#53009 = DIRECTION ( 'NONE',  ( 0.000000000000000000, 0.000000000000000000, 1.000000000000000000 ) ) ;
#53010 = CARTESIAN_POINT ( 'NONE',  ( 5.897433631820129918, 8.863794422890064695, -1.082531754730537976 ) ) ;
#53012 =( BOUNDED_CURVE ( )  B_SPLINE_CURVE ( 2, ( #167144, #51256, #100002, #38205, #68539, #166069, #168202, #153020, #202808, #121675, #134667, #34984, #154092, #69606, #4595, #120600, #200670, #17656, #84813, #102133, #186577, #71740, #187640, #55519, #83739, #18729, #5660, #104279, #19801, #170323, #184436, #137854, #21911, #149831, #1401, #101055, #88020, #169267, #203875, #67462, #133608, #199613, #183378, #150902, #37126, #20853, #2463, #185501, #103205, #52320, #118449, #36053, #85885, #135713, #151961, #3531, #201739, #53380, #119515, #194245, #108802, #160686, #75171, #144480, #211547, #93573, #95713, #92516, #78359, #29628, #61049, #63182, #127209, #126132, #109872, #13358, #193177, #12281, #142337, #141281, #143408, #207289, #175885 ),
 .UNSPECIFIED., .F., .T. ) 
 B_SPLINE_CURVE_WITH_KNOTS ( ( 3, 2, 2, 2, 2, 2, 2, 2, 2, 2, 2, 2, 2, 2, 2, 2, 2, 2, 2, 2, 2, 2, 2, 2, 2, 2, 2, 2, 2, 2, 2, 2, 2, 2, 2, 2, 2, 2, 2, 2, 2, 3 ),
 ( 0.1856859352924667417, 0.1944444444444444475, 0.2083333333333333426, 0.2222222222222222099, 0.2361111111111111049, 0.2500000000000000000, 0.2638888888888888951, 0.2777777777777777901, 0.2916666666666666852, 0.3055555555555555802, 0.3194444444444444198, 0.3333333333333333148, 0.3472222222222222099, 0.3611111111111111049, 0.3750000000000000000, 0.3888888888888888951, 0.4027777777777777901, 0.4166666666666666852, 0.4305555555555555802, 0.4444444444444444198, 0.4583333333333333148, 0.4722222222222222099, 0.4861111111111111049, 0.5000000000000000000, 0.5138888888888888395, 0.5277777777777777901, 0.5416666666666666297, 0.5555555555555555802, 0.5694444444444444198, 0.5833333333333333703, 0.5972222222222222099, 0.6111111111111111605, 0.6250000000000000000, 0.6388888888888888395, 0.6527777777777777901, 0.6666666666666667407, 0.6805555555555555802, 0.6944444444444444198, 0.7083333333333332593, 0.7222222222222220989, 0.7361111111111111605, 0.7435077961461751261 ),
 .UNSPECIFIED. ) 
 CURVE ( )  GEOMETRIC_REPRESENTATION_ITEM ( )  RATIONAL_B_SPLINE_CURVE ( ( 0.9375838258011983672, 0.9155139236497713551, 1.000000000000000000, 0.8660254037844387076, 1.000000000000000000, 0.8660254037844387076, 1.000000000000000000, 0.8660254037844387076, 1.000000000000000000, 0.8660254037844387076, 1.000000000000000000, 0.8660254037844387076, 1.000000000000000000, 0.8660254037844387076, 1.000000000000000000, 0.8660254037844387076, 1.000000000000000000, 0.8660254037844387076, 1.000000000000000000, 0.8660254037844387076, 1.000000000000000000, 0.8660254037844387076, 1.000000000000000000, 0.8660254037844387076, 1.000000000000000000, 0.8660254037844387076, 1.000000000000000000, 0.8660254037844387076, 1.000000000000000000, 0.8660254037844387076, 1.000000000000000000, 0.8660254037844387076, 1.000000000000000000, 0.8660254037844387076, 1.000000000000000000, 0.8660254037844387076, 1.000000000000000000, 0.8660254037844387076, 1.000000000000000000, 0.8660254037844387076, 1.000000000000000000, 0.8660254037844387076, 1.000000000000000000, 0.8660254037844387076, 1.000000000000000000, 0.8660254037844387076, 1.000000000000000000, 0.8660254037844387076, 1.000000000000000000, 0.8660254037844387076, 1.000000000000000000, 0.8660254037844387076, 1.000000000000000000, 0.8660254037844387076, 1.000000000000000000, 0.8660254037844387076, 1.000000000000000000, 0.8660254037844387076, 1.000000000000000000, 0.8660254037844387076, 1.000000000000000000, 0.8660254037844387076, 1.000000000000000000, 0.8660254037844387076, 1.000000000000000000, 0.8660254037844387076, 1.000000000000000000, 0.8660254037844387076, 1.000000000000000000, 0.8660254037844387076, 1.000000000000000000, 0.8660254037844387076, 1.000000000000000000, 0.8660254037844387076, 1.000000000000000000, 0.8660254037844387076, 1.000000000000000000, 0.8660254037844387076, 1.000000000000000000, 0.8660254037844387076, 1.000000000000000000, 0.9286503118547393409, 0.9332967922701964625 ) ) 
 REPRESENTATION_ITEM ( '' )  );
#53011 = CARTESIAN_POINT ( 'NONE',  ( 1.364683531249996529, 13.27604166700806765, 0.7879004041258403923 ) ) ;
#53014 = CARTESIAN_POINT ( 'NONE',  ( 1.101899038012419174, -0.8149344392366760781, 1.617857622727811862 ) ) ;
#53013 = CARTESIAN_POINT ( 'NONE',  ( 6.343235766347262938, 8.493804042195527870, -1.599625672291281386 ) ) ;
#53015 = CARTESIAN_POINT ( 'NONE',  ( -8.128276786592724790, 9.441743324901704426, -1.199719254218446718 ) ) ;
#53016 = CARTESIAN_POINT ( 'NONE',  ( 4.656335691289526402, 7.519809842224722374, -1.199719254218452047 ) ) ;
#53017 = DIRECTION ( 'NONE',  ( -1.000000000000000000, 5.578564026256490882E-16, -1.264049978315544409E-61 ) ) ;
#53018 = CARTESIAN_POINT ( 'NONE',  ( -11.49978884755372732, 11.24270821162817668, 3.429452816445257124 ) ) ;
#53019 = CARTESIAN_POINT ( 'NONE',  ( 3.928111819657337911, 5.605883094398769195, 1.599625672291267398 ) ) ;
#53020 = ORIENTED_EDGE ( 'NONE', *, *, #129464, .T. ) ;
#53021 = CARTESIAN_POINT ( 'NONE',  ( 5.923453886551514280, -1.462456689723025782, -1.388475849216065372 ) ) ;
#53022 = CARTESIAN_POINT ( 'NONE',  ( -0.1104750535120025967, -0.004616138082884357029, -2.103378236956429337 ) ) ;
#53023 = CARTESIAN_POINT ( 'NONE',  ( -2.995508107964761191, 6.411541510041463887, -0.7147908198718248007 ) ) ;
#53024 = CARTESIAN_POINT ( 'NONE',  ( 0.1405533004714800693, 1.287645162063441928, -2.525240623925705474 ) ) ;
#53025 = DIRECTION ( 'NONE',  ( 6.314299915563594049E-62, 8.546850786086437571E-32, 1.000000000000000000 ) ) ;
#53026 = CARTESIAN_POINT ( 'NONE',  ( -4.067082894419624672, 6.728385229256075739, 1.082531754730560403 ) ) ;
#53027 = CARTESIAN_POINT ( 'NONE',  ( 8.595506201384004896, 12.01154575404795466, 1.082531754730546636 ) ) ;
#53028 = CARTESIAN_POINT ( 'NONE',  ( 3.731269929808676000, 0.05278475387572807015, -1.968924232409387409 ) ) ;
#53029 = CARTESIAN_POINT ( 'NONE',  ( 4.288685525864014636, 1.556897452430844320, -1.281376678550147474 ) ) ;
#53030 = CARTESIAN_POINT ( 'NONE',  ( -5.910464900553636269, 8.982960586366182554, -1.199719254218440723 ) ) ;
#53031 = CARTESIAN_POINT ( 'NONE',  ( 6.727182134110196721, 6.033756510516266935, 2.783943001041962795 ) ) ;
#53032 = CARTESIAN_POINT ( 'NONE',  ( 4.752002516643937469, 0.8370584164609263800, 2.025481692006773748 ) ) ;
#53033 = CARTESIAN_POINT ( 'NONE',  ( -10.18461545817740088, 3.956598013261175772, 5.433575010662861082 ) ) ;
#53034 = CARTESIAN_POINT ( 'NONE',  ( 2.625899107431714175, -1.107553820047700199, -1.575994028688005644 ) ) ;
#53035 = CARTESIAN_POINT ( 'NONE',  ( -8.694856585065634746, 9.038420858865048757, 0.7998128361456462443 ) ) ;
#53036 = CARTESIAN_POINT ( 'NONE',  ( -0.1294898018152226826, 6.948707995275583471, -2.521562306467279857 ) ) ;
#53037 = CARTESIAN_POINT ( 'NONE',  ( 0.1533209562146371774, -1.769702838771534559, 1.318327933512997152 ) ) ;
#53038 = DIRECTION ( 'NONE',  ( 1.214306433183764966E-17, 1.000000000000000000, 5.200010849845536803E-32 ) ) ;
#53039 = EDGE_CURVE ( 'NONE', #145305, #160077, #106576, .T. ) ;
#53040 = VERTEX_POINT ( 'NONE', #155279 ) ;
#53041 = CARTESIAN_POINT ( 'NONE',  ( 5.085717018901939390, 5.105960408239938353, 0.000000000000000000 ) ) ;
#53042 = ORIENTED_EDGE ( 'NONE', *, *, #207178, .T. ) ;
#53043 = CARTESIAN_POINT ( 'NONE',  ( 5.102387438446081447, 1.963913563476852309, 0.1487572088093111478 ) ) ;
#53045 = CARTESIAN_POINT ( 'NONE',  ( 4.248693477488805215, 1.974695210492120045, 0.3904942472512766827 ) ) ;
#53044 = CARTESIAN_POINT ( 'NONE',  ( 0.6791179963998601465, 1.305170301278056444, 1.438240348306470739 ) ) ;
#53046 = CARTESIAN_POINT ( 'NONE',  ( 5.782642724008081103, -2.244312133422786015, 0.4951331349164668216 ) ) ;
#53048 = CARTESIAN_POINT ( 'NONE',  ( 3.994834637159989654, 0.2691826048217076384, 1.841218289905453664 ) ) ;
#53047 = CARTESIAN_POINT ( 'NONE',  ( 10.59763834280244232, 9.799999999999998934, -3.303285708550596222 ) ) ;
#53049 = CARTESIAN_POINT ( 'NONE',  ( 6.688968683495743583, 8.897159112202094988, -1.599625672291283607 ) ) ;
#53050 = CARTESIAN_POINT ( 'NONE',  ( -7.777967379493323286, -6.134628647623485698, -7.664830294503433450 ) ) ;
#53051 = CARTESIAN_POINT ( 'NONE',  ( 4.207966135563078858, 7.175396087857926375, 7.500000000000000000 ) ) ;
#53052 = CARTESIAN_POINT ( 'NONE',  ( -5.194745412330402878, 9.212286747694129474, 0.000000000000000000 ) ) ;
#53053 = CARTESIAN_POINT ( 'NONE',  ( -3.375444385298249195, -0.9484041558699626284, 0.1508549929727657779 ) ) ;
#53054 = CARTESIAN_POINT ( 'NONE',  ( 0.4334776158547505864, -1.553986563932317377, -1.545601477622601472 ) ) ;
#53055 = CARTESIAN_POINT ( 'NONE',  ( 6.371969008742804697, 7.496680600697164465, -1.082531754730543083 ) ) ;
#53056 = VERTEX_POINT ( 'NONE', #74028 ) ;
#53057 = LINE ( 'NONE', #88779, #150419 ) ;
#53058 = CARTESIAN_POINT ( 'NONE',  ( 0.4162703231485806454, 1.261427835099769634, -1.320066674804179385 ) ) ;
#53059 = CARTESIAN_POINT ( 'NONE',  ( -5.284980951228653190, 5.060232619388524533, 0.000000000000000000 ) ) ;
#53060 = AXIS2_PLACEMENT_3D ( 'NONE', #127579, #211912, #195687 ) ;
#53061 = CARTESIAN_POINT ( 'NONE',  ( 2.478840559695635548, -1.729657056378102853, -0.1252908626025364403 ) ) ;
#53062 = CARTESIAN_POINT ( 'NONE',  ( 1.499999999999959588, 8.500000000000000000, -10.89724735885168805 ) ) ;
#53063 = CARTESIAN_POINT ( 'NONE',  ( -11.04536101718726293, 10.09409062111168964, -1.100000000000000311 ) ) ;
#53064 = CARTESIAN_POINT ( 'NONE',  ( 0.4288785890452541105, 3.049942316455306113, 0.4196807566830256797 ) ) ;
#53065 = TOROIDAL_SURFACE ( 'NONE', #70209, 10.89999999999920632, 0.2000000000000000111 ) ;
#53066 = CARTESIAN_POINT ( 'NONE',  ( 5.022008369909983116, -0.9795521577263366364, -1.540466923627185292 ) ) ;
#53067 = CARTESIAN_POINT ( 'NONE',  ( 2.957805016080543137, -0.6199431972748243869, 1.861265166911832081 ) ) ;
#53068 = CARTESIAN_POINT ( 'NONE',  ( 0.6124999999999534150, -1.104166665983841167, 1.060881119635882497 ) ) ;
#53069 = CARTESIAN_POINT ( 'NONE',  ( -8.422639742587602285, 10.84949900448412841, -1.599625672291263179 ) ) ;
#53070 = CARTESIAN_POINT ( 'NONE',  ( 7.558834334818744338, 8.777393797832065303, 1.199719254218462483 ) ) ;
#53071 = CARTESIAN_POINT ( 'NONE',  ( 4.600305182625006317, -0.9987976242244798186, 1.870504488178956759 ) ) ;
#53072 = CARTESIAN_POINT ( 'NONE',  ( 7.856023664475727308, 8.130058794835305136, -0.7998128361456341429 ) ) ;
#53073 = CARTESIAN_POINT ( 'NONE',  ( -10.48453286206953727, 11.12637651536962125, 0.7998128361456462443 ) ) ;
#53074 = CIRCLE ( 'NONE', #87714, 0.07999999999999993228 ) ;
#53075 = CARTESIAN_POINT ( 'NONE',  ( 2.711853232431875593, 0.5564382603544039130, -1.993978196652478996 ) ) ;
#53077 = B_SPLINE_CURVE_WITH_KNOTS ( 'NONE', 3,
 ( #73815, #173478, #140995, #157212, #207003, #9872, #124787, #13061, #29336, #159329 ),
 .UNSPECIFIED., .F., .F.,
 ( 4, 3, 3, 4 ),
 ( 3.907308343762969252E-16, 8.899070015639609047E-05, 0.0001343825223669382267, 0.0001804666533476734377 ),
 .UNSPECIFIED. ) ;
#53076 = CARTESIAN_POINT ( 'NONE',  ( 1.364683531249986537, 0.4260416670080872659, 0.7879004041258500513 ) ) ;
#53079 = ORIENTED_EDGE ( 'NONE', *, *, #18341, .F. ) ;
#53078 = CARTESIAN_POINT ( 'NONE',  ( 4.336746411289113645, 1.366526421497065824, -1.751164563135388041 ) ) ;
#53080 = CARTESIAN_POINT ( 'NONE',  ( 3.323114718373169740, 1.032193166631629078, -2.053959190227053533 ) ) ;
#53081 = CARTESIAN_POINT ( 'NONE',  ( 7.619319141200051604, 11.83303006480134911, 0.7216878364870438212 ) ) ;
#53083 = CARTESIAN_POINT ( 'NONE',  ( 3.285556943749998737, -3.055208332855376518, -1.896917185911906500 ) ) ;
#53082 = CARTESIAN_POINT ( 'NONE',  ( 6.373741612200160667, 9.489763409991955001, 1.082531754730549078 ) ) ;
#53084 = ADVANCED_FACE ( 'NONE', ( #53501 ), #195363, .F. ) ;
#53085 = CARTESIAN_POINT ( 'NONE',  ( 0.000000000000000000, 2.499999999999998668, -4.500000000000000000 ) ) ;
#53086 =( NAMED_UNIT ( * ) PLANE_ANGLE_UNIT ( ) SI_UNIT ( $, .RADIAN. ) );
#53087 = ORIENTED_EDGE ( 'NONE', *, *, #118912, .F. ) ;
#53088 = CARTESIAN_POINT ( 'NONE',  ( -5.520955638564554846, 6.243838396700211568, -0.9653654033580265637 ) ) ;
#53089 = CARTESIAN_POINT ( 'NONE',  ( 2.918110517850933672, -1.910018876965378309, 0.09814724848770939314 ) ) ;
#53090 = CARTESIAN_POINT ( 'NONE',  ( 3.475000000000000533, -1.254166666666665098, 2.006292185433948827 ) ) ;
#53091 = CARTESIAN_POINT ( 'NONE',  ( 4.295721138614797319, -0.6590762262537721572, 1.594082981517078945 ) ) ;
#53092 = CARTESIAN_POINT ( 'NONE',  ( 2.887907956677421062, -2.014008092954455265, 0.1037802451031161616 ) ) ;
#53093 = CARTESIAN_POINT ( 'NONE',  ( 4.500793239850611194, -2.254531372669385636, 0.4477389049844481272 ) ) ;
#53094 = CARTESIAN_POINT ( 'NONE',  ( 0.000000000000000000, 13.49999999999999822, -1.500000000000000222 ) ) ;
#53095 = CARTESIAN_POINT ( 'NONE',  ( 6.076811011874215573, -1.999271364452784638, -0.6623750905550094270 ) ) ;
#53096 = CARTESIAN_POINT ( 'NONE',  ( -5.858531774880906262, 6.967946837850073294, 1.082531754730549078 ) ) ;
#53097 = ORIENTED_EDGE ( 'NONE', *, *, #209714, .F. ) ;
#53098 = CARTESIAN_POINT ( 'NONE',  ( 4.885902211565920972, -0.8344178305333300738, 1.560695085661115922 ) ) ;
#53099 = EDGE_CURVE ( 'NONE', #75305, #186393, #36441, .T. ) ;
#53101 = CARTESIAN_POINT ( 'NONE',  ( 0.7621917111494004304, 1.134545731666029011, 1.991736209811171054 ) ) ;
#53100 = CARTESIAN_POINT ( 'NONE',  ( 6.230854113932139171, 9.427024345299638952, 1.199719254218452047 ) ) ;
#53102 = CARTESIAN_POINT ( 'NONE',  ( 0.05802509242504564485, -1.552030147408272054, -0.7874549631982865616 ) ) ;
#53103 = CARTESIAN_POINT ( 'NONE',  ( -1.843739406749240750, 8.499999999999996447, -0.7749999999999996891 ) ) ;
#53104 = CARTESIAN_POINT ( 'NONE',  ( 6.386699327874667098, 1.908680410311427433, -1.076638258889956345 ) ) ;
#53105 = CARTESIAN_POINT ( 'NONE',  ( -5.004894982100124068, 5.868074229652107121, 1.199719254218452935 ) ) ;
#53106 = DIRECTION ( 'NONE',  ( -0.000000000000000000, 1.000000000000000000, -0.000000000000000000 ) ) ;
#53107 = CARTESIAN_POINT ( 'NONE',  ( 3.953965674029162436, 7.318484642604417445, -0.9046105126420730391 ) ) ;
#53108 = CARTESIAN_POINT ( 'NONE',  ( 6.777786256569462431, -2.009253640576996514, 0.4989836931604470505 ) ) ;
#53109 = CARTESIAN_POINT ( 'NONE',  ( 1.639861632979456418, 2.010800986640928656, -0.1531718788195315928 ) ) ;
#53110 = CARTESIAN_POINT ( 'NONE',  ( 1.364683531249990311, 5.613541667008087543, 0.7879004041258500513 ) ) ;
#53111 = CARTESIAN_POINT ( 'NONE',  ( 4.951747152513418904, 0.6024649636334912239, -1.829943702413504791 ) ) ;
#53112 = CARTESIAN_POINT ( 'NONE',  ( -1.364683531250010295, 11.38020833367473728, 0.7879004041258445001 ) ) ;
#53113 = CARTESIAN_POINT ( 'NONE',  ( 1.354101172232239580, -1.613524214714330940, -1.527088627841047375 ) ) ;
#53115 = VERTEX_POINT ( 'NONE', #75094 ) ;
#53114 = CARTESIAN_POINT ( 'NONE',  ( 8.380911511541880188, 12.92948053010758258, 0.7998128361456462443 ) ) ;
#53117 = DIRECTION ( 'NONE',  ( 0.000000000000000000, 1.000000000000000000, 6.661338147750951075E-16 ) ) ;
#53116 = CARTESIAN_POINT ( 'NONE',  ( 1.217358635584784965, 3.014784080462326266, -0.7749999999999840350 ) ) ;
#53118 = CYLINDRICAL_SURFACE ( 'NONE', #102730, 1.250000000000000000 ) ;
#53119 = CARTESIAN_POINT ( 'NONE',  ( 9.134442807305049428, 11.67993591332117376, 1.599625672291281386 ) ) ;
#53120 = CARTESIAN_POINT ( 'NONE',  ( -5.395781948114519722, 5.397426482329451325, 0.000000000000000000 ) ) ;
#53121 = LINE ( 'NONE', #3278, #177088 ) ;
#53122 = CARTESIAN_POINT ( 'NONE',  ( 4.616618505336416156, -0.07905358554981949115, 1.738770568734932853 ) ) ;
#53123 = CARTESIAN_POINT ( 'NONE',  ( 1.996468121258226924, 1.940055844723225009, 0.2909814450420752929 ) ) ;
#53125 = CARTESIAN_POINT ( 'NONE',  ( -0.6823417656250003738, 3.030208333674754062, -1.181850606188749264 ) ) ;
#53124 = CARTESIAN_POINT ( 'NONE',  ( 3.388648328411762556, 6.040841252200647382, 1.199719254218462483 ) ) ;
#53126 = CARTESIAN_POINT ( 'NONE',  ( -5.852179643265606579, 6.035944939585320412, -0.4116468081218557784 ) ) ;
#53127 = CARTESIAN_POINT ( 'NONE',  ( 8.530051201292206287, 13.10347683481629488, 0.000000000000000000 ) ) ;
#53128 = CIRCLE ( 'NONE', #136171, 0.07999999999999940492 ) ;
#53129 = VECTOR ( 'NONE', #203836, 1000.000000000000000 ) ;
#53130 = CARTESIAN_POINT ( 'NONE',  ( 6.197705743426439540, -1.420020466879829302, -1.353909852041992767 ) ) ;
#53131 = CARTESIAN_POINT ( 'NONE',  ( -7.588813295347149435, 9.876701482703580837, -1.599625672291263179 ) ) ;
#53132 = EDGE_CURVE ( 'NONE', #21505, #62722, #147729, .T. ) ;
#53133 = CARTESIAN_POINT ( 'NONE',  ( -3.253593677155282471, 6.739683690082376444, 1.040834085586084257E-14 ) ) ;
#53134 = CARTESIAN_POINT ( 'NONE',  ( 1.499281897245376527, 1.848817473390499844, -1.303928773892924609 ) ) ;
#53136 = VERTEX_POINT ( 'NONE', #131367 ) ;
#53135 = CARTESIAN_POINT ( 'NONE',  ( -5.904739593951539689, 6.847616600153594746, 1.199719254218450271 ) ) ;
#53137 = CARTESIAN_POINT ( 'NONE',  ( -0.7500000000000006661, 0.3895833340161539149, -1.299038105676652011 ) ) ;
#53138 = CARTESIAN_POINT ( 'NONE',  ( 1.809613641711980359, -1.857008771552502768, 0.2239427725650791623 ) ) ;
#53139 = CARTESIAN_POINT ( 'NONE',  ( 0.2989044949552251418, 1.198067244415670141, -1.254020425504979164 ) ) ;
#53140 = VECTOR ( 'NONE', #42323, 1000.000000000000114 ) ;
#53141 = CARTESIAN_POINT ( 'NONE',  ( 4.704715985517350596, 1.906866092115505840, 1.080010033982371498 ) ) ;
#53142 = CARTESIAN_POINT ( 'NONE',  ( 5.034332918631054810, 1.191367258472323831, -1.976142064534849307 ) ) ;
#53143 = CARTESIAN_POINT ( 'NONE',  ( 1.463821189631772990, 2.030551501382936497, -0.3513165408277911794 ) ) ;
#53144 = CARTESIAN_POINT ( 'NONE',  ( 3.152217820003437421, -1.470166820979129207, 1.268861441860974049 ) ) ;
#53145 = CARTESIAN_POINT ( 'NONE',  ( -4.406036734316900905, 5.203092947200234519, -1.082531754730543971 ) ) ;
#53146 = CARTESIAN_POINT ( 'NONE',  ( 5.395714598229544023, -0.6742385858747660388, 1.744967798948720228 ) ) ;
#53147 = CARTESIAN_POINT ( 'NONE',  ( 4.001984418394623155, 7.593073144423666321, -0.1798963839820325039 ) ) ;
#53148 = CARTESIAN_POINT ( 'NONE',  ( 6.556017512941495262, 1.755498886817616677, -0.9912500394320120645 ) ) ;
#53149 = CARTESIAN_POINT ( 'NONE',  ( 4.041739190649647817, 6.769093918182960579, -1.082531754730548412 ) ) ;
#53150 = CARTESIAN_POINT ( 'NONE',  ( -1.360316468750013108, 1.140625000341413564, -2.081668171172168513E-14 ) ) ;
#53152 = CARTESIAN_POINT ( 'NONE',  ( 4.430314669760617718, -1.560499787156752971, -1.277043788614096176 ) ) ;
#53151 = AXIS2_PLACEMENT_3D ( 'NONE', #35961, #18637, #134574 ) ;
#53153 = CARTESIAN_POINT ( 'NONE',  ( -4.758548728272219641, 4.653987725846768342, 0.7216878364870317197 ) ) ;
#53154 = CARTESIAN_POINT ( 'NONE',  ( -6.642568916052639771, 6.714361588341672515, 0.000000000000000000 ) ) ;
#53155 = CARTESIAN_POINT ( 'NONE',  ( 8.259941899223605333, 10.65968485389279508, -1.599625672291268286 ) ) ;
#53157 = CARTESIAN_POINT ( 'NONE',  ( -1.230761180058579152, 3.146116465842661025, 0.7750000000000100142 ) ) ;
#53156 = CARTESIAN_POINT ( 'NONE',  ( 1.646812808029130215, -1.543121136568927243, 0.9753659028155501343 ) ) ;
#53158 = CARTESIAN_POINT ( 'NONE',  ( -4.797606254389363833, 6.690569611577942943, 1.599625672291263179 ) ) ;
#53159 = CARTESIAN_POINT ( 'NONE',  ( -5.438755897737433287, 6.374245297895642537, -1.199719254218453823 ) ) ;
#53160 = CARTESIAN_POINT ( 'NONE',  ( -10.12531724201500616, 3.239403609407997653, 5.873437370650227862 ) ) ;
#53161 = VERTEX_POINT ( 'NONE', #98819 ) ;
#53162 = CARTESIAN_POINT ( 'NONE',  ( -6.007671464186866928, 8.102312356341712984, 1.443375672974058777 ) ) ;
#53163 = UNCERTAINTY_MEASURE_WITH_UNIT (LENGTH_MEASURE( 1.000000000000000082E-05 ), #207917, 'distance_accuracy_value', 'NONE');
#53164 = CARTESIAN_POINT ( 'NONE',  ( -3.898132859128961236, 4.506575409527250997, -1.199719254218452047 ) ) ;
#53165 = CARTESIAN_POINT ( 'NONE',  ( -10.63367255181986160, 11.30037282007833532, 1.040834085586084257E-14 ) ) ;
#53166 = CARTESIAN_POINT ( 'NONE',  ( 5.795571226005820087, 1.865288689459403848, -0.7749498061812712946 ) ) ;
#53168 = ORIENTED_EDGE ( 'NONE', *, *, #106621, .T. ) ;
#53167 = CARTESIAN_POINT ( 'NONE',  ( 0.5398874254142792539, -2.012210497580559476, 0.6691108114003360141 ) ) ;
#53169 = CARTESIAN_POINT ( 'NONE',  ( -6.180537922983287302, 8.303989891604203422, -1.599625672291271394 ) ) ;
#53170 = CARTESIAN_POINT ( 'NONE',  ( 6.166260936116925606, 6.088392601758203071, 0.7998128361456341429 ) ) ;
#53171 = CARTESIAN_POINT ( 'NONE',  ( 5.084866380259029484, -0.2499542577577648639, -2.045595823183245621 ) ) ;
#53172 = CARTESIAN_POINT ( 'NONE',  ( 4.606092368833686557, -0.09613688574180989654, 2.014232646917232916 ) ) ;
#53173 = VERTEX_POINT ( 'NONE', #197362 ) ;
#53174 = ORIENTED_EDGE ( 'NONE', *, *, #185954, .T. ) ;
#53175 = CARTESIAN_POINT ( 'NONE',  ( 10.04733898909039702, 1.529612873802630224, 6.247711339170956890 ) ) ;
#53176 = CARTESIAN_POINT ( 'NONE',  ( -1.861683537984881509, 2.483860266822599083, 2.478752606221127142 ) ) ;
#53178 = ORIENTED_EDGE ( 'NONE', *, *, #151345, .F. ) ;
#53177 = CARTESIAN_POINT ( 'NONE',  ( -5.468734858265826837, 7.473552982767158070, 1.599625672291263179 ) ) ;
#53179 = CARTESIAN_POINT ( 'NONE',  ( 5.184698244283005408, 7.856242361780820360, 1.254847465626233616 ) ) ;
#53180 = CARTESIAN_POINT ( 'NONE',  ( 5.518907608433407219, 2.013924273726455549, -0.09612181791086168992 ) ) ;
#53181 = CARTESIAN_POINT ( 'NONE',  ( 3.960763856159645879, 0.2235175650571289141, -1.827449369368571386 ) ) ;
#53182 = CARTESIAN_POINT ( 'NONE',  ( -0.02319159430947542386, 0.2540490248266329965, -1.846305437520213477 ) ) ;
#53183 = CARTESIAN_POINT ( 'NONE',  ( 1.647554839532150872, -1.947651944554330772, 1.237524531948221096 ) ) ;
#53184 = CARTESIAN_POINT ( 'NONE',  ( 7.679767667498067496, 7.924426798361372093, 0.000000000000000000 ) ) ;
#53185 = CARTESIAN_POINT ( 'NONE',  ( 4.376362478467909156, -1.248523626585487989, 1.764366501186130698 ) ) ;
#53186 = CARTESIAN_POINT ( 'NONE',  ( 7.086107841436786181, 11.41887624831828418, 1.040834085586084257E-14 ) ) ;
#53188 = CARTESIAN_POINT ( 'NONE',  ( 2.676970549635893537, 1.727063564601112100, -1.040793759654296213 ) ) ;
#53187 = CARTESIAN_POINT ( 'NONE',  ( -0.05917297228825654093, -1.501800262597710267, -1.231000148999121357 ) ) ;
#53189 = CARTESIAN_POINT ( 'NONE',  ( -6.084912014434944894, 5.993485526462540847, -0.7998128361456291469 ) ) ;
#53190 = DIRECTION ( 'NONE',  ( -0.6743504407188151140, 0.000000000000000000, -0.7384114592165670343 ) ) ;
#53191 = CARTESIAN_POINT ( 'NONE',  ( -3.578989363883261277, 7.119311991265024453, 1.040834085586084257E-14 ) ) ;
#53192 = CARTESIAN_POINT ( 'NONE',  ( 3.819104250046548632, -0.1383300533824398659, 1.865606469731183825 ) ) ;
#53193 = CARTESIAN_POINT ( 'NONE',  ( 6.631714602856194851, -1.287423518921044341, -1.493153376739835947 ) ) ;
#53195 = CARTESIAN_POINT ( 'NONE',  ( -7.425025402139490360, 8.691559719698066289, 1.199719254218452047 ) ) ;
#53194 = CARTESIAN_POINT ( 'NONE',  ( -0.7500000000000249800, -1.277083332650516656, 1.299038105676659116 ) ) ;
#53196 = CARTESIAN_POINT ( 'NONE',  ( 1.541937560865791479, -1.600244427420342896, -1.519961040588948986 ) ) ;
#53197 = ORIENTED_EDGE ( 'NONE', *, *, #212020, .T. ) ;
#53198 = CARTESIAN_POINT ( 'NONE',  ( 11.78331023100045627, 13.79999999999998295, 1.799999999999999600 ) ) ;
#53199 = CARTESIAN_POINT ( 'NONE',  ( 3.181359600701000989, 6.863336634126477875, 0.000000000000000000 ) ) ;
#53200 = CARTESIAN_POINT ( 'NONE',  ( -3.411848212133334446, 7.132240014130862171, 0.7998128361456341429 ) ) ;
#53201 = CARTESIAN_POINT ( 'NONE',  ( -7.784592198500340565, -5.601927612791713251, 7.772296586883744141 ) ) ;
#53202 = CARTESIAN_POINT ( 'NONE',  ( 6.789933821422706295, -0.8420773930338676383, 1.780570074765168043 ) ) ;
#53203 = CARTESIAN_POINT ( 'NONE',  ( 0.3765545373161778286, 1.332373789618445770, 1.883912488508274752 ) ) ;
#53204 = CARTESIAN_POINT ( 'NONE',  ( 0.4671467121175364445, 1.705069321186868159, 0.9702857188121425391 ) ) ;
#53205 = CARTESIAN_POINT ( 'NONE',  ( 4.522371018022923295, 0.9678747400500853360, 1.821345444039919270 ) ) ;
#53206 = CARTESIAN_POINT ( 'NONE',  ( 5.666945020832177882, 6.674152614801420746, 1.082531754730558626 ) ) ;
#53207 = CARTESIAN_POINT ( 'NONE',  ( 5.397027666691686321, 8.454226823519094935, 1.199719254218451159 ) ) ;
#53208 = ORIENTED_EDGE ( 'NONE', *, *, #198981, .F. ) ;
#53209 =( BOUNDED_CURVE ( )  B_SPLINE_CURVE ( 2, ( #172382, #156136, #7718, #139896, #27176, #62876, #79129, #177716, #109582 ),
 .UNSPECIFIED., .F., .T. ) 
 B_SPLINE_CURVE_WITH_KNOTS ( ( 3, 2, 2, 2, 3 ),
 ( 0.8660714285714286031, 0.8690476190476190688, 0.8750000000000000000, 0.8809523809523809312, 0.8839285714285713969 ),
 .UNSPECIFIED. ) 
 CURVE ( )  GEOMETRIC_REPRESENTATION_ITEM ( )  RATIONAL_B_SPLINE_CURVE ( ( 0.9330127018922194093, 0.9330127018922194093, 1.000000000000000000, 0.8660254037844387076, 1.000000000000000000, 0.8660254037844387076, 1.000000000000000000, 0.9330127018922194093, 0.9330127018922194093 ) ) 
 REPRESENTATION_ITEM ( '' )  );
#53210 = CARTESIAN_POINT ( 'NONE',  ( 7.795575137733369075, 9.157554417852841411, -1.082531754730537976 ) ) ;
#53211 = CARTESIAN_POINT ( 'NONE',  ( 1.364683531249990311, 5.196875000341417916, 1.214306433183764966E-14 ) ) ;
#53212 = CARTESIAN_POINT ( 'NONE',  ( -10.30773516381138855, 3.837475087047823141, -6.058016394929252257 ) ) ;
#53213 = CARTESIAN_POINT ( 'NONE',  ( 4.731432421044862835, 6.543090462684225450, -1.443375672974051449 ) ) ;
#53214 = CARTESIAN_POINT ( 'NONE',  ( 6.602019255160630706, 0.8372048429528687885, -2.003470777635954381 ) ) ;
#53216 = CARTESIAN_POINT ( 'NONE',  ( 5.618664544990171095, -0.03892770779775727580, 1.841008343696965310 ) ) ;
#53215 = CARTESIAN_POINT ( 'NONE',  ( 9.498884310698278099, -9.746166700192997467, -0.1658036423878402332 ) ) ;
#53217 = CARTESIAN_POINT ( 'NONE',  ( -2.483409115735836892, 3.555461883994699868, 11.68352130004407030 ) ) ;
#53218 = CARTESIAN_POINT ( 'NONE',  ( 1.947569660854353790, 3.752493983412333645, 0.4616071351972801939 ) ) ;
#53219 = DIRECTION ( 'NONE',  ( 0.000000000000000000, 0.000000000000000000, -1.000000000000000000 ) ) ;
#53220 = CARTESIAN_POINT ( 'NONE',  ( -4.357679483485834560, 7.387146062586773532, 1.181458644690215998 ) ) ;
#53221 = CARTESIAN_POINT ( 'NONE',  ( -0.4000000000000114575, 2.902482508373164904, 2.023857702507793288 ) ) ;
#53222 = CARTESIAN_POINT ( 'NONE',  ( 5.364607279338250656, 7.693244595681929532, -1.319704323257679057 ) ) ;
#53223 = CARTESIAN_POINT ( 'NONE',  ( -0.6823417656249969321, 5.280208333674756283, -1.181850606188749264 ) ) ;
#53224 = CARTESIAN_POINT ( 'NONE',  ( 1.629408300089077111, -0.2329066467734331181, 1.897959532673603844 ) ) ;
#53225 = CARTESIAN_POINT ( 'NONE',  ( 1.709447022217532641, -1.756973726300320449, 0.2123998563456699906 ) ) ;
#53226 = CARTESIAN_POINT ( 'NONE',  ( 5.883453010584854148, 0.1459518013421389204, -2.007843741401983184 ) ) ;
#53228 = CARTESIAN_POINT ( 'NONE',  ( 4.306187113567048641, 1.175507255964372222, -1.512451795395561405 ) ) ;
#53227 = CARTESIAN_POINT ( 'NONE',  ( -8.292783513053063160, 12.82666453187061073, 0.7998128361456481317 ) ) ;
#53229 = DIRECTION ( 'NONE',  ( -7.387867266669436732E-31, -1.000000000000000000, 8.546850786086437571E-32 ) ) ;
#53230 = B_SPLINE_CURVE_WITH_KNOTS ( 'NONE', 3,
 ( #167611, #84221, #129865, #115714 ),
 .UNSPECIFIED., .F., .F.,
 ( 4, 4 ),
 ( -1.944647862007489213E-06, 0.0001035599091551129175 ),
 .UNSPECIFIED. ) ;
#53231 = CARTESIAN_POINT ( 'NONE',  ( 5.125436402459787821, 0.1948648891074710732, -1.959901157258244098 ) ) ;
#53232 = CARTESIAN_POINT ( 'NONE',  ( 0.3871773095200456982, -1.998849835692744659, -0.7086421328065874992 ) ) ;
#53233 = CARTESIAN_POINT ( 'NONE',  ( 0.000000000000000000, -6.893137084989842123, 0.000000000000000000 ) ) ;
#53234 = CARTESIAN_POINT ( 'NONE',  ( 4.240975883383619305, -1.627667033997456381, 0.9218181776217827528 ) ) ;
#53236 = ORIENTED_EDGE ( 'NONE', *, *, #58935, .F. ) ;
#53235 = CARTESIAN_POINT ( 'NONE',  ( 6.340463942928090901, 1.707257656261139234, 0.2451334271395839426 ) ) ;
#53238 = DIRECTION ( 'NONE',  ( -0.05727394217551268901, 3.884134901109067902E-16, -0.9983585005135560131 ) ) ;
#53237 = CARTESIAN_POINT ( 'NONE',  ( 3.651171877326536030, -1.804458330144659950, 1.270265763067345066 ) ) ;
#53239 = EDGE_CURVE ( 'NONE', #146583, #64997, #10735, .T. ) ;
#53240 = CARTESIAN_POINT ( 'NONE',  ( -0.6823417656250212460, 4.113541667008085767, 1.181850606188767472 ) ) ;
#53241 = CARTESIAN_POINT ( 'NONE',  ( 0.8188879582939897483, -1.495318261269963589, 1.421039783695568604 ) ) ;
#53242 = CARTESIAN_POINT ( 'NONE',  ( 8.288111976655649471, 8.563885482386732306, -0.7998128361456291469 ) ) ;
#53243 = CARTESIAN_POINT ( 'NONE',  ( -7.492852449846775897, 11.89341162479659531, 0.000000000000000000 ) ) ;
#53244 = CARTESIAN_POINT ( 'NONE',  ( -9.333041836226904309, 15.44694763438996077, -7.472413793095822321 ) ) ;
#53245 = CARTESIAN_POINT ( 'NONE',  ( -4.416205349749324327, 6.175325546172741653, 1.599625672291267175 ) ) ;
#53246 = CARTESIAN_POINT ( 'NONE',  ( -5.277545713794630444, 7.647399700472480077, -1.235574677996098325 ) ) ;
#53247 = ORIENTED_EDGE ( 'NONE', *, *, #910, .F. ) ;
#53248 = CARTESIAN_POINT ( 'NONE',  ( 2.945825538390862697, 1.462269270728074222, 1.465923284304726737 ) ) ;
#53249 = CARTESIAN_POINT ( 'NONE',  ( 1.499999999999990896, 4.275000000000021672, 1.214306433183764966E-14 ) ) ;
#53250 = CARTESIAN_POINT ( 'NONE',  ( 5.335297142177534369, 6.183267073083954735, -1.199719254218452047 ) ) ;
#53251 = CARTESIAN_POINT ( 'NONE',  ( -6.592485395868785680, 6.772832640907240354, 0.2792626473412176957 ) ) ;
#53252 = CARTESIAN_POINT ( 'NONE',  ( 0.9088601047923352549, -0.4930153254206064428, -1.958433058913966018 ) ) ;
#53253 = SURFACE_STYLE_FILL_AREA ( #186437 ) ;
#53254 = EDGE_LOOP ( 'NONE', ( #74761, #81117, #9415, #66185, #149490 ) ) ;
#53256 = CARTESIAN_POINT ( 'NONE',  ( 7.890482213473377193, 11.18901776815221716, -1.082531754730543083 ) ) ;
#53255 = CARTESIAN_POINT ( 'NONE',  ( 0.07499057489264349119, 0.2503043380940940810, -1.990932473338621778 ) ) ;
#53257 = CARTESIAN_POINT ( 'NONE',  ( 6.626327358740755180, 0.3474107405085808953, -1.985797104380654376 ) ) ;
#53258 = CARTESIAN_POINT ( 'NONE',  ( 5.577321932364699641, 1.455147452656019524, 1.246156846922679584 ) ) ;
#53259 = CARTESIAN_POINT ( 'NONE',  ( 6.539320575229251808, 6.034535422585679321, 2.798157489527762554 ) ) ;
#53260 = CARTESIAN_POINT ( 'NONE',  ( 4.212563348414651188, 2.004022095860341413, 0.8874167208733558798 ) ) ;
#53261 = CARTESIAN_POINT ( 'NONE',  ( -1.499999999999997780, 3.931250000682819046, 1.214306433183764966E-14 ) ) ;
#53262 = CARTESIAN_POINT ( 'NONE',  ( 3.129067941553372645, 1.730785544086024696, 0.8136490247460312908 ) ) ;
#53263 = CARTESIAN_POINT ( 'NONE',  ( -4.055860508782465068, 7.883587693554856557, 1.040834085586084257E-14 ) ) ;
#53264 = CARTESIAN_POINT ( 'NONE',  ( 3.755245360860917536, 5.404205559136275205, -1.443375672974051449 ) ) ;
#53266 = CARTESIAN_POINT ( 'NONE',  ( 0.6851730022342136239, 1.650096953764205399, 1.158669022729153175 ) ) ;
#53265 = LINE ( 'NONE', #205903, #73478 ) ;
#53267 = CARTESIAN_POINT ( 'NONE',  ( -1.364683531250010295, 11.44270833367472662, 0.7879004041258445001 ) ) ;
#53269 = CARTESIAN_POINT ( 'NONE',  ( -4.817943484809863008, 6.714296380401858499, 1.599625672291263179 ) ) ;
#53268 = CARTESIAN_POINT ( 'NONE',  ( 5.776942576169182608, 2.025397260235710206, -0.8375503648087383457 ) ) ;
#53271 = EDGE_LOOP ( 'NONE', ( #103103, #212461, #64697, #109125 ) ) ;
#53270 = CARTESIAN_POINT ( 'NONE',  ( 3.311258828109595154, -0.3375135790737812114, 1.691226829923969666 ) ) ;
#53272 = CARTESIAN_POINT ( 'NONE',  ( -0.1405533004718313439, 1.431097497908106808, -1.984188993888830632 ) ) ;
#53273 = CARTESIAN_POINT ( 'NONE',  ( 6.771407655021410399, 9.987393799911945536, -1.199719254218441611 ) ) ;
#53274 = CARTESIAN_POINT ( 'NONE',  ( 5.660692828905515839, 6.562895374266609849, -1.199719254218445830 ) ) ;
#53275 = DIRECTION ( 'NONE',  ( 0.000000000000000000, 1.000000000000000000, 0.000000000000000000 ) ) ;
#53276 = CARTESIAN_POINT ( 'NONE',  ( 1.381223342121252085, -0.05156877537583307025, 1.961363007973878858 ) ) ;
#53277 = CARTESIAN_POINT ( 'NONE',  ( 3.734381245560244089, 6.444196322207211836, 1.199719254218462483 ) ) ;
#53278 = CARTESIAN_POINT ( 'NONE',  ( 0.1755611466353291517, 1.991966693188641280, -2.657903234774192658 ) ) ;
#53279 = ORIENTED_EDGE ( 'NONE', *, *, #174533, .T. ) ;
#53280 = CARTESIAN_POINT ( 'NONE',  ( 0.000000000000000000, 2.000000000000001776, -10.25000000000000000 ) ) ;
#53281 = ORIENTED_EDGE ( 'NONE', *, *, #78072, .T. ) ;
#53282 = CARTESIAN_POINT ( 'NONE',  ( 4.336430608486574911, 1.111010274217393956, -1.430681851146862416 ) ) ;
#53283 = EDGE_LOOP ( 'NONE', ( #167868, #163308, #30424, #119957 ) ) ;
#53284 = CARTESIAN_POINT ( 'NONE',  ( 9.348510611822643313, 10.86534945433664134, 1.199719254218453823 ) ) ;
#53285 = DIRECTION ( 'NONE',  ( -0.6483454320283799088, 0.000000000000000000, 0.7613463080411786432 ) ) ;
#53286 = CARTESIAN_POINT ( 'NONE',  ( 5.197853184559683370, 1.220981990389960581, 1.338314830865680261 ) ) ;
#53287 = CARTESIAN_POINT ( 'NONE',  ( 6.441532379824158383, 9.568852638886589546, -1.082531754730548412 ) ) ;
#53288 = CARTESIAN_POINT ( 'NONE',  ( -6.500815859342971237, -6.554751161430533379, -6.901817408925770891 ) ) ;
#53289 = CARTESIAN_POINT ( 'NONE',  ( 5.387724311900628393, 6.300193624175450147, -1.063853923354351361 ) ) ;
#53291 = CARTESIAN_POINT ( 'NONE',  ( -0.6823417656250039265, 15.31770833367473372, -1.181850606188755259 ) ) ;
#53290 = CARTESIAN_POINT ( 'NONE',  ( 5.160548226176637776, -0.6268552802725676498, -1.752456121274186263 ) ) ;
#53292 = CARTESIAN_POINT ( 'NONE',  ( 2.653800294728881681, 1.026947457930127872, 1.616878242289141676 ) ) ;
#53293 = MECHANICAL_DESIGN_GEOMETRIC_PRESENTATION_REPRESENTATION (  '', ( #105266 ), #11829 ) ;
#53294 = CARTESIAN_POINT ( 'NONE',  ( -6.625366561259609988, -8.010031549403139550, -6.808607288253771372 ) ) ;
#53295 = CARTESIAN_POINT ( 'NONE',  ( -10.47476631618627252, 5.237304525980054137, 5.169966676860812349 ) ) ;
#53296 = CARTESIAN_POINT ( 'NONE',  ( 0.000000000000000000, 0.000000000000000000, 0.000000000000000000 ) ) ;
#53297 = CARTESIAN_POINT ( 'NONE',  ( 11.44791656467458552, 13.79999999999997939, 3.303228920649576406 ) ) ;
#53298 = VECTOR ( 'NONE', #154735, 1000.000000000000000 ) ;
#53299 = CARTESIAN_POINT ( 'NONE',  ( 6.697364695470787943, 7.876308901879812474, -1.082531754730543083 ) ) ;
#53300 = CARTESIAN_POINT ( 'NONE',  ( -8.351459436338023679, 12.68719374246231624, -0.7216878364870267237 ) ) ;
#53301 = CARTESIAN_POINT ( 'NONE',  ( 0.08116279290028630133, -0.1557560750096824431, -2.127278773206460638 ) ) ;
#53302 = CARTESIAN_POINT ( 'NONE',  ( -4.776215253764153346, 8.794277906025310898, -0.7998128361456362523 ) ) ;
#53303 = CARTESIAN_POINT ( 'NONE',  ( 2.572312895708084302, -2.000810251872984225, -0.6062274732134291799 ) ) ;
#53304 = CARTESIAN_POINT ( 'NONE',  ( 4.583538449871731757, 7.505156070562471804, 1.199719254218451159 ) ) ;
#53305 = CARTESIAN_POINT ( 'NONE',  ( 0.4635302585514287088, 1.806487598472360956, -0.2625014351145052438 ) ) ;
#53306 = CARTESIAN_POINT ( 'NONE',  ( -5.091250377131585125, 5.898545847196970726, 1.199719254218450271 ) ) ;
#53307 = CARTESIAN_POINT ( 'NONE',  ( 2.309345278970798887, -0.4025885200794159235, 1.780468244869021222 ) ) ;
#53308 = CARTESIAN_POINT ( 'NONE',  ( -5.378281411895281749, 4.339595938922590435, 2.499999999999998668 ) ) ;
#53309 = CARTESIAN_POINT ( 'NONE',  ( 1.986440140746603911, -1.173720106059353396, 1.509789020923378189 ) ) ;
#53310 = CARTESIAN_POINT ( 'NONE',  ( 2.242574321144190641, -1.930940592676654965, -0.3871509593617681322 ) ) ;
#53311 = CARTESIAN_POINT ( 'NONE',  ( 4.265135581495039574, 1.882949608596860669, -0.4750026310351186387 ) ) ;
#53312 = CARTESIAN_POINT ( 'NONE',  ( -7.774674742793745708, 8.035151719539642912, 0.7998128361456341429 ) ) ;
#53314 = CARTESIAN_POINT ( 'NONE',  ( 4.236665939827915395, 1.302216991916404387, -1.673619383358643908 ) ) ;
#53313 = CARTESIAN_POINT ( 'NONE',  ( 6.481679955784983349, 9.719654494127929922, -1.199719254218452047 ) ) ;
#53315 = CARTESIAN_POINT ( 'NONE',  ( 6.576431128232845147, -6.604036961759876867, 7.015831072854276762 ) ) ;
#53316 = CARTESIAN_POINT ( 'NONE',  ( 9.206149998879153529, 10.69926207256923689, 1.199719254218453823 ) ) ;
#53317 = CARTESIAN_POINT ( 'NONE',  ( 6.067817914410090552, 6.045155426100865981, -0.3955105627355664510 ) ) ;
#53318 = LINE ( 'NONE', #264, #28593 ) ;
#53319 = ORIENTED_EDGE ( 'NONE', *, *, #37763, .T. ) ;
#53320 = CARTESIAN_POINT ( 'NONE',  ( 7.700104897918568447, 7.948153567185284096, 0.000000000000000000 ) ) ;
#53321 = CARTESIAN_POINT ( 'NONE',  ( 11.94105721237523277, 12.69999999999999929, -1.187919463087248939 ) ) ;
#53322 = CARTESIAN_POINT ( 'NONE',  ( 3.527797039230845311, -1.088449851438414218, -1.465592618984489670 ) ) ;
#53323 = DIRECTION ( 'NONE',  ( 0.000000000000000000, 0.000000000000000000, 1.000000000000000000 ) ) ;
#53324 = CARTESIAN_POINT ( 'NONE',  ( -9.341204650135658483, 10.00041963468749984, 1.040834085586084257E-14 ) ) ;
#53325 = CARTESIAN_POINT ( 'NONE',  ( -4.681723370323557454, 8.380211346474826684, 0.6239904028470877329 ) ) ;
#53326 = CARTESIAN_POINT ( 'NONE',  ( 3.680326755797796778, 6.126960397039161066, -1.194586299139585694 ) ) ;
#53327 = CARTESIAN_POINT ( 'NONE',  ( 4.873830839387755631, 1.077430855447782942, 1.529020332772989210 ) ) ;
#53328 = CARTESIAN_POINT ( 'NONE',  ( 6.577677080924314801, 10.82570702772039262, 1.040834085586084257E-14 ) ) ;
#53329 = CARTESIAN_POINT ( 'NONE',  ( 1.770020429662170658, 0.9901332625182661662, 1.652458556229096320 ) ) ;
#53330 = CARTESIAN_POINT ( 'NONE',  ( 6.297705697576845729, -1.418553083497756884, -1.355282376159852475 ) ) ;
#53331 = CARTESIAN_POINT ( 'NONE',  ( 3.785751206713845018, 5.439795712631356750, 1.599625672291267398 ) ) ;
#53332 = CARTESIAN_POINT ( 'NONE',  ( 1.364683531250000303, 9.567708333674735499, -0.7879004041258355073 ) ) ;
#53333 = CARTESIAN_POINT ( 'NONE',  ( -6.226218857173722476, 8.287007971501239467, 1.599625672291283607 ) ) ;
#53334 = CARTESIAN_POINT ( 'NONE',  ( 2.171277156482887882, 5.684907115872006145, -0.7998128361456291469 ) ) ;
#53335 = CARTESIAN_POINT ( 'NONE',  ( -3.757017964318317471, 6.436919154129725484, 1.082531754730549967 ) ) ;
#53336 = CARTESIAN_POINT ( 'NONE',  ( 1.388444276177196235, -0.7657061372807508759, -1.974083799386998406 ) ) ;
#53337 = CIRCLE ( 'NONE', #143371, 11.92000000000000171 ) ;
#53338 = DIRECTION ( 'NONE',  ( 1.000000000000000000, -7.771561172376096769E-16, -4.440892098500627148E-16 ) ) ;
#53339 = CARTESIAN_POINT ( 'NONE',  ( -2.246985366954051155, 2.726529103553844813, 2.500000000000000444 ) ) ;
#53340 = CARTESIAN_POINT ( 'NONE',  ( 6.069205674026176389, 1.823072449729469247, 0.9810699074010442722 ) ) ;
#53342 = CARTESIAN_POINT ( 'NONE',  ( 4.176068722599148408, 7.364853391560295393, -0.8050483301465498620 ) ) ;
#53341 = CARTESIAN_POINT ( 'NONE',  ( 0.8898994657863326108, -0.4472179738511591895, -1.785967584704901912 ) ) ;
#53343 = CARTESIAN_POINT ( 'NONE',  ( 6.223268877717999636, 2.273007049229976761, 0.3419319510214839930 ) ) ;
#53344 = CARTESIAN_POINT ( 'NONE',  ( 5.504247177468175600, 8.405076892812779477, 1.082531754730558626 ) ) ;
#53346 = FILL_AREA_STYLE_COLOUR ( '', #77413 ) ;
#53345 = CARTESIAN_POINT ( 'NONE',  ( 5.397554552016228691, 5.469770863539975991, 0.7216878364870328300 ) ) ;
#53347 = CARTESIAN_POINT ( 'NONE',  ( 1.289493641233057319, 1.738593318175378766, 1.494007209952723958 ) ) ;
#53348 = CARTESIAN_POINT ( 'NONE',  ( 0.3282377607281172782, 0.4263354503153867214, -1.225000000000017852 ) ) ;
#53349 = CARTESIAN_POINT ( 'NONE',  ( -4.936050443827081580, 7.916420063510339666, 1.199719254218452935 ) ) ;
#53350 = CARTESIAN_POINT ( 'NONE',  ( 5.876890087061106271, 1.793433424740819904, -0.7452851482259108540 ) ) ;
#53351 = ORIENTED_EDGE ( 'NONE', *, *, #94831, .F. ) ;
#53352 = CARTESIAN_POINT ( 'NONE',  ( 8.880227426826646564, 9.462612874160329923, 0.7216878364870458196 ) ) ;
#53353 = CARTESIAN_POINT ( 'NONE',  ( 0.2990880961862537601, -0.2507095357664780866, -1.997497332983847906 ) ) ;
#53355 = FACE_OUTER_BOUND ( 'NONE', #143186, .T. ) ;
#53354 = CARTESIAN_POINT ( 'NONE',  ( -7.181014916732457287, 11.52960116949655678, -0.7998128361456291469 ) ) ;
#53356 = CARTESIAN_POINT ( 'NONE',  ( -9.470186914265017464, 4.005096909781187264, 6.837150237413082365 ) ) ;
#53358 = CARTESIAN_POINT ( 'NONE',  ( 0.9183970251232485005, 1.633131562045697649, 0.6825882272994202582 ) ) ;
#53357 = CARTESIAN_POINT ( 'NONE',  ( 3.029325995398450821, -1.404573224648179242, -1.548692548079745546 ) ) ;
#53359 = CARTESIAN_POINT ( 'NONE',  ( 4.145001782281397595, 7.224479003952448686, 1.099888014807400616 ) ) ;
#53360 = ADVANCED_FACE ( 'NONE', ( #179010 ), #201475, .T. ) ;
#53362 = CARTESIAN_POINT ( 'NONE',  ( 3.996227152750064349, -0.7175114184741685497, -2.177131142417339849 ) ) ;
#53361 = CARTESIAN_POINT ( 'NONE',  ( 4.869313445963426190, 5.709895770826003414, 1.199719254218452935 ) ) ;
#53363 = CARTESIAN_POINT ( 'NONE',  ( 3.644249385861945800, -1.421566135898670646, 1.003629588703761621 ) ) ;
#53364 = CARTESIAN_POINT ( 'NONE',  ( 10.40318394038753702, 11.03146944007395724, -0.7998128361456281477 ) ) ;
#53365 = CARTESIAN_POINT ( 'NONE',  ( 5.896870467300973750, 5.844380064798101237, 0.7998128361456350310 ) ) ;
#53366 = CARTESIAN_POINT ( 'NONE',  ( 3.426783358884141428, 0.7772304037446680081, 1.549921577765429825 ) ) ;
#53367 = CARTESIAN_POINT ( 'NONE',  ( 4.106061665437168884, 0.7349691374628541940, -2.043110004675054103 ) ) ;
#53368 = CARTESIAN_POINT ( 'NONE',  ( 3.714044015139744914, 6.420469553383295391, 1.199719254218462483 ) ) ;
#53369 = CARTESIAN_POINT ( 'NONE',  ( 4.874232570624013050, -2.001857581374043349, -0.2420344392276354561 ) ) ;
#53370 = CARTESIAN_POINT ( 'NONE',  ( 3.437500000000002665, 1.451031289060976448, -1.451031289061255780 ) ) ;
#53371 = CARTESIAN_POINT ( 'NONE',  ( -1.201851678989727383E-14, 4.118750000682818602, -1.732050807568863648 ) ) ;
#53372 = CARTESIAN_POINT ( 'NONE',  ( 1.975490806028988633, 1.844176287694970995, -0.5568081592420818238 ) ) ;
#53373 = CARTESIAN_POINT ( 'NONE',  ( -1.500000000000008216, 9.031250000682797818, 3.469446951953614189E-15 ) ) ;
#53374 = CARTESIAN_POINT ( 'NONE',  ( 4.359788498249434596, -1.718402401499378840, -1.407797849641032828 ) ) ;
#53375 = EDGE_LOOP ( 'NONE', ( #7160, #91801, #165974, #75771 ) ) ;
#53376 = CARTESIAN_POINT ( 'NONE',  ( -0.2108831679770961920, 2.882544375557041239, -2.385815782126240236 ) ) ;
#53377 = CARTESIAN_POINT ( 'NONE',  ( -1.500000000000013101, 1.629166666666691077, -0.8660254037844313801 ) ) ;
#53378 = CARTESIAN_POINT ( 'NONE',  ( 6.582647274634798151, 7.638508894284114170, 1.199719254218462483 ) ) ;
#53379 = CARTESIAN_POINT ( 'NONE',  ( 3.321384445223597659, 6.818772919495430074, -0.7216878364870267237 ) ) ;
#53380 = CARTESIAN_POINT ( 'NONE',  ( -3.285556943749998737, -2.530208332855374831, 1.896917185911908721 ) ) ;
#53381 = CARTESIAN_POINT ( 'NONE',  ( 0.4521970297205242240, -1.575145348204033180, -1.566492488853583387 ) ) ;
#53382 = CARTESIAN_POINT ( 'NONE',  ( 5.547302793442128177, 1.730978599593002043, -0.9233319674036490898 ) ) ;
#53383 = CARTESIAN_POINT ( 'NONE',  ( 8.514157279702022407, 10.95626946445095307, -1.443375672974063439 ) ) ;
#53384 = CARTESIAN_POINT ( 'NONE',  ( 6.643838010208884981, 0.8751278368869718216, -2.086507859592637626 ) ) ;
#53385 = CARTESIAN_POINT ( 'NONE',  ( 5.499767588998890844, 6.445425604367387429, 1.199719254218451159 ) ) ;
#53386 = CARTESIAN_POINT ( 'NONE',  ( -3.675669043080673770, 7.302381293653823491, 0.000000000000000000 ) ) ;
#53387 = CARTESIAN_POINT ( 'NONE',  ( 3.174340740746087075, -1.014436240984006865, -1.795896229016210821 ) ) ;
#53388 = CARTESIAN_POINT ( 'NONE',  ( -5.590039407536138150, 5.416134151747256986, 0.000000000000000000 ) ) ;
#53389 = CARTESIAN_POINT ( 'NONE',  ( -1.500000000000011324, 3.452083334016151639, 0.8660254037844403729 ) ) ;
#53390 = CARTESIAN_POINT ( 'NONE',  ( -0.6823417656249969321, 5.280208333674756283, -1.181850606188749264 ) ) ;
#53391 = CARTESIAN_POINT ( 'NONE',  ( 5.536355731483205922, 1.842701317132239724, 0.3206550288221421963 ) ) ;
#53392 = CARTESIAN_POINT ( 'NONE',  ( 4.183993884235046146, 1.395953275470160682, 1.028640563475995640 ) ) ;
#53393 = CARTESIAN_POINT ( 'NONE',  ( 3.245385237338119566, 1.740626721681370670, -0.003331538806947489072 ) ) ;
#53394 = CARTESIAN_POINT ( 'NONE',  ( 2.173718093399327422, 1.413494431062709333, 1.804626757829434380 ) ) ;
#53395 = CARTESIAN_POINT ( 'NONE',  ( 1.364683531249988535, 3.926041667008087543, 0.7879004041258500513 ) ) ;
#53396 = CARTESIAN_POINT ( 'NONE',  ( 5.267163683669145335, 2.014557126142228594, -0.5589344999666242542 ) ) ;
#53397 = CARTESIAN_POINT ( 'NONE',  ( 6.492136518976993287, -0.5202676277693082385, -1.870896455867506747 ) ) ;
#53398 = DIRECTION ( 'NONE',  ( 0.000000000000000000, 0.000000000000000000, 1.000000000000000000 ) ) ;
#53399 = FILL_AREA_STYLE_COLOUR ( '', #190373 ) ;
#53400 = CARTESIAN_POINT ( 'NONE',  ( 1.406875202279284753, -1.122500148236497575, -1.674886495921081631 ) ) ;
#53401 = CARTESIAN_POINT ( 'NONE',  ( 0.2874129202556953144, 1.626693421326959710, 1.468627725614686463 ) ) ;
#53402 = CARTESIAN_POINT ( 'NONE',  ( 8.111888149748871513, 13.89538954745913912, -9.737069523379568992 ) ) ;
#53403 = CARTESIAN_POINT ( 'NONE',  ( -7.004758919754800139, 11.32396917302262018, 0.000000000000000000 ) ) ;
#53404 = CARTESIAN_POINT ( 'NONE',  ( 5.133733721068893807, 9.141106441222381918, 1.040834085586084257E-14 ) ) ;
#53405 = CARTESIAN_POINT ( 'NONE',  ( 2.737105750116640923, 1.997451989420237606, 0.7121958652205606644 ) ) ;
#53406 = CARTESIAN_POINT ( 'NONE',  ( -3.894033820048823813, 8.999999999999998224, -0.7749999999999979128 ) ) ;
#53407 = CARTESIAN_POINT ( 'NONE',  ( 5.672426548614882158, -1.154804106291613675, 1.414059844683832834 ) ) ;
#53408 = VERTEX_POINT ( 'NONE', #65216 ) ;
#53409 = CARTESIAN_POINT ( 'NONE',  ( -5.661411662158206681, 8.762674818229999829, -1.199719254218452047 ) ) ;
#53410 = CIRCLE ( 'NONE', #105394, 0.08000000000000040412 ) ;
#53411 = CARTESIAN_POINT ( 'NONE',  ( 0.000000000000000000, 0.9200000000000041478, 0.000000000000000000 ) ) ;
#53412 = CARTESIAN_POINT ( 'NONE',  ( -3.475000000000000533, -3.806249999044084564, 0.000000000000000000 ) ) ;
#53413 = CARTESIAN_POINT ( 'NONE',  ( -6.938021921891187382, 9.117444880338284818, -1.599625672291263179 ) ) ;
#53414 = CARTESIAN_POINT ( 'NONE',  ( 2.092062652781300880, 1.246029564253118282, 1.589516146451919631 ) ) ;
#53415 = CARTESIAN_POINT ( 'NONE',  ( 0.2179827029432715169, -2.065224962065722369, 0.4112614876821736321 ) ) ;
#53416 = CARTESIAN_POINT ( 'NONE',  ( 10.71502147350184231, 11.39527989537399755, 0.000000000000000000 ) ) ;
#53417 = CARTESIAN_POINT ( 'NONE',  ( 4.135495018730405370, 1.753490048523008049, -0.6236645969141580981 ) ) ;
#53418 = CARTESIAN_POINT ( 'NONE',  ( 9.725276259704228821, 10.24057714594344048, 0.7998128361456462443 ) ) ;
#53419 = CARTESIAN_POINT ( 'NONE',  ( 11.84104725192624130, 13.60983537451419778, -1.443823348526961814 ) ) ;
#53420 = ORIENTED_EDGE ( 'NONE', *, *, #39019, .T. ) ;
#53421 = CARTESIAN_POINT ( 'NONE',  ( -5.115504031057831469, 4.862509545855891346, 0.7998128361456341429 ) ) ;
#53422 = CARTESIAN_POINT ( 'NONE',  ( -7.832860060393135093, 10.16142270859057462, 1.599625672291295375 ) ) ;
#53423 = CARTESIAN_POINT ( 'NONE',  ( 5.531824841778981927, -1.161409778037244100, -1.408645805323349487 ) ) ;
#53425 = CARTESIAN_POINT ( 'NONE',  ( -3.985474048508588663, 7.835680043367737824, -0.2278754907324483936 ) ) ;
#53424 = CARTESIAN_POINT ( 'NONE',  ( -7.096767062110449942, 7.244259425409119046, -0.7998128361456362523 ) ) ;
#53426 = CARTESIAN_POINT ( 'NONE',  ( -1.402160292154681736E-14, -1.178124999658576311, 1.575800808251672791 ) ) ;
#53427 = CARTESIAN_POINT ( 'NONE',  ( 1.317307599089176939, -1.370793471230176808, 1.061547382435957587 ) ) ;
#53428 = CARTESIAN_POINT ( 'NONE',  ( 6.439398882927052981, 0.6998097629446423662, -1.703160347957879850 ) ) ;
#53430 = CARTESIAN_POINT ( 'NONE',  ( 7.280365300858406385, 11.43758391773608984, 1.040834085586084257E-14 ) ) ;
#53429 = CARTESIAN_POINT ( 'NONE',  ( 6.041700318104039624, -1.667111694969125368, -1.595929347687746747 ) ) ;
#53431 = CARTESIAN_POINT ( 'NONE',  ( -10.52284260640670688, 5.420240069097000735, -5.071998063130033430 ) ) ;
#53432 = CARTESIAN_POINT ( 'NONE',  ( 1.106794710556399997, 1.562239816646590285, -1.344093658231941824 ) ) ;
#53433 = CARTESIAN_POINT ( 'NONE',  ( 5.575427483717746213, 7.527751369135936343, 1.599625672291267398 ) ) ;
#53434 = CARTESIAN_POINT ( 'NONE',  ( 0.5970295589228531430, 1.038836743281198238, -1.727736137786803461 ) ) ;
#53435 = CARTESIAN_POINT ( 'NONE',  ( 7.978204059565677575, 15.27351506021529381, -8.905885731102706870 ) ) ;
#53437 = TOROIDAL_SURFACE ( 'NONE', #95060, 0.8299999999999999600, 0.08000000000000000167 ) ;
#53436 = CARTESIAN_POINT ( 'NONE',  ( -6.557303570864871034, 7.679217583210999010, -1.199719254218452047 ) ) ;
#53438 = CARTESIAN_POINT ( 'NONE',  ( 0.1277242839827036902, -1.211146277544056460, -1.556326691921037675 ) ) ;
#53439 = COLOUR_RGB ( '', 0.66274510, 0.83137255, 0.94901961) ;
#53441 = CARTESIAN_POINT ( 'NONE',  ( -4.146814880933400005, 5.931313009212638931, 1.599625672291270506 ) ) ;
#53440 = CARTESIAN_POINT ( 'NONE',  ( 3.392734571251673881, -1.844325299564765652, -0.5055192353106837677 ) ) ;
#53442 = CARTESIAN_POINT ( 'NONE',  ( 5.373716497573798101, 2.127666891504222058, -0.5857064233696291922 ) ) ;
#53443 = CARTESIAN_POINT ( 'NONE',  ( -1.225000000000044276, 1.791666667349484321, -0.7072540797573277915 ) ) ;
#53444 = CARTESIAN_POINT ( 'NONE',  ( -7.892254816486440561, 8.380254505421877553, 0.000000000000000000 ) ) ;
#53445 = CARTESIAN_POINT ( 'NONE',  ( 4.868786560638889149, 6.773613302202437403, 1.443375672974065660 ) ) ;
#53446 = CARTESIAN_POINT ( 'NONE',  ( -4.963693635934603776, 4.963599794778024155, 0.000000000000000000 ) ) ;
#53447 = CARTESIAN_POINT ( 'NONE',  ( 5.988958055669808545, -2.013456733998910231, -0.6654305520411086805 ) ) ;
#53448 = VERTEX_POINT ( 'NONE', #163824 ) ;
#53449 = CARTESIAN_POINT ( 'NONE',  ( 3.118547318853508887, -1.136067310315771905, -2.008477146686512782 ) ) ;
#53450 = CARTESIAN_POINT ( 'NONE',  ( 4.228923158279327410, -1.829750178516520442, -0.7082015076659909925 ) ) ;
#53451 = CARTESIAN_POINT ( 'NONE',  ( 7.721398836998401904, -6.134628647623499909, 7.721398836998376147 ) ) ;
#53452 = CARTESIAN_POINT ( 'NONE',  ( 0.6374591745182572877, 1.832550977151351290, -0.7006947966294306829 ) ) ;
#53453 = CARTESIAN_POINT ( 'NONE',  ( 1.387358672531703974, 7.315968950352358391, 4.254625267140708544 ) ) ;
#53454 = CARTESIAN_POINT ( 'NONE',  ( 0.07933194154555710254, -7.215597533182092960, -9.499668754385616865 ) ) ;
#53456 = ORIENTED_EDGE ( 'NONE', *, *, #113684, .F. ) ;
#53455 = B_SPLINE_CURVE_WITH_KNOTS ( 'NONE', 3,
 ( #26047, #73742, #157147, #124718, #175527, #24984 ),
 .UNSPECIFIED., .F., .F.,
 ( 4, 2, 4 ),
 ( 0.000000000000000000, 0.001226111284895916101, 0.002452222569791831768 ),
 .UNSPECIFIED. ) ;
#53457 = CARTESIAN_POINT ( 'NONE',  ( 5.823453932400854960, -1.463924103857511039, -1.387103351090559711 ) ) ;
#53458 = CARTESIAN_POINT ( 'NONE',  ( -7.971304249830880373, 11.38727316052296601, 1.199719254218453823 ) ) ;
#53460 = CARTESIAN_POINT ( 'NONE',  ( -15.75000000000000000, 9.799999999999982947, 3.199999999999997957 ) ) ;
#53459 = CIRCLE ( 'NONE', #126215, 1.250000000000000222 ) ;
#53461 = CARTESIAN_POINT ( 'NONE',  ( 3.661125528703466525, 1.714762188600306825, -1.331539952715065978 ) ) ;
#53462 = CARTESIAN_POINT ( 'NONE',  ( -0.4141348083894534349, 3.002424519313423801, 1.957929617241564335 ) ) ;
#53463 = CARTESIAN_POINT ( 'NONE',  ( 0.5805319366703353134, 1.050441701016215923, 1.842106252469346117 ) ) ;
#53464 = CARTESIAN_POINT ( 'NONE',  ( 1.499999999999989120, 2.285416667349482012, 0.8660254037844524744 ) ) ;
#53465 = CARTESIAN_POINT ( 'NONE',  ( 10.55232363013785246, 11.20546574478267132, 0.000000000000000000 ) ) ;
#53466 = CARTESIAN_POINT ( 'NONE',  ( 11.94651559118242901, 13.65130655878981791, -1.135242698369562042 ) ) ;
#53467 = CARTESIAN_POINT ( 'NONE',  ( 6.272253174914359519, 6.990222103910356921, -0.9563742486745248073 ) ) ;
#53468 = CARTESIAN_POINT ( 'NONE',  ( 1.634131612217240681, 1.018193428692963698, -1.791617596397138801 ) ) ;
#53470 = DIRECTION ( 'NONE',  ( -0.7592566023653017915, -0.6507913734559624963, 9.298211678181604981E-17 ) ) ;
#53469 = CARTESIAN_POINT ( 'NONE',  ( -10.47775378526269918, 11.11846759242831872, -0.7998128361456221525 ) ) ;
#53471 = CARTESIAN_POINT ( 'NONE',  ( -1.364683531250000748, 2.259375000341422357, 1.214306433183764966E-14 ) ) ;
#53472 = CARTESIAN_POINT ( 'NONE',  ( 0.000000000000000000, 13.88000000000000078, 0.000000000000000000 ) ) ;
#53473 = ORIENTED_EDGE ( 'NONE', *, *, #36152, .T. ) ;
#53474 = CARTESIAN_POINT ( 'NONE',  ( 4.951771945676144426, -1.355037094400749487, -1.349591858340569717 ) ) ;
#53475 = CARTESIAN_POINT ( 'NONE',  ( 11.81907076198602802, 12.34268775403521623, -1.592066415281268243 ) ) ;
#53476 = VECTOR ( 'NONE', #108209, 1000.000000000000000 ) ;
#53477 = CARTESIAN_POINT ( 'NONE',  ( -2.266184231778562541, 5.795632037050281404, 1.040834085586084257E-14 ) ) ;
#53478 = CARTESIAN_POINT ( 'NONE',  ( -0.1407840215364779823, -1.400018645128609629, -1.149511601580233577 ) ) ;
#53480 = CARTESIAN_POINT ( 'NONE',  ( 0.3037315811481311467, -1.027229472348114347, -1.616837036282785078 ) ) ;
#53479 = CARTESIAN_POINT ( 'NONE',  ( 7.712474369503348193, -6.289226506789209914, 7.712474369503325100 ) ) ;
#53481 = CARTESIAN_POINT ( 'NONE',  ( 1.891162872569674080, 0.2007839719405465906, 2.060584128686280714 ) ) ;
#53482 = CARTESIAN_POINT ( 'NONE',  ( 0.6823417656249882723, 0.4052083336747516751, 1.181850606188755259 ) ) ;
#53483 = CARTESIAN_POINT ( 'NONE',  ( 0.3738188115672124168, 1.133047686669987675, 1.613170723887060065 ) ) ;
#53484 = CARTESIAN_POINT ( 'NONE',  ( 2.965264444195826243, 0.2674972279559268973, -1.805858685475017378 ) ) ;
#53486 = CARTESIAN_POINT ( 'NONE',  ( 6.086061792568233209, 7.019478939793144967, 0.9900148145245997178 ) ) ;
#53485 = CARTESIAN_POINT ( 'NONE',  ( 0.1535068347273665368, -1.849414538273885578, 1.380102022147772667 ) ) ;
#53487 = EDGE_CURVE ( 'NONE', #69637, #19069, #77036, .T. ) ;
#53488 = CARTESIAN_POINT ( 'NONE',  ( -0.6823417656250212460, 2.051041667008083991, 1.181850606188767472 ) ) ;
#53489 = CARTESIAN_POINT ( 'NONE',  ( 4.229007335028351910, -1.923526752047514110, -0.7451934795693700986 ) ) ;
#53490 = CARTESIAN_POINT ( 'NONE',  ( -6.388916700537716764, 8.476822122092563916, 1.599625672291283607 ) ) ;
#53491 = CARTESIAN_POINT ( 'NONE',  ( 7.588813295347141441, 9.876701482703580837, -1.599625672291262513 ) ) ;
#53492 = DIRECTION ( 'NONE',  ( -1.000000000000000000, 0.000000000000000000, 0.000000000000000000 ) ) ;
#53493 = CARTESIAN_POINT ( 'NONE',  ( 4.008406971134620633, 7.828225232965717595, 0.7998128361456321445 ) ) ;
#53496 = CARTESIAN_POINT ( 'NONE',  ( 0.7499999999999885647, 3.566666666666690411, -1.299038105676658228 ) ) ;
#53495 = MECHANICAL_DESIGN_GEOMETRIC_PRESENTATION_REPRESENTATION (  '', ( #39728 ), #181641 ) ;
#53494 = CARTESIAN_POINT ( 'NONE',  ( 5.596739085487917542, -0.5086175864091507792, -2.043493955398622219 ) ) ;
#53497 = CARTESIAN_POINT ( 'NONE',  ( 0.2214384409217939054, -1.939739064610836339, -0.9756505802681545436 ) ) ;
#53498 = CARTESIAN_POINT ( 'NONE',  ( -0.6823417656250003738, 2.030208333674753174, -1.181850606188749264 ) ) ;
#53499 = CARTESIAN_POINT ( 'NONE',  ( 3.444745247808535638, 0.5215555581963465803, 2.097624034931542703 ) ) ;
#53500 = CARTESIAN_POINT ( 'NONE',  ( 4.336585317048437638, 1.240917556630851237, -1.593414756171371183 ) ) ;
#53501 = FACE_OUTER_BOUND ( 'NONE', #213478, .T. ) ;
#53503 = EDGE_CURVE ( 'NONE', #187284, #175139, #133478, .T. ) ;
#53502 = VECTOR ( 'NONE', #172165, 1000.000000000000000 ) ;
#53506 = CARTESIAN_POINT ( 'NONE',  ( 5.178851490740196795, 7.065079377328788546, 1.443375672974062551 ) ) ;
#53505 = CARTESIAN_POINT ( 'NONE',  ( 1.642778471875000035, -4.076041666188710444, -2.845375778867859751 ) ) ;
#53504 = CARTESIAN_POINT ( 'NONE',  ( -0.4000000000000236144, -3.469446951953614189E-14, -3.989863994746656317E-14 ) ) ;
#53507 = CARTESIAN_POINT ( 'NONE',  ( -6.629010762438975135, 6.698543742459062145, -0.7998128361456362523 ) ) ;
#53508 = CARTESIAN_POINT ( 'NONE',  ( 1.956267901341804283, -1.236798062192035363, 1.592663274815858676 ) ) ;
#53509 = CARTESIAN_POINT ( 'NONE',  ( -8.422639742587602285, 10.84949900448412841, -1.599625672291263179 ) ) ;
#53511 = CARTESIAN_POINT ( 'NONE',  ( -4.292360784660903761, 7.401453155497748959, -1.060140167543128564 ) ) ;
#53510 = CARTESIAN_POINT ( 'NONE',  ( -5.264643720808155791, 5.036505850564608089, 0.000000000000000000 ) ) ;
#53512 = DIRECTION ( 'NONE',  ( 0.000000000000000000, 0.000000000000000000, -1.000000000000000000 ) ) ;
#53513 = SURFACE_STYLE_USAGE ( .BOTH. , #51393 ) ;
#53514 = CARTESIAN_POINT ( 'NONE',  ( -10.99768633959234521, 5.378919375605944353, -4.807944750716973026 ) ) ;
#53516 = CARTESIAN_POINT ( 'NONE',  ( 4.411732571322396268, -1.242743209197882059, -1.587826168943158089 ) ) ;
#53515 = CARTESIAN_POINT ( 'NONE',  ( -7.415946836550729948, 9.675023947441092176, 1.443375672974090751 ) ) ;
#53517 = CARTESIAN_POINT ( 'NONE',  ( 1.499999999999987121, 4.795833333333353821, -0.8660254037844323793 ) ) ;
#53518 = CARTESIAN_POINT ( 'NONE',  ( 0.2402810872906081530, 0.2891477966728701610, 1.700304936625576024 ) ) ;
#53519 = CARTESIAN_POINT ( 'NONE',  ( 6.496291879603339758, 7.608037276739255006, 1.199719254218452935 ) ) ;
#53521 = CYLINDRICAL_SURFACE ( 'NONE', #163548, 1.500000000000000222 ) ;
#53520 = CARTESIAN_POINT ( 'NONE',  ( 7.619319141200051604, 11.83303006480134911, 0.7216878364870438212 ) ) ;
#53522 = CARTESIAN_POINT ( 'NONE',  ( 1.284279953904126748, 10.64264068711930733, -0.7749999999999874767 ) ) ;
#53523 = CARTESIAN_POINT ( 'NONE',  ( 5.800035319642947051, -1.870726058474009079, -0.0005997126256013227737 ) ) ;
#53524 = CARTESIAN_POINT ( 'NONE',  ( 0.1178376421791422907, -0.5346926475991298222, 1.940734443874014836 ) ) ;
#53525 = DIRECTION ( 'NONE',  ( 0.000000000000000000, 1.000000000000000000, 0.000000000000000000 ) ) ;
#53526 = CARTESIAN_POINT ( 'NONE',  ( -6.685579144870156476, 9.853573864773576219, 1.082531754730549967 ) ) ;
#53527 = EDGE_LOOP ( 'NONE', ( #92713, #68394, #30388, #70297 ) ) ;
#53528 = CARTESIAN_POINT ( 'NONE',  ( 10.53432216769390095, 11.39239007183880581, -0.7216878364870257245 ) ) ;
#53530 = ADVANCED_FACE ( 'NONE', ( #82544 ), #18606, .F. ) ;
#53529 = CARTESIAN_POINT ( 'NONE',  ( 1.194935658704935566, 1.779638138761422628, 0.9480210990304924756 ) ) ;
#53531 = CARTESIAN_POINT ( 'NONE',  ( 1.705023097204850346, 1.575028893885391579, -0.8949447657340557916 ) ) ;
#53532 = CARTESIAN_POINT ( 'NONE',  ( 5.356880090730874677, 5.422317325373725794, 0.7216878364870328300 ) ) ;
#53533 = CARTESIAN_POINT ( 'NONE',  ( -1.734723475976807094E-15, -6.134628647623513231, -10.91970695577494332 ) ) ;
#53534 = CARTESIAN_POINT ( 'NONE',  ( 7.226132685959389512, 11.37431253368722750, -0.7216878364870267237 ) ) ;
#53535 = CARTESIAN_POINT ( 'NONE',  ( 6.938021921891177612, 9.117444880338284818, -1.599625672291262513 ) ) ;
#53537 = CARTESIAN_POINT ( 'NONE',  ( 6.450803866275835574, -1.753708343991422502, -0.7711757456045026382 ) ) ;
#53536 = CARTESIAN_POINT ( 'NONE',  ( -5.199715606040888005, 6.025088614257851027, -1.199719254218446718 ) ) ;
#53538 = CARTESIAN_POINT ( 'NONE',  ( 1.887367962963598211, 8.990012987145949097, 0.7750000000000004663 ) ) ;
#53539 = CARTESIAN_POINT ( 'NONE',  ( -1.237941840313982578, 1.374772708486763806, 1.500000000000001332 ) ) ;
#53540 = CARTESIAN_POINT ( 'NONE',  ( 7.090551149822744925, 7.374657217655760100, 0.7216878364870317197 ) ) ;
#53541 = ADVANCED_FACE ( 'NONE', ( #196315 ), #212544, .F. ) ;
#53542 = CARTESIAN_POINT ( 'NONE',  ( 1.419999999999999485, 7.176846818246214177, 4.202462424328220258 ) ) ;
#53544 = ORIENTED_EDGE ( 'NONE', *, *, #137732, .F. ) ;
#53543 = CARTESIAN_POINT ( 'NONE',  ( 3.009546912553647147, 5.494593250412460606, -1.082531754730543083 ) ) ;
#53545 = CARTESIAN_POINT ( 'NONE',  ( -3.460355519985875983, 5.060167411448709629, 1.599625672291267398 ) ) ;
#53546 = CARTESIAN_POINT ( 'NONE',  ( 4.610339536224768331, -0.9213992672730474398, -1.955631277330005968 ) ) ;
#53547 = EDGE_CURVE ( 'NONE', #163622, #163559, #97765, .T. ) ;
#53548 = CARTESIAN_POINT ( 'NONE',  ( -5.790741006812557323, 9.769965251341050205, 0.000000000000000000 ) ) ;
#53549 = CARTESIAN_POINT ( 'NONE',  ( 6.048345925472183637, 8.149765894507963182, 1.443375672974065660 ) ) ;
#53550 = CARTESIAN_POINT ( 'NONE',  ( 0.2816890862925770511, 0.2015970107726860194, -2.110973810222869229 ) ) ;
#53551 = CARTESIAN_POINT ( 'NONE',  ( 5.754876975610782708, -1.437719105923901841, 1.124948175183659638 ) ) ;
#53552 = CARTESIAN_POINT ( 'NONE',  ( 1.985558396190547858, 1.356547016436062014, 1.430631702862941168 ) ) ;
#53553 = CARTESIAN_POINT ( 'NONE',  ( 4.166199421025416960, 1.911861072351704882, -0.05224187775455800542 ) ) ;
#53554 = VERTEX_POINT ( 'NONE', #147570 ) ;
#53555 = CARTESIAN_POINT ( 'NONE',  ( -6.116136693540540570, 10.14959355252369910, 0.000000000000000000 ) ) ;
#53556 = CARTESIAN_POINT ( 'NONE',  ( 6.092246201825009422, 0.9720536035879873138, -1.712898845271645820 ) ) ;
#53557 = CARTESIAN_POINT ( 'NONE',  ( 0.3923911919363164413, 1.615042221312415371, -1.078049841609552306 ) ) ;
#53558 = ORIENTED_EDGE ( 'NONE', *, *, #68305, .T. ) ;
#53559 = CARTESIAN_POINT ( 'NONE',  ( -5.157951095356222204, 4.982307464195829816, 0.000000000000000000 ) ) ;
#53561 = CARTESIAN_POINT ( 'NONE',  ( 6.864213375409820905, -6.776276029125531508, -6.558483974470185274 ) ) ;
#53560 = CARTESIAN_POINT ( 'NONE',  ( -5.008811405605897882, 4.808311159487113073, 0.7998128361456281477 ) ) ;
#53563 = CARTESIAN_POINT ( 'NONE',  ( 5.519577934094852978, 7.532869904567736974, 1.443375672974064550 ) ) ;
#53562 = CARTESIAN_POINT ( 'NONE',  ( 6.421758314367153275, 10.64380180007036891, -0.7998128361456291469 ) ) ;
#53565 = ORIENTED_EDGE ( 'NONE', *, *, #72633, .F. ) ;
#53564 = CARTESIAN_POINT ( 'NONE',  ( 4.705663775918221603, 1.419457463540532816, 1.281590252682027087 ) ) ;
#53566 = CARTESIAN_POINT ( 'NONE',  ( 0.9564373720404686363, 2.204146663617879476, -0.1098798544595935567 ) ) ;
#53567 = CARTESIAN_POINT ( 'NONE',  ( 1.506334365903699402, 8.679455619938613253, 2.541882285198393987 ) ) ;
#53568 = CARTESIAN_POINT ( 'NONE',  ( 6.498696042004469930, -1.974701156420979542, -0.3904368389309967324 ) ) ;
#53569 = B_SPLINE_CURVE_WITH_KNOTS ( 'NONE', 3,
 ( #153714, #150525, #87644, #22614, #137476, #203490, #120215, #121289 ),
 .UNSPECIFIED., .F., .F.,
 ( 4, 2, 2, 4 ),
 ( 3.127317220692750373E-18, 0.003096353334791364376, 0.004644530002187043961, 0.006192706669582723547 ),
 .UNSPECIFIED. ) ;
#53570 = CARTESIAN_POINT ( 'NONE',  ( -0.02338929933911031503, 1.420967854922173368, -1.971839201816010911 ) ) ;
#53571 = CARTESIAN_POINT ( 'NONE',  ( 10.99943592164172479, -8.240513804456435665, -0.1113975120798833818 ) ) ;
#53572 = LINE ( 'NONE', #85001, #54653 ) ;
#53573 = CARTESIAN_POINT ( 'NONE',  ( 3.209495720308676248, -1.691010085789945716, -1.194244797349801157 ) ) ;
#53574 = CARTESIAN_POINT ( 'NONE',  ( -5.412729640353771465, 7.337937218544611895, 1.599625672291269396 ) ) ;
#53575 = CARTESIAN_POINT ( 'NONE',  ( -4.620365152176808543, 8.363145938788004941, -0.2588828456067792660 ) ) ;
#53577 = CARTESIAN_POINT ( 'NONE',  ( 1.042116488573753497, 0.8753402851892390091, -1.976733581976031218 ) ) ;
#53576 = CARTESIAN_POINT ( 'NONE',  ( -3.578462479003122976, 6.262291094557191684, 1.199719254218464037 ) ) ;
#53578 = CARTESIAN_POINT ( 'NONE',  ( -11.40791084141324951, 7.888933430996066143, -3.732120612452610953 ) ) ;
#53579 =( NAMED_UNIT ( * ) SI_UNIT ( $, .STERADIAN. ) SOLID_ANGLE_UNIT ( ) );
#53580 = CARTESIAN_POINT ( 'NONE',  ( 3.602337597214539753E-15, 1.000000000682806034, -1.225000000000015410 ) ) ;
#53581 = CARTESIAN_POINT ( 'NONE',  ( -0.6823417656250003738, 12.96354166700806942, 1.181850606188754593 ) ) ;
#53583 = CARTESIAN_POINT ( 'NONE',  ( -6.642568916052639771, 6.714361588341672515, 0.000000000000000000 ) ) ;
#53582 = CARTESIAN_POINT ( 'NONE',  ( 6.825078400183573812, 0.002648415797040087893, 1.855566311045192540 ) ) ;
#53585 = CARTESIAN_POINT ( 'NONE',  ( 5.590364566445758854, -0.4131642248683431440, 1.684076740667529881 ) ) ;
#53584 = TOROIDAL_SURFACE ( 'NONE', #1764, 1.600000000000000311, 0.1000000000000000056 ) ;
#53586 = CARTESIAN_POINT ( 'NONE',  ( -4.613852347352193739, 4.277249248199312071, 1.214306433183764966E-14 ) ) ;
#53587 = CARTESIAN_POINT ( 'NONE',  ( 3.291909242638372923, -1.386922682245657734, -1.537212927083357217 ) ) ;
#53588 = CARTESIAN_POINT ( 'NONE',  ( 4.464542613241986757, -2.054094600764106548, -0.5127786416893320709 ) ) ;
#53589 = CIRCLE ( 'NONE', #188407, 8.500000000000000000 ) ;
#53590 = CARTESIAN_POINT ( 'NONE',  ( 5.615048174354031474, 9.702639970055050966, 0.7998128361456462443 ) ) ;
#53591 = CARTESIAN_POINT ( 'NONE',  ( 1.364683531249988535, 4.655208333674755394, -0.7879004041258300672 ) ) ;
#53592 = CARTESIAN_POINT ( 'NONE',  ( 2.694150338025066205, 0.9325801345280826382, -1.734679099899273824 ) ) ;
#53593 = CARTESIAN_POINT ( 'NONE',  ( 0.4922593472763935329, -1.060406550076501642, 1.591262010887870115 ) ) ;
#53594 = CARTESIAN_POINT ( 'NONE',  ( 5.191491443341288203, -0.8287821522852161227, 2.137368679509048963 ) ) ;
#53595 = CARTESIAN_POINT ( 'NONE',  ( 3.193790821891542286, -0.7392406677243366087, 1.669511829839696038 ) ) ;
#53596 = CARTESIAN_POINT ( 'NONE',  ( 5.662465432362883355, 6.635239754958710989, 1.199719254218451159 ) ) ;
#53597 = CARTESIAN_POINT ( 'NONE',  ( 5.056828107772846082, 6.922718763866881453, -1.443375672974051449 ) ) ;
#53598 = CARTESIAN_POINT ( 'NONE',  ( -5.208303565944065738, 9.228104593576741621, -0.7998128361456231517 ) ) ;
#53599 = CARTESIAN_POINT ( 'NONE',  ( 4.324480843662709795, -0.8647720088908043001, -1.818167814553457884 ) ) ;
#53600 =( BOUNDED_CURVE ( )  B_SPLINE_CURVE ( 2, ( #153524, #85309, #134099, #2965, #50675, #83163, #102636, #184926, #168693 ),
 .UNSPECIFIED., .F., .T. ) 
 B_SPLINE_CURVE_WITH_KNOTS ( ( 3, 2, 2, 2, 3 ),
 ( 0.9732142857142856984, 0.9761904761904761640, 0.9821428571428570953, 0.9880952380952381375, 0.9910714285714286031 ),
 .UNSPECIFIED. ) 
 CURVE ( )  GEOMETRIC_REPRESENTATION_ITEM ( )  RATIONAL_B_SPLINE_CURVE ( ( 0.9330127018922194093, 0.9330127018922194093, 1.000000000000000000, 0.8660254037844387076, 1.000000000000000000, 0.8660254037844387076, 1.000000000000000000, 0.9330127018922194093, 0.9330127018922194093 ) ) 
 REPRESENTATION_ITEM ( '' )  );
#53601 = CARTESIAN_POINT ( 'NONE',  ( 3.555471618195928496, 1.543666060651678551, 1.210462546525910010 ) ) ;
#53602 = CARTESIAN_POINT ( 'NONE',  ( -6.170932472514347289, 10.35117165124207972, 0.000000000000000000 ) ) ;
#53603 = CARTESIAN_POINT ( 'NONE',  ( -6.586563698140583512, 6.578745824119123675, 1.040834085586084257E-14 ) ) ;
#53604 = CARTESIAN_POINT ( 'NONE',  ( 1.526556658859585313E-16, 1.899999999999999023, -2.750000000000000000 ) ) ;
#53606 = CARTESIAN_POINT ( 'NONE',  ( 4.908955397393719444, 1.540865433829426090, 0.8705488387463419242 ) ) ;
#53605 = CARTESIAN_POINT ( 'NONE',  ( 6.193323979940683621, -0.7056316722037699884, 1.968093674265839477 ) ) ;
#53607 = FACE_OUTER_BOUND ( 'NONE', #84567, .T. ) ;
#53608 = EDGE_CURVE ( 'NONE', #44957, #121448, #111559, .T. ) ;
#53609 = CARTESIAN_POINT ( 'NONE',  ( 0.3752731597879420677, 2.043270790221253908, -0.7926104125151807178 ) ) ;
#53610 = CARTESIAN_POINT ( 'NONE',  ( 6.316323101372843141, 1.626595589989995982, 0.6193309307870945579 ) ) ;
#53611 = CARTESIAN_POINT ( 'NONE',  ( 6.252281394196331554, 10.44607872653774372, 1.040834085586084257E-14 ) ) ;
#53612 = CARTESIAN_POINT ( 'NONE',  ( 0.1333692844072559280, 6.947498546895843674, -2.648624074793118233 ) ) ;
#53613 = CARTESIAN_POINT ( 'NONE',  ( 0.5040132504689893711, -0.5763820916803040761, -1.625860608634047244 ) ) ;
#53614 =( BOUNDED_CURVE ( )  B_SPLINE_CURVE ( 3, ( #181139, #169154, #100945, #51145 ),
 .UNSPECIFIED., .F., .T. ) 
 B_SPLINE_CURVE_WITH_KNOTS ( ( 4, 4 ),
 ( 0.4999999999999957812, 1.000000000000000000 ),
 .UNSPECIFIED. ) 
 CURVE ( )  GEOMETRIC_REPRESENTATION_ITEM ( )  RATIONAL_B_SPLINE_CURVE ( ( 1.000000000000005773, 0.3333333333333334259, 0.3333333333333278192, 1.000000000000000222 ) ) 
 REPRESENTATION_ITEM ( '' )  );
#53615 = CARTESIAN_POINT ( 'NONE',  ( 0.9959476074029065540, -2.191739723303194332, 0.005169097091584088505 ) ) ;
#53616 = CARTESIAN_POINT ( 'NONE',  ( 2.684424123961434816, -1.133677649706768431, 1.893296980138805097 ) ) ;
#53617 = CARTESIAN_POINT ( 'NONE',  ( 6.707499178395360140, -1.739742505839674047, -1.298780901186733505 ) ) ;
#53618 = LINE ( 'NONE', #103438, #110380 ) ;
#53619 = CARTESIAN_POINT ( 'NONE',  ( 1.147838861943322630, 2.084982156806517661, -0.3680304603586990742 ) ) ;
#53621 = AXIS2_PLACEMENT_3D ( 'NONE', #100947, #37015, #152910 ) ;
#53620 = CARTESIAN_POINT ( 'NONE',  ( 3.625000000000002665, -2.052068128417946280, 2.068584262981140017E-13 ) ) ;
#53622 = CARTESIAN_POINT ( 'NONE',  ( 6.727182134110178069, 2.947419669445831669, 2.641212418657997496 ) ) ;
#53623 = CARTESIAN_POINT ( 'NONE',  ( 5.438475939130889891, 1.897888883619626821, 0.3293186976999362137 ) ) ;
#53624 = ORIENTED_EDGE ( 'NONE', *, *, #126049, .F. ) ;
#53626 = CARTESIAN_POINT ( 'NONE',  ( -0.7500000000000215383, 5.441666666666685082, 1.299038105676671107 ) ) ;
#53625 = CARTESIAN_POINT ( 'NONE',  ( 1.066458480799619135, -1.449176446249898831, 1.776219484066744903 ) ) ;
#53627 = CARTESIAN_POINT ( 'NONE',  ( 3.551346171775753735, 6.230655402791975384, 1.199719254218462483 ) ) ;
#53628 = CARTESIAN_POINT ( 'NONE',  ( 4.819033534653518025, 7.709623992816043270, -1.199719254218452047 ) ) ;
#53629 = CARTESIAN_POINT ( 'NONE',  ( 4.055513949679364849, -1.932427950605047018, 1.095304516859375799 ) ) ;
#53630 = CARTESIAN_POINT ( 'NONE',  ( -6.385527162356466668, 10.39360608948380182, 0.000000000000000000 ) ) ;
#53631 = CARTESIAN_POINT ( 'NONE',  ( 6.805829924380118356, 7.042482454639357847, 0.7216878364870317197 ) ) ;
#53632 = CARTESIAN_POINT ( 'NONE',  ( -7.171900071504729191, 11.31104115015678779, -0.7216878364870267237 ) ) ;
#53633 = CARTESIAN_POINT ( 'NONE',  ( 6.549997609177859559, 6.814287763561861944, 0.000000000000000000 ) ) ;
#53634 = CARTESIAN_POINT ( 'NONE',  ( 1.529922885524274134, -1.701946718671920600, 1.081067414773040802 ) ) ;
#53636 = CARTESIAN_POINT ( 'NONE',  ( 1.481379835429663228, -0.05473030402166743219, 2.062018025990194126 ) ) ;
#53635 = CARTESIAN_POINT ( 'NONE',  ( 6.913768267964901071, 10.15348118167935709, -1.199719254218441611 ) ) ;
#53637 =( LENGTH_UNIT ( ) NAMED_UNIT ( * ) SI_UNIT ( .MILLI., .METRE. ) );
#53638 = CARTESIAN_POINT ( 'NONE',  ( 5.194182247366861738, 9.073980031987776584, 0.7216878364870317197 ) ) ;
#53639 = CARTESIAN_POINT ( 'NONE',  ( 0.1515692981730529243, 0.7036590017722235135, 1.701685288394996665 ) ) ;
#53640 = CARTESIAN_POINT ( 'NONE',  ( 9.579665964935223599, -7.246166700194470067, 5.204170427930421283E-15 ) ) ;
#53641 = CARTESIAN_POINT ( 'NONE',  ( -1.364683531249997417, 2.509375000341422357, 1.214306433183764966E-14 ) ) ;
#53642 = CARTESIAN_POINT ( 'NONE',  ( 2.741159958678766717, -1.308340514575502045, -1.191892431489706805 ) ) ;
#53643 = CARTESIAN_POINT ( 'NONE',  ( 1.318982659667154334, 0.9913977828604101372, -1.755770081111128977 ) ) ;
#53644 = CARTESIAN_POINT ( 'NONE',  ( -0.05938221139379848412, -1.422385081007140117, -1.168950373246782526 ) ) ;
#53645 = CARTESIAN_POINT ( 'NONE',  ( 5.126663105998436443, 0.1666055143465100530, 2.286395203598155845 ) ) ;
#53646 = CARTESIAN_POINT ( 'NONE',  ( 3.732213890823964597, 0.2717154217161937280, 1.820854149191558635 ) ) ;
#53647 = ADVANCED_FACE ( 'NONE', ( #16464 ), #17524, .T. ) ;
#53648 = CARTESIAN_POINT ( 'NONE',  ( 7.072549687823125097, 11.40305840243567381, -0.7998128361456291469 ) ) ;
#53649 = CARTESIAN_POINT ( 'NONE',  ( 3.645350208285046634, -1.381898811119431691, -1.193016960613018096 ) ) ;
#53650 = CARTESIAN_POINT ( 'NONE',  ( 5.467422714486909641, -1.967887220244109558, -0.4390321945699494632 ) ) ;
#53651 = CARTESIAN_POINT ( 'NONE',  ( -7.655550293210764856, 12.08322577538792331, 0.000000000000000000 ) ) ;
#53653 = CARTESIAN_POINT ( 'NONE',  ( -5.447343857640614573, 9.577261277214532242, -0.7998128361456362523 ) ) ;
#53652 = CARTESIAN_POINT ( 'NONE',  ( 3.432755235230527280, 2.206939294067700619, 0.4977334550177249795 ) ) ;
#53654 = CARTESIAN_POINT ( 'NONE',  ( 0.1004013553109489865, -2.105664478878019441, -0.04916207707313274139 ) ) ;
#53655 = DIRECTION ( 'NONE',  ( 1.000000000000000000, -0.000000000000000000, -0.000000000000000000 ) ) ;
#53656 = CARTESIAN_POINT ( 'NONE',  ( 3.332542965736586371, -1.235447621225284509, 1.661183390374972424 ) ) ;
#53657 = CARTESIAN_POINT ( 'NONE',  ( 8.353795204314554468, 12.89784483834236184, -0.7998128361456352531 ) ) ;
#53658 = CARTESIAN_POINT ( 'NONE',  ( -1.360316468750036645, 1.901041667008058988, -0.7853790794159222211 ) ) ;
#53659 = CARTESIAN_POINT ( 'NONE',  ( 5.514351353798126354, -2.120667953778174741, 0.0001357579994532010219 ) ) ;
#53660 = SHAPE_DEFINITION_REPRESENTATION ( #159541, #142805 ) ;
#53662 = CARTESIAN_POINT ( 'NONE',  ( 2.016120517293042536, -0.9081000056256024466, -1.699051532819460197 ) ) ;
#53661 = CARTESIAN_POINT ( 'NONE',  ( -9.317477881089553549, 11.89347683273641820, 1.599625672291281386 ) ) ;
#53664 = UNCERTAINTY_MEASURE_WITH_UNIT (LENGTH_MEASURE( 1.000000000000000082E-05 ), #37696, 'distance_accuracy_value', 'NONE');
#53663 = B_SPLINE_CURVE_WITH_KNOTS ( 'NONE', 3,
 ( #34844, #148624, #191, #66260, #132408, #150766, #198410, #33790, #165932, #64177, #17517, #67326, #205077, #207225, #154220, #170457, #57783, #56719, #122887, #54582, #105494, #139050, #25274, #75104, #104408, #24190, #9030, #141215, #40482, #140129, #42627, #188846, #58849, #6869, #155287, #38331, #7948, #5792, #125005, #71869, #74038, #190962, #91376, #206155, #123944, #108737, #186703, #23119, #174765, #189912, #26338, #106585, #187768, #41557, #70799, #89236, #156363, #171526, #120730, #22042, #172614, #90293, #107670, #173698, #157436, #88152, #92452, #4724, #55645, #136912, #137978, #202939, #203996, #121801, #39399, #72948, #63119, #146536, #30635, #62062, #143343, #47968, #59911, #158491, #110868, #196324, #144418, #60986, #210420, #160619, #192029, #80437, #145488, #128217, #211483, #208280, #113009, #78292, #29561, #10090, #176873, #114084, #28485, #127139, #43692, #31698, #180075, #126067, #76164, #94576, #142269, #194179, #193111, #45824, #12220, #109809, #212555, #129284, #111945, #44760, #64194, #177947, #95653, #209337, #77224, #161703, #175818, #27411, #93509, #13296, #79369, #195259, #46894, #159550, #11147, #179018, #96720, #162769, #14347, #130335, #99886, #181127, #147581, #66277, #67342, #65225, #149703, #185381, #201613, #85761, #17532, #1284, #133487, #148641, #168083, #132425, #198426, #84695, #97773, #213599, #165948, #83621, #151841, #32748, #49013, #150782, #199490, #51135, #131375, #50072, #3418, #182179, #98830, #200552, #163833, #16474, #102014, #15412, #115132, #164880, #197371, #69484, #117257, #33807, #82554, #100934, #207, #19683, #116193, #167021, #183256, #135592, #118325, #18615, #2345, #53262, #34860, #68421, #119393, #134548, #81502, #52199, #184311, #35935, #157177, #56465, #4472, #153970, #152893, #120475, #156106, #6619, #72699, #204814, #122627, #70543, #206967, #57535, #87897, #55394, #173437, #155034, #137730, #71618, #172353, #5537, #8771, #188589, #136662, #203750, #202687, #186448, #7691, #138794, #40221, #106332, #23943, #54336, #58597, #123693, #121549, #189654, #38084, #187520, #124752, #37001, #39151, #73774, #140956, #105232, #171273, #104156, #103083, #169139, #170204, #20734, #22866, #74854, #88980, #90047, #139870, #21788, #86829, #205901, #25016, #41305, #107413, #91118, #14872, #159291, #175562, #109558, #93257, #75913, #42373, #9837, #76965, #27153, #143092, #10890, #92199, #66802, #163290, #130849, #48484, #158249, #142016, #65743, #59659, #26084, #209084, #80964, #208031, #31164, #190712, #83079, #181645, #113539, #97237, #147055, #63652, #47424, #129807, #131890, #108484, #179543, #195786, #191778, #213076, #33272, #125816, #43434, #32217, #64706, #196846, #114602, #180593, #99357, #98291, #164352, #82021, #15937, #197898, #49527, #148112, #214116, #17004, #115650, #165407, #149158, #736, #174508, #136129, #134018, #137202, #200025, #202144, #150245, #38620, #153440, #53804, #121022, #100409, #182716, #101476, #102544, #166478, #184842, #6088, #22334, #186989, #52724, #36471, #168608, #183790, #203225, #167547, #19146, #119934, #132943, #34334, #51677, #118857, #104697, #67871, #84158, #185910, #20210, #86298, #18070, #85221, #170748, #2878, #1813, #21264, #198948, #117798, #54869, #50591, #35398, #151310, #152367, #88448, #135070, #68948, #201083, #37545 ),
 .UNSPECIFIED., .F., .F.,
 ( 4, 1, 1, 1, 1, 1, 1, 1, 1, 1, 1, 1, 1, 1, 1, 1, 1, 1, 1, 1, 1, 1, 1, 1, 1, 1, 1, 1, 1, 1, 1, 1, 1, 1, 1, 1, 1, 1, 1, 1, 1, 1, 1, 1, 1, 1, 1, 1, 1, 1, 1, 1, 1, 1, 1, 1, 1, 1, 1, 1, 1, 1, 1, 1, 1, 1, 1, 1, 1, 1, 1, 1, 1, 1, 1, 1, 1, 1, 1, 1, 1, 1, 1, 1, 1, 1, 1, 1, 1, 1, 1, 1, 1, 1, 1, 1, 1, 1, 1, 1, 1, 1, 1, 1, 1, 1, 1, 1, 1, 1, 1, 1, 1, 1, 1, 1, 1, 1, 1, 1, 1, 1, 1, 1, 1, 1, 1, 1, 1, 1, 1, 1, 1, 1, 1, 1, 1, 1, 1, 1, 1, 1, 1, 1, 1, 1, 1, 1, 1, 1, 1, 1, 1, 1, 1, 1, 1, 1, 1, 1, 1, 1, 1, 1, 1, 1, 1, 1, 1, 1, 1, 1, 1, 1, 1, 1, 1, 1, 1, 1, 1, 1, 1, 1, 1, 1, 1, 1, 1, 1, 1, 1, 1, 1, 1, 1, 1, 1, 1, 1, 1, 1, 1, 1, 1, 1, 1, 1, 1, 1, 1, 1, 1, 1, 1, 1, 1, 1, 1, 1, 1, 1, 1, 1, 1, 1, 1, 1, 1, 1, 1, 1, 1, 1, 1, 1, 1, 1, 1, 1, 1, 1, 1, 1, 1, 1, 1, 1, 1, 1, 1, 1, 1, 1, 1, 1, 1, 1, 1, 1, 1, 1, 1, 1, 1, 1, 1, 1, 1, 1, 1, 1, 1, 1, 1, 1, 1, 1, 1, 1, 1, 1, 1, 1, 1, 1, 1, 1, 1, 1, 1, 1, 1, 1, 1, 1, 1, 1, 1, 1, 1, 1, 1, 1, 1, 1, 1, 1, 1, 1, 1, 1, 1, 1, 1, 1, 1, 1, 1, 1, 1, 1, 1, 1, 1, 1, 1, 1, 1, 1, 1, 1, 1, 1, 1, 1, 1, 1, 1, 1, 1, 1, 1, 1, 1, 1, 1, 1, 1, 1, 1, 1, 1, 1, 1, 1, 1, 1, 1, 1, 1, 1, 1, 1, 1, 1, 1, 1, 1, 1, 1, 1, 1, 1, 1, 1, 1, 1, 1, 1, 1, 1, 1, 1, 4 ),
 ( 0.000000000000000000, 0.002600137934918278840, 0.005208846947063642402, 0.007813284371963545236, 0.01041597565644012714, 0.01302123463190214131, 0.01562472912267370319, 0.01822934229245065652, 0.02083335053635077330, 0.02343730581734793095, 0.02604195799539401474, 0.02864545692284610826, 0.03125045498156164142, 0.03385385361191795006, 0.03645873261014952182, 0.03906243010681619693, 0.04166674480109257978, 0.04427107247243720900, 0.04687475664952634596, 0.04947964045798968619, 0.05208303702386667122, 0.05468803228817373241, 0.05729153353077973132, 0.05989618223844375006, 0.06250015876865079589, 0.06510412050499821135, 0.06770877833268285073, 0.07031227041168378045, 0.07291726700687002627, 0.07552066596874357218, 0.07812554330212571896, 0.08072923942118487295, 0.08333355289058355653, 0.08593787945419822938, 0.08854156225015286097, 0.09114644488045960113, 0.09374984019314609729, 0.09635483420994474246, 0.09895833431534489799, 0.1015629817166532611, 0.1041669571688737805, 0.1067709175595765864, 0.1093755742645453749, 0.1119790650618166516, 0.1145840604711090005, 0.1171874582687142119, 0.1197923343547293018, 0.1223960294069747767, 0.1250003415701952669, 0.1276046670722256471, 0.1302083485727723866, 0.1328132300777099817, 0.1354166241949035232, 0.1380216170238739992, 0.1406251160503516617, 0.1432297622036773077, 0.1458337366370238142, 0.1484376957407889386, 0.1510423513813509144, 0.1536458409560605698, 0.1562508352375901466, 0.1588542319300798034, 0.1614591068269417562, 0.1640628008713490293, 0.1666671117869774343, 0.1692714362859856492, 0.1718751165501164191, 0.1744799969878772505, 0.1770833899687347668, 0.1796883816679979429, 0.1822918796746371972, 0.1848965246383280081, 0.1875004981115827030, 0.1901044559872153150, 0.1927091106216977379, 0.1953125990329364348, 0.1979175922448092595, 0.2005209878913200294, 0.2031258616572126918, 0.2057295547527302204, 0.2083338644793258920, 0.2109381880338489224, 0.2135418671205281671, 0.2161467465492790951, 0.2187501384529311477, 0.2213551290805818306, 0.2239586261264417955, 0.2265632699588193688, 0.2291672425307399730, 0.2317711992370185270, 0.2343758529237242316, 0.2369793402305566954, 0.2395843324308542799, 0.2421877270904984059, 0.2447925997835804779, 0.2473962919891333490, 0.2500006005852301039, 0.2526049232537817546, 0.2552086012219486610, 0.2578134796998332035, 0.2604168705853860954, 0.2630218601994954719, 0.2656253563436123954, 0.2682299991029740149, 0.2708339708322964334, 0.2734379264279751531, 0.2760425792251849364, 0.2786460654866522724, 0.2812510567334335909, 0.2838544504653006673, 0.2864593221437078951, 0.2890630135181997962, 0.2916673210423081364, 0.2942716428833813125, 0.2968753197919519748, 0.2994801973770923054, 0.3020835873036303854, 0.3046885759622478540, 0.3072920712636373342, 0.3098967130082584398, 0.3125006839536987324, 0.3151046384975096371, 0.3177092904634842285, 0.3203127757386058927, 0.3229177660899096303, 0.3255211589530693228, 0.3281260296749167193, 0.3307297202772326306, 0.3333340267878420748, 0.3359383478599109463, 0.3385420237677806976, 0.3411469005182800607, 0.3437502895448679152, 0.3463552773060237788, 0.3489587718236830116, 0.3515634126118191150, 0.3541673828320756612, 0.3567713363827305639, 0.3593759875757128741, 0.3619794719234893932, 0.3645844614373360826, 0.3671878534908398217, 0.3697927233142242476, 0.3723964132032320795, 0.3750007187588132451, 0.3776050391203355505, 0.3802087140863810166, 0.3828135900603256703, 0.3854169782460106219, 0.3880219651677176973, 0.3906254589606275029, 0.3932300988505167960, 0.3958340684042725433, 0.3984380210204655492, 0.4010426714986830565, 0.4036461549780977487, 0.4062511437124918245, 0.4088545350153757196, 0.4114594039983773821, 0.4140630932329303349, 0.4166673978919369636, 0.4192717176013560643, 0.4218753916844373286, 0.4244802669398990425, 0.4270836543437129262, 0.4296886404839689866, 0.4322921336110964741, 0.4348967726609613837, 0.4375007416068860122, 0.4401046933472957945, 0.4427093431689624881, 0.4453128258389836835, 0.4479178138519160357, 0.4505212044632024293, 0.4531260726638874359, 0.4557297613028266636, 0.4583340651236982866, 0.4609383842394453867, 0.4635420574984087105, 0.4661469320934465421, 0.4687503187744080368, 0.4713553041911981989, 0.4739587967114984313, 0.4765634349795482838, 0.4791674033763006491, 0.4817713542995921694, 0.4843760035229108252, 0.4869794854424946973, 0.4895844727919445583, 0.4921878627706443576, 0.4947927302470669919, 0.4973964183492232127, 0.5000007213903868708, 0.5026050399708832384, 0.5052087124645624483, 0.5078135864572254077, 0.5104169724743423675, 0.5130219572256408123, 0.5156254491980594157, 0.5182300867424926016, 0.5208340546487225664, 0.5234380048135498509, 0.5260426534967141965, 0.5286461347248060383, 0.5312511214687432037, 0.5338545108738584899, 0.5364593776840630435, 0.5390630653082590928, 0.5416673676281316130, 0.5442716857317909662, 0.5468753575190105076, 0.5494802309673390006, 0.5520836163796108975, 0.5546886005233833128, 0.5572920920068584749, 0.5598967288858642810, 0.5625006963602153798, 0.5651046458252231286, 0.5677092940264200083, 0.5703127746219572858, 0.5729177608183441128, 0.5755211497088699169, 0.5781260159108934094, 0.5807297031159460721, 0.5833340047729366207, 0.5859383224581667937, 0.5885419935977430628, 0.5911468665597719996, 0.5937502514261915332, 0.5963552350203973340, 0.5989587260738620245, 0.6015633623456233536, 0.6041673294467342359, 0.6067712782705607655, 0.6093759260479724160, 0.6119794060698863225, 0.6145843917766802278, 0.6171877802116071399, 0.6197926458634805957, 0.6223963327082033814, 0.6250006337607152407, 0.6276049510859208480, 0.6302086216366651339, 0.6328134941704254279, 0.6354168785499811900, 0.6380218616525755726, 0.6406253523349600965, 0.6432299880576550777, 0.6458339548441623945, 0.6484379030854412473, 0.6510425504972472410, 0.6536460300044655281, 0.6562510152796211527, 0.6588544033179367654, 0.6614592684776883225, 0.6640629550208935195, 0.6666672555273263079, 0.6692715725509107427, 0.6718752425716313370, 0.6744801147351520143, 0.6770834986868305982, 0.6796884813557668714, 0.6822919717260003125, 0.6848966069578048543, 0.6875005734883452568, 0.6901045212057073108, 0.6927091683100871089, 0.6953126473615357517, 0.6979176322630067375, 0.7005210199636988655, 0.7031258846893556624, 0.7057295709898557812, 0.7083338710086078960, 0.7109381877889758838, 0.7135418573384794128, 0.7161467291897904985, 0.7187501127725786088, 0.7213550950658099703, 0.7239585851828231888, 0.7265632199819130888, 0.7291671863151253374, 0.7317711335672014705, 0.7343757804223364216, 0.7369792590769420615, 0.7395842436626837157, 0.7421876310847422831, 0.7447924954343322357, 0.7473961815509432283, 0.7500004811404139549, 0.7526047977359727748, 0.7552084668730677519, 0.7578133384702019359, 0.7604167217430886083, 0.7630217037185706985, 0.7656251936412983294, 0.7682298280658512724, 0.7708337942603785686, 0.7734377411058018792, 0.7760423877698768846, 0.7786458660865690495, 0.7812508504145402322, 0.7838542376169586046, 0.7864591016485131814, 0.7890627876400562180, 0.7916670868586475063, 0.7942714033278103214, 0.7968750721113085911, 0.7994799435123028930, 0.8020833265342820484, 0.8046883082499752815, 0.8072917980373575109, 0.8098964321455554005, 0.8125003982600473851, 0.8151043447574546352, 0.8177089912886614798, 0.8203124693263749156, 0.8229174534545398156, 0.8255208404963184643, 0.8281257042678743518, 0.8307293901931780411, 0.8333336890992975032, 0.8359380055004849153, 0.8385416739892034288, 0.8411465452521027508, 0.8437499280821748604, 0.8463549095960458679, 0.8489583993070312085, 0.8515630331570626099, 0.8541669992501779163, 0.8567709454582125295, 0.8593755919147509914, 0.8619790697324273276, 0.8645840537187589048, 0.8671874406589066275, 0.8697923042285079509, 0.8723959901464106714, 0.8750002887984731359, 0.8776046051901155165, 0.8802082734428797739, 0.8828131446257380111, 0.8854165273229123168, 0.8880215086929368340, 0.8906249983864840125, 0.8932296320365455955, 0.8958335981669537373, 0.8984375441442679078, 0.9010421905843485346, 0.9036456682409392815, 0.9062506521434200435, 0.9088540390409564074, 0.9114589024666573946, 0.9140625884360091824, 0.9166668868924389146, 0.9192712033329777377, 0.9218748714086243412, 0.9244797425695093773, 0.9270831251927963423, 0.9296881064769593195, 0.9322915962120889022, 0.9348962297203436966, 0.9375001959466012780, 0.9401041417521586174, 0.9427087882339971747, 0.9453122657876905643, 0.9479172496658602176, 0.9505206365780075606, 0.9531254999124115779, 0.9557291860198475764, 0.9583334843266348990, 0.9609378007344983041, 0.9635414689593263526, 0.9661463405142474148, 0.9687497214891268582, 0.9713547029754164841, 0.9739581985331400293, 0.9765628250748574768, 0.9791667834374845336, 0.9817707607320566021, 0.9843753697534296521, 0.9869788348889786400, 0.9895840831931937975, 0.9921867700316038263, 0.9947911815772807476, 0.9973998924267860611, 1.000000000000000000 ),
 .UNSPECIFIED. ) ;
#53665 = CARTESIAN_POINT ( 'NONE',  ( 9.579665964935223599, -7.246166700194470067, 5.204170427930421283E-15 ) ) ;
#53666 = CARTESIAN_POINT ( 'NONE',  ( 6.473500209388782345, -0.2444377345085078923, 1.954170833970412913 ) ) ;
#53667 = CARTESIAN_POINT ( 'NONE',  ( 4.380693030546913391, 7.164540064729805202, 1.082531754730549078 ) ) ;
#53668 = CARTESIAN_POINT ( 'NONE',  ( 5.888650760256147088, 5.979308965038350188, -0.1076000636002025918 ) ) ;
#53669 = CARTESIAN_POINT ( 'NONE',  ( -2.442440228756222353, 6.001264033524212671, -0.7998128361456281477 ) ) ;
#53670 = CARTESIAN_POINT ( 'NONE',  ( 0.4576791451081770323, -1.901157720872756141, 1.148870853762502753 ) ) ;
#53671 = CARTESIAN_POINT ( 'NONE',  ( 2.942513229011092690, 2.089901898437613870, 0.2590637233205703716 ) ) ;
#53672 = CARTESIAN_POINT ( 'NONE',  ( -5.490125858891038213, 5.369844688319787451, -0.7998128361456362523 ) ) ;
#53673 = CARTESIAN_POINT ( 'NONE',  ( 7.344766530301147789, 9.591980256816594164, 1.599625672291281386 ) ) ;
#53674 = CARTESIAN_POINT ( 'NONE',  ( 0.8185401059354965314, -1.351722143400556631, 1.279475349031534259 ) ) ;
#53675 = CARTESIAN_POINT ( 'NONE',  ( 5.991813822235618758, 9.077867661661846554, 1.199719254218462483 ) ) ;
#53676 = CARTESIAN_POINT ( 'NONE',  ( 5.172599298813543633, 5.993452922492633839, -1.199719254218452047 ) ) ;
#53677 = CARTESIAN_POINT ( 'NONE',  ( -5.790741006812557323, 9.769965251341050205, 0.000000000000000000 ) ) ;
#53678 = CARTESIAN_POINT ( 'NONE',  ( -6.548225005720456515, 10.58342024007512983, 0.000000000000000000 ) ) ;
#53679 =( BOUNDED_SURFACE ( )  B_SPLINE_SURFACE ( 3, 2, ( 
 ( #86221, #167476, #183715 ),
 ( #19071, #87289, #214046 ),
 ( #99288, #35323, #17995 ),
 ( #101401, #181575, #182643 ) ),
 .UNSPECIFIED., .F., .F., .T. ) 
 B_SPLINE_SURFACE_WITH_KNOTS ( ( 4, 4 ),
 ( 3, 3 ),
 ( 1.570796326794896558, 2.636531018672052085 ),
 ( 0.000000000000000000, 1.000000000000000000 ),
 .UNSPECIFIED. ) 
 GEOMETRIC_REPRESENTATION_ITEM ( )  RATIONAL_B_SPLINE_SURFACE ( (
 ( 1.000000000000000000, 0.7071067811865716646, 1.000000000000000000),
 ( 1.000000000000000000, 0.8161930835858144384, 1.000000000000000000),
 ( 1.000000000000000000, 0.8980788380693711659, 1.000000000000000000),
 ( 1.000000000000000000, 0.9374448844494299715, 1.000000000000000000) ) ) 
 REPRESENTATION_ITEM ( '' )  SURFACE ( )  );
#53680 = CARTESIAN_POINT ( 'NONE',  ( 1.476976393720278002, -1.495863523836362896, 1.503369785937097136 ) ) ;
#53681 = CARTESIAN_POINT ( 'NONE',  ( -6.237633190739009237, 9.434933268240943249, 1.199719254218452047 ) ) ;
#53683 = CARTESIAN_POINT ( 'NONE',  ( 4.422284181769401634, 0.9229163912191931107, 1.731201473044993167 ) ) ;
#53682 = CARTESIAN_POINT ( 'NONE',  ( -0.6125000000000314637, 0.9583333333333388104, -1.060881119635965764 ) ) ;
#53684 = CARTESIAN_POINT ( 'NONE',  ( 2.008865009297224447, 1.601992838228694316, -1.451600824242594845 ) ) ;
#53685 = CARTESIAN_POINT ( 'NONE',  ( 1.329379181053941483, 0.9071106928158387817, -1.602193565413398746 ) ) ;
#53687 = CARTESIAN_POINT ( 'NONE',  ( -5.513283157632952403, 6.248865724650796594, -0.9728955443181900309 ) ) ;
#53686 = CARTESIAN_POINT ( 'NONE',  ( -5.171509248969888617, 4.998125310078441075, 0.7998128361456281477 ) ) ;
#53688 = CARTESIAN_POINT ( 'NONE',  ( 3.538731034799988073, -1.318886434843706601, -1.135564254951209273 ) ) ;
#53689 = CARTESIAN_POINT ( 'NONE',  ( -9.117697077654417726, 14.00000000001154987, -7.299999999986900079 ) ) ;
#53690 = CARTESIAN_POINT ( 'NONE',  ( 5.721177635286841756, 6.737423998331861341, -1.082531754730543083 ) ) ;
#53691 = CARTESIAN_POINT ( 'NONE',  ( -11.14501278000869355, 7.223412960316487386, -3.546411330735405265 ) ) ;
#53692 = CARTESIAN_POINT ( 'NONE',  ( 2.325270847726228940, -0.0006328605136555342939, 2.161883445422786654 ) ) ;
#53693 = EDGE_CURVE ( 'NONE', #160642, #11923, #48609, .T. ) ;
#53694 = CIRCLE ( 'NONE', #192054, 1.219999999999999751 ) ;
#53695 = CARTESIAN_POINT ( 'NONE',  ( 3.093124880496417983, 1.122326866504215426, -1.674630914042275709 ) ) ;
#53696 = CARTESIAN_POINT ( 'NONE',  ( -0.5000000000000038858, 3.949999999999995293, -0.4000000000000166755 ) ) ;
#53697 = CARTESIAN_POINT ( 'NONE',  ( -3.363304624641834106, 6.081549941127532222, -1.199719254218452047 ) ) ;
#53698 = CARTESIAN_POINT ( 'NONE',  ( 3.467610927914951624, 1.923740664667829225, -0.4305075535177785295 ) ) ;
#53699 = DIRECTION ( 'NONE',  ( 0.000000000000000000, 1.000000000000000000, 0.000000000000000000 ) ) ;
#53700 = CARTESIAN_POINT ( 'NONE',  ( 2.401813893259804100, -0.7453968187615340746, -1.793506507769267788 ) ) ;
#53703 = ORIENTED_EDGE ( 'NONE', *, *, #179393, .T. ) ;
#53702 = CARTESIAN_POINT ( 'NONE',  ( -4.719646871332968452, 5.639247783710797712, 1.082531754730549078 ) ) ;
#53701 =( LENGTH_UNIT ( ) NAMED_UNIT ( * ) SI_UNIT ( .MILLI., .METRE. ) );
#53704 = CARTESIAN_POINT ( 'NONE',  ( -4.109529958273628658, 7.808552361378938045, 0.7216878364870338292 ) ) ;
#53705 = CARTESIAN_POINT ( 'NONE',  ( 6.222266154028957885, 6.224008365980749247, 0.7998128361456352531 ) ) ;
#53706 = CARTESIAN_POINT ( 'NONE',  ( -5.143339171537843590, 7.093924681584509173, 1.599625672291263179 ) ) ;
#53708 = VERTEX_POINT ( 'NONE', #167014 ) ;
#53707 = CARTESIAN_POINT ( 'NONE',  ( -6.631873415740034083, 7.766215735565355160, 1.199719254218452047 ) ) ;
#53709 = CARTESIAN_POINT ( 'NONE',  ( -9.937763408692596556, 11.65677406730528887, -1.082531754730537976 ) ) ;
#53710 = CARTESIAN_POINT ( 'NONE',  ( 0.4642757356001780966, 2.182421439735841684, -0.3260586787675948117 ) ) ;
#53711 = DIRECTION ( 'NONE',  ( -3.706092522800016599E-15, 0.000000000000000000, -1.000000000000000000 ) ) ;
#53712 = CARTESIAN_POINT ( 'NONE',  ( 4.100408672059585591, 1.951911038179511726, 0.1965976633130430695 ) ) ;
#53713 = CARTESIAN_POINT ( 'NONE',  ( 6.923409998072794558, 11.22906209772695618, 1.040834085586084257E-14 ) ) ;
#53714 = CARTESIAN_POINT ( 'NONE',  ( 1.740861508391436274, 2.010826320759526720, -0.1511413081683593562 ) ) ;
#53715 = ORIENTED_EDGE ( 'NONE', *, *, #56647, .F. ) ;
#53716 = CARTESIAN_POINT ( 'NONE',  ( 3.731751022097353321, 0.7093996228057770637, -1.995120430414954349 ) ) ;
#53717 = CARTESIAN_POINT ( 'NONE',  ( 1.499999999999989120, 2.056250000682817269, 1.214306433183764966E-14 ) ) ;
#53719 = CARTESIAN_POINT ( 'NONE',  ( -4.771579997005698459, 7.654261532226910525, -1.199719254218452047 ) ) ;
#53718 = CARTESIAN_POINT ( 'NONE',  ( -10.38894090356600231, 1.970899860167847795, 5.551243578534467815 ) ) ;
#53720 = CARTESIAN_POINT ( 'NONE',  ( 3.591602706507342369, -1.839109287420921834, -0.08896477992388628075 ) ) ;
#53721 = ORIENTED_EDGE ( 'NONE', *, *, #156347, .F. ) ;
#53722 = CARTESIAN_POINT ( 'NONE',  ( -8.833300774503376473, 10.26427131079744193, 1.199719254218462483 ) ) ;
#53723 = CYLINDRICAL_SURFACE ( 'NONE', #179613, 0.3999999999999997446 ) ;
#53724 = CARTESIAN_POINT ( 'NONE',  ( 3.533539421053989660, -0.1523460092780377639, 2.115156586662121363 ) ) ;
#53725 = CARTESIAN_POINT ( 'NONE',  ( 4.370663978927065152, 5.060324124126029943, 1.009771797811723326 ) ) ;
#53726 = CARTESIAN_POINT ( 'NONE',  ( 7.610204295972345712, 7.772993188256215547, 0.7998128361456341429 ) ) ;
#53727 = EDGE_CURVE ( 'NONE', #6407, #55540, #191136, .T. ) ;
#53728 = CARTESIAN_POINT ( 'NONE',  ( 5.378222296270031677, -1.148346438381561363, 1.710960936357192264 ) ) ;
#53730 = CARTESIAN_POINT ( 'NONE',  ( 2.243484787601189634, 1.840893492186860492, 0.04347913094143729396 ) ) ;
#53729 = CARTESIAN_POINT ( 'NONE',  ( -7.172426956829277778, 8.326585190177668849, -1.199719254218452935 ) ) ;
#53731 = CARTESIAN_POINT ( 'NONE',  ( 8.289920859751990889, 11.75899253876431416, 1.199719254218450271 ) ) ;
#53732 = CARTESIAN_POINT ( 'NONE',  ( -1.001543065824772872E-14, 5.571875000341416140, 1.575800808251672791 ) ) ;
#53733 = CYLINDRICAL_SURFACE ( 'NONE', #125837, 11.09999999999999964 ) ;
#53734 = CARTESIAN_POINT ( 'NONE',  ( -6.474900878978163021, 9.711745571186627402, -1.199719254218452047 ) ) ;
#53735 = CARTESIAN_POINT ( 'NONE',  ( 3.475000000000000533, -1.560416665710748996, 2.006292185433948827 ) ) ;
#53736 = CARTESIAN_POINT ( 'NONE',  ( 2.350463684150871035, 2.206416367115513477, 0.05273732197710182673 ) ) ;
#53737 = CARTESIAN_POINT ( 'NONE',  ( 4.288523069895104456, -2.236996925053718055, -0.3375187357864944393 ) ) ;
#53738 = CARTESIAN_POINT ( 'NONE',  ( -8.026063749610061748, 9.426457798375635022, -1.082531754730543971 ) ) ;
#53739 = CARTESIAN_POINT ( 'NONE',  ( 4.781432078664868079, 0.1701398743050798745, -1.803555781593807250 ) ) ;
#53740 = CARTESIAN_POINT ( 'NONE',  ( 4.505048170306029220, -0.08773398713153966744, 1.913818227509517023 ) ) ;
#53741 = CARTESIAN_POINT ( 'NONE',  ( -1.364683531249997417, 4.571875000341417028, 1.214306433183764966E-14 ) ) ;
#53742 = CARTESIAN_POINT ( 'NONE',  ( 3.678557393866654923, -1.899675168901427513, -0.5269097987367215019 ) ) ;
#53743 = CARTESIAN_POINT ( 'NONE',  ( 4.574985519202336981, -0.0001439422951596270033, -1.870836309977530920 ) ) ;
#53744 = CARTESIAN_POINT ( 'NONE',  ( 3.282123524285113003, 1.463787882210180191, 1.784030387633539938 ) ) ;
#53745 = CARTESIAN_POINT ( 'NONE',  ( 4.861673063681271501, -0.4970775243713953517, 1.793344219904927206 ) ) ;
#53746 = CARTESIAN_POINT ( 'NONE',  ( 1.364683531249990311, 5.134375000341417916, 1.214306433183764966E-14 ) ) ;
#53747 = AXIS2_PLACEMENT_3D ( 'NONE', #69873, #53655, #36324 ) ;
#53748 = CARTESIAN_POINT ( 'NONE',  ( -6.471393748265563239, 5.229711127717889596, 2.419999999999998597 ) ) ;
#53750 = CARTESIAN_POINT ( 'NONE',  ( 1.981218818260335413, -0.1044028718686483975, -2.103608768903475035 ) ) ;
#53749 = CARTESIAN_POINT ( 'NONE',  ( -4.406036734316900905, 5.203092947200234519, -1.082531754730543971 ) ) ;
#53751 = PRESENTATION_LAYER_ASSIGNMENT (  '', '', ( #212833 ) ) ;
#53752 = CARTESIAN_POINT ( 'NONE',  ( 2.806174607904299734, 5.257325561654889512, -1.082531754730543083 ) ) ;
#53754 = CARTESIAN_POINT ( 'NONE',  ( -9.938290294017125603, 11.55342575023019691, -1.199719254218441611 ) ) ;
#53753 = CARTESIAN_POINT ( 'NONE',  ( -0.6823417656249969321, 4.780208333674755394, -1.181850606188749264 ) ) ;
#53755 = CARTESIAN_POINT ( 'NONE',  ( 3.129257641292593650, 1.918792544363761454, 0.9031103230835100248 ) ) ;
#53757 = FACE_OUTER_BOUND ( 'NONE', #52650, .T. ) ;
#53756 = B_SPLINE_CURVE_WITH_KNOTS ( 'NONE', 3,
 ( #5496, #171228, #185337, #173388, #71577, #88937 ),
 .UNSPECIFIED., .F., .F.,
 ( 4, 2, 4 ),
 ( 0.000000000000000000, 0.0003779448103413554985, 0.0007558896206827109970 ),
 .UNSPECIFIED. ) ;
#53758 = CARTESIAN_POINT ( 'NONE',  ( 0.7561249178302269502, 0.8145892717734238841, -1.848413388458100215 ) ) ;
#53759 = CARTESIAN_POINT ( 'NONE',  ( -1.364683531250012516, 0.7802083336747528408, 0.7879004041258379498 ) ) ;
#53760 = CARTESIAN_POINT ( 'NONE',  ( -3.253593677599670109, 5.779314476299451719, 1.082531754730560403 ) ) ;
#53761 = CARTESIAN_POINT ( 'NONE',  ( 4.792970997630896512, 5.550553237779539018, 1.199719254218464037 ) ) ;
#53762 = ORIENTED_EDGE ( 'NONE', *, *, #2635, .T. ) ;
#53763 = ADVANCED_FACE ( 'NONE', ( #99876 ), #165939, .F. ) ;
#53764 = CARTESIAN_POINT ( 'NONE',  ( 2.513140823169751847, 1.929641211675875878, 0.9743453106897670413 ) ) ;
#53765 = CARTESIAN_POINT ( 'NONE',  ( 6.610000000000011866, 2.967812824040619191, 2.453181572820534395 ) ) ;
#53768 = DIRECTION ( 'NONE',  ( 3.451266460341927524E-31, -0.6000000000000035305, 0.7999999999999974909 ) ) ;
#53767 = CARTESIAN_POINT ( 'NONE',  ( 6.925078400183546812, 3.702220002068328242, 2.370079373711677206 ) ) ;
#53766 = CARTESIAN_POINT ( 'NONE',  ( 4.817943484809818600, 6.714296380401858499, 1.599625672291269396 ) ) ;
#53769 = LINE ( 'NONE', #152334, #141450 ) ;
#53770 = CARTESIAN_POINT ( 'NONE',  ( 5.805875103277515770, -1.124240986939632592, -1.673857227857282082 ) ) ;
#53771 = CARTESIAN_POINT ( 'NONE',  ( -9.192064960385334160, 9.826423329978791088, 0.7216878364870438212 ) ) ;
#53772 = CARTESIAN_POINT ( 'NONE',  ( 0.2049558871960316941, 1.909868400323280424, 1.074723926240577221 ) ) ;
#53773 = CARTESIAN_POINT ( 'NONE',  ( 0.000000000000000000, 4.000000000000003553, -11.50000000000000000 ) ) ;
#53775 = CARTESIAN_POINT ( 'NONE',  ( 1.364683531249996529, 12.21354166700805877, 0.7879004041258403923 ) ) ;
#53774 = CARTESIAN_POINT ( 'NONE',  ( 0.9719599696450488269, 2.179858136331577434, -0.6057951801161051142 ) ) ;
#53776 = CARTESIAN_POINT ( 'NONE',  ( -8.025536864285518490, 11.45054454405341282, -1.199719254218446718 ) ) ;
#53777 = CARTESIAN_POINT ( 'NONE',  ( -4.568734577680887199, 6.353276312092901890, -1.443375672974051449 ) ) ;
#53778 = CARTESIAN_POINT ( 'NONE',  ( 0.6823417656249882723, 1.738541667008083991, -1.181850606188749264 ) ) ;
#53779 = LINE ( 'NONE', #106849, #151305 ) ;
#53780 = CARTESIAN_POINT ( 'NONE',  ( -6.009258394948636914E-15, 9.437499999999996447, -1.732050807568875195 ) ) ;
#53781 = CARTESIAN_POINT ( 'NONE',  ( 4.371539443043367612, 1.672179000890521516, -0.4225743650863537648 ) ) ;
#53782 = CARTESIAN_POINT ( 'NONE',  ( 5.662465432362883355, 6.635239754958710989, 1.199719254218451159 ) ) ;
#53783 = CARTESIAN_POINT ( 'NONE',  ( 2.565387841970759197, 1.736461783412158955, -0.3405875811831828859 ) ) ;
#53784 = CARTESIAN_POINT ( 'NONE',  ( 3.018229385809416687, -2.010681777978724494, 0.1011178238035769505 ) ) ;
#53785 = CARTESIAN_POINT ( 'NONE',  ( 9.398826802771546696, 11.98838390803207865, -1.599625672291262513 ) ) ;
#53787 = AXIS2_PLACEMENT_3D ( 'NONE', #195317, #141269, #43748 ) ;
#53786 = CARTESIAN_POINT ( 'NONE',  ( 4.823365732668142947, -0.1123398232194070118, 2.204042774474362254 ) ) ;
#53788 = VERTEX_POINT ( 'NONE', #40211 ) ;
#53789 = CARTESIAN_POINT ( 'NONE',  ( 3.885024839820313325, -1.886105071096555230, -0.7231171000243222791 ) ) ;
#53790 = CARTESIAN_POINT ( 'NONE',  ( -5.576146316970437944, 9.727530813099326323, 0.000000000000000000 ) ) ;
#53792 = CARTESIAN_POINT ( 'NONE',  ( 4.288685525864014636, 1.556897452430844320, -1.281376678550147474 ) ) ;
#53791 = CARTESIAN_POINT ( 'NONE',  ( 5.496778590849229040, -2.068848325035842706, -0.4644329061709790429 ) ) ;
#53793 = VERTEX_POINT ( 'NONE', #169131 ) ;
#53794 = EDGE_LOOP ( 'NONE', ( #89421, #88183, #132044, #199946, #26203, #51432, #141597, #139329, #175578, #137751, #46600, #165333, #201812, #65987, #206476, #133507, #7549, #204912, #140151, #148727 ) ) ;
#53795 = CARTESIAN_POINT ( 'NONE',  ( 1.533845512228737551, 0.9248708299973290581, -1.625957014461040906 ) ) ;
#53796 = CARTESIAN_POINT ( 'NONE',  ( -10.91808280586644564, -9.921948886890824326, 0.1881369732364187586 ) ) ;
#53797 = CARTESIAN_POINT ( 'NONE',  ( 6.024035747493574178, -1.796918165027236780, 0.2286857708345239326 ) ) ;
#53799 = VECTOR ( 'NONE', #148417, 1000.000000000000000 ) ;
#53798 = DIRECTION ( 'NONE',  ( 0.000000000000000000, -1.000000000000000000, 0.000000000000000000 ) ) ;
#53800 = CARTESIAN_POINT ( 'NONE',  ( -9.748930057865852206, 3.057420161666833280, -6.444087955423147385 ) ) ;
#53801 = PRESENTATION_STYLE_ASSIGNMENT (( #103622 ) ) ;
#53802 = ADVANCED_FACE ( 'NONE', ( #69476 ), #205044, .T. ) ;
#53803 = CARTESIAN_POINT ( 'NONE',  ( -0.6823417656249969321, 3.280208333674754062, -1.181850606188749264 ) ) ;
#53804 = CARTESIAN_POINT ( 'NONE',  ( 0.5801457039020865292, 0.9447208859736742070, 1.662703529197881558 ) ) ;
#53805 = CIRCLE ( 'NONE', #195597, 0.07999999999999984901 ) ;
#53806 = CARTESIAN_POINT ( 'NONE',  ( 6.373741612200171325, 7.569024981389272710, 1.082531754730549967 ) ) ;
#53807 = CARTESIAN_POINT ( 'NONE',  ( 1.926150285298435572, 1.005797860886543660, 1.684270608208485065 ) ) ;
#53808 = EDGE_CURVE ( 'NONE', #184764, #9073, #4463, .T. ) ;
#53809 = CYLINDRICAL_SURFACE ( 'NONE', #172026, 1.250000000000000000 ) ;
#53810 = CARTESIAN_POINT ( 'NONE',  ( -5.773793314573309132, 7.829454515125894964, 1.599625672291263179 ) ) ;
#53811 = CARTESIAN_POINT ( 'NONE',  ( 3.797228045176269440, -0.2112621354826669517, -2.110076569278092062 ) ) ;
#53812 = CARTESIAN_POINT ( 'NONE',  ( 10.39640486358069360, 11.02356051713265650, 0.7998128361456462443 ) ) ;
#53813 = CARTESIAN_POINT ( 'NONE',  ( 5.677018108359257020, -0.04579235393691384604, -1.970973552702318443 ) ) ;
#53814 = CARTESIAN_POINT ( 'NONE',  ( 1.364683531249988757, 1.384375000341421469, 0.000000000000000000 ) ) ;
#53815 = CARTESIAN_POINT ( 'NONE',  ( 0.8439947366445134103, -1.280256340399921200, -1.553649900018534202 ) ) ;
#53816 = EDGE_LOOP ( 'NONE', ( #210474, #191284, #204265, #207156 ) ) ;
#53817 = CARTESIAN_POINT ( 'NONE',  ( 0.9138395863287234189, -1.346417975848941406, -1.633941036375158973 ) ) ;
#53818 = CARTESIAN_POINT ( 'NONE',  ( 11.39494474744699737, 7.467063048907871092, -3.787837880199416585 ) ) ;
#53819 = CARTESIAN_POINT ( 'NONE',  ( 2.313015868914463091, -1.601887806243259771, 1.311650804931147274 ) ) ;
#53820 = CARTESIAN_POINT ( 'NONE',  ( 5.011674058906918638, 5.875983152593414971, 1.199719254218452047 ) ) ;
#53821 = CARTESIAN_POINT ( 'NONE',  ( 4.037295881819344956, 7.932205305423046582, -0.7998128361456362523 ) ) ;
#53822 = ORIENTED_EDGE ( 'NONE', *, *, #37827, .T. ) ;
#53824 = CARTESIAN_POINT ( 'NONE',  ( 3.845709127770629010, 7.638411082374393146, 0.7998128361456321445 ) ) ;
#53823 = CARTESIAN_POINT ( 'NONE',  ( 5.244118971382810912, 0.6063552182394044143, 2.000762070341703502 ) ) ;
#53827 = ORIENTED_EDGE ( 'NONE', *, *, #3571, .F. ) ;
#53826 = CARTESIAN_POINT ( 'NONE',  ( 2.051130129875160968, -1.617795175136220509, 0.8151331081446986371 ) ) ;
#53825 = CARTESIAN_POINT ( 'NONE',  ( 3.575057022766346737, 0.04566639709948847742, -1.825179878808772305 ) ) ;
#53828 = CARTESIAN_POINT ( 'NONE',  ( 9.622536337397022521, 12.24937836509514710, 1.599625672291281386 ) ) ;
#53829 = DIRECTION ( 'NONE',  ( -0.9781476007338056888, 0.000000000000000000, -0.2079116908177593703 ) ) ;
#53830 = CARTESIAN_POINT ( 'NONE',  ( 11.83562794788958072, 6.758279503156755297, 3.688202522935868810 ) ) ;
#53831 = CARTESIAN_POINT ( 'NONE',  ( 5.315527377757141458, -0.3284926246858720922, 2.182075488366498117 ) ) ;
#53832 = CARTESIAN_POINT ( 'NONE',  ( 1.364683531250000748, 8.817708333674731946, -0.7879004041258355073 ) ) ;
#53833 = EDGE_LOOP ( 'NONE', ( #182161, #121566, #70842, #84516 ) ) ;
#53834 = CARTESIAN_POINT ( 'NONE',  ( 4.529883686416775745, -1.874680353417649492, 0.3764776581506729114 ) ) ;
#53835 = CARTESIAN_POINT ( 'NONE',  ( -2.839543107058306592, 5.400218493954923815, -1.199719254218446718 ) ) ;
#53836 = CARTESIAN_POINT ( 'NONE',  ( 9.121938423896107651, 9.536683004167278099, -0.7998128361456221525 ) ) ;
#53837 = DIRECTION ( 'NONE',  ( 0.7592566023652994600, 0.6507913734559651608, 0.000000000000000000 ) ) ;
#53838 = DIRECTION ( 'NONE',  ( 0.000000000000000000, -1.000000000000000000, 0.000000000000000000 ) ) ;
#53839 = CARTESIAN_POINT ( 'NONE',  ( 6.427279137517246888, -1.429865906218323435, -1.660902671979214595 ) ) ;
#53840 = CARTESIAN_POINT ( 'NONE',  ( 5.300918301777743480, 7.749796750553542779, -1.302405036909856761 ) ) ;
#53841 = CARTESIAN_POINT ( 'NONE',  ( -5.991201129311522600, 15.51884043574794880, -10.40697265741862054 ) ) ;
#53842 = ORIENTED_EDGE ( 'NONE', *, *, #175406, .T. ) ;
#53843 = CARTESIAN_POINT ( 'NONE',  ( -11.92046840572485777, 12.44747875205729670, -1.382231356234943309 ) ) ;
#53844 = CARTESIAN_POINT ( 'NONE',  ( 3.549935554046261821, 1.870726058081632504, 0.003126486288931861444 ) ) ;
#53845 = CARTESIAN_POINT ( 'NONE',  ( -0.02319159430947542039, 5.725354828811364705, -2.405035539666657840 ) ) ;
#53846 = DIRECTION ( 'NONE',  ( 0.000000000000000000, 1.000000000000000000, 0.000000000000000000 ) ) ;
#53847 = CARTESIAN_POINT ( 'NONE',  ( -7.782016984564068096, 10.10210578678999482, 1.443375672974090751 ) ) ;
#53848 = CARTESIAN_POINT ( 'NONE',  ( 5.598591087800349086, 5.496387455380669529, -0.7998128361456481317 ) ) ;
#53849 = CARTESIAN_POINT ( 'NONE',  ( 6.986529229743720926, 7.045372277656132276, -0.7998128361456281477 ) ) ;
#53850 = CARTESIAN_POINT ( 'NONE',  ( 0.4792732452305690782, -0.1022114018467655538, 1.966944630885968603 ) ) ;
#53851 = CARTESIAN_POINT ( 'NONE',  ( 0.8082205221912192039, 1.198841770460257194, -1.621197638953228548 ) ) ;
#53852 = CARTESIAN_POINT ( 'NONE',  ( -8.299562589859897699, 12.83457345481192036, -0.7998128361456281477 ) ) ;
#53853 = CARTESIAN_POINT ( 'NONE',  ( 5.234329823327693809, 8.264412672927770487, 1.199719254218451159 ) ) ;
#53854 = DIRECTION ( 'NONE',  ( 0.000000000000000000, -1.000000000000000000, 0.000000000000000000 ) ) ;
#53855 = CARTESIAN_POINT ( 'NONE',  ( 0.8498829323080080433, 2.188760582993890313, -0.1110106097068005726 ) ) ;
#53856 = CARTESIAN_POINT ( 'NONE',  ( 6.721331454403435934, -0.1262074967819451221, 1.796610827203233063 ) ) ;
#53857 = CARTESIAN_POINT ( 'NONE',  ( -3.972702704004144714, 4.593573561881607148, 1.199719254218462483 ) ) ;
#53858 = CARTESIAN_POINT ( 'NONE',  ( 4.909461021924244051, 6.821066840368686712, 1.443375672974065660 ) ) ;
#53859 = CARTESIAN_POINT ( 'NONE',  ( 9.561524646135536543, 12.17819805862340310, -1.599625672291262513 ) ) ;
#53860 = CARTESIAN_POINT ( 'NONE',  ( 4.552840656090682891, 4.206068941727564514, 1.214306433183764966E-14 ) ) ;
#53861 = CARTESIAN_POINT ( 'NONE',  ( 4.415115299905642665, 5.179997933758551554, -1.199719254218450271 ) ) ;
#53862 = ORIENTED_EDGE ( 'NONE', *, *, #169914, .F. ) ;
#53864 = CARTESIAN_POINT ( 'NONE',  ( 0.6275903186243469989, -0.2933333519314991755, 1.991482607974030206 ) ) ;
#53863 = CARTESIAN_POINT ( 'NONE',  ( 4.265079090171526310, 1.784866007061826298, -0.4516350764028759235 ) ) ;
#53865 = CARTESIAN_POINT ( 'NONE',  ( 2.214639623771569088, -1.845710301178200119, -1.369457037089250484 ) ) ;
#53867 = CARTESIAN_POINT ( 'NONE',  ( 6.174655700867183405, 1.320063289540554408, -1.451312704123429498 ) ) ;
#53866 = CARTESIAN_POINT ( 'NONE',  ( 4.853455804012228647, 4.764712647543454693, 0.7216878364870317197 ) ) ;
#53868 = CARTESIAN_POINT ( 'NONE',  ( -3.285556943750000514, -3.288541666188709023, -1.896917185911906500 ) ) ;
#53869 = CARTESIAN_POINT ( 'NONE',  ( -5.915435094264120508, 5.795762452929912101, 0.000000000000000000 ) ) ;
#53870 = CARTESIAN_POINT ( 'NONE',  ( 4.207966135563082410, 7.175396087857922822, -1.043745235818753780 ) ) ;
#53871 = CARTESIAN_POINT ( 'NONE',  ( 4.922078805074791674, -1.902621863305080430, 0.1933406509087298719 ) ) ;
#53872 = CARTESIAN_POINT ( 'NONE',  ( -8.123306592882240551, 12.62894145833798376, 0.000000000000000000 ) ) ;
#53873 = CARTESIAN_POINT ( 'NONE',  ( 6.272547281004660746, 6.891683285556123195, -0.7655605874731727933 ) ) ;
#53874 = CARTESIAN_POINT ( 'NONE',  ( -4.995253251992230581, 4.792493313604505367, 0.000000000000000000 ) ) ;
#53876 = CARTESIAN_POINT ( 'NONE',  ( 2.535844406030359544, 0.8837261853790435717, -1.648756255988912400 ) ) ;
#53875 = CARTESIAN_POINT ( 'NONE',  ( 3.720331632570073932, 1.985922124624572627, 0.6539709493295197129 ) ) ;
#53877 = CARTESIAN_POINT ( 'NONE',  ( 7.782016984564054773, 10.10210578678999482, 1.443375672974076540 ) ) ;
#53878 = CARTESIAN_POINT ( 'NONE',  ( 0.6823417656249899377, 5.238541667008086655, -1.181850606188754593 ) ) ;
#53879 = CARTESIAN_POINT ( 'NONE',  ( 3.614586527008158523, -0.1238012486478034802, 1.736083139875769676 ) ) ;
#53880 = CARTESIAN_POINT ( 'NONE',  ( 5.522248639467795428, 5.337044922334209573, -0.7998128361456231517 ) ) ;
#53881 = CARTESIAN_POINT ( 'NONE',  ( -6.844806938814769204, -6.074287852078585459, -7.461813752226478691 ) ) ;
#53882 = CARTESIAN_POINT ( 'NONE',  ( 4.494587217144647262, -0.3816326207147257010, -1.681953545215847168 ) ) ;
#53883 = CARTESIAN_POINT ( 'NONE',  ( 4.212563348414651188, 2.004022095860341413, 0.8874167208733558798 ) ) ;
#53884 = CARTESIAN_POINT ( 'NONE',  ( 6.639307388351803674, -1.973492857608965423, 0.9879489342229507143 ) ) ;
#53885 = CARTESIAN_POINT ( 'NONE',  ( 1.426686711745578151, 7.396164654317697540, 4.272688476054470996 ) ) ;
#53886 = CARTESIAN_POINT ( 'NONE',  ( 3.168971741543443077, 1.575705016696099081, -1.493804678357780524 ) ) ;
#53887 = CARTESIAN_POINT ( 'NONE',  ( 2.068725586703868746, -1.668841220716179130, -0.7407507213199536755 ) ) ;
#53888 = CARTESIAN_POINT ( 'NONE',  ( 0.3913574919355842785, -1.795980968407092426, 0.7896611536716554580 ) ) ;
#53889 = CARTESIAN_POINT ( 'NONE',  ( 4.241493788847498614, 0.4602237217972443561, -2.066584722733503909 ) ) ;
#53890 = VERTEX_POINT ( 'NONE', #88970 ) ;
#53892 = CARTESIAN_POINT ( 'NONE',  ( 0.6823417656249899377, 3.155208333674754062, 1.181850606188765695 ) ) ;
#53891 = CARTESIAN_POINT ( 'NONE',  ( 4.282983983471492451, 2.047787327626307441, -1.030491903107624951 ) ) ;
#53893 = CARTESIAN_POINT ( 'NONE',  ( 6.720655732516655156, 7.629137130509086262, 2.526260288887293814 ) ) ;
#53894 = CARTESIAN_POINT ( 'NONE',  ( 8.543609354905870035, 13.11929468069890525, 0.7998128361456462443 ) ) ;
#53895 = CARTESIAN_POINT ( 'NONE',  ( 0.3641364058636682999, 0.6611385597973111761, -2.014868753213174823 ) ) ;
#53896 = CARTESIAN_POINT ( 'NONE',  ( -5.585596099150193616, 6.579245539505756746, -1.082531754730544860 ) ) ;
#53897 = AXIS2_PLACEMENT_3D ( 'NONE', #202847, #122796, #72857 ) ;
#53898 = CARTESIAN_POINT ( 'NONE',  ( -5.688757509019083614, 5.629766575900002401, -2.500000000000000444 ) ) ;
#53899 = CARTESIAN_POINT ( 'NONE',  ( -6.060131475184148186, 6.172500930577367484, 0.7216878364870317197 ) ) ;
#53901 = CARTESIAN_POINT ( 'NONE',  ( -6.009258394948636914E-15, 10.96875000068279249, -1.732050807568875195 ) ) ;
#53900 = DIRECTION ( 'NONE',  ( -0.6249999999683966134, 6.689064965917005136E-09, 0.7806247498251027706 ) ) ;
#53903 = ORIENTED_EDGE ( 'NONE', *, *, #123570, .F. ) ;
#53902 = AXIS2_PLACEMENT_3D ( 'NONE', #210039, #144043, #172515 ) ;
#53904 = CARTESIAN_POINT ( 'NONE',  ( 5.361953999179126740, -0.05229508359532940298, -2.015913028294749942 ) ) ;
#53906 = CARTESIAN_POINT ( 'NONE',  ( 4.715719689075464238, 0.4568931354213046636, -2.011171341922016076 ) ) ;
#53905 = CARTESIAN_POINT ( 'NONE',  ( 4.313465427442102929, 8.184126765324453601, 0.7998128361456462443 ) ) ;
#53908 = CARTESIAN_POINT ( 'NONE',  ( -0.2409995289980245703, 0.2355275985303668385, -2.034371242098035548 ) ) ;
#53907 = CARTESIAN_POINT ( 'NONE',  ( 7.205232291019763480, 7.370802192470005565, -0.7998128361456341429 ) ) ;
#53909 = CARTESIAN_POINT ( 'NONE',  ( 6.770317605177710085, 8.992066187497757213, 1.599625672291268286 ) ) ;
#53910 = CARTESIAN_POINT ( 'NONE',  ( -3.285556943750000070, -1.859374999522041882, 0.000000000000000000 ) ) ;
#53911 = CARTESIAN_POINT ( 'NONE',  ( 0.4454078864507329816, 0.6539998520847762897, -1.985780399853773526 ) ) ;
#53912 = CARTESIAN_POINT ( 'NONE',  ( 4.377577386359387646, -0.4445010797573499817, -1.966645064109616481 ) ) ;
#53913 = CARTESIAN_POINT ( 'NONE',  ( 3.491602800004707241, -1.839307750763185645, -0.08696504193297231733 ) ) ;
#53914 = CARTESIAN_POINT ( 'NONE',  ( 7.142447996300871793, 7.227277505306155092, 0.7998128361456341429 ) ) ;
#53915 =( LENGTH_UNIT ( ) NAMED_UNIT ( * ) SI_UNIT ( .MILLI., .METRE. ) );
#53916 = CARTESIAN_POINT ( 'NONE',  ( 0.7270763493693053192, -1.639898566368836130, 0.5346300883638678281 ) ) ;
#53917 = CARTESIAN_POINT ( 'NONE',  ( 0.000000000000000000, -2.079999999999998295, 10.99999999999999112 ) ) ;
#53918 = CARTESIAN_POINT ( 'NONE',  ( 0.6866852740153045476, 1.883736933065732533, 1.317207514508748734 ) ) ;
#53919 = CARTESIAN_POINT ( 'NONE',  ( -5.605406444246153974, 8.627059054007450101, -1.199719254218440723 ) ) ;
#53920 = CARTESIAN_POINT ( 'NONE',  ( 6.526273518496622295, 1.309208030111205900, -1.845092234498114658 ) ) ;
#53921 = CARTESIAN_POINT ( 'NONE',  ( 2.772209899791327370, 1.127123820452385017, 1.778883819610539208 ) ) ;
#53922 = CARTESIAN_POINT ( 'NONE',  ( -5.418418667316934112, 6.350518529071726981, -1.199719254218453823 ) ) ;
#53923 = CARTESIAN_POINT ( 'NONE',  ( 7.558834334818744338, 8.777393797832065303, 1.199719254218462483 ) ) ;
#53924 = CARTESIAN_POINT ( 'NONE',  ( 6.658462837642799670, 7.901199744405670522, 1.082531754730549967 ) ) ;
#53925 = CARTESIAN_POINT ( 'NONE',  ( 5.781250000000004441, 0.7852924748302878566, 1.895863743163952453 ) ) ;
#53926 = CARTESIAN_POINT ( 'NONE',  ( -7.711890448074853133, 7.891627032375787998, -0.7998128361456291469 ) ) ;
#53927 = CARTESIAN_POINT ( 'NONE',  ( 6.683806541412754321, 8.820860269780128604, -1.443375672974058777 ) ) ;
#53928 = CARTESIAN_POINT ( 'NONE',  ( 4.137223920935246824, 7.648466568186386816, 0.7801199165378830402 ) ) ;
#53929 = ADVANCED_FACE ( 'NONE', ( #135583 ), #127764, .T. ) ;
#53930 = CARTESIAN_POINT ( 'NONE',  ( -4.894657149733403045, 5.669187081899118574, -1.199719254218446718 ) ) ;
#53932 = CARTESIAN_POINT ( 'NONE',  ( 3.762163318865581640, 0.7457541186767223662, -2.092641825391368560 ) ) ;
#53931 = CARTESIAN_POINT ( 'NONE',  ( 2.496466685713152334, -1.086271176545396067, 1.821091972856798913 ) ) ;
#53933 = CARTESIAN_POINT ( 'NONE',  ( 1.851786237446376049, 2.185420115623282200, -0.1633297828415938846 ) ) ;
#53934 = CARTESIAN_POINT ( 'NONE',  ( -6.098470168048611306, 6.009303372345148553, 1.040834085586084257E-14 ) ) ;
#53935 = CARTESIAN_POINT ( 'NONE',  ( -4.981695098378565945, 4.776675467721892332, -0.7998128361456362523 ) ) ;
#53936 = CARTESIAN_POINT ( 'NONE',  ( 5.969191311310417802, 1.729517061547349632, 0.9261464158661563140 ) ) ;
#53937 = CARTESIAN_POINT ( 'NONE',  ( -1.201851678989727383E-14, 2.071875000341422801, 1.575800808251672791 ) ) ;
#53938 = CARTESIAN_POINT ( 'NONE',  ( -3.933273961740340496, 5.682181936820735579, 1.443375672974065660 ) ) ;
#53939 = CARTESIAN_POINT ( 'NONE',  ( -4.934804725694220906, 7.740727365743146571, -1.082531754730549967 ) ) ;
#53940 = CARTESIAN_POINT ( 'NONE',  ( 4.043311264919998038, 0.1072909356813686182, 2.118029240109862155 ) ) ;
#53941 = CARTESIAN_POINT ( 'NONE',  ( -4.390861645979385663, 6.216034235099629157, -1.599625672291271394 ) ) ;
#53942 = ORIENTED_EDGE ( 'NONE', *, *, #64855, .F. ) ;
#53944 = CARTESIAN_POINT ( 'NONE',  ( 6.666866396406604167, -1.974176978123330040, -0.8811043787171415342 ) ) ;
#53943 = CARTESIAN_POINT ( 'NONE',  ( -4.489158259900630554, 8.251452046610447510, 0.000000000000000000 ) ) ;
#53945 = CARTESIAN_POINT ( 'NONE',  ( 7.318703993278529829, 7.432909501780090800, 1.040834085586084257E-14 ) ) ;
#53946 = CARTESIAN_POINT ( 'NONE',  ( 5.196754805642953556, 1.508532920973480795, 1.055450849767838539 ) ) ;
#53947 = CARTESIAN_POINT ( 'NONE',  ( -1.402160292154681736E-14, 2.509375000341417028, -1.575800808251660134 ) ) ;
#53948 = CARTESIAN_POINT ( 'NONE',  ( 1.417106933825535986, -0.9663644154882103932, -1.447271084069596370 ) ) ;
#53950 = EDGE_CURVE ( 'NONE', #201145, #37826, #129092, .T. ) ;
#53949 = CARTESIAN_POINT ( 'NONE',  ( 11.44800751629993130, 12.29999999999998295, 3.302956944461088451 ) ) ;
#53951 = DIRECTION ( 'NONE',  ( 1.276756478318932585E-15, -1.000000000000000000, 1.665334536937738262E-16 ) ) ;
#53952 = CARTESIAN_POINT ( 'NONE',  ( 8.992125047306153363, 12.32489318961469316, -7.949360258372097476 ) ) ;
#53953 = CARTESIAN_POINT ( 'NONE',  ( 5.313408243115379292, -0.3210861823062813314, 2.137610926513198617 ) ) ;
#53954 = CARTESIAN_POINT ( 'NONE',  ( -3.438964519360665051, 7.163875705896082913, -0.7998128361456281477 ) ) ;
#53955 = CARTESIAN_POINT ( 'NONE',  ( -6.195713011320783892, 10.17215624660883577, -0.7216878364870267237 ) ) ;
#53956 = CARTESIAN_POINT ( 'NONE',  ( 4.083022661009271914, -0.2092679848491978134, -2.151539631373246220 ) ) ;
#53957 = CARTESIAN_POINT ( 'NONE',  ( 4.868415619454742327, -1.289772430030609707, 1.490937899079747497 ) ) ;
#53958 = CARTESIAN_POINT ( 'NONE',  ( 4.006995869149078793, 1.725434352394356052, 0.1705419362300845121 ) ) ;
#53959 = CARTESIAN_POINT ( 'NONE',  ( 1.048660896456204528, -1.724490848714568259, 1.352309724062021878 ) ) ;
#53960 = CARTESIAN_POINT ( 'NONE',  ( 2.222082089356589130, -2.238238103340572049, 0.5610464132631690637 ) ) ;
#53961 = CARTESIAN_POINT ( 'NONE',  ( 4.095036773856917556, 1.742982576809920303, -1.099142878725319239 ) ) ;
#53962 = CARTESIAN_POINT ( 'NONE',  ( 6.532770933798597746, -1.732582191135303651, 0.8775855664264734513 ) ) ;
#53964 = ORIENTED_EDGE ( 'NONE', *, *, #84877, .T. ) ;
#53963 = CARTESIAN_POINT ( 'NONE',  ( -7.985389288324703294, 9.379004260209384825, -1.082531754730543083 ) ) ;
#53965 = AXIS2_PLACEMENT_3D ( 'NONE', #120525, #204865, #8826 ) ;
#53966 = CARTESIAN_POINT ( 'NONE',  ( -3.983063267364693960, 7.868933921892603323, -0.7998128361456481317 ) ) ;
#53967 = DIRECTION ( 'NONE',  ( 1.000000000000000000, 0.000000000000000000, 1.224646799147353207E-16 ) ) ;
#53968 = CARTESIAN_POINT ( 'NONE',  ( 1.355252715606880543E-15, 3.019799309333501824, -12.05075272264721242 ) ) ;
#53969 = CARTESIAN_POINT ( 'NONE',  ( -6.033015167956800262, 9.021972881716168402, -1.082531754730537976 ) ) ;
#53970 = CARTESIAN_POINT ( 'NONE',  ( 3.522699392456357881, 1.401646575410384843, -1.704459333586107794 ) ) ;
#53971 = CARTESIAN_POINT ( 'NONE',  ( -1.642778471874998480, -2.588541666188707957, 2.845375778867863303 ) ) ;
#53972 = ORIENTED_EDGE ( 'NONE', *, *, #56788, .F. ) ;
#53973 = CARTESIAN_POINT ( 'NONE',  ( 0.2680791809135505410, -0.7890318081985218113, -1.684091100025336463 ) ) ;
#53974 = CARTESIAN_POINT ( 'NONE',  ( -0.1288028175206621384, 0.6694653996850441491, -2.353626493485785343 ) ) ;
#53975 =( NAMED_UNIT ( * ) PLANE_ANGLE_UNIT ( ) SI_UNIT ( $, .RADIAN. ) );
#53976 = FACE_OUTER_BOUND ( 'NONE', #117626, .T. ) ;
#53978 = CARTESIAN_POINT ( 'NONE',  ( 6.825078400183552496, 6.035069422732725286, 2.639236294420511442 ) ) ;
#53977 = CARTESIAN_POINT ( 'NONE',  ( -6.481153920547079395, 6.846182452143763086, -0.6414432093310319383 ) ) ;
#53979 = CARTESIAN_POINT ( 'NONE',  ( 4.871153761480780275, 8.051123856976298399, 0.9350251597124116243 ) ) ;
#53980 = ORIENTED_EDGE ( 'NONE', *, *, #57301, .T. ) ;
#53981 = CARTESIAN_POINT ( 'NONE',  ( 3.520434746236697610, 1.308796515248649817, -1.591936018771279659 ) ) ;
#53982 = CARTESIAN_POINT ( 'NONE',  ( 0.6801582343749813520, 0.2239583336747300035, 1.178068619123796568 ) ) ;
#53983 = CARTESIAN_POINT ( 'NONE',  ( -4.720210035852093533, 8.658662141802762946, -0.7998128361456281477 ) ) ;
#53984 = DIRECTION ( 'NONE',  ( 1.000000000000000000, -0.000000000000000000, -0.000000000000000000 ) ) ;
#53985 = CARTESIAN_POINT ( 'NONE',  ( 4.334856428067313416, 6.080418470877079429, -1.599625672291256295 ) ) ;
#53986 = CARTESIAN_POINT ( 'NONE',  ( 1.586866656640874451, -0.3012919939810917436, -2.038609575755165437 ) ) ;
#53988 = CARTESIAN_POINT ( 'NONE',  ( -1.364683531250010295, 13.13020833367472839, 0.7879004041258445001 ) ) ;
#53987 = CARTESIAN_POINT ( 'NONE',  ( 1.500000000000032641, 7.750000000000000000, 9.886859966642587594 ) ) ;
#53989 = CARTESIAN_POINT ( 'NONE',  ( 6.388916700537700777, 8.476822122092563916, 1.599625672291281386 ) ) ;
#53990 = B_SPLINE_CURVE_WITH_KNOTS ( 'NONE', 1,
 ( #168294, #166153 ),
 .UNSPECIFIED., .F., .F.,
 ( 2, 2 ),
 ( 0.000000000000000000, 0.6655069273901945692 ),
 .UNSPECIFIED. ) ;
#53991 = CARTESIAN_POINT ( 'NONE',  ( 1.792484642137021078, 2.460830816602564752, 2.500000000000000444 ) ) ;
#53992 = CARTESIAN_POINT ( 'NONE',  ( 6.111994396789379280, -2.190734547077430872, 0.2660306753756238041 ) ) ;
#53993 = CARTESIAN_POINT ( 'NONE',  ( 0.9487563388480976245, 0.6265645459165304354, 2.068816658077163861 ) ) ;
#53994 = CARTESIAN_POINT ( 'NONE',  ( -5.612712406377534435, 5.650512016969639895, 0.7216878364870317197 ) ) ;
#53995 = CARTESIAN_POINT ( 'NONE',  ( 0.6730650033222317363, 1.776164188848127878, -0.9548607967814757291 ) ) ;
#53996 = CARTESIAN_POINT ( 'NONE',  ( 1.915759298113205666, 0.7205626639651928622, 2.182595962359680897 ) ) ;
#53997 = DIRECTION ( 'NONE',  ( 0.000000000000000000, 0.000000000000000000, 1.000000000000000000 ) ) ;
#53998 = CARTESIAN_POINT ( 'NONE',  ( -1.115562610750309283E-14, 11.59375000068279604, 1.500000000000001554 ) ) ;
#54000 = ORIENTED_EDGE ( 'NONE', *, *, #89762, .T. ) ;
#53999 = DIRECTION ( 'NONE',  ( 1.000000000000000000, -0.000000000000000000, -0.000000000000000000 ) ) ;
#54001 = CARTESIAN_POINT ( 'NONE',  ( 1.990876257202532695, 1.628914321797021669, -0.9196232060951770038 ) ) ;
#54002 = CARTESIAN_POINT ( 'NONE',  ( 3.380092458137720968, -2.014432998692190058, -0.09411721906785883163 ) ) ;
#54004 = CARTESIAN_POINT ( 'NONE',  ( 6.639320575229258559, 7.052241914652472410, 2.701414248926166994 ) ) ;
#54003 = CARTESIAN_POINT ( 'NONE',  ( -0.6823417656250003738, 0.9677083336747521747, -1.181850606188749264 ) ) ;
#54006 = CARTESIAN_POINT ( 'NONE',  ( 4.600280035732231987, -2.105589688358105782, -0.05227242994678206467 ) ) ;
#54005 = CARTESIAN_POINT ( 'NONE',  ( -8.311311860377216476, 9.655284244316948872, -1.199719254218446718 ) ) ;
#54007 = CARTESIAN_POINT ( 'NONE',  ( 6.714312387265682247, 8.856450423275211037, 1.599625672291281386 ) ) ;
#54009 = CARTESIAN_POINT ( 'NONE',  ( -6.028571859570855729, 10.18508426947466816, 0.000000000000000000 ) ) ;
#54008 = CARTESIAN_POINT ( 'NONE',  ( 5.585032934186686226, 5.480569609498057382, 0.000000000000000000 ) ) ;
#54010 = CARTESIAN_POINT ( 'NONE',  ( -0.4299312922663480752, -6.708819892820486963, -9.481437597266031858 ) ) ;
#54011 = CARTESIAN_POINT ( 'NONE',  ( 3.603775140268844712, 1.465814181579458753, 1.389848736882649094 ) ) ;
#54012 = CARTESIAN_POINT ( 'NONE',  ( 1.499999999999987566, -0.6937499993171849511, 0.000000000000000000 ) ) ;
#54013 = CARTESIAN_POINT ( 'NONE',  ( 1.041928790383022774, 1.382269897723470642, 1.531051681482889393 ) ) ;
#54014 = CARTESIAN_POINT ( 'NONE',  ( 7.456621297836061757, 11.64321591421002644, 0.7216878364870438212 ) ) ;
#54015 = EDGE_CURVE ( 'NONE', #67678, #153088, #156682, .T. ) ;
#54016 = CARTESIAN_POINT ( 'NONE',  ( 5.536455037250767930, 2.128579029500421438, 0.3755436860354774420 ) ) ;
#54017 = CARTESIAN_POINT ( 'NONE',  ( 5.013482942003290255, 9.071090208970993274, -0.7998128361456481317 ) ) ;
#54018 = CARTESIAN_POINT ( 'NONE',  ( -1.402160292154681736E-14, -0.7406249996585823059, -1.575800808251665908 ) ) ;
#54020 = CARTESIAN_POINT ( 'NONE',  ( -0.2106854629475244101, -0.004120941679102127324, -1.996958217618934661 ) ) ;
#54019 = CARTESIAN_POINT ( 'NONE',  ( 4.366607992053101128, 7.252070536440704096, -1.199719254218448494 ) ) ;
#54021 = CARTESIAN_POINT ( 'NONE',  ( 6.602457619730756733, 9.686322408785807525, 1.082531754730558626 ) ) ;
#54023 = FILL_AREA_STYLE ('',( #16157 ) ) ;
#54022 = CARTESIAN_POINT ( 'NONE',  ( 2.752568609338637895, -2.165203543660359387, -0.1620229588487445971 ) ) ;
#54025 = CARTESIAN_POINT ( 'NONE',  ( 1.716098596715152746, 1.718394358364897068, 0.6617865747741287219 ) ) ;
#54024 = CARTESIAN_POINT ( 'NONE',  ( -6.100805936469506641, 6.219954468743612352, 0.7216878364870317197 ) ) ;
#54026 = PRESENTATION_LAYER_ASSIGNMENT (  '', '', ( #71310 ) ) ;
#54027 = CARTESIAN_POINT ( 'NONE',  ( -1.364683531250012516, 3.530208333674758059, 0.7879004041258379498 ) ) ;
#54028 = CARTESIAN_POINT ( 'NONE',  ( 3.773127072069931032, 2.063069237518061705, -0.7396954945804237180 ) ) ;
#54029 = CARTESIAN_POINT ( 'NONE',  ( 3.146123468421266001, 6.442327133617253843, 0.5169845646841256803 ) ) ;
#54030 = CARTESIAN_POINT ( 'NONE',  ( 4.364347144703619286, 1.063191675971109307, 1.997143021516068595 ) ) ;
#54031 = CARTESIAN_POINT ( 'NONE',  ( -5.368138756007025947, 8.350246751061767725, 1.199719254218452047 ) ) ;
#54032 = CARTESIAN_POINT ( 'NONE',  ( -1.364683531250010295, 5.801041667008088432, -0.7879004041258300672 ) ) ;
#54033 = CARTESIAN_POINT ( 'NONE',  ( 6.229241538080760421, 6.920885192246182704, -0.8282608007674150397 ) ) ;
#54034 = CARTESIAN_POINT ( 'NONE',  ( -0.7500000000000179856, 13.29166666666666607, 1.299038105676658228 ) ) ;
#54035 = CARTESIAN_POINT ( 'NONE',  ( -4.760321331729590710, 8.567808963744235839, 0.7216878364870267237 ) ) ;
#54036 = CARTESIAN_POINT ( 'NONE',  ( 4.909461021924231616, 8.741805268971372556, 0.7216878364870317197 ) ) ;
#54037 = EDGE_CURVE ( 'NONE', #57355, #80549, #92917, .T. ) ;
#54038 = CARTESIAN_POINT ( 'NONE',  ( 4.921055611120458195, -0.08698325021493956422, 1.767741905644197642 ) ) ;
#54039 = CARTESIAN_POINT ( 'NONE',  ( 3.475247029965710777, -1.776355867393118126, -0.9471225605895690070 ) ) ;
#54040 = CARTESIAN_POINT ( 'NONE',  ( 7.747594715205354809, 11.12627870345989756, -1.199719254218446718 ) ) ;
#54041 = CARTESIAN_POINT ( 'NONE',  ( 2.344876439239967247, 0.4604487725310001389, 2.054841016598129233 ) ) ;
#54043 = CARTESIAN_POINT ( 'NONE',  ( -0.7499999999999972244, 3.108333333333358706, -1.299038105676652011 ) ) ;
#54042 = CARTESIAN_POINT ( 'NONE',  ( -1.364683531250000748, 11.85937500034139802, 0.000000000000000000 ) ) ;
#54044 = CARTESIAN_POINT ( 'NONE',  ( 2.014047288863869412, 1.964499257916036079, -0.1416769614510370867 ) ) ;
#54045 = CARTESIAN_POINT ( 'NONE',  ( 9.508009452561562824, 4.000000000000000888, 7.612500000000001599 ) ) ;
#54046 = CARTESIAN_POINT ( 'NONE',  ( 8.914213045750530640, 3.487142912321096855, 8.026393478126198744 ) ) ;
#54048 = ORIENTED_EDGE ( 'NONE', *, *, #109604, .F. ) ;
#54047 = CARTESIAN_POINT ( 'NONE',  ( 5.994382934279598452, -0.9612500426990595592, 1.535330125949084135 ) ) ;
#54049 = CARTESIAN_POINT ( 'NONE',  ( 5.775410249741494972, 8.721433810464993996, -1.082531754730537088 ) ) ;
#54050 = CARTESIAN_POINT ( 'NONE',  ( 0.1145072494591141549, 3.480000000000001315, -2.000000000000000000 ) ) ;
#54052 = CARTESIAN_POINT ( 'NONE',  ( 6.034044788248046132, 0.9204803733943857091, -1.628451883209979689 ) ) ;
#54051 = AXIS2_PLACEMENT_3D ( 'NONE', #122606, #109536, #172335 ) ;
#54053 = CARTESIAN_POINT ( 'NONE',  ( 2.530568227245037605, 6.104080031761181857, 0.000000000000000000 ) ) ;
#54054 = CARTESIAN_POINT ( 'NONE',  ( 5.682505902380680318, 1.237739610710281823, -1.659335868388504220 ) ) ;
#54055 = CARTESIAN_POINT ( 'NONE',  ( -3.956095110007852622E-14, 2.937500000000021760, -1.414508159514583419 ) ) ;
#54056 = CARTESIAN_POINT ( 'NONE',  ( -6.251718229232867685, 6.466295153626015590, -0.7216878364870338292 ) ) ;
#54057 = DIRECTION ( 'NONE',  ( -0.7592566023653016805, 0.6507913734559627184, 0.000000000000000000 ) ) ;
#54059 = CARTESIAN_POINT ( 'NONE',  ( -1.500000000000001332, 0.9000000000000187850, 0.000000000000000000 ) ) ;
#54058 = CONICAL_SURFACE ( 'NONE', #164755, 4.000000000000000000, 0.8960553845713404852 ) ;
#54060 = CARTESIAN_POINT ( 'NONE',  ( 6.903072767652295383, 11.20533532890304684, 1.040834085586084257E-14 ) ) ;
#54061 = CARTESIAN_POINT ( 'NONE',  ( -7.669108446824431269, 12.09904362127053545, -0.7998128361456291469 ) ) ;
#54062 = CARTESIAN_POINT ( 'NONE',  ( 6.150558962454855561, 7.204682206732687000, 1.199719254218452047 ) ) ;
#54063 = EDGE_CURVE ( 'NONE', #69090, #183003, #46087, .T. ) ;
#54064 = CARTESIAN_POINT ( 'NONE',  ( -0.6823417656250246877, 0.5510416670080897639, 1.181850606188755259 ) ) ;
#54065 = CARTESIAN_POINT ( 'NONE',  ( 1.499999999999987121, 1.795833333333355819, -0.8660254037844253849 ) ) ;
#54067 = CARTESIAN_POINT ( 'NONE',  ( 4.741601036477289810, 6.554953847355395880, 1.599625672291267398 ) ) ;
#54066 = CARTESIAN_POINT ( 'NONE',  ( 4.932062528313536198, 1.127988425013145779, 1.604980062286972542 ) ) ;
#54068 = EDGE_CURVE ( 'NONE', #29554, #66830, #108344, .T. ) ;
#54069 = CARTESIAN_POINT ( 'NONE',  ( 3.163435312993330140, -0.5825663732807913053, -1.930122257003751063 ) ) ;
#54070 = CARTESIAN_POINT ( 'NONE',  ( 2.131924177892559058, 1.915402082336896461, 0.04262488632780260522 ) ) ;
#54071 = CARTESIAN_POINT ( 'NONE',  ( 0.2577194443907256383, 2.166829308800602316, -0.3276212646995610989 ) ) ;
#54072 = CARTESIAN_POINT ( 'NONE',  ( 0.1333692844072316419, 7.629137130509075604, -2.653547345224521514 ) ) ;
#54073 = CARTESIAN_POINT ( 'NONE',  ( 1.686563950722594685, -0.2693046698774223535, -1.850923959389898288 ) ) ;
#54074 = CARTESIAN_POINT ( 'NONE',  ( -1.001543065824772872E-14, 4.821875000341419693, 1.575800808251672791 ) ) ;
#54075 = CARTESIAN_POINT ( 'NONE',  ( 4.500248159151196248, -0.9453760218497176959, 1.777399672076788617 ) ) ;
#54076 = CARTESIAN_POINT ( 'NONE',  ( -8.453672473320708036, 9.821371626084353323, -1.199719254218446718 ) ) ;
#54078 = CARTESIAN_POINT ( 'NONE',  ( 4.359064374566766986, -0.001685027751544953406, -2.117403152337670846 ) ) ;
#54077 = CARTESIAN_POINT ( 'NONE',  ( -6.087247782855839340, 6.204136622861004646, 0.000000000000000000 ) ) ;
#54079 = DIRECTION ( 'NONE',  ( 1.000000000000000000, 0.000000000000000000, 0.000000000000000000 ) ) ;
#54080 = CARTESIAN_POINT ( 'NONE',  ( 6.144996677366851401, -0.2998803957653916608, -2.048400609436632269 ) ) ;
#54082 = CARTESIAN_POINT ( 'NONE',  ( 4.015551651036665781, 7.573759128756977432, -0.3041731733383628566 ) ) ;
#54081 = CARTESIAN_POINT ( 'NONE',  ( 0.6442209307526406414, 0.6107738465899931191, 1.999526160293135568 ) ) ;
#54084 = ORIENTED_EDGE ( 'NONE', *, *, #37600, .T. ) ;
#54083 = CARTESIAN_POINT ( 'NONE',  ( 6.475623784153278883, 1.746001614453606576, -0.5331787911772439825 ) ) ;
#54085 = CARTESIAN_POINT ( 'NONE',  ( 5.940443861082012944, 10.08226827123770697, 0.7998128361456462443 ) ) ;
#54086 = CARTESIAN_POINT ( 'NONE',  ( 8.002408263929950749, -6.836568542494916301, -7.346809171966858010 ) ) ;
#54087 = LINE ( 'NONE', #151596, #3073 ) ;
#54088 = CARTESIAN_POINT ( 'NONE',  ( 6.114364089638782751, 9.116879957011832403, 1.082531754730558626 ) ) ;
#54089 = CARTESIAN_POINT ( 'NONE',  ( -1.914442667406964116, 3.262253226107984183, 0.4355078757043848170 ) ) ;
#54091 = CARTESIAN_POINT ( 'NONE',  ( 1.031567638852897373, -1.767431343716918013, 0.3961611186833951526 ) ) ;
#54090 = CARTESIAN_POINT ( 'NONE',  ( 7.666209513884374438, 7.908608952478760834, 0.7998128361456281477 ) ) ;
#54093 = CARTESIAN_POINT ( 'NONE',  ( -8.453672473320708036, 9.821371626084353323, -1.199719254218446718 ) ) ;
#54092 = VECTOR ( 'NONE', #152908, 1000.000000000000000 ) ;
#54094 = CARTESIAN_POINT ( 'NONE',  ( 5.005985031943777308, 6.863401842066294556, -1.599625672291256295 ) ) ;
#54095 = CARTESIAN_POINT ( 'NONE',  ( 0.09510031644101717141, -6.698521824825868443, 10.99968117833243042 ) ) ;
#54096 = CARTESIAN_POINT ( 'NONE',  ( -0.7500000000000006661, 12.23958333401613174, -1.299038105676657340 ) ) ;
#54097 = CARTESIAN_POINT ( 'NONE',  ( 2.347533153460546806, 5.890539112345938300, 0.000000000000000000 ) ) ;
#54098 = ORIENTED_EDGE ( 'NONE', *, *, #89413, .F. ) ;
#54099 = AXIS2_PLACEMENT_3D ( 'NONE', #183683, #66695, #118746 ) ;
#54100 = CARTESIAN_POINT ( 'NONE',  ( 5.888296041240274725, -0.7283935311428509918, -1.880430420734761965 ) ) ;
#54101 = CARTESIAN_POINT ( 'NONE',  ( 0.8914570141239013257, -0.05588796005432519753, -2.119924415460701983 ) ) ;
#54102 = CARTESIAN_POINT ( 'NONE',  ( 1.157928058570472318, -6.779921613290400011E-15, -0.6014056109540196760 ) ) ;
#54103 = CARTESIAN_POINT ( 'NONE',  ( 2.273922426215241099, 5.667243959216540006, 0.4897358640176532329 ) ) ;
#54104 = CARTESIAN_POINT ( 'NONE',  ( -1.561525566895192618, 8.688907412369037075, -2.501944002935404310 ) ) ;
#54105 = CARTESIAN_POINT ( 'NONE',  ( -5.260200412422213923, 6.199617238323108737, -1.082531754730544860 ) ) ;
#54106 = CARTESIAN_POINT ( 'NONE',  ( 8.256552361042350796, 12.57646882128404187, 1.040834085586084257E-14 ) ) ;
#54107 = CARTESIAN_POINT ( 'NONE',  ( 3.573067284968055812, 1.778583338327298646, 0.8461400097728142278 ) ) ;
#54108 = CARTESIAN_POINT ( 'NONE',  ( 4.798453934790239295, 1.388474963651475269, -1.462457531588717830 ) ) ;
#54109 = CARTESIAN_POINT ( 'NONE',  ( -6.287230548435221777, 8.358188277972981695, -1.599625672291263179 ) ) ;
#54110 = LINE ( 'NONE', #60232, #31394 ) ;
#54111 = CARTESIAN_POINT ( 'NONE',  ( 6.727182134110194944, 2.413774403037728167, 2.569658639860139093 ) ) ;
#54112 = CIRCLE ( 'NONE', #81785, 0.07999999999999983513 ) ;
#54113 = CARTESIAN_POINT ( 'NONE',  ( 5.033237522093748417, -1.548190877955179179, -1.551241237171486098 ) ) ;
#54114 = CARTESIAN_POINT ( 'NONE',  ( 6.518203450479836292, 5.167241622962441383, 2.437504649502901355 ) ) ;
#54115 = CARTESIAN_POINT ( 'NONE',  ( 3.082943253306829057, -0.1403151614269258773, -1.921328324580730440 ) ) ;
#54116 = CARTESIAN_POINT ( 'NONE',  ( -6.157374318900681764, 10.33535380535947290, 0.7998128361456481317 ) ) ;
#54117 = CARTESIAN_POINT ( 'NONE',  ( -0.1294898018151836583, 0.7212281881416956475, -2.008332099035778917 ) ) ;
#54118 = CARTESIAN_POINT ( 'NONE',  ( 0.1331565106231571705, 2.881392620029461504, -2.434650611646618223 ) ) ;
#54119 = EDGE_LOOP ( 'NONE', ( #41943, #204692, #175033, #37200 ) ) ;
#54120 = CARTESIAN_POINT ( 'NONE',  ( 4.665414256878284149, 6.536345614481700927, -1.443375672974068769 ) ) ;
#54121 = CARTESIAN_POINT ( 'NONE',  ( 4.698083300297758669, 0.8457734583860087030, -1.778757171186759134 ) ) ;
#54122 = ORIENTED_EDGE ( 'NONE', *, *, #86771, .T. ) ;
#54124 = CARTESIAN_POINT ( 'NONE',  ( 3.527992865196138972, -1.982922396879973626, 0.3464002264041438073 ) ) ;
#54123 = CARTESIAN_POINT ( 'NONE',  ( 0.6263844939735198070, 0.1443197301355322315, 1.936771776935701794 ) ) ;
#54125 = CARTESIAN_POINT ( 'NONE',  ( 5.923294579110739200, 0.9235710928677911546, 2.104827929701275302 ) ) ;
#54127 = CARTESIAN_POINT ( 'NONE',  ( 3.819077715518546690, -1.639399709636097713, -0.8806717989592935947 ) ) ;
#54126 = CARTESIAN_POINT ( 'NONE',  ( -4.137366601288475110, 8.820714325924946309, -0.7750000000000000222 ) ) ;
#54128 = CARTESIAN_POINT ( 'NONE',  ( 5.040599249230596435, 9.102725900736217568, 0.7998128361456341429 ) ) ;
#54129 = CYLINDRICAL_SURFACE ( 'NONE', #8654, 12.00000000000000178 ) ;
#54130 = EDGE_CURVE ( 'NONE', #107270, #179291, #137181, .T. ) ;
#54131 = DIRECTION ( 'NONE',  ( 0.000000000000000000, 1.000000000000000000, 0.000000000000000000 ) ) ;
#54132 = CARTESIAN_POINT ( 'NONE',  ( -6.181627972826976958, 9.299317504018391745, 1.199719254218452047 ) ) ;
#54133 = CARTESIAN_POINT ( 'NONE',  ( -5.668717624289589807, 5.786127781192186958, 0.7216878364870257245 ) ) ;
#54134 = CARTESIAN_POINT ( 'NONE',  ( 0.5916818631664167993, -0.7834642122952638621, 2.046923429677327100 ) ) ;
#54135 = CARTESIAN_POINT ( 'NONE',  ( 5.341549334104188418, 7.254893527920112994, 1.443375672974062551 ) ) ;
#54136 = CARTESIAN_POINT ( 'NONE',  ( 0.3866926556111174862, 2.897682894409570054, 2.027578619373079594 ) ) ;
#54137 = CARTESIAN_POINT ( 'NONE',  ( 0.000000000000000000, 0.000000000000000000, 0.000000000000000000 ) ) ;
#54138 = CARTESIAN_POINT ( 'NONE',  ( 0.09986456629675066754, -1.825204794925545881, -0.04862044751281074939 ) ) ;
#54139 = CARTESIAN_POINT ( 'NONE',  ( -3.262708522383007903, 6.958243709422141876, 1.040834085586084257E-14 ) ) ;
#54140 = CARTESIAN_POINT ( 'NONE',  ( 2.900671442982618142, -0.8568821622233543378, -1.507568437789049032 ) ) ;
#54141 = CARTESIAN_POINT ( 'NONE',  ( -10.32992389895503393, 1.000000000000000888, -6.106772653521458594 ) ) ;
#54142 = CARTESIAN_POINT ( 'NONE',  ( 6.609000000000012420, 2.456927087449762404, 2.283703893460458989 ) ) ;
#54143 = CARTESIAN_POINT ( 'NONE',  ( -4.855791571988752331, 8.816840600628864877, 0.7998128361456481317 ) ) ;
#54144 = CARTESIAN_POINT ( 'NONE',  ( -5.903988413730030693, 6.004926949446717011, -0.1838238861417510472 ) ) ;
#54145 = CARTESIAN_POINT ( 'NONE',  ( 6.059193749186201572, -1.568369423792463024, -0.9343120793870243190 ) ) ;
#54146 = CARTESIAN_POINT ( 'NONE',  ( 3.713678095275750657, 0.4809820416172749802, -1.901733992618503066 ) ) ;
#54147 = CARTESIAN_POINT ( 'NONE',  ( -0.6125000000000053735, -1.145833332650537884, 1.060881119635925796 ) ) ;
#54148 = CARTESIAN_POINT ( 'NONE',  ( -9.341731535015849630, 10.85744053139533349, 1.199719254218462483 ) ) ;
#54149 = CARTESIAN_POINT ( 'NONE',  ( 7.263417608619159083, 9.497073181520933716, -1.599625672291262513 ) ) ;
#54150 = CARTESIAN_POINT ( 'NONE',  ( 3.281995766809755466, 2.068381274212594878, -0.4664580258975092875 ) ) ;
#54151 = CARTESIAN_POINT ( 'NONE',  ( 8.167861197590044142, 8.493869250135347215, 0.000000000000000000 ) ) ;
#54152 = CARTESIAN_POINT ( 'NONE',  ( -9.053093885623068715, 11.58502883802551153, -1.599625672291263179 ) ) ;
#54153 = CARTESIAN_POINT ( 'NONE',  ( 2.026315959858393967, 1.060668813445601044, 1.777738962378045295 ) ) ;
#54155 = CARTESIAN_POINT ( 'NONE',  ( -1.500000000000001110, 14.80208333401612997, 0.8660254037844419273 ) ) ;
#54154 = CARTESIAN_POINT ( 'NONE',  ( -11.97185388258315086, 11.37999990720392418, 0.8311143155443556640 ) ) ;
#54157 = EDGE_LOOP ( 'NONE', ( #201472, #22586 ) ) ;
#54156 = CARTESIAN_POINT ( 'NONE',  ( 4.705860574468672120, 1.645629519818484932, 1.492201155203516150 ) ) ;
#54158 = CARTESIAN_POINT ( 'NONE',  ( 1.512731952202387653, -2.162554957723664462, 0.7796286979407650586 ) ) ;
#54159 = CARTESIAN_POINT ( 'NONE',  ( 9.571693261567965294, 10.26932301469188857, 0.7216878364870438212 ) ) ;
#54161 = CARTESIAN_POINT ( 'NONE',  ( -3.285556943750000070, -2.209374999522041527, 0.000000000000000000 ) ) ;
#54160 = CARTESIAN_POINT ( 'NONE',  ( 5.858531774880875176, 9.849054480754103835, -0.7216878364870458196 ) ) ;
#54162 = SURFACE_SIDE_STYLE ('',( #50963 ) ) ;
#54163 = EDGE_LOOP ( 'NONE', ( #108356, #145038, #171104, #152327 ) ) ;
#54164 = CARTESIAN_POINT ( 'NONE',  ( -5.426287360647527258, 6.306760859481674864, -1.047964138152550406 ) ) ;
#54165 = CARTESIAN_POINT ( 'NONE',  ( 2.759904966095374501, 0.6844231338998980618, -1.785916880244736715 ) ) ;
#54166 = CARTESIAN_POINT ( 'NONE',  ( -0.1822957779078477336, 6.496859778797933416, -3.113708315861777098 ) ) ;
#54167 = CARTESIAN_POINT ( 'NONE',  ( 4.436358534413815669, 1.691719876958649227, 0.3350348670820638142 ) ) ;
#54168 = CARTESIAN_POINT ( 'NONE',  ( 1.868375392651611122, -1.978555653031977446, -0.3886301775877995524 ) ) ;
#54169 = CARTESIAN_POINT ( 'NONE',  ( 3.463815647965732936, -2.215898795117266840, -0.6112515151598179042 ) ) ;
#54170 = CARTESIAN_POINT ( 'NONE',  ( 6.533818191484063398, -1.374270492279753286, -1.595981979862278077 ) ) ;
#54171 = CARTESIAN_POINT ( 'NONE',  ( -5.072158865288277418, 7.010880990960010273, 1.443375672974058777 ) ) ;
#54172 = CARTESIAN_POINT ( 'NONE',  ( 5.307753102408475421, -1.761140305208692913, 0.1738094965475830145 ) ) ;
#54174 = CARTESIAN_POINT ( 'NONE',  ( 1.166458296791187621, -1.450650017800562575, 1.774850106915156100 ) ) ;
#54173 = CARTESIAN_POINT ( 'NONE',  ( 6.444921918449731280, 8.612437886315108315, 1.599625672291268286 ) ) ;
#54175 = CARTESIAN_POINT ( 'NONE',  ( 0.3041415704291222100, 1.511679331021776207, 0.8621369596173468208 ) ) ;
#54176 = CARTESIAN_POINT ( 'NONE',  ( -4.029797971759847997, 5.724516938518342535, -1.599625672291256295 ) ) ;
#54177 = CARTESIAN_POINT ( 'NONE',  ( 5.455090197064776270, 0.4301712223657681022, -2.148646160378755443 ) ) ;
#54178 = CARTESIAN_POINT ( 'NONE',  ( -6.466312919074983512, 6.508729591867735031, -0.7998128361456362523 ) ) ;
#54179 = CARTESIAN_POINT ( 'NONE',  ( -0.6801582343750559589, -0.03645833299194961574, 1.178068619123796568 ) ) ;
#54180 = CARTESIAN_POINT ( 'NONE',  ( -0.08000000000000367928, -9.746166700180788567, -9.579665964948867796 ) ) ;
#54181 = CARTESIAN_POINT ( 'NONE',  ( 6.672334155782003506, -0.9722939650993901450, -1.827837255792996718 ) ) ;
#54182 = CARTESIAN_POINT ( 'NONE',  ( 0.7609543035823238544, -0.05432987398422234326, -2.015980609757315190 ) ) ;
#54183 = CARTESIAN_POINT ( 'NONE',  ( 1.499999999999987566, -1.193749999317185395, 0.000000000000000000 ) ) ;
#54184 = CARTESIAN_POINT ( 'NONE',  ( 4.231024032915966515, 0.09596189134018082156, 1.924231256547383362 ) ) ;
#54185 = CARTESIAN_POINT ( 'NONE',  ( -1.364683531250014514, 11.33854166700806410, -0.7879004041258335089 ) ) ;
#54186 = CARTESIAN_POINT ( 'NONE',  ( 0.8619570425896695420, -1.755772037458620316, -1.360811342731186979 ) ) ;
#54188 = VERTEX_POINT ( 'NONE', #76954 ) ;
#54187 = CARTESIAN_POINT ( 'NONE',  ( 10.55232363013785246, 11.20546574478267132, 0.000000000000000000 ) ) ;
#54190 = CARTESIAN_POINT ( 'NONE',  ( 0.07727525906045540349, 7.079397053215386038, -2.120984693056187531 ) ) ;
#54189 = CARTESIAN_POINT ( 'NONE',  ( 1.123270288250309834, 2.971052654332832610, -0.7749999999993620881 ) ) ;
#54191 = CARTESIAN_POINT ( 'NONE',  ( -3.765305043611756552, 7.354576300424668922, -0.6638232778202641793 ) ) ;
#54192 = CARTESIAN_POINT ( 'NONE',  ( 2.544126380858701797, 6.119897877643793116, 0.7998128361456462443 ) ) ;
#54193 = CARTESIAN_POINT ( 'NONE',  ( -10.50000000000000000, 10.90000000000000036, -3.600000000000002309 ) ) ;
#54194 = CARTESIAN_POINT ( 'NONE',  ( 0.1831564129048668388, 7.629137130509052511, -2.545826866328745997 ) ) ;
#54195 = CARTESIAN_POINT ( 'NONE',  ( 3.807932448155851191, 1.227607710457185197, -1.234010206841095636 ) ) ;
#54197 = EDGE_CURVE ( 'NONE', #179060, #14542, #3016, .T. ) ;
#54196 = CARTESIAN_POINT ( 'NONE',  ( 2.910546574502240968, 0.6583626327048962557, 1.848246418561696913 ) ) ;
#54199 = CARTESIAN_POINT ( 'NONE',  ( -1.364683531249997417, 3.071875000341423245, 1.214306433183764966E-14 ) ) ;
#54198 = CARTESIAN_POINT ( 'NONE',  ( 6.094553744542824170, 7.069066442510145265, 1.199719254218462483 ) ) ;
#54200 = CARTESIAN_POINT ( 'NONE',  ( -4.836546220603817225, 6.746162335969787094, 1.249072166269946216 ) ) ;
#54201 = CARTESIAN_POINT ( 'NONE',  ( 9.541187415715040032, 12.15447128979948310, -1.599625672291262513 ) ) ;
#54202 = AXIS2_PLACEMENT_3D ( 'NONE', #90986, #158114, #75782 ) ;
#54203 = CARTESIAN_POINT ( 'NONE',  ( 0.1509074155349584279, -0.4535863444464246497, -2.019966333402842817 ) ) ;
#54204 = CARTESIAN_POINT ( 'NONE',  ( -7.157815033010924921, 10.43820240756634199, 1.199719254218453823 ) ) ;
#54205 =( BOUNDED_SURFACE ( )  B_SPLINE_SURFACE ( 3, 3, ( 
 ( #99450, #131988, #214210, #31258, #16031, #83177, #181738, #97332, #115748, #195882, #33369 ),
 ( #165507, #79987, #211038, #78913, #161252, #194805, #180688, #34434, #62664, #30180, #199045 ),
 ( #82115, #163390, #197997, #66904, #48578, #14964, #32313, #50692, #17099, #98381, #130947 ),
 ( #164444, #149260, #838, #81061, #148208, #96271, #145035, #116816, #46441, #129897, #162321 ),
 ( #133044, #128823, #147146, #112560, #47520, #182818, #113633, #146091, #213172, #212102, #64801 ),
 ( #63739, #179638, #196938, #114694, #22436, #18171, #2983, #103724, #20313, #203319, #153539 ),
 ( #84258, #69050, #101576, #21364, #88546, #102652, #52824, #135170, #122193, #36566, #168709 ) ),
 .UNSPECIFIED., .T., .F., .T. ) 
 B_SPLINE_SURFACE_WITH_KNOTS ( ( 4, 3, 4 ),
 ( 4, 1, 1, 1, 1, 1, 1, 1, 4 ),
 ( 0.000000000000000000, 0.5000000000000000000, 1.000000000000000000 ),
 ( 0.000000000000000000, 0.2255509035172358623, 0.3975895543896152406, 0.5252637114030099807, 0.6177357421269481508, 0.6841390318922365710, 0.7334310489036851566, 0.7741974304450970346, 1.000000000000000000 ),
 .UNSPECIFIED. ) 
 GEOMETRIC_REPRESENTATION_ITEM ( )  RATIONAL_B_SPLINE_SURFACE ( (
 ( 1.000000000000000000, 1.000000000000000000, 1.000000000000000000, 1.000000000000000000, 1.000000000000000444, 0.9999999999999997780, 1.000000000000000000, 1.000000000000000000, 1.000000000000000000, 1.000000000000000000, 1.000000000000000000),
 ( 0.3333333333333333703, 0.3333333333333333703, 0.3333333333333332593, 0.3333333333333334814, 0.3333333333333334814, 0.3333333333333333148, 0.3333333333333333703, 0.3333333333333333703, 0.3333333333333333703, 0.3333333333333334259, 0.3333333333333333703),
 ( 0.3333333333333333703, 0.3333333333333333703, 0.3333333333333332593, 0.3333333333333334814, 0.3333333333333334814, 0.3333333333333333148, 0.3333333333333333703, 0.3333333333333333703, 0.3333333333333333703, 0.3333333333333334259, 0.3333333333333333703),
 ( 1.000000000000000000, 1.000000000000000000, 1.000000000000000000, 1.000000000000000000, 1.000000000000000444, 0.9999999999999997780, 1.000000000000000000, 1.000000000000000000, 1.000000000000000000, 1.000000000000000000, 1.000000000000000000),
 ( 0.3333333333333333703, 0.3333333333333333703, 0.3333333333333332593, 0.3333333333333334814, 0.3333333333333334814, 0.3333333333333333148, 0.3333333333333333703, 0.3333333333333333703, 0.3333333333333333703, 0.3333333333333334259, 0.3333333333333333703),
 ( 0.3333333333333333703, 0.3333333333333333703, 0.3333333333333332593, 0.3333333333333334814, 0.3333333333333334814, 0.3333333333333333148, 0.3333333333333333703, 0.3333333333333333703, 0.3333333333333333703, 0.3333333333333334259, 0.3333333333333333703),
 ( 1.000000000000000000, 1.000000000000000000, 1.000000000000000000, 1.000000000000000000, 1.000000000000000444, 0.9999999999999997780, 1.000000000000000000, 1.000000000000000000, 1.000000000000000000, 1.000000000000000000, 1.000000000000000000) ) ) 
 REPRESENTATION_ITEM ( '' )  SURFACE ( )  );
#54206 = CARTESIAN_POINT ( 'NONE',  ( -5.056828107772866510, 5.962349549565537643, -1.082531754730543971 ) ) ;
#54207 = CARTESIAN_POINT ( 'NONE',  ( 5.190638768449240992, 1.523797776992100284, -1.320824044268428255 ) ) ;
#54208 = CARTESIAN_POINT ( 'NONE',  ( 0.7962373781299083575, -0.8115885651059464578, 2.112105989495225877 ) ) ;
#54210 = VERTEX_POINT ( 'NONE', #125805 ) ;
#54209 = CARTESIAN_POINT ( 'NONE',  ( -5.392392409933270514, 7.314210449720692786, 1.599625672291269396 ) ) ;
#54211 = CARTESIAN_POINT ( 'NONE',  ( -0.7500000000000215383, 0.4729166673494850093, 1.299038105676659116 ) ) ;
#54212 = CARTESIAN_POINT ( 'NONE',  ( 1.669004442688322154, 0.1428430569143137041, -1.865171992484420338 ) ) ;
#54213 = CARTESIAN_POINT ( 'NONE',  ( 0.6329805529394582075, 0.5017471949167272571, 1.659931108299773639 ) ) ;
#54215 = CARTESIAN_POINT ( 'NONE',  ( 4.546525781634036534, -1.759932548463913671, 1.305750774140898685 ) ) ;
#54214 = CARTESIAN_POINT ( 'NONE',  ( -1.360316468750008667, 2.369791667008076974, -0.7853790794159001276 ) ) ;
#54216 = CARTESIAN_POINT ( 'NONE',  ( 5.596783072813162896, -0.5536939349623200002, -2.240073236831362280 ) ) ;
#54217 = CARTESIAN_POINT ( 'NONE',  ( 0.4091470207043126917, 1.792883176943863122, 1.016159331636699470 ) ) ;
#54218 = CARTESIAN_POINT ( 'NONE',  ( 3.380740619721524620, 1.755215216048062521, -0.8311813869739079763 ) ) ;
#54219 = CARTESIAN_POINT ( 'NONE',  ( -4.894130264408878439, 4.812166184672871161, -0.7216878364870197293 ) ) ;
#54220 = CARTESIAN_POINT ( 'NONE',  ( 0.4702634422546589366, 7.494255424137728383, -4.464191613399470349 ) ) ;
#54222 = ADVANCED_FACE ( 'NONE', ( #59647 ), #192831, .T. ) ;
#54221 = CARTESIAN_POINT ( 'NONE',  ( 3.770576118376306241, 6.452737000530752276, 1.082531754730549078 ) ) ;
#54223 = CARTESIAN_POINT ( 'NONE',  ( 1.360316468749988683, 0.2656250003413990202, -1.387778780781445676E-14 ) ) ;
#54224 = CARTESIAN_POINT ( 'NONE',  ( 4.746720300533005421, 1.994071680685698400, -0.2986252114312442640 ) ) ;
#54225 = CARTESIAN_POINT ( 'NONE',  ( -4.595850884908229794, 4.464173575255435011, 0.7216878364870317197 ) ) ;
#54226 = CARTESIAN_POINT ( 'NONE',  ( -5.875479466675803231, 7.948088359245467416, -1.599625672291271394 ) ) ;
#54227 = CARTESIAN_POINT ( 'NONE',  ( 9.433775957010412938, 9.900493459467314850, 0.000000000000000000 ) ) ;
#54229 = DIRECTION ( 'NONE',  ( 0.2275916378995520295, -0.8825604872558504566, -0.4114474847327602713 ) ) ;
#54228 = CARTESIAN_POINT ( 'NONE',  ( 1.330379832379691818, 1.758967509726565792, 0.4888242021733391618 ) ) ;
#54230 = CARTESIAN_POINT ( 'NONE',  ( -5.123001941117347080, 7.070197912760590064, 1.599625672291263179 ) ) ;
#54231 = CARTESIAN_POINT ( 'NONE',  ( -5.991777542596674166, 5.955104985976372944, 0.000000000000000000 ) ) ;
#54232 = CARTESIAN_POINT ( 'NONE',  ( -10.52476609942256758, 3.676887381874808902, 5.198941853688804571 ) ) ;
#54233 = EDGE_LOOP ( 'NONE', ( #109194, #88953, #86656, #28151, #152869 ) ) ;
#54234 = CARTESIAN_POINT ( 'NONE',  ( 0.09294085500742564621, -0.4768749645070144982, -2.116232079886640971 ) ) ;
#54235 = CARTESIAN_POINT ( 'NONE',  ( -5.112833325684904118, 8.979072956692109031, -0.7216878364870338292 ) ) ;
#54236 = CARTESIAN_POINT ( 'NONE',  ( -6.781144757626059061, -7.161464053357560644, 6.776370306708066948 ) ) ;
#54237 = CARTESIAN_POINT ( 'NONE',  ( -9.592557376868645846, 11.15007068022363157, -1.199719254218441611 ) ) ;
#54238 = CARTESIAN_POINT ( 'NONE',  ( 5.865880358592049149, 0.5843737978505449959, -1.933295926576389379 ) ) ;
#54240 = ORIENTED_EDGE ( 'NONE', *, *, #56647, .T. ) ;
#54239 = CARTESIAN_POINT ( 'NONE',  ( 5.654997643673960184, 0.4312606369310955645, 2.178877383265501066 ) ) ;
#54241 = CARTESIAN_POINT ( 'NONE',  ( -4.516801452008150086, 5.298631777878131111, 1.199719254218452935 ) ) ;
#54242 = CARTESIAN_POINT ( 'NONE',  ( 5.867981556616276073, 5.740399992340775803, -0.7998128361456281477 ) ) ;
#54243 = CARTESIAN_POINT ( 'NONE',  ( 5.383688703920392449, 1.382483038487541283, 1.528581890270568122 ) ) ;
#54244 = CARTESIAN_POINT ( 'NONE',  ( 4.043592392309851569, -1.492256208629010761, 1.356298961253152413 ) ) ;
#54245 = ORIENTED_EDGE ( 'NONE', *, *, #124333, .T. ) ;
#54246 = ORIENTED_EDGE ( 'NONE', *, *, #66712, .F. ) ;
#54247 = FACE_OUTER_BOUND ( 'NONE', #42829, .T. ) ;
#54248 = CARTESIAN_POINT ( 'NONE',  ( 3.541704441667858472, 5.155074486744371853, -1.599625672291262513 ) ) ;
#54249 = CIRCLE ( 'NONE', #23131, 4.000000000000000000 ) ;
#54251 = ORIENTED_EDGE ( 'NONE', *, *, #34448, .T. ) ;
#54250 = CARTESIAN_POINT ( 'NONE',  ( -6.095272577795516789, 9.268845886473535245, 1.199719254218452047 ) ) ;
#54252 = CARTESIAN_POINT ( 'NONE',  ( 4.636584873806110174, 8.438537862545894441, 0.4145994950837776916 ) ) ;
#54253 = CARTESIAN_POINT ( 'NONE',  ( 4.165388622617651748, -0.6297791189726584804, -1.915306643112117291 ) ) ;
#54254 = CARTESIAN_POINT ( 'NONE',  ( 3.908013947242465314, 1.300727540704300633, -1.303293010247716488 ) ) ;
#54255 = CARTESIAN_POINT ( 'NONE',  ( 4.542476715900265916, 4.951051008190067826, -0.8264431066547142102 ) ) ;
#54256 = CARTESIAN_POINT ( 'NONE',  ( 2.596638674903679167, -2.301597171833298372, -0.1684899434626195847 ) ) ;
#54257 = CARTESIAN_POINT ( 'NONE',  ( 3.464990776744291345, 6.200183785247111778, 1.199719254218452047 ) ) ;
#54258 = CARTESIAN_POINT ( 'NONE',  ( 5.202478051755599964, -0.7228594145181690411, -2.037298988101433839 ) ) ;
#54259 = CARTESIAN_POINT ( 'NONE',  ( 8.932124273304774320, 9.315233161810734686, 0.7998128361456462443 ) ) ;
#54260 = CARTESIAN_POINT ( 'NONE',  ( 6.497600353373155002, -1.840680978339729545, 0.05264081064878384231 ) ) ;
#54261 = CARTESIAN_POINT ( 'NONE',  ( -5.005985031943793295, 6.863401842066301661, -1.599625672291256295 ) ) ;
#54262 = AXIS2_PLACEMENT_3D ( 'NONE', #69116, #123330, #185009 ) ;
#54263 = CARTESIAN_POINT ( 'NONE',  ( -4.836645478815604804, 15.51845284201978004, 10.99103774147543255 ) ) ;
#54264 = DIRECTION ( 'NONE',  ( -6.695352868347761696E-17, 0.000000000000000000, -1.000000000000000000 ) ) ;
#54265 = CARTESIAN_POINT ( 'NONE',  ( 2.799504582125960095, -0.5885537693137884441, 1.775713401224961574 ) ) ;
#54266 = CARTESIAN_POINT ( 'NONE',  ( 6.684453674706574589, -1.933370886519528264, -0.3848441959667763257 ) ) ;
#54268 = CARTESIAN_POINT ( 'NONE',  ( -6.994027139803241866, 9.253060644560830994, -1.599625672291271394 ) ) ;
#54267 = CARTESIAN_POINT ( 'NONE',  ( -1.364683531250010295, 5.738541667008088432, -0.7879004041258300672 ) ) ;
#54269 = CARTESIAN_POINT ( 'NONE',  ( 1.946200625105892312, 0.8427435547867198062, -2.039832142532324255 ) ) ;
#54270 = ORIENTED_EDGE ( 'NONE', *, *, #104314, .T. ) ;
#54271 = DIRECTION ( 'NONE',  ( 1.224646799147353454E-16, 0.000000000000000000, -1.000000000000000000 ) ) ;
#54272 = CARTESIAN_POINT ( 'NONE',  ( 4.111146893441827821, 5.819424013814004759, 1.599625672291267398 ) ) ;
#54273 = CARTESIAN_POINT ( 'NONE',  ( -5.759516327706961647, 5.613857225279885732, -0.7998128361456221525 ) ) ;
#54274 = CARTESIAN_POINT ( 'NONE',  ( 11.86685672517501899, 13.60918917859810584, 1.056525322636017172 ) ) ;
#54275 = CARTESIAN_POINT ( 'NONE',  ( 6.526250059115050739, 1.135311405967744935, -1.611567521105742751 ) ) ;
#54276 = CARTESIAN_POINT ( 'NONE',  ( 0.5875216112017033199, -0.2866185507822028855, -2.289643093864159429 ) ) ;
#54277 = CARTESIAN_POINT ( 'NONE',  ( 0.4847190467827041105, 1.876267867961832980, 0.5731238010058882226 ) ) ;
#54278 = CARTESIAN_POINT ( 'NONE',  ( 3.731348124473393479, 0.05553323764710679095, -2.061997793915891553 ) ) ;
#54279 = CARTESIAN_POINT ( 'NONE',  ( 6.168596704537822717, 6.299043698156668647, 1.040834085586084257E-14 ) ) ;
#54280 = ADVANCED_FACE ( 'NONE', ( #107403 ), #132586, .T. ) ;
#54281 = CARTESIAN_POINT ( 'NONE',  ( 6.017840079619279692, 8.114175741012878973, -1.599625672291281386 ) ) ;
#54282 = ORIENTED_EDGE ( 'NONE', *, *, #72514, .T. ) ;
#54283 = CARTESIAN_POINT ( 'NONE',  ( 8.554831740098659765, 10.04335378727902395, 1.082531754730558626 ) ) ;
#54284 = CARTESIAN_POINT ( 'NONE',  ( -1.201851678989727383E-14, 3.009375000341419248, -1.575800808251660134 ) ) ;
#54285 = DIRECTION ( 'NONE',  ( 3.122502256758252154E-17, 2.602085213965210950E-17, 1.000000000000000000 ) ) ;
#54286 = CARTESIAN_POINT ( 'NONE',  ( 5.626270559546826533, 5.666329862333828515, 0.7216878364870317197 ) ) ;
#54287 = CARTESIAN_POINT ( 'NONE',  ( 5.934065736658769019, 1.288437188380668452, 1.747434731901863936 ) ) ;
#54289 = CARTESIAN_POINT ( 'NONE',  ( 5.583513413114173041, -0.8223277247318347971, 1.647484189299788682 ) ) ;
#54288 = LINE ( 'NONE', #104106, #73538 ) ;
#54290 = CARTESIAN_POINT ( 'NONE',  ( 5.530578433931943927, 6.204385438716983003, -0.9373897679112530579 ) ) ;
#54291 = DIRECTION ( 'NONE',  ( -0.000000000000000000, -1.000000000000000000, -0.000000000000000000 ) ) ;
#54292 = CARTESIAN_POINT ( 'NONE',  ( 0.3154175708385241750, -1.835744252435017598, 0.3582649291258357960 ) ) ;
#54293 = CARTESIAN_POINT ( 'NONE',  ( -5.301779071304492774, 6.560601962741976045, 1.383466813282836716 ) ) ;
#54294 = CARTESIAN_POINT ( 'NONE',  ( -10.85717823004580040, -6.836271227032190367, 0.3852658704378439936 ) ) ;
#54295 = CARTESIAN_POINT ( 'NONE',  ( 6.083581728852979431, 7.123651168416324175, -1.137916992902558100 ) ) ;
#54296 = CARTESIAN_POINT ( 'NONE',  ( -1.350866880800077663, 3.446184751535887436, 0.3155278943301856320 ) ) ;
#54297 =( BOUNDED_SURFACE ( )  B_SPLINE_SURFACE ( 3, 2, ( 
 ( #123462, #155868, #138560 ),
 ( #41066, #173200, #206733 ),
 ( #26909, #58363, #42135 ),
 ( #108247, #207792, #59420 ),
 ( #125576, #93016, #159059 ),
 ( #10655, #76728, #83929 ),
 ( #66584, #52503, #163082 ),
 ( #130641, #14663, #151092 ) ),
 .UNSPECIFIED., .F., .F., .T. ) 
 B_SPLINE_SURFACE_WITH_KNOTS ( ( 4, 2, 2, 4 ),
 ( 3, 3 ),
 ( 0.000000000000000000, 0.0004912655988793406025, 0.0007368983983190109579, 0.0009825311977586812049 ),
 ( 0.000000000000000000, 1.000000000000000000 ),
 .UNSPECIFIED. ) 
 GEOMETRIC_REPRESENTATION_ITEM ( )  RATIONAL_B_SPLINE_SURFACE ( (
 ( 1.000000000000000000, 0.7100530722026748842, 1.000000000000000000),
 ( 1.000000000000000000, 0.6561915434212005627, 1.000000000000000000),
 ( 1.000000000000000000, 0.5915413786749507130, 1.000000000000000000),
 ( 1.000000000000000000, 0.4908282809844877748, 1.000000000000000000),
 ( 1.000000000000000000, 0.4560392263211181518, 1.000000000000000000),
 ( 1.000000000000000000, 0.3997350557756911282, 1.000000000000000000),
 ( 1.000000000000000000, 0.3799210206805033185, 1.000000000000000000),
 ( 1.000000000000000000, 0.3826834323650902259, 1.000000000000000000) ) ) 
 REPRESENTATION_ITEM ( '' )  SURFACE ( )  );
#54298 = CARTESIAN_POINT ( 'NONE',  ( 2.430210232679584248, 1.715968397599322737, 0.4327865170333042300 ) ) ;
#54299 = CARTESIAN_POINT ( 'NONE',  ( 6.129547061768469085, -0.2442746830248194168, 1.998141925448652989 ) ) ;
#54301 = CARTESIAN_POINT ( 'NONE',  ( 4.253473425383147877, 1.857088099111468216, -0.4692844457289280236 ) ) ;
#54300 = CARTESIAN_POINT ( 'NONE',  ( -9.317477881089553549, 11.89347683273641820, 1.599625672291281386 ) ) ;
#54302 = CARTESIAN_POINT ( 'NONE',  ( -0.1409997244346088141, -0.002808977843308038680, -2.000147647483838220 ) ) ;
#54303 = CARTESIAN_POINT ( 'NONE',  ( 5.846149472147661896, -0.8869723270901458401, 1.758618239599341937 ) ) ;
#54304 = CARTESIAN_POINT ( 'NONE',  ( -0.1049925189658337810, -2.058569791948822392, -0.5088776734372552069 ) ) ;
#54305 = CARTESIAN_POINT ( 'NONE',  ( -4.081167932913447594, 4.720116328942494555, -1.199719254218452047 ) ) ;
#54306 = CARTESIAN_POINT ( 'NONE',  ( 3.045614982896325262, 0.6747646648952825288, -1.744891315567910439 ) ) ;
#54308 = EDGE_LOOP ( 'NONE', ( #174420, #211180, #138405, #189321 ) ) ;
#54307 = CARTESIAN_POINT ( 'NONE',  ( 6.674431755534494748, -1.054235620458108702, 1.365612558063566073 ) ) ;
#54310 = CARTESIAN_POINT ( 'NONE',  ( 4.229780737783593203, 4.037091736943370535, -0.7216878364870188411 ) ) ;
#54309 = CARTESIAN_POINT ( 'NONE',  ( 3.510573375967055654, -0.8941257848905452832, -2.017821460644920073 ) ) ;
#54311 = CARTESIAN_POINT ( 'NONE',  ( -1.201851678989727383E-14, 3.384375000341421469, 1.575800808251672791 ) ) ;
#54312 = CARTESIAN_POINT ( 'NONE',  ( 0.2739786698724961944, -2.023204396000506833, 0.4007670430965051822 ) ) ;
#54313 = CARTESIAN_POINT ( 'NONE',  ( 6.449928391799196525, 8.548002428564306143, -1.599625672291262513 ) ) ;
#54314 = CARTESIAN_POINT ( 'NONE',  ( -8.479735010343349089, 11.98044238112085758, 1.199719254218453823 ) ) ;
#54315 = CARTESIAN_POINT ( 'NONE',  ( -8.123305787156343882, 15.44793803671086252, -8.783211840604518983 ) ) ;
#54316 = CARTESIAN_POINT ( 'NONE',  ( -5.264643720808155791, 5.036505850564608089, 0.000000000000000000 ) ) ;
#54317 = CARTESIAN_POINT ( 'NONE',  ( 0.000000000000000000, 4.400000000000001243, 0.000000000000000000 ) ) ;
#54318 = VERTEX_POINT ( 'NONE', #28219 ) ;
#54319 = CARTESIAN_POINT ( 'NONE',  ( 2.770052221688572125, -2.048192801557855436, 0.3012726569043902569 ) ) ;
#54320 = CARTESIAN_POINT ( 'NONE',  ( 1.499999999999989120, 4.504166666666688634, 0.8660254037844524744 ) ) ;
#54321 = CARTESIAN_POINT ( 'NONE',  ( 4.473300617505036492, 7.306268922809479704, -1.199719254218452047 ) ) ;
#54322 = CARTESIAN_POINT ( 'NONE',  ( -6.329738897986983304, 6.948428204275519882, 0.9008771187248975076 ) ) ;
#54323 = CARTESIAN_POINT ( 'NONE',  ( 1.031905740238812097, -1.969920897724128483, 0.4447463068311637846 ) ) ;
#54324 = B_SPLINE_CURVE_WITH_KNOTS ( 'NONE', 3,
 ( #32442, #109771, #175778, #140090, #11110, #209298, #143307, #60946, #206115, #127102, #193067, #44719, #81191, #35622 ),
 .UNSPECIFIED., .F., .F.,
 ( 4, 2, 2, 2, 2, 2, 4 ),
 ( 0.001731424703407325729, 0.001978656695461683979, 0.002225888687516043747, 0.002720352671624761548, 0.002967584663679120015, 0.003214816655733478482, 0.003709280639842196282 ),
 .UNSPECIFIED. ) ;
#54325 = CARTESIAN_POINT ( 'NONE',  ( 1.499999999999990674, 8.226475397238271370, 3.114076396431860960 ) ) ;
#54326 = EDGE_CURVE ( 'NONE', #74349, #116385, #28806, .T. ) ;
#54327 = CARTESIAN_POINT ( 'NONE',  ( -1.364683531249997417, 4.509375000341424133, 1.214306433183764966E-14 ) ) ;
#54328 = ORIENTED_EDGE ( 'NONE', *, *, #95057, .F. ) ;
#54330 = CARTESIAN_POINT ( 'NONE',  ( 9.408995418203971894, 11.03987807840189816, 1.082531754730549967 ) ) ;
#54329 = CARTESIAN_POINT ( 'NONE',  ( 0.1745949693968328886, 2.059235863126197774, -2.173049245862024303 ) ) ;
#54331 = CARTESIAN_POINT ( 'NONE',  ( 2.000000000000011990, -0.1960773996331451885, 0.5999999999999923173 ) ) ;
#54332 = CARTESIAN_POINT ( 'NONE',  ( 6.087116770962817114, 1.596809997336025022, 1.058066368194489959 ) ) ;
#54333 = FACE_OUTER_BOUND ( 'NONE', #117274, .T. ) ;
#54334 = CARTESIAN_POINT ( 'NONE',  ( 3.861010967126534688, 0.2669419790740577558, -2.175157288012785184 ) ) ;
#54335 = CARTESIAN_POINT ( 'NONE',  ( 0.7499999999999885647, 1.847916667349486231, -1.299038105676652899 ) ) ;
#54336 = CARTESIAN_POINT ( 'NONE',  ( 2.390748813209525814, -1.831196095803063528, -0.5514187292172747501 ) ) ;
#54337 = CARTESIAN_POINT ( 'NONE',  ( -5.148345644887285744, 7.029489223833707001, -1.599625672291256295 ) ) ;
#54338 = EDGE_CURVE ( 'NONE', #130349, #182554, #212375, .T. ) ;
#54339 = CARTESIAN_POINT ( 'NONE',  ( 3.348500752450937590, 5.890039396959305229, 1.082531754730558626 ) ) ;
#54341 = CARTESIAN_POINT ( 'NONE',  ( 0.6148615108944045504, 0.1511614643284354409, 2.010825953887733775 ) ) ;
#54340 = CARTESIAN_POINT ( 'NONE',  ( 10.23127510237375937, 3.700502905159951172, -5.878152162067817876 ) ) ;
#54342 = CARTESIAN_POINT ( 'NONE',  ( 1.364683531250000303, 11.31770833367473550, -0.7879004041258355073 ) ) ;
#54344 = CARTESIAN_POINT ( 'NONE',  ( -6.466312919074983512, 6.508729591867735031, -0.7998128361456362523 ) ) ;
#54343 = CARTESIAN_POINT ( 'NONE',  ( 5.794512526436308875, 1.792401445336734733, -1.260760892635464980 ) ) ;
#54346 = VERTEX_POINT ( 'NONE', #143079 ) ;
#54345 = CARTESIAN_POINT ( 'NONE',  ( 2.924480221818404946, 1.623360404532696810, 0.5830473908832736196 ) ) ;
#54347 = CARTESIAN_POINT ( 'NONE',  ( 0.1394461523057136665, 6.947783040739019533, -2.314776707679897516 ) ) ;
#54348 = CARTESIAN_POINT ( 'NONE',  ( 6.795661308947685164, 8.951357498570873261, -1.599625672291262513 ) ) ;
#54349 = CARTESIAN_POINT ( 'NONE',  ( 5.172599298813543633, 5.993452922492633839, -1.199719254218452047 ) ) ;
#54350 =( LENGTH_UNIT ( ) NAMED_UNIT ( * ) SI_UNIT ( .MILLI., .METRE. ) );
#54351 = CARTESIAN_POINT ( 'NONE',  ( 1.803102349535959714, -1.659081995624330563, 1.046767247423967095 ) ) ;
#54352 = SURFACE_STYLE_USAGE ( .BOTH. , #134564 ) ;
#54353 = CARTESIAN_POINT ( 'NONE',  ( 3.655894977179307226, 7.416961240017848844, -0.7998128361456291469 ) ) ;
#54354 = DIRECTION ( 'NONE',  ( -1.000000000000000000, 0.000000000000000000, 0.000000000000000000 ) ) ;
#54355 = ORIENTED_EDGE ( 'NONE', *, *, #74843, .T. ) ;
#54356 = PLANE ( 'NONE',  #47782 ) ;
#54357 = ORIENTED_EDGE ( 'NONE', *, *, #96785, .T. ) ;
#54358 = CARTESIAN_POINT ( 'NONE',  ( 4.037629478943724592, -1.732251659483119433, 0.5297805909155322013 ) ) ;
#54359 = ORIENTED_EDGE ( 'NONE', *, *, #138422, .T. ) ;
#54360 = CARTESIAN_POINT ( 'NONE',  ( 8.432281472695482449, 11.92507992053172572, 1.199719254218450271 ) ) ;
#54361 = FACE_OUTER_BOUND ( 'NONE', #28249, .T. ) ;
#54362 = CARTESIAN_POINT ( 'NONE',  ( 4.564998375345614257, -1.451947166338814377, 1.082946968254307585 ) ) ;
#54363 = CARTESIAN_POINT ( 'NONE',  ( 0.1523027874134948167, -6.731960136058440902, 9.611344009005483358 ) ) ;
#54364 = LINE ( 'NONE', #55421, #107693 ) ;
#54365 = CARTESIAN_POINT ( 'NONE',  ( 5.064587263324675348, 6.532718652379178259, -1.222898410871699593 ) ) ;
#54367 = FACE_OUTER_BOUND ( 'NONE', #50364, .T. ) ;
#54366 = CARTESIAN_POINT ( 'NONE',  ( 5.600015889513015210, 0.7539677941885476464, -1.701683582386106952 ) ) ;
#54368 = CARTESIAN_POINT ( 'NONE',  ( 2.495587842290597713, -1.894396863028270594, 0.2834604161582406356 ) ) ;
#54369 = CARTESIAN_POINT ( 'NONE',  ( 3.469446951953614189E-15, 5.290451655907108197, 1.214306433183764966E-14 ) ) ;
#54370 = CARTESIAN_POINT ( 'NONE',  ( -4.853455804012230423, 6.685451076146141425, 1.443375672974064550 ) ) ;
#54371 = ADVANCED_FACE ( 'NONE', ( #58586 ), #175551, .T. ) ;
#54372 = AXIS2_PLACEMENT_3D ( 'NONE', #126480, #176226, #27828 ) ;
#54373 = DIRECTION ( 'NONE',  ( 6.314299915563594049E-62, 8.546850786086437571E-32, 1.000000000000000000 ) ) ;
#54374 = CARTESIAN_POINT ( 'NONE',  ( 1.364683531249986537, -1.136458332991912235, 0.7879004041258500513 ) ) ;
#54375 = CARTESIAN_POINT ( 'NONE',  ( 8.270110514656037637, 8.750809809961280550, 0.7216878364870458196 ) ) ;
#54376 = CARTESIAN_POINT ( 'NONE',  ( -4.939248034080176097, 4.656877549381960080, 1.214306433183764966E-14 ) ) ;
#54377 = CARTESIAN_POINT ( 'NONE',  ( 1.429752723428807215, 1.029013270877369379, -1.819774963352964292 ) ) ;
#54378 = CARTESIAN_POINT ( 'NONE',  ( 4.681308178468477799, 8.683552984847038303, 0.000000000000000000 ) ) ;
#54379 = CARTESIAN_POINT ( 'NONE',  ( 0.1295496576057716120, -1.118478952742516519, -1.443350188048427851 ) ) ;
#54380 = CARTESIAN_POINT ( 'NONE',  ( -5.901876940650454095, 5.779944607047298177, -0.7998128361456291469 ) ) ;
#54381 = CARTESIAN_POINT ( 'NONE',  ( 2.748829393344632166, -1.518919317350690967, 1.012417160375630898 ) ) ;
#54382 = CARTESIAN_POINT ( 'NONE',  ( 10.16976112282614508, 11.75387517088144484, 7.514388995082887490 ) ) ;
#54383 = CARTESIAN_POINT ( 'NONE',  ( 2.179812656587180264, 1.874749209517186710, -0.3766967574026017229 ) ) ;
#54384 = CARTESIAN_POINT ( 'NONE',  ( 1.820693447614455618, -1.395048584331352703, 1.390583823087336857 ) ) ;
#54385 = CARTESIAN_POINT ( 'NONE',  ( 4.300292543067584461, 1.499173285595749583, -1.234514081855079048 ) ) ;
#54386 = EDGE_LOOP ( 'NONE', ( #149977, #174401, #94219, #193501, #85663, #8235 ) ) ;
#54387 = CARTESIAN_POINT ( 'NONE',  ( -0.4000000000000166755, 3.949999999999995293, -0.8338124244296005738 ) ) ;
#54388 = CARTESIAN_POINT ( 'NONE',  ( -4.950662367645459305, 5.804802846121667415, -1.199719254218453823 ) ) ;
#54390 = CARTESIAN_POINT ( 'NONE',  ( 3.867525618572264623, -1.764951123045129577, -1.175235903013646332 ) ) ;
#54389 = CARTESIAN_POINT ( 'NONE',  ( 8.167861197590044142, 8.493869250135347215, 0.000000000000000000 ) ) ;
#54391 = CARTESIAN_POINT ( 'NONE',  ( 6.692370362268437844, -7.020359948791616844, 6.743487189264702586 ) ) ;
#54392 = CARTESIAN_POINT ( 'NONE',  ( 8.127223016387999266, 11.56917838817298616, 1.199719254218460707 ) ) ;
#54393 = CARTESIAN_POINT ( 'NONE',  ( 6.067506501917478090, 6.045351875519452634, 0.3962785553160239616 ) ) ;
#54394 = CARTESIAN_POINT ( 'NONE',  ( -11.01135777277262484, 10.09501355085105878, -1.400000000000001021 ) ) ;
#54395 = ORIENTED_EDGE ( 'NONE', *, *, #123006, .T. ) ;
#54396 = CARTESIAN_POINT ( 'NONE',  ( 6.176621499477501054, 9.363752961769195693, -1.199719254218452047 ) ) ;
#54397 = DIRECTION ( 'NONE',  ( -0.6507913734559640506, -0.7592566023653004592, 0.000000000000000000 ) ) ;
#54398 = CARTESIAN_POINT ( 'NONE',  ( 3.773894676421325478, 1.015518775504126614, 1.516979517045339509 ) ) ;
#54399 = CARTESIAN_POINT ( 'NONE',  ( -3.763657168278658816, 3.180244510940675173, 2.446973152615721236 ) ) ;
#54400 = CARTESIAN_POINT ( 'NONE',  ( -10.03267048443264109, 11.76749898900197877, 1.082531754730558626 ) ) ;
#54401 = VECTOR ( 'NONE', #160936, 1000.000000000000000 ) ;
#54402 = CARTESIAN_POINT ( 'NONE',  ( -5.289925464687482481, 7.757115612407050165, 1.311310741419260628 ) ) ;
#54403 = CARTESIAN_POINT ( 'NONE',  ( 6.781144757626058173, -7.161464053357574855, -6.776370306708051849 ) ) ;
#54404 = CARTESIAN_POINT ( 'NONE',  ( 4.416781281874038179, 1.710313510141375115, 0.7581657270378170388 ) ) ;
#54405 = CARTESIAN_POINT ( 'NONE',  ( 7.751511138711133064, 10.06651563329490529, -1.599625672291262513 ) ) ;
#54406 = CARTESIAN_POINT ( 'NONE',  ( 2.244641533702110614, 0.4219287677580378926, 1.879577339372063838 ) ) ;
#54407 = CARTESIAN_POINT ( 'NONE',  ( 6.912952593004608737, -1.518390278170888230, 1.241885805282372912 ) ) ;
#54408 = CARTESIAN_POINT ( 'NONE',  ( -0.6823417656250003738, 8.963541667008065872, 1.181850606188754593 ) ) ;
#54409 = CARTESIAN_POINT ( 'NONE',  ( -7.009729113465285266, 8.136771039586342624, -1.199719254218446718 ) ) ;
#54410 = CARTESIAN_POINT ( 'NONE',  ( 4.039439701867726384, 6.800097854565950506, 1.199719254218462483 ) ) ;
#54411 = CARTESIAN_POINT ( 'NONE',  ( -4.299344108864953995, 7.069632989434141201, -1.082531754730551743 ) ) ;
#54412 = CARTESIAN_POINT ( 'NONE',  ( 1.230240178466317724, 2.114980979692267393, 0.09988113581482771508 ) ) ;
#54413 = CARTESIAN_POINT ( 'NONE',  ( 0.2412978493891524412, 7.030157881589111035, 3.919897618274023277 ) ) ;
#54414 = CARTESIAN_POINT ( 'NONE',  ( 5.260626886859606444, -0.6923115906582855139, -1.951227211109484383 ) ) ;
#54416 = CARTESIAN_POINT ( 'NONE',  ( 4.459584003380381745, 7.054591843250856975, -1.127873490090089748 ) ) ;
#54415 = CARTESIAN_POINT ( 'NONE',  ( 0.3273695209934923689, 0.9472894719858866441, -1.578709817245539604 ) ) ;
#54417 = VERTEX_POINT ( 'NONE', #29288 ) ;
#54418 = CARTESIAN_POINT ( 'NONE',  ( 6.399114681295562157, -1.079681622539971464, -2.029393132690388235 ) ) ;
#54419 = CARTESIAN_POINT ( 'NONE',  ( 5.260200412422194383, 7.159986452624450770, -1.443375672974051449 ) ) ;
#54421 = CARTESIAN_POINT ( 'NONE',  ( 0.4019237886466778820, 9.604914550367428916, 1.500000000000001554 ) ) ;
#54420 = CARTESIAN_POINT ( 'NONE',  ( 3.445180431648313224, 7.033477913649446300, 0.7216878364870257245 ) ) ;
#54422 = CARTESIAN_POINT ( 'NONE',  ( 1.605870876717029549, -2.274517881136278508, 0.2841979012723067077 ) ) ;
#54423 = CARTESIAN_POINT ( 'NONE',  ( 7.900729602272468455, -6.805008568744117525, -7.460470246983064158 ) ) ;
#54424 = PRESENTATION_LAYER_ASSIGNMENT (  '', '', ( #106271 ) ) ;
#54425 = CARTESIAN_POINT ( 'NONE',  ( -5.692444392891315097, 7.734547439830227411, -1.599625672291271394 ) ) ;
#54426 = CARTESIAN_POINT ( 'NONE',  ( 6.070255116781061666, -1.844781929399732290, -0.6067975954986597475 ) ) ;
#54427 = ORIENTED_EDGE ( 'NONE', *, *, #31849, .F. ) ;
#54428 = CARTESIAN_POINT ( 'NONE',  ( 8.120970824461352322, 9.537182719035495637, -1.082531754730543083 ) ) ;
#54429 = ORIENTED_EDGE ( 'NONE', *, *, #170447, .F. ) ;
#54430 = CARTESIAN_POINT ( 'NONE',  ( -0.1579526903544171412, -1.242116785587377592, -1.585096312452577205 ) ) ;
#54431 = CARTESIAN_POINT ( 'NONE',  ( -8.947491310014823895, 12.52615806407091803, 1.199719254218462483 ) ) ;
#54433 = CARTESIAN_POINT ( 'NONE',  ( 0.4659925305415726360, -6.893137084989842123, 10.91005274787796608 ) ) ;
#54432 = CARTESIAN_POINT ( 'NONE',  ( -7.690499447449645309, 9.995335326823163058, 1.599625672291295375 ) ) ;
#54434 = CARTESIAN_POINT ( 'NONE',  ( 3.285556943750000514, -0.4010416661887095113, 1.896917185911906500 ) ) ;
#54436 = CARTESIAN_POINT ( 'NONE',  ( 1.111743784240331712, -0.7909239834335696218, -1.583357840528883287 ) ) ;
#54435 = CARTESIAN_POINT ( 'NONE',  ( 3.011755509560889443, -1.030818127458534184, -1.818759449385324078 ) ) ;
#54437 = CARTESIAN_POINT ( 'NONE',  ( 0.01979919457416898926, -6.863887352872461989, -9.496663240426190811 ) ) ;
#54439 = CARTESIAN_POINT ( 'NONE',  ( 3.855682016854941274, 2.275109001451373292, -0.2794487578934058969 ) ) ;
#54438 = CARTESIAN_POINT ( 'NONE',  ( 5.435893244436359240, 5.306573304789342416, -0.7998128361456481317 ) ) ;
#54440 = CARTESIAN_POINT ( 'NONE',  ( 2.976183818757103250, -0.1284355763333933920, -1.735648432857107126 ) ) ;
#54441 = CARTESIAN_POINT ( 'NONE',  ( 4.054051625686104998, 4.688480637177271149, -1.199719254218446718 ) ) ;
#54442 = CARTESIAN_POINT ( 'NONE',  ( -4.908225742414364490, 4.881379242517357220, -0.5727826874471857455 ) ) ;
#54443 = CARTESIAN_POINT ( 'NONE',  ( 3.778401656274816389, -1.708383637232064878, 0.2947856008331130040 ) ) ;
#54444 = CARTESIAN_POINT ( 'NONE',  ( 3.736941271748619009, -2.091586689864731063, -0.5821943698010292323 ) ) ;
#54445 = CARTESIAN_POINT ( 'NONE',  ( 3.649115900372475796, 7.409052317076538330, 1.040834085586084257E-14 ) ) ;
#54446 = CARTESIAN_POINT ( 'NONE',  ( 4.803922858132807505, -1.082837210388952309, -1.700963621564715700 ) ) ;
#54447 = CARTESIAN_POINT ( 'NONE',  ( 2.218750000000001332, -0.7852924748298697466, 1.895863743164134974 ) ) ;
#54448 = CARTESIAN_POINT ( 'NONE',  ( -0.7500000000000215383, 2.222916667349486453, 1.299038105676671107 ) ) ;
#54449 = CARTESIAN_POINT ( 'NONE',  ( 1.518447027862340093, 1.295632655171574665, -1.425748867336932513 ) ) ;
#54450 = CARTESIAN_POINT ( 'NONE',  ( -1.500000000000001110, 9.052083334016126415, 0.8660254037844419273 ) ) ;
#54451 = CARTESIAN_POINT ( 'NONE',  ( 5.010122972300034228, -0.7987708819462059351, 2.073016528135694703 ) ) ;
#54452 = ORIENTED_EDGE ( 'NONE', *, *, #118396, .T. ) ;
#54453 = CARTESIAN_POINT ( 'NONE',  ( -0.2106854629475244378, -0.004120941679102134263, -1.996958217618934661 ) ) ;
#54454 = CARTESIAN_POINT ( 'NONE',  ( -1.500000000000001332, 1.150000000000019007, 0.000000000000000000 ) ) ;
#54455 = CARTESIAN_POINT ( 'NONE',  ( 7.344766530301147789, 9.591980256816594164, 1.599625672291281386 ) ) ;
#54456 = CARTESIAN_POINT ( 'NONE',  ( 5.327991180046175224, 5.318337252916401248, -0.7216878364870207285 ) ) ;
#54457 = CARTESIAN_POINT ( 'NONE',  ( 0.9268046190927975436, -1.003647134691580289, -1.981720526202688015 ) ) ;
#54459 = ADVANCED_FACE ( 'NONE', ( #144152 ), #53065, .T. ) ;
#54458 = CARTESIAN_POINT ( 'NONE',  ( 5.406682003534418079, 0.5678430586343993225, 1.877905798087247335 ) ) ;
#54460 = CARTESIAN_POINT ( 'NONE',  ( 9.761507412159302177, 10.49077285704843199, -0.7216878364870257245 ) ) ;
#54461 = LINE ( 'NONE', #206027, #14505 ) ;
#54462 = CARTESIAN_POINT ( 'NONE',  ( 6.854744688279930998, -1.755419801747569286, 1.426855864884185809 ) ) ;
#54463 = CARTESIAN_POINT ( 'NONE',  ( -3.838366886444665393, 7.492195444245147939, 0.000000000000000000 ) ) ;
#54464 = CARTESIAN_POINT ( 'NONE',  ( 3.332538901969614553, -1.230775513943611399, 1.655089866650825581 ) ) ;
#54465 = CARTESIAN_POINT ( 'NONE',  ( -6.403528624356093601, 6.365204904703887223, 1.040834085586084257E-14 ) ) ;
#54466 = CARTESIAN_POINT ( 'NONE',  ( 1.499999999999990896, 4.306250000682819490, 1.214306433183764966E-14 ) ) ;
#54467 = CARTESIAN_POINT ( 'NONE',  ( 1.364683531249992088, 5.696875000341418804, 1.214306433183764966E-14 ) ) ;
#54468 = CARTESIAN_POINT ( 'NONE',  ( 5.290257391050456448, -1.856285702826396156, -0.2301478561287788605 ) ) ;
#54469 = CARTESIAN_POINT ( 'NONE',  ( 3.586273015720359503, -0.4996269028240771237, 1.660617844614233674 ) ) ;
#54470 = CARTESIAN_POINT ( 'NONE',  ( 3.016877700344788416, -1.676514204431644783, 0.4670218299706177523 ) ) ;
#54471 = CARTESIAN_POINT ( 'NONE',  ( 1.206998765908244176, 2.024556473040285187, 1.075228724532976132 ) ) ;
#54472 = CARTESIAN_POINT ( 'NONE',  ( -0.6823417656249969321, 4.530208333674755394, -1.181850606188749264 ) ) ;
#54473 = CARTESIAN_POINT ( 'NONE',  ( 4.054300615058183510, -1.547851416709244310, 1.405648825684354897 ) ) ;
#54474 = CARTESIAN_POINT ( 'NONE',  ( 6.615187027077672255, -1.883050660437551205, 0.4742715046822160718 ) ) ;
#54475 = CARTESIAN_POINT ( 'NONE',  ( 0.1588445005388132991, -6.630981418884858591, 9.484513308955760280 ) ) ;
#54476 = CARTESIAN_POINT ( 'NONE',  ( 1.881482635453747720, -0.5404922439061732309, -1.942541187959702764 ) ) ;
#54477 = DIRECTION ( 'NONE',  ( 0.000000000000000000, 0.000000000000000000, 1.000000000000000000 ) ) ;
#54478 = CARTESIAN_POINT ( 'NONE',  ( 8.335182146949760451, 13.17516691652663319, -8.541839703048623278 ) ) ;
#54479 = CARTESIAN_POINT ( 'NONE',  ( -6.353967546298838087, 10.56471257065732416, 0.000000000000000000 ) ) ;
#54480 =( BOUNDED_SURFACE ( )  B_SPLINE_SURFACE ( 3, 3, ( 
 ( #115703, #149213, #15986, #62621, #48532, #99406, #165459, #66855, #128782, #17054, #53582 ),
 ( #119716, #37329, #212059, #63699, #103403, #194761, #195837, #47477, #57850, #90366, #125079 ),
 ( #136981, #71938, #154291, #141287, #6937, #54648, #189978, #153218, #120797, #108809, #25345 ),
 ( #56785, #24260, #156433, #186774, #203008, #173768, #170526, #38400, #55714, #122953, #104480 ),
 ( #174832, #191035, #75177, #73018, #205143, #188913, #138048, #157505, #121867, #187838, #74109 ),
 ( #22109, #89303, #40552, #124011, #8018, #88221, #5866, #9101, #42702, #172683, #204062 ),
 ( #139115, #107744, #207296, #39465, #106656, #91444, #58920, #140202, #206224, #87146, #41630 ) ),
 .UNSPECIFIED., .T., .F., .T. ) 
 B_SPLINE_SURFACE_WITH_KNOTS ( ( 4, 3, 4 ),
 ( 4, 1, 1, 1, 1, 1, 1, 1, 4 ),
 ( 0.000000000000000000, 0.5000000000000000000, 1.000000000000000000 ),
 ( 0.000000000000000000, 0.2254179815473072723, 0.3971144120416517653, 0.5241699701252212629, 0.6156743509408303394, 0.6807935377546089351, 0.7289379548928518471, 0.7696256121123346006, 1.000000000000000000 ),
 .UNSPECIFIED. ) 
 GEOMETRIC_REPRESENTATION_ITEM ( )  RATIONAL_B_SPLINE_SURFACE ( (
 ( 1.000000000000000000, 1.000000000000000000, 1.000000000000000222, 0.9999999999999997780, 0.9999999999999997780, 1.000000000000000222, 0.9999999999999997780, 1.000000000000000222, 0.9999999999999992228, 1.000000000000000000, 1.000000000000000000),
 ( 0.3333333333333333703, 0.3333333333333334259, 0.3333333333333334259, 0.3333333333333332593, 0.3333333333333333703, 0.3333333333333334259, 0.3333333333333333703, 0.3333333333333334814, 0.3333333333333332038, 0.3333333333333333703, 0.3333333333333333703),
 ( 0.3333333333333333703, 0.3333333333333334259, 0.3333333333333334259, 0.3333333333333332593, 0.3333333333333333703, 0.3333333333333334259, 0.3333333333333333703, 0.3333333333333334814, 0.3333333333333332038, 0.3333333333333333703, 0.3333333333333333703),
 ( 1.000000000000000000, 1.000000000000000000, 1.000000000000000222, 0.9999999999999997780, 0.9999999999999997780, 1.000000000000000222, 0.9999999999999997780, 1.000000000000000222, 0.9999999999999992228, 1.000000000000000000, 1.000000000000000000),
 ( 0.3333333333333333703, 0.3333333333333334259, 0.3333333333333334259, 0.3333333333333332593, 0.3333333333333333703, 0.3333333333333334259, 0.3333333333333333703, 0.3333333333333334814, 0.3333333333333332038, 0.3333333333333333703, 0.3333333333333333703),
 ( 0.3333333333333333703, 0.3333333333333334259, 0.3333333333333334259, 0.3333333333333332593, 0.3333333333333333703, 0.3333333333333334259, 0.3333333333333333703, 0.3333333333333334814, 0.3333333333333332038, 0.3333333333333333703, 0.3333333333333333703),
 ( 1.000000000000000000, 1.000000000000000000, 1.000000000000000222, 0.9999999999999997780, 0.9999999999999997780, 1.000000000000000222, 0.9999999999999997780, 1.000000000000000222, 0.9999999999999992228, 1.000000000000000000, 1.000000000000000000) ) ) 
 REPRESENTATION_ITEM ( '' )  SURFACE ( )  );
#54481 = CARTESIAN_POINT ( 'NONE',  ( 5.575427483717746213, 7.527751369135936343, 1.599625672291267398 ) ) ;
#54482 = CARTESIAN_POINT ( 'NONE',  ( 2.262495435604610527, 2.120074037919957632, 0.04929290001921824566 ) ) ;
#54483 = CARTESIAN_POINT ( 'NONE',  ( 1.063464886906835938, -4.211945764156021177, -0.1580247838118454540 ) ) ;
#54484 = CARTESIAN_POINT ( 'NONE',  ( 6.059193749186201572, -1.568369423792463024, -0.9343120793870243190 ) ) ;
#54485 = ORIENTED_EDGE ( 'NONE', *, *, #180841, .T. ) ;
#54486 = CARTESIAN_POINT ( 'NONE',  ( -5.824109505522200081, 8.952488968821326054, -1.199719254218452047 ) ) ;
#54487 = CARTESIAN_POINT ( 'NONE',  ( 2.273217432877753463, 5.716990842764664293, 0.1274701612217898072 ) ) ;
#54488 = CARTESIAN_POINT ( 'NONE',  ( 5.831415467209187575, 9.817418788470464008, 0.000000000000000000 ) ) ;
#54489 = CARTESIAN_POINT ( 'NONE',  ( 1.642778471875001811, -0.4302083328553765740, 2.845375778867859751 ) ) ;
#54490 = CARTESIAN_POINT ( 'NONE',  ( -7.854251061018346469, 8.057714414143200443, -0.7998128361456291469 ) ) ;
#54491 = CARTESIAN_POINT ( 'NONE',  ( 2.144791408438687430, 1.960151896008819117, 0.4867283015469162644 ) ) ;
#54492 = CARTESIAN_POINT ( 'NONE',  ( 6.721690211428396289, -2.142211831252617493, 0.5295551626897446740 ) ) ;
#54493 = CARTESIAN_POINT ( 'NONE',  ( 8.204655514564224816, 12.72384853363364066, 1.040834085586084257E-14 ) ) ;
#54494 = CARTESIAN_POINT ( 'NONE',  ( 4.153051346612735450, 1.574026050290713963, -0.9924080308383613769 ) ) ;
#54495 = CARTESIAN_POINT ( 'NONE',  ( 8.757677159423465696, 12.30470822171437284, 1.199719254218450271 ) ) ;
#54496 = CARTESIAN_POINT ( 'NONE',  ( -0.4288785890453234995, 3.049942316455299451, -0.4196807566834767078 ) ) ;
#54497 = CARTESIAN_POINT ( 'NONE',  ( -3.242371291962510504, 6.934516940598226320, 1.040834085586084257E-14 ) ) ;
#54498 = CARTESIAN_POINT ( 'NONE',  ( -6.347188469492005325, 10.55680364771601809, -0.7998128361456291469 ) ) ;
#54499 = CARTESIAN_POINT ( 'NONE',  ( 4.775911370473768791, 1.053640644303525331, 1.490772598166143048 ) ) ;
#54501 = CARTESIAN_POINT ( 'NONE',  ( -4.044288467547167976, 7.756266588949179308, -0.5710662792986564984 ) ) ;
#54500 = CARTESIAN_POINT ( 'NONE',  ( -6.563028877466991595, 9.814561569423593923, 1.199719254218452935 ) ) ;
#54502 = CARTESIAN_POINT ( 'NONE',  ( 1.364683531249986537, -1.136458332991912235, 0.7879004041258500513 ) ) ;
#54503 = CARTESIAN_POINT ( 'NONE',  ( 0.8250588069352093878, -1.261192405561472274, 1.190076739608906697 ) ) ;
#54504 = CARTESIAN_POINT ( 'NONE',  ( 0.1107398820658512667, -1.707777377628461046, 0.3340355821882161069 ) ) ;
#54505 = CARTESIAN_POINT ( 'NONE',  ( 5.971339433669736962, 0.1760496889521658836, -2.301030538967073991 ) ) ;
#54506 = CARTESIAN_POINT ( 'NONE',  ( -10.45142907045522129, 5.144535043903895932, -5.216774619840575333 ) ) ;
#54507 = CARTESIAN_POINT ( 'NONE',  ( 1.968112693492467979, 1.056634718301739717, 1.769108711375965148 ) ) ;
#54508 = CARTESIAN_POINT ( 'NONE',  ( 5.819474248763732760, 7.812472595022922128, -1.599625672291262513 ) ) ;
#54509 = CARTESIAN_POINT ( 'NONE',  ( 0.2806244687772480040, -1.977743564115455932, 0.3905345501400147024 ) ) ;
#54510 = CARTESIAN_POINT ( 'NONE',  ( -1.431838407952683134, -3.232243495192085092, 2.960863168642819510 ) ) ;
#54511 = CARTESIAN_POINT ( 'NONE',  ( -5.936491157937300756, 8.019268665717216749, 1.599625672291263179 ) ) ;
#54512 = CARTESIAN_POINT ( 'NONE',  ( 5.858239598252557911, 0.7595784280203803362, 1.709674162104061645 ) ) ;
#54513 = AXIS2_PLACEMENT_3D ( 'NONE', #202513, #20572, #102909 ) ;
#54515 = CARTESIAN_POINT ( 'NONE',  ( -4.659162064951642535, 5.464719159645540003, 1.199719254218452935 ) ) ;
#54514 = CARTESIAN_POINT ( 'NONE',  ( 3.656429697474584017, 1.903630103707624865, 0.1825790434749063051 ) ) ;
#54516 = CARTESIAN_POINT ( 'NONE',  ( 5.531908139154323223, -1.397534428995873546, -1.707979418440738195 ) ) ;
#54517 = CARTESIAN_POINT ( 'NONE',  ( 1.224999999999961009, 1.416666667349490538, 0.7072540797572558491 ) ) ;
#54518 = CARTESIAN_POINT ( 'NONE',  ( -7.453913518772577795, -5.212532583863431768, -8.072398248062480519 ) ) ;
#54519 = CARTESIAN_POINT ( 'NONE',  ( 5.383996397958233260, 5.453953017138946535, -0.7216878364870458196 ) ) ;
#54520 = CARTESIAN_POINT ( 'NONE',  ( -6.441532379824190357, 6.687744995982559892, 0.7216878364870257245 ) ) ;
#54521 = CARTESIAN_POINT ( 'NONE',  ( 6.006510593949522026, -2.110231943656666331, -0.2080817731764383061 ) ) ;
#54522 = ORIENTED_EDGE ( 'NONE', *, *, #152126, .T. ) ;
#54523 = CARTESIAN_POINT ( 'NONE',  ( 3.364621831457567769, 1.035725732715401470, 2.062151656813861145 ) ) ;
#54524 = CARTESIAN_POINT ( 'NONE',  ( 4.123457186961496213, 0.2424046295769199388, -1.946780420294342617 ) ) ;
#54525 = CARTESIAN_POINT ( 'NONE',  ( -6.283277845290492714, 6.295188672452495915, -0.7998128361456361413 ) ) ;
#54526 = CARTESIAN_POINT ( 'NONE',  ( 0.6023038706522118035, 1.956103482322549825, 0.1501044349687257751 ) ) ;
#54527 = PLANE ( 'NONE',  #130360 ) ;
#54528 = CARTESIAN_POINT ( 'NONE',  ( 4.913904330310220558, 4.697586238308844919, 0.000000000000000000 ) ) ;
#54529 = EDGE_LOOP ( 'NONE', ( #178808, #207018, #113995, #38932 ) ) ;
#54530 = CARTESIAN_POINT ( 'NONE',  ( 6.016814611094169152, 0.2024578496369993375, 2.006372135924570088 ) ) ;
#54531 = CARTESIAN_POINT ( 'NONE',  ( -8.296699936558862731, 11.76690146170562201, 1.199719254218453823 ) ) ;
#54532 = CARTESIAN_POINT ( 'NONE',  ( -4.080641063585716211, 5.783833847506671511, -1.249999999999999334 ) ) ;
#54533 = CARTESIAN_POINT ( 'NONE',  ( 3.256845431185355633, -0.6256494993409821292, -2.079000826131827129 ) ) ;
#54534 = CARTESIAN_POINT ( 'NONE',  ( 1.002369745560643510, -0.9483682245385971488, 1.896766750748935415 ) ) ;
#54535 = CARTESIAN_POINT ( 'NONE',  ( -1.500000000000013101, 1.952083334016152527, 0.8660254037844403729 ) ) ;
#54536 = CARTESIAN_POINT ( 'NONE',  ( 9.673906298550626559, 11.24497775551929557, 1.199719254218452047 ) ) ;
#54537 = CARTESIAN_POINT ( 'NONE',  ( 11.86687215968023601, 13.60942212305790022, -1.056395335932036383 ) ) ;
#54538 = CARTESIAN_POINT ( 'NONE',  ( 4.966250736084032447, 8.070317005903060448, 1.090833899539983554 ) ) ;
#54539 = CARTESIAN_POINT ( 'NONE',  ( 0.4915707408097417797, 1.525207926881542830, 1.386002245639144981 ) ) ;
#54541 = CARTESIAN_POINT ( 'NONE',  ( 6.827182134110238110, 6.038038905730811479, 2.505852844092556264 ) ) ;
#54540 = CARTESIAN_POINT ( 'NONE',  ( -8.533967624797991647, 12.04371376465130439, -1.199719254218446718 ) ) ;
#54542 = CARTESIAN_POINT ( 'NONE',  ( 1.364683531249988757, 1.884375000341421913, 0.000000000000000000 ) ) ;
#54543 = SURFACE_STYLE_FILL_AREA ( #153112 ) ;
#54544 = ORIENTED_EDGE ( 'NONE', *, *, #74564, .F. ) ;
#54545 = CARTESIAN_POINT ( 'NONE',  ( 3.967365900211225593, -1.591558630706500832, -1.059764132600553355 ) ) ;
#54546 = CIRCLE ( 'NONE', #19895, 0.08000000000000014044 ) ;
#54547 = CARTESIAN_POINT ( 'NONE',  ( 5.717594842608604289, -1.725906139129701478, 0.3911541089357990497 ) ) ;
#54548 = CARTESIAN_POINT ( 'NONE',  ( 6.170896192875352959, 7.228408975556602556, 1.199719254218453823 ) ) ;
#54549 = CARTESIAN_POINT ( 'NONE',  ( -3.253066792275140173, 5.882662793374543675, 1.199719254218462483 ) ) ;
#54550 = CARTESIAN_POINT ( 'NONE',  ( 0.7381712907078247232, 1.078401568856072412, -1.455492281976622504 ) ) ;
#54552 = CARTESIAN_POINT ( 'NONE',  ( 1.200237320533149799, 1.284028115529710190, -1.421911532115504029 ) ) ;
#54551 = CARTESIAN_POINT ( 'NONE',  ( -0.3247179164460003986, 6.996819380137557332, -3.870394258462603432 ) ) ;
#54553 = CARTESIAN_POINT ( 'NONE',  ( 1.486871883557450369, 1.994755712061954123, 0.5540851298423480342 ) ) ;
#54554 = CARTESIAN_POINT ( 'NONE',  ( 0.6823417656249882723, 0.4885416670080827695, -1.181850606188749264 ) ) ;
#54555 = AXIS2_PLACEMENT_3D ( 'NONE', #180088, #196338, #14361 ) ;
#54556 = CARTESIAN_POINT ( 'NONE',  ( 0.8308620510419548744, 0.1428995296039961560, 1.966335887032538032 ) ) ;
#54557 = CARTESIAN_POINT ( 'NONE',  ( 3.299243935302543118, 1.439784963707075649, 1.122460502641378755 ) ) ;
#54559 = CARTESIAN_POINT ( 'NONE',  ( 5.417061852544872380, 7.532864896096530316, 1.248242807326222392 ) ) ;
#54558 = CARTESIAN_POINT ( 'NONE',  ( 0.3996046210705077595, 1.915144275937111340, -1.287252092841030260 ) ) ;
#54560 = CARTESIAN_POINT ( 'NONE',  ( -1.402160292154681736E-14, 0.07187500034142156602, 1.575800808251672791 ) ) ;
#54561 = CARTESIAN_POINT ( 'NONE',  ( 4.404768648179163471, 0.5469982912414109721, 1.988780625590305329 ) ) ;
#54562 = CARTESIAN_POINT ( 'NONE',  ( -6.144869935491728441, 8.192100896205577243, -1.599625672291263179 ) ) ;
#54563 = CARTESIAN_POINT ( 'NONE',  ( 7.401861798056875053, 10.72292363345333399, -1.199719254218441611 ) ) ;
#54564 = CARTESIAN_POINT ( 'NONE',  ( 3.842846474469570062, 6.570739089268092137, -1.199719254218452047 ) ) ;
#54565 = CARTESIAN_POINT ( 'NONE',  ( 6.667912619822566000, 6.673652899414787676, 1.040834085586084257E-14 ) ) ;
#54567 = CARTESIAN_POINT ( 'NONE',  ( -1.201851678989727383E-14, 3.212500000000018119, 1.732050807568877637 ) ) ;
#54566 = CARTESIAN_POINT ( 'NONE',  ( 5.491282870796595716, 1.858858430755592428, -0.9897807336930256605 ) ) ;
#54568 = CARTESIAN_POINT ( 'NONE',  ( 5.986797818411375260, 1.994257276370488219, 0.5558945855626205024 ) ) ;
#54569 = CARTESIAN_POINT ( 'NONE',  ( -1.201851678989727383E-14, 1.884375000341422135, 1.575800808251672791 ) ) ;
#54570 = CARTESIAN_POINT ( 'NONE',  ( 3.989662644735529451, 1.562606173494068829, 1.493797087085822373 ) ) ;
#54571 = CARTESIAN_POINT ( 'NONE',  ( 3.949871522956601932, -1.394395303408175080, -1.461305941245706119 ) ) ;
#54572 =( NAMED_UNIT ( * ) SI_UNIT ( $, .STERADIAN. ) SOLID_ANGLE_UNIT ( ) );
#54575 = CARTESIAN_POINT ( 'NONE',  ( 5.002595493762530765, 8.780185809457538681, 1.040834085586084257E-14 ) ) ;
#54574 = CARTESIAN_POINT ( 'NONE',  ( 3.285556943749998737, -3.055208332855376518, -1.896917185911906500 ) ) ;
#54573 = CARTESIAN_POINT ( 'NONE',  ( 3.982994815507484354, 7.308283119008860851, -0.9368446653362592080 ) ) ;
#54576 = CARTESIAN_POINT ( 'NONE',  ( -5.794130544993808307, 7.853181283949808744, 1.599625672291263179 ) ) ;
#54577 = CARTESIAN_POINT ( 'NONE',  ( 2.342982756445275427, -1.756855002775299379, -0.9896843009072553432 ) ) ;
#54578 = CARTESIAN_POINT ( 'NONE',  ( -8.259941899223614215, 10.65968485389279508, -1.599625672291263179 ) ) ;
#54580 = DIRECTION ( 'NONE',  ( -0.000000000000000000, 1.000000000000000000, -0.000000000000000000 ) ) ;
#54579 = CARTESIAN_POINT ( 'NONE',  ( -5.278201874421821316, 5.052323696447222900, 0.7998128361456341429 ) ) ;
#54581 = CARTESIAN_POINT ( 'NONE',  ( -11.94105721237523099, 12.69999999999999929, -1.187919463087248939 ) ) ;
#54582 = CARTESIAN_POINT ( 'NONE',  ( 6.222915752822945734, 1.412394824171304908, -1.289504995239741714 ) ) ;
#54583 = DIRECTION ( 'NONE',  ( 1.000000000000000000, 0.000000000000000000, 0.000000000000000000 ) ) ;
#54584 = ADVANCED_FACE ( 'NONE', ( #123682 ), #187121, .T. ) ;
#54586 = CARTESIAN_POINT ( 'NONE',  ( 4.148064665909578785, 0.9530284220014314522, 1.777003606838889915 ) ) ;
#54585 = CARTESIAN_POINT ( 'NONE',  ( -8.365017589507372620, 9.821903944922480534, 1.082531754730558626 ) ) ;
#54587 = CARTESIAN_POINT ( 'NONE',  ( -1.500000000000011324, 5.629166666666693963, -0.8660254037844313801 ) ) ;
#54588 = CARTESIAN_POINT ( 'NONE',  ( -1.364683531250014514, 8.588541667008067648, -0.7879004041258335089 ) ) ;
#54589 = CARTESIAN_POINT ( 'NONE',  ( 0.01170749999939314084, -0.7329999334961794233, -1.560365621481168086 ) ) ;
#54590 = CARTESIAN_POINT ( 'NONE',  ( 6.561219994370630637, 6.619454513046008515, 0.000000000000000000 ) ) ;
#54592 = CARTESIAN_POINT ( 'NONE',  ( 6.535912570239620578, 9.782925877658371405, 1.199719254218452047 ) ) ;
#54591 = CARTESIAN_POINT ( 'NONE',  ( 8.920901888111989919, 11.43080484092926241, 1.443375672974076540 ) ) ;
#54593 = CARTESIAN_POINT ( 'NONE',  ( -4.324687812634898876, 6.068555086205916105, 1.443375672974064550 ) ) ;
#54594 = CARTESIAN_POINT ( 'NONE',  ( 5.870339087135666212, -1.187030499695044039, 1.445606174157453738 ) ) ;
#54595 = CARTESIAN_POINT ( 'NONE',  ( 6.539320575229251808, 0.004279804010676873348, 1.996977849922920267 ) ) ;
#54596 = CARTESIAN_POINT ( 'NONE',  ( 2.430607852509637290, -1.277051959022021066, 1.629327859714514659 ) ) ;
#54597 = CARTESIAN_POINT ( 'NONE',  ( -7.905812970100109638, 8.396072351304486148, 0.7216878364870317197 ) ) ;
#54598 = ORIENTED_EDGE ( 'NONE', *, *, #96366, .T. ) ;
#54599 = CARTESIAN_POINT ( 'NONE',  ( 8.880227426826630577, 12.34372051706435869, 1.082531754730546636 ) ) ;
#54600 = CARTESIAN_POINT ( 'NONE',  ( 0.7027501817156032171, 1.864177386631180822, 0.7691025790682110008 ) ) ;
#54601 = CARTESIAN_POINT ( 'NONE',  ( 3.241808126998965811, 6.796210224891872542, 0.7216878364870257245 ) ) ;
#54602 = CARTESIAN_POINT ( 'NONE',  ( 0.000000000000000000, 5.499999999999998224, 0.000000000000000000 ) ) ;
#54603 = CARTESIAN_POINT ( 'NONE',  ( 7.076992996209058973, 11.20031622897851165, 1.040834085586084257E-14 ) ) ;
#54604 = CARTESIAN_POINT ( 'NONE',  ( 6.076025397218672630, 10.24044673006381245, -0.7998128361456291469 ) ) ;
#54606 = CARTESIAN_POINT ( 'NONE',  ( 5.765228759176680207, 1.768025090248021902, -0.7378185885129113775 ) ) ;
#54605 = CARTESIAN_POINT ( 'NONE',  ( -5.747767057189642870, 8.793146435774861658, -1.199719254218440723 ) ) ;
#54607 = CARTESIAN_POINT ( 'NONE',  ( 1.860351378971565550, 8.967085675740335660, 0.7750000000000004663 ) ) ;
#54608 = CARTESIAN_POINT ( 'NONE',  ( -4.113984376790197572, 3.977835813768412887, -0.5576404437566493399 ) ) ;
#54609 = EDGE_CURVE ( 'NONE', #34845, #20233, #14860, .T. ) ;
#54610 = CARTESIAN_POINT ( 'NONE',  ( -11.00009153390426597, -6.553298220693309695, 0.005414006223999826353 ) ) ;
#54612 = ORIENTED_EDGE ( 'NONE', *, *, #17110, .T. ) ;
#54611 = CARTESIAN_POINT ( 'NONE',  ( 3.877268743828270470, 5.546566172598190292, 1.443375672974062551 ) ) ;
#54613 = CARTESIAN_POINT ( 'NONE',  ( -3.918470089549458635, 4.530302178351167441, -1.199719254218452047 ) ) ;
#54614 = CARTESIAN_POINT ( 'NONE',  ( 2.518638242371186386, 1.412657066830936392, -1.636333507658905173 ) ) ;
#54615 = CARTESIAN_POINT ( 'NONE',  ( -6.563555762791521531, 9.711213252348503744, 1.082531754730549967 ) ) ;
#54616 = CARTESIAN_POINT ( 'NONE',  ( 5.370438244788902971, 9.279612028980123384, -0.7216878364870458196 ) ) ;
#54617 = CARTESIAN_POINT ( 'NONE',  ( 0.7035762090183244055, 1.867434778015097940, -1.004864118554361863 ) ) ;
#54618 = CARTESIAN_POINT ( 'NONE',  ( 6.159193757800505153, -1.567253032978152660, -0.9359774744091067245 ) ) ;
#54619 = CARTESIAN_POINT ( 'NONE',  ( 2.600799297785437947, 1.585616864491301348, -1.171192495528531330 ) ) ;
#54620 = CARTESIAN_POINT ( 'NONE',  ( 4.816621285000030284, -0.6497861859515661198, -1.798733151862880186 ) ) ;
#54621 = ORIENTED_EDGE ( 'NONE', *, *, #37827, .F. ) ;
#54622 = CARTESIAN_POINT ( 'NONE',  ( 9.477100695693454924, -6.554910290221281244, -0.2834499523633078333 ) ) ;
#54623 = CARTESIAN_POINT ( 'NONE',  ( 4.826587240018016089, -1.288162778474700287, 1.489951593160773635 ) ) ;
#54624 = CARTESIAN_POINT ( 'NONE',  ( 0.2166051034824221788, -0.09641855276349860226, 1.939669501089319015 ) ) ;
#54625 = ORIENTED_EDGE ( 'NONE', *, *, #135323, .F. ) ;
#54626 = CARTESIAN_POINT ( 'NONE',  ( -4.447956913735107598, 7.346977611736363656, 1.199719254218452935 ) ) ;
#54627 = CARTESIAN_POINT ( 'NONE',  ( -7.431277594066152403, 8.802816960232885179, -1.082531754730549967 ) ) ;
#54629 = CARTESIAN_POINT ( 'NONE',  ( 4.855228407025239612, 8.678533884922511987, 0.000000000000000000 ) ) ;
#54628 = CARTESIAN_POINT ( 'NONE',  ( 6.771407655021410399, 9.987393799911945536, -1.199719254218441611 ) ) ;
#54631 = VERTEX_POINT ( 'NONE', #202712 ) ;
#54630 = CARTESIAN_POINT ( 'NONE',  ( 5.197880135092803222, 1.287283252470315720, 1.414272151883423589 ) ) ;
#54632 = CARTESIAN_POINT ( 'NONE',  ( 1.343116161061377767, 0.4315099961175078991, 2.164003993775004187 ) ) ;
#54633 = CARTESIAN_POINT ( 'NONE',  ( 0.3999999999999858113, 3.372708439410149417, -0.5000000000000373035 ) ) ;
#54634 = CARTESIAN_POINT ( 'NONE',  ( 6.533844907621704223, -1.952130696095262463, 0.4912315161729706725 ) ) ;
#54635 = CARTESIAN_POINT ( 'NONE',  ( -0.7500000000000179856, 8.791666666666669627, 1.299038105676658228 ) ) ;
#54636 = DIRECTION ( 'NONE',  ( 0.000000000000000000, 1.000000000000000000, 0.000000000000000000 ) ) ;
#54637 = CARTESIAN_POINT ( 'NONE',  ( -2.680963302752292332, 0.4788041664876945269, 8.638326563840814180E-32 ) ) ;
#54638 = CARTESIAN_POINT ( 'NONE',  ( 3.402844027952243167, 0.5003511028610057032, 2.008882729757965890 ) ) ;
#54639 = CARTESIAN_POINT ( 'NONE',  ( -5.713871673155502151, 8.753601821068331290, 1.199719254218452047 ) ) ;
#54640 = AXIS2_PLACEMENT_3D ( 'NONE', #108542, #9900, #124812 ) ;
#54641 = CARTESIAN_POINT ( 'NONE',  ( -4.606260857482554982, 8.381206713624141713, 0.1075878075270080697 ) ) ;
#54643 = CARTESIAN_POINT ( 'NONE',  ( 0.1808504484964272296, -2.097240537080494516, -0.5235256853268267507 ) ) ;
#54642 = CARTESIAN_POINT ( 'NONE',  ( -3.066115294984855133, 6.728884944124295053, 0.7998128361456341429 ) ) ;
#54644 = DIRECTION ( 'NONE',  ( 0.000000000000000000, 0.000000000000000000, 1.000000000000000000 ) ) ;
#54645 = SURFACE_STYLE_FILL_AREA ( #34127 ) ;
#54646 = CARTESIAN_POINT ( 'NONE',  ( 0.01083140255524605265, -7.162053774861989908, 9.500385102287577155 ) ) ;
#54647 = CARTESIAN_POINT ( 'NONE',  ( -1.364683531250014514, 12.65104166700806232, -0.7879004041258335089 ) ) ;
#54649 = CARTESIAN_POINT ( 'NONE',  ( -4.606738333593328072, 8.596554832492683929, 0.7998128361456281477 ) ) ;
#54648 = CARTESIAN_POINT ( 'NONE',  ( 6.925078400183590333, 2.970608243536181359, 2.408862486266015512 ) ) ;
#54650 = CARTESIAN_POINT ( 'NONE',  ( 6.451818256879360725, -1.589883334587833152, -0.6930036952102114345 ) ) ;
#54651 = CARTESIAN_POINT ( 'NONE',  ( -5.101945877444165944, 4.846691699973280976, 0.000000000000000000 ) ) ;
#54653 = VECTOR ( 'NONE', #153208, 1000.000000000000114 ) ;
#54652 = AXIS2_PLACEMENT_3D ( 'NONE', #43, #19508, #66107 ) ;
#54654 = CARTESIAN_POINT ( 'NONE',  ( 3.256751887857904926, -0.5965066610371800859, -1.982489643792232137 ) ) ;
#54655 = CARTESIAN_POINT ( 'NONE',  ( 4.077823013788191453, -0.8085361882982607939, 1.956954002425244088 ) ) ;
#54656 = CARTESIAN_POINT ( 'NONE',  ( 6.775324078527185989, 8.927630729746953264, -1.599625672291262513 ) ) ;
#54657 = CARTESIAN_POINT ( 'NONE',  ( -1.201851678989727383E-14, 4.196875000341417028, -1.575800808251660134 ) ) ;
#54658 = CARTESIAN_POINT ( 'NONE',  ( 2.430458318764291192, -1.215629356985904685, 1.549377053225237111 ) ) ;
#54659 = CARTESIAN_POINT ( 'NONE',  ( 1.195406425308798148, 1.765864799226088744, -0.7346160280939582066 ) ) ;
#54660 = CARTESIAN_POINT ( 'NONE',  ( 4.558679923290005043, -2.046282147472633373, -1.033175111039591698 ) ) ;
#54661 = CARTESIAN_POINT ( 'NONE',  ( 2.279681363911123970, 1.122676072794186908, 1.439608767588994365 ) ) ;
#54662 = CARTESIAN_POINT ( 'NONE',  ( 4.420840606507738357, 7.315341919971147355, 1.199719254218451159 ) ) ;
#54663 = CARTESIAN_POINT ( 'NONE',  ( 5.788968402910805722, 7.776882441527838807, 1.443375672974062551 ) ) ;
#54664 = CARTESIAN_POINT ( 'NONE',  ( -7.588813295347149435, 9.876701482703580837, -1.599625672291263179 ) ) ;
#54665 = CARTESIAN_POINT ( 'NONE',  ( 2.953388010686915255, -1.773442693046624496, 0.9528950618205129786 ) ) ;
#54666 = CARTESIAN_POINT ( 'NONE',  ( 3.696105151714265347, 0.8860871710942277435, -1.750347149911928968 ) ) ;
#54667 = CARTESIAN_POINT ( 'NONE',  ( -5.859094939400033120, 9.987361195942037639, -0.7998128361456231517 ) ) ;
#54668 = CARTESIAN_POINT ( 'NONE',  ( -6.112028321662274166, 6.025121218227761588, 0.7998128361456341429 ) ) ;
#54669 = CARTESIAN_POINT ( 'NONE',  ( 0.07556134207192893859, 1.990881419511018935, -2.657973000608151448 ) ) ;
#54671 = CARTESIAN_POINT ( 'NONE',  ( 4.961649905909814251, 1.750258134581949232, -0.2615843724830448913 ) ) ;
#54670 = CARTESIAN_POINT ( 'NONE',  ( 6.087849878328269071, -2.080457216024658607, -0.2059406971956292964 ) ) ;
#54672 = DIRECTION ( 'NONE',  ( 0.000000000000000000, 0.000000000000000000, -1.000000000000000000 ) ) ;
#54673 = CARTESIAN_POINT ( 'NONE',  ( 0.7619990552875830492, 1.083242598816274382, 1.904929396514772444 ) ) ;
#54674 = CARTESIAN_POINT ( 'NONE',  ( 6.421804192028983671, 0.9955936683583621605, -1.427223192643598537 ) ) ;
#54675 = CARTESIAN_POINT ( 'NONE',  ( 6.265839547809997079, 10.46189657242035587, 0.7998128361456462443 ) ) ;
#54676 = DIRECTION ( 'NONE',  ( 0.000000000000000000, 0.000000000000000000, -1.000000000000000000 ) ) ;
#54677 = CARTESIAN_POINT ( 'NONE',  ( 0.2987795159231512176, -2.099866535080958663, 0.9347484894880775386 ) ) ;
#54678 = CARTESIAN_POINT ( 'NONE',  ( 0.5740950506661415265, -1.212703583203307511, 1.825263377225619266 ) ) ;
#54679 = CARTESIAN_POINT ( 'NONE',  ( 1.858336453454629611, 2.200810804183956026, -0.1644699235988852648 ) ) ;
#54680 = AXIS2_PLACEMENT_3D ( 'NONE', #92884, #207664, #158929 ) ;
#54681 = CARTESIAN_POINT ( 'NONE',  ( 6.689883316565048865, -1.412897867115006978, -1.648663827357793155 ) ) ;
#54682 = DIRECTION ( 'NONE',  ( 0.000000000000000000, 1.000000000000000000, 0.000000000000000000 ) ) ;
#54683 = CARTESIAN_POINT ( 'NONE',  ( 1.200578840252497947, 1.417437365323451104, -1.573097661806458936 ) ) ;
#54684 = CARTESIAN_POINT ( 'NONE',  ( 3.875000000000003553, 2.052068128417946724, -2.337016516192933888E-13 ) ) ;
#54685 = CARTESIAN_POINT ( 'NONE',  ( 6.727182134110222478, 4.688348259194305534, 2.751590707055273199 ) ) ;
#54686 = CARTESIAN_POINT ( 'NONE',  ( 5.842784322950494769, 0.3761301977728331858, 1.889152344147272178 ) ) ;
#54687 = VERTEX_POINT ( 'NONE', #172381 ) ;
#54689 = CARTESIAN_POINT ( 'NONE',  ( -0.7500000000000215383, 5.191666666666685082, 1.299038105676671107 ) ) ;
#54688 = CARTESIAN_POINT ( 'NONE',  ( 1.769451523944377769, 2.192225184321832554, -0.6701302238534474487 ) ) ;
#54690 = CARTESIAN_POINT ( 'NONE',  ( 5.007038802148489509, 4.735966778795008381, 0.7998128361456341429 ) ) ;
#54691 = CARTESIAN_POINT ( 'NONE',  ( 5.361359679200154105, 8.342337828120466980, 1.199719254218462483 ) ) ;
#54692 = VECTOR ( 'NONE', #209657, 1000.000000000000000 ) ;
#54693 = CARTESIAN_POINT ( 'NONE',  ( 4.020361658589631126, -2.215315801286695585, 0.1640026922601171833 ) ) ;
#54694 = CARTESIAN_POINT ( 'NONE',  ( -7.646435448427427062, 10.90429654226522693, 1.082531754730549967 ) ) ;
#54696 = EDGE_CURVE ( 'NONE', #100951, #29554, #23625, .T. ) ;
#54695 = CARTESIAN_POINT ( 'NONE',  ( -1.154700538379266339, -4.295408888568413630, 2.602085213965210642E-15 ) ) ;
#54697 = CARTESIAN_POINT ( 'NONE',  ( 4.989037340148863464, 8.764367963574922982, -0.7216878364870257245 ) ) ;
#54698 = CARTESIAN_POINT ( 'NONE',  ( -7.443063143778079649, 10.66702885350765584, 1.082531754730549967 ) ) ;
#54699 = CARTESIAN_POINT ( 'NONE',  ( 4.556949027968946631, 8.330541276023501140, -0.7216878364870357165 ) ) ;
#54700 = VERTEX_POINT ( 'NONE', #203776 ) ;
#54701 = CARTESIAN_POINT ( 'NONE',  ( 1.389296306420295224, -0.7283806465635984662, -1.880434191983325398 ) ) ;
#54703 = CARTESIAN_POINT ( 'NONE',  ( 6.514137810226229064, 2.057410315668557921, -0.1480156956644717581 ) ) ;
#54702 = CARTESIAN_POINT ( 'NONE',  ( 8.209625708274705502, 9.536650400197368427, 1.199719254218462483 ) ) ;
#54704 = DIRECTION ( 'NONE',  ( 0.000000000000000000, 0.000000000000000000, -1.000000000000000000 ) ) ;
#54705 = CARTESIAN_POINT ( 'NONE',  ( 4.868786560638878491, 8.694351730805124134, 0.7216878364870317197 ) ) ;
#54706 = CARTESIAN_POINT ( 'NONE',  ( 6.005355179794888976, -1.726165566969834586, 0.2220549178573327509 ) ) ;
#54707 = CARTESIAN_POINT ( 'NONE',  ( -1.201851678989727383E-14, 2.071875000341422801, 1.575800808251672791 ) ) ;
#54708 = CARTESIAN_POINT ( 'NONE',  ( 1.545802484126792109, 1.767419949743149532, 0.09338694931935660748 ) ) ;
#54709 = CARTESIAN_POINT ( 'NONE',  ( 0.5279704824466545654, -1.728000714500482982, 1.038995864524896673 ) ) ;
#54710 = CARTESIAN_POINT ( 'NONE',  ( 0.09881949811249221560, -0.4921898920670075839, 1.774194203830472993 ) ) ;
#54711 = CARTESIAN_POINT ( 'NONE',  ( 4.353268756680241047, 0.5026898720560546430, -2.236438357558430123 ) ) ;
#54712 = CARTESIAN_POINT ( 'NONE',  ( 3.837712106225504183, 1.832433245109680531, 0.1787696065849928018 ) ) ;
#54713 = EDGE_CURVE ( 'NONE', #162878, #147411, #114263, .T. ) ;
#54714 = CARTESIAN_POINT ( 'NONE',  ( 7.910292558569346433, 11.31609285405122556, -1.199719254218446718 ) ) ;
#54715 = DIRECTION ( 'NONE',  ( 0.000000000000000000, 0.000000000000000000, -1.000000000000000000 ) ) ;
#54716 = CARTESIAN_POINT ( 'NONE',  ( 4.278209411971904075, -1.050932907216840295, 1.492538610026641122 ) ) ;
#54717 = CARTESIAN_POINT ( 'NONE',  ( 4.781875055470904634, 1.674888562130649960, -1.122497055794105192 ) ) ;
#54718 = CARTESIAN_POINT ( 'NONE',  ( -7.804689982961090955, 12.25722208009664094, 0.7998128361456481317 ) ) ;
#54720 = CARTESIAN_POINT ( 'NONE',  ( -7.445362632559989535, 8.715286488521982733, 1.199719254218452047 ) ) ;
#54719 = CARTESIAN_POINT ( 'NONE',  ( 3.520660345214459586, 1.437014610000959314, -1.747548891452437081 ) ) ;
#54721 = CARTESIAN_POINT ( 'NONE',  ( 0.06524607375175436874, -1.882416456675739092, -0.9446200181052357703 ) ) ;
#54722 = CARTESIAN_POINT ( 'NONE',  ( -6.563028877466991595, 9.814561569423593923, 1.199719254218452935 ) ) ;
#54723 = CARTESIAN_POINT ( 'NONE',  ( 3.455589482447298355, 1.630370400113918095, 1.275915752658786095 ) ) ;
#54724 = CARTESIAN_POINT ( 'NONE',  ( 9.378489572351044856, 11.96465713920816043, -1.599625672291262513 ) ) ;
#54725 = CARTESIAN_POINT ( 'NONE',  ( -9.514659125335341649E-15, 1.359375000341400463, -1.570758158831806250 ) ) ;
#54726 = CARTESIAN_POINT ( 'NONE',  ( 5.637388408723053246, -0.05200288984260474645, 2.120005899716829401 ) ) ;
#54728 = CARTESIAN_POINT ( 'NONE',  ( 2.068856375562718508, -1.761265384887151342, -0.7809992120406393790 ) ) ;
#54727 = CARTESIAN_POINT ( 'NONE',  ( -9.154780037725563702, 11.70366268214508487, 1.599625672291281386 ) ) ;
#54729 = CARTESIAN_POINT ( 'NONE',  ( -10.51582573219070227, 11.11290858478269783, 3.554376768052134317 ) ) ;
#54730 = CARTESIAN_POINT ( 'NONE',  ( 0.5374760852590576565, 1.839023226330655625, -0.7055796775109841601 ) ) ;
#54731 = CARTESIAN_POINT ( 'NONE',  ( 4.217995187182922656, 6.014356699837137832, 1.443375672974058777 ) ) ;
#54732 = CARTESIAN_POINT ( 'NONE',  ( 5.874728247277303694, 5.987702652136856152, -0.2291304890473921385 ) ) ;
#54733 = PLANE ( 'NONE',  #59725 ) ;
#54734 = VECTOR ( 'NONE', #208773, 1000.000000000000000 ) ;
#54735 = CARTESIAN_POINT ( 'NONE',  ( -5.199715606040888005, 6.025088614257851027, -1.199719254218446718 ) ) ;
#54736 = CARTESIAN_POINT ( 'NONE',  ( 0.5630927014088433769, 0.6521865704650819939, 2.123503569120980927 ) ) ;
#54737 = CARTESIAN_POINT ( 'NONE',  ( 3.663195928028176063, -1.856456087625086182, -0.9943140874985546551 ) ) ;
#54738 = CARTESIAN_POINT ( 'NONE',  ( -2.993318053567081360, 6.714231172462041819, 0.000000000000000000 ) ) ;
#54739 = CARTESIAN_POINT ( 'NONE',  ( 7.182068686937156166, 9.402166106225269715, 1.599625672291281386 ) ) ;
#54740 = CARTESIAN_POINT ( 'NONE',  ( 0.2384088454224670139, -1.803645845812065440, -0.4582378156636581767 ) ) ;
#54741 = CARTESIAN_POINT ( 'NONE',  ( 7.284808609244363353, 7.393364887073558656, 0.7998128361456341429 ) ) ;
#54742 = CARTESIAN_POINT ( 'NONE',  ( 5.834086172582112262, 5.700855377634248100, 1.040834085586084257E-14 ) ) ;
#54743 = CARTESIAN_POINT ( 'NONE',  ( -5.804299160426224624, 9.785783097223662352, -0.7216878364870338292 ) ) ;
#54744 = CARTESIAN_POINT ( 'NONE',  ( -7.971831135155409420, 11.28392484344787405, 1.082531754730549967 ) ) ;
#54745 = CARTESIAN_POINT ( 'NONE',  ( 1.195735321641926197, 1.957225868588155837, -0.8166992996602240318 ) ) ;
#54746 = CARTESIAN_POINT ( 'NONE',  ( -7.611976899429754084, 7.845337568948314022, 0.7998128361456341429 ) ) ;
#54748 = CARTESIAN_POINT ( 'NONE',  ( 3.754310534785664899, -1.959519245081872585, -0.09869234604030494018 ) ) ;
#54747 = CARTESIAN_POINT ( 'NONE',  ( -1.225000000000042277, 0.5208333333333544646, 0.7072540797572777205 ) ) ;
#54749 = CARTESIAN_POINT ( 'NONE',  ( 1.868271315571629509, 1.111147431007172726, 1.854118885846419262 ) ) ;
#54750 = CARTESIAN_POINT ( 'NONE',  ( 1.188719773494644860, 1.394467456127197025, 1.202481090285527632 ) ) ;
#54752 = CARTESIAN_POINT ( 'NONE',  ( -5.125485847170801357, 6.519186964134095597, -1.210412105186658094 ) ) ;
#54751 = CARTESIAN_POINT ( 'NONE',  ( -4.146814880933400005, 5.931313009212638931, 1.599625672291270506 ) ) ;
#54753 = EDGE_CURVE ( 'NONE', #95626, #186548, #201783, .T. ) ;
#54754 = CARTESIAN_POINT ( 'NONE',  ( 3.327794560494615084, 1.698141246764593770, 0.3800555388253792355 ) ) ;
#54755 = CARTESIAN_POINT ( 'NONE',  ( 0.000000000000000000, 9.200000000000020606, 0.4000000000000166755 ) ) ;
#54756 = CARTESIAN_POINT ( 'NONE',  ( 6.507550544879468823, 6.694489845221929691, -0.7216878364870257245 ) ) ;
#54757 = CARTESIAN_POINT ( 'NONE',  ( -10.02504487015220569, 5.769816241140256707, -5.888073156868665059 ) ) ;
#54758 = CARTESIAN_POINT ( 'NONE',  ( 0.5323697292517782786, 1.110078392871534314, -1.854780036684190669 ) ) ;
#54759 = CARTESIAN_POINT ( 'NONE',  ( 3.831407535526813124, -1.356092489331266027, 1.492026659919619247 ) ) ;
#54760 = CARTESIAN_POINT ( 'NONE',  ( -9.612367721964606204, 12.23751498042398289, -1.443375672974058777 ) ) ;
#54761 = CARTESIAN_POINT ( 'NONE',  ( -2.959422669532919326, 6.674686557755516780, 0.7998128361456352531 ) ) ;
#54762 = CARTESIAN_POINT ( 'NONE',  ( 3.397303563958519401, 1.553371746707431500, 1.213851982216722636 ) ) ;
#54763 = EDGE_CURVE ( 'NONE', #211245, #213399, #57410, .T. ) ;
#54764 = CARTESIAN_POINT ( 'NONE',  ( 1.499999999999989120, 6.280000000000042881, 2.580000000000000515 ) ) ;
#54765 = CARTESIAN_POINT ( 'NONE',  ( 2.436971693805603856, -1.440716923005976646, -1.302479457752574232 ) ) ;
#54768 = ORIENTED_EDGE ( 'NONE', *, *, #202175, .F. ) ;
#54767 = CARTESIAN_POINT ( 'NONE',  ( -4.285785955695645910, 7.053815144069948140, 1.082531754730549967 ) ) ;
#54766 = CARTESIAN_POINT ( 'NONE',  ( 6.381121926128928479, -1.751337275642101510, -0.7685668267764720341 ) ) ;
#54770 = EDGE_CURVE ( 'NONE', #41218, #143294, #160389, .T. ) ;
#54769 = CARTESIAN_POINT ( 'NONE',  ( -3.472296738431328134, 7.065113604896248845, 0.000000000000000000 ) ) ;
#54771 = CARTESIAN_POINT ( 'NONE',  ( -0.2106854629475244378, 6.948332279000682732, -2.592197477433130448 ) ) ;
#54772 = CARTESIAN_POINT ( 'NONE',  ( 3.874598038455354665, 7.742391154831717692, -0.7998128361456362523 ) ) ;
#54773 = CARTESIAN_POINT ( 'NONE',  ( -5.173318132066234476, 8.193232366456022930, -1.199719254218453823 ) ) ;
#54774 = CARTESIAN_POINT ( 'NONE',  ( -5.769876891067536206, 8.889217585290882795, 1.199719254218454489 ) ) ;
#54775 = CARTESIAN_POINT ( 'NONE',  ( -6.645678883216806554, 6.734777780655774038, 0.1184763017797350326 ) ) ;
#54776 = CARTESIAN_POINT ( 'NONE',  ( 6.475599238194152285, 2.210894796874377288, -0.6610463658997690617 ) ) ;
#54777 = CARTESIAN_POINT ( 'NONE',  ( -10.40218499402273800, 5.060399005975109610, 5.893486624065884527 ) ) ;
#54778 = CARTESIAN_POINT ( 'NONE',  ( 3.748837004188230182, -0.3782986639458625899, -1.924763881548184230 ) ) ;
#54779 = CARTESIAN_POINT ( 'NONE',  ( 7.446452682403650769, 9.710614100936176385, -1.599625672291262513 ) ) ;
#54780 = CARTESIAN_POINT ( 'NONE',  ( 2.004529941291322448, -1.955172360644286789, 0.4926429297785542283 ) ) ;
#54781 = ORIENTED_EDGE ( 'NONE', *, *, #160757, .T. ) ;
#54782 = CARTESIAN_POINT ( 'NONE',  ( 2.343091305525629497, -1.844686447908544746, -1.039184121536258942 ) ) ;
#54783 = CARTESIAN_POINT ( 'NONE',  ( 0.7499999999999902300, 2.014583334016148530, 1.299038105676669330 ) ) ;
#54785 = CARTESIAN_POINT ( 'NONE',  ( -6.067437437315529536, 7.037430750744921859, 1.199719254218450271 ) ) ;
#54784 = CARTESIAN_POINT ( 'NONE',  ( -4.295235737431041478, 3.905529869957963029, -0.7998128361456221525 ) ) ;
#54786 = CARTESIAN_POINT ( 'NONE',  ( 3.099365256270599112, -1.839010575856118823, 0.09107247011905240941 ) ) ;
#54787 = ORIENTED_EDGE ( 'NONE', *, *, #1928, .F. ) ;
#54788 =( REPRESENTATION_RELATIONSHIP ('NONE','NONE', #84563, #141543 ) REPRESENTATION_RELATIONSHIP_WITH_TRANSFORMATION ( #162914 )SHAPE_REPRESENTATION_RELATIONSHIP( ) );
#54789 = CARTESIAN_POINT ( 'NONE',  ( -9.996439331977562404, 10.55693406359564790, 0.7998128361456462443 ) ) ;
#54790 = CARTESIAN_POINT ( 'NONE',  ( 0.4499999999999764744, 3.999999999999955147, 0.4999999999999813483 ) ) ;
#54791 = CARTESIAN_POINT ( 'NONE',  ( 3.972980863544761654, -1.569110274459505350, 1.426624754300914510 ) ) ;
#54792 = CARTESIAN_POINT ( 'NONE',  ( 0.2164228883963260908, -0.09351453081237262599, 1.838880455306932227 ) ) ;
#54793 = DIRECTION ( 'NONE',  ( 0.000000000000000000, -1.000000000000000000, 0.000000000000000000 ) ) ;
#54794 = CARTESIAN_POINT ( 'NONE',  ( 5.926885707468349196, 10.06645042535509660, 1.040834085586084257E-14 ) ) ;
#54795 = CARTESIAN_POINT ( 'NONE',  ( 4.622373940358720290, 1.271062617260295458, -1.621988140548079826 ) ) ;
#54797 = CARTESIAN_POINT ( 'NONE',  ( 2.612652284633736777, -0.1782932461553646819, 1.832575692395449485 ) ) ;
#54796 = CARTESIAN_POINT ( 'NONE',  ( -6.028571859570855729, 10.18508426947466816, 0.000000000000000000 ) ) ;
#54798 = CARTESIAN_POINT ( 'NONE',  ( 7.801827329660018684, 11.18955008699033726, 1.199719254218460707 ) ) ;
#54799 = CARTESIAN_POINT ( 'NONE',  ( -6.471393748265538370, 5.229711127717889596, -2.419999999999995044 ) ) ;
#54800 = DIRECTION ( 'NONE',  ( 8.638326563840814399E-31, 0.000000000000000000, 1.000000000000000000 ) ) ;
#54801 = CARTESIAN_POINT ( 'NONE',  ( -1.580000000000021165, 8.674529973577531194, 2.500000000000011102 ) ) ;
#54802 = DIRECTION ( 'NONE',  ( 0.000000000000000000, 0.000000000000000000, -1.000000000000000000 ) ) ;
#54803 = CIRCLE ( 'NONE', #186204, 0.08000000000000040412 ) ;
#54804 = CARTESIAN_POINT ( 'NONE',  ( 1.770444396619451632, 1.136427050704125419, 1.891651738277564831 ) ) ;
#54805 = CARTESIAN_POINT ( 'NONE',  ( 4.077597889297270406, 2.132052650593726728, -0.7572755323067262845 ) ) ;
#54806 = CARTESIAN_POINT ( 'NONE',  ( -6.697364695470783502, 10.75741654478384035, 0.7216878364870458196 ) ) ;
#54807 = CARTESIAN_POINT ( 'NONE',  ( 3.884856352912366972, -1.692463592844297704, -0.6465920371584426007 ) ) ;
#54808 = CARTESIAN_POINT ( 'NONE',  ( 4.100734417499996454, 1.753908128398029787, 0.7709784123341425488 ) ) ;
#54809 = CARTESIAN_POINT ( 'NONE',  ( 5.459458695672200435, 1.690470114046587646, 1.195012289465044564 ) ) ;
#54810 = CARTESIAN_POINT ( 'NONE',  ( -1.364683531250010295, 4.092708333674751842, 0.7879004041258379498 ) ) ;
#54811 = CARTESIAN_POINT ( 'NONE',  ( 3.502765367584356859, 1.555092314170872347, -1.211676150289840992 ) ) ;
#54812 = CARTESIAN_POINT ( 'NONE',  ( 1.623919080003157545, -1.068017489352061533, -1.603033266432315918 ) ) ;
#54813 = CARTESIAN_POINT ( 'NONE',  ( 3.678450976403758066, -1.802590750232490491, -0.4997190347926713794 ) ) ;
#54814 = CARTESIAN_POINT ( 'NONE',  ( 3.334905300413065543, 2.251431139208215804, 0.5058342958955232005 ) ) ;
#54815 = CARTESIAN_POINT ( 'NONE',  ( 5.055058894927250357, 1.547480351173950552, -1.033501273311630886 ) ) ;
#54816 = CARTESIAN_POINT ( 'NONE',  ( 0.07933543236773606122, -9.910877263631659773, 9.499668725233687994 ) ) ;
#54817 = AXIS2_PLACEMENT_3D ( 'NONE', #68333, #146445, #81412 ) ;
#54818 = PLANE ( 'NONE',  #93068 ) ;
#54819 = CARTESIAN_POINT ( 'NONE',  ( 1.612088513325710126, -2.090005036333367539, 0.2590644908504329824 ) ) ;
#54820 = CARTESIAN_POINT ( 'NONE',  ( 2.697709378994964879, 6.091152008895348580, 0.7216878364870338292 ) ) ;
#54822 = CARTESIAN_POINT ( 'NONE',  ( -10.31505594189871111, 10.92865344183699428, -0.7998128361456291469 ) ) ;
#54821 = CARTESIAN_POINT ( 'NONE',  ( -1.201851678989727383E-14, 5.759375000341417028, -1.575800808251660801 ) ) ;
#54823 = CARTESIAN_POINT ( 'NONE',  ( -1.905110947044342140, 8.996536036952683446, -0.7749999999999996891 ) ) ;
#54824 = CARTESIAN_POINT ( 'NONE',  ( 3.111701630267147412, 1.674174984267240429, 1.301503359413098249 ) ) ;
#54825 = CARTESIAN_POINT ( 'NONE',  ( 6.343417644170677328, 6.506394916557118435, -2.500000000000000444 ) ) ;
#54826 = CARTESIAN_POINT ( 'NONE',  ( 0.5100284451979911760, -0.7230318888242005526, 1.886137889315203875 ) ) ;
#54827 = CARTESIAN_POINT ( 'NONE',  ( -1.402160292154681736E-14, 0.4468750003414233563, -1.575800808251665908 ) ) ;
#54828 = CARTESIAN_POINT ( 'NONE',  ( -4.134873662487946966, 3.926366815765101936, 1.214306433183764966E-14 ) ) ;
#54829 = CARTESIAN_POINT ( 'NONE',  ( 4.985647801523278133, 6.839675073242382553, -1.599625672291256295 ) ) ;
#54830 = ORIENTED_EDGE ( 'NONE', *, *, #64219, .F. ) ;
#54831 = CARTESIAN_POINT ( 'NONE',  ( 2.284651837757902371, -2.119410549416993916, -0.4241055355862289877 ) ) ;
#54832 = CARTESIAN_POINT ( 'NONE',  ( 6.609999999999998543, 2.109033691136730226, 2.032371550245914094 ) ) ;
#54835 = CARTESIAN_POINT ( 'NONE',  ( 7.013428937081407355, 5.939655416065874327, -2.436399677959149468 ) ) ;
#54834 = CARTESIAN_POINT ( 'NONE',  ( 5.346851039111029991, 6.199209027673978412, 7.500000000000000000 ) ) ;
#54833 = CARTESIAN_POINT ( 'NONE',  ( 3.888156192069020634, 7.758209000714329839, 1.040834085586084257E-14 ) ) ;
#54836 = CARTESIAN_POINT ( 'NONE',  ( 0.000000000000000000, -9.999999999999994671, 10.99999999999999112 ) ) ;
#54837 = CARTESIAN_POINT ( 'NONE',  ( 5.946499988598237252, -1.422611626450220434, 1.429444749906971790 ) ) ;
#54838 = CARTESIAN_POINT ( 'NONE',  ( -7.700668062882072284, 10.00719871149432549, -1.443375672974059665 ) ) ;
#54839 = CARTESIAN_POINT ( 'NONE',  ( 6.392138156072928901, -0.5583118246898631787, -2.014728688386701272 ) ) ;
#54840 = CARTESIAN_POINT ( 'NONE',  ( -0.4637852190931971985, -7.024005807102851051, -10.66594404249593531 ) ) ;
#54842 = CARTESIAN_POINT ( 'NONE',  ( 1.364683531249996529, 12.46354166700806232, 0.7879004041258403923 ) ) ;
#54841 = CARTESIAN_POINT ( 'NONE',  ( 0.4095021115802527922, 1.970281763946807541, 1.112102026807944677 ) ) ;
#54843 = CARTESIAN_POINT ( 'NONE',  ( -8.890396042259075315, 11.39521468743417998, -1.599625672291263179 ) ) ;
#54844 = EDGE_CURVE ( 'NONE', #91101, #116385, #108504, .T. ) ;
#54845 = CARTESIAN_POINT ( 'NONE',  ( -4.216222583725562245, 7.862750747747711877, 0.7216878364870317197 ) ) ;
#54846 = CARTESIAN_POINT ( 'NONE',  ( -1.364683531250012516, 1.592708333674756727, 0.7879004041258379498 ) ) ;
#54847 = CARTESIAN_POINT ( 'NONE',  ( -1.162044386198238935E-15, 2.625000000682799151, 1.224999999999985656 ) ) ;
#54848 = CARTESIAN_POINT ( 'NONE',  ( -1.500000000000001110, 10.02083333333333393, 0.8660254037844419273 ) ) ;
#54849 = CARTESIAN_POINT ( 'NONE',  ( 3.070621489812708660, -1.593986286245190565, -0.6595977741803840111 ) ) ;
#54850 = CARTESIAN_POINT ( 'NONE',  ( 3.691562964670865199, 7.528850235416478576, -0.7998128361456362523 ) ) ;
#54851 = CARTESIAN_POINT ( 'NONE',  ( 2.354462415756667593, -1.371198970962312691, 1.118854571612490245 ) ) ;
#54852 = CARTESIAN_POINT ( 'NONE',  ( 5.262800499965147871, -1.601618428465928057, 1.518362080380669221 ) ) ;
#54853 = VERTEX_POINT ( 'NONE', #75936 ) ;
#54854 = CARTESIAN_POINT ( 'NONE',  ( 4.465106368662499214, -1.619631974074808412, 1.206539259511850259 ) ) ;
#54855 = CARTESIAN_POINT ( 'NONE',  ( -5.562588163356775972, 9.711712967216715953, 0.7998128361456291469 ) ) ;
#54857 = CARTESIAN_POINT ( 'NONE',  ( 4.306267660493944049, 1.238306454277863677, -1.591331080693689559 ) ) ;
#54856 = CARTESIAN_POINT ( 'NONE',  ( 4.600305182625006317, -0.9987976242244798186, 1.870504488178956759 ) ) ;
#54859 = ORIENTED_EDGE ( 'NONE', *, *, #138938, .F. ) ;
#54858 = CARTESIAN_POINT ( 'NONE',  ( 4.693523411346745000, 1.687728755266065139, -0.6588045490927648684 ) ) ;
#54860 = CARTESIAN_POINT ( 'NONE',  ( 4.875038752565570732, 7.845239757038595663, -1.199719254218452047 ) ) ;
#54861 = VERTEX_POINT ( 'NONE', #110640 ) ;
#54862 = CARTESIAN_POINT ( 'NONE',  ( 1.393192293617943944, 1.414286473764417185, 1.224485199485196629 ) ) ;
#54863 = FACE_OUTER_BOUND ( 'NONE', #95761, .T. ) ;
#54864 = CARTESIAN_POINT ( 'NONE',  ( 5.637325938770506362, -0.03788160184842354061, 1.811251791611239170 ) ) ;
#54865 = CARTESIAN_POINT ( 'NONE',  ( 1.499999999999993117, 9.604166666666669627, 0.8660254037844408170 ) ) ;
#54866 = CARTESIAN_POINT ( 'NONE',  ( -10.81809272050965376, 3.158133435639066899, -6.646723133134004868 ) ) ;
#54867 = CARTESIAN_POINT ( 'NONE',  ( 0.4373225248172890045, -5.223431457505089526, 10.96785329849812385 ) ) ;
#54868 = CARTESIAN_POINT ( 'NONE',  ( -1.364683531249997417, 2.821875000341422801, 1.214306433183764966E-14 ) ) ;
#54869 = CARTESIAN_POINT ( 'NONE',  ( -0.07025823700084612988, -1.875094440630159065, 0.3749275819610526916 ) ) ;
#54870 = CARTESIAN_POINT ( 'NONE',  ( 6.536439455564150514, 9.679577560583279450, 1.082531754730549078 ) ) ;
#54871 = CARTESIAN_POINT ( 'NONE',  ( 2.207404936347991065, -1.573848641742966459, -1.171066219227391070 ) ) ;
#54872 = ADVANCED_FACE ( 'NONE', ( #209108 ), #62516, .F. ) ;
#54873 = CARTESIAN_POINT ( 'NONE',  ( -3.201133666602369310, 6.748756687762456963, -0.7216878364870458196 ) ) ;
#54874 = CARTESIAN_POINT ( 'NONE',  ( -5.855142236255304944, 7.924361590421551860, -1.599625672291271394 ) ) ;
#54875 = CARTESIAN_POINT ( 'NONE',  ( 4.201511661969238531, 1.892856375164463367, -0.9562558712687405649 ) ) ;
#54876 = CARTESIAN_POINT ( 'NONE',  ( -0.02968770228140016343, 0.003472272166151618711, -1.826291111852257343 ) ) ;
#54877 = CARTESIAN_POINT ( 'NONE',  ( 5.079350664050449105, 1.840474797211266944, -0.7068060451330003824 ) ) ;
#54878 = CARTESIAN_POINT ( 'NONE',  ( 1.364683531249988757, 1.634375000341421691, 0.000000000000000000 ) ) ;
#54879 = CARTESIAN_POINT ( 'NONE',  ( 1.195565668251681535, 1.858513546554524609, -0.7743570246632487386 ) ) ;
#54880 = ORIENTED_EDGE ( 'NONE', *, *, #134668, .T. ) ;
#54881 = CARTESIAN_POINT ( 'NONE',  ( -0.01776408051935850912, -2.116861762172245420, -0.04693027993646693707 ) ) ;
#54882 = CARTESIAN_POINT ( 'NONE',  ( 11.99989233169111991, 6.624601663682995856, 0.5005250340842011259 ) ) ;
#54883 = CARTESIAN_POINT ( 'NONE',  ( 3.016144355299533952, 2.060630728401948275, -0.2003171163396169074 ) ) ;
#54884 = CARTESIAN_POINT ( 'NONE',  ( 3.553118775233146120, 6.302999783484076524, -1.199719254218453823 ) ) ;
#54885 = CARTESIAN_POINT ( 'NONE',  ( 4.227110032410640095, 8.153655147779589996, 0.7998128361456271485 ) ) ;
#54886 = EDGE_LOOP ( 'NONE', ( #93422, #189119, #106476, #115247 ) ) ;
#54888 = CARTESIAN_POINT ( 'NONE',  ( 4.222474775652216294, 7.013638773981186958, 1.199719254218462483 ) ) ;
#54887 = CARTESIAN_POINT ( 'NONE',  ( 4.593745122936496728, -2.090168268563397547, -0.05157397306862486486 ) ) ;
#54891 = ORIENTED_EDGE ( 'NONE', *, *, #34539, .T. ) ;
#54890 = CARTESIAN_POINT ( 'NONE',  ( 1.330386229028382772, 1.216896677575128205, -1.342046333077246967 ) ) ;
#54889 = CARTESIAN_POINT ( 'NONE',  ( 2.608196206841297826, -0.6965810133783244540, -1.687657492251873226 ) ) ;
#54892 = CARTESIAN_POINT ( 'NONE',  ( 6.516270054225981490, -1.036149114087565382, -1.948532232987249424 ) ) ;
#54893 = CARTESIAN_POINT ( 'NONE',  ( 0.000000000000000000, -9.919999999999998153, 0.000000000000000000 ) ) ;
#54894 = CARTESIAN_POINT ( 'NONE',  ( 3.944505925199864649, 2.195883038551619038, 0.2190369969904403802 ) ) ;
#54896 =( BOUNDED_SURFACE ( )  B_SPLINE_SURFACE ( 3, 2, ( 
 ( #60927, #83279, #58791 ),
 ( #17204, #126008, #29504 ),
 ( #145429, #49728, #115857 ),
 ( #33478, #99551, #165615 ),
 ( #144362, #93455, #194120 ),
 ( #207167, #193047, #143289 ) ),
 .UNSPECIFIED., .F., .F., .F. ) 
 B_SPLINE_SURFACE_WITH_KNOTS ( ( 4, 2, 4 ),
 ( 3, 3 ),
 ( 0.000000000000000000, 0.0003831327362561329415, 0.0007662654725122658829 ),
 ( 0.000000000000000000, 1.000000000000000000 ),
 .UNSPECIFIED. ) 
 GEOMETRIC_REPRESENTATION_ITEM ( )  RATIONAL_B_SPLINE_SURFACE ( (
 ( 1.000000000000000000, 0.5879095031487664436, 1.000000000000000000),
 ( 1.000000000000000000, 0.5873691247590056008, 1.000000000000000000),
 ( 1.000000000000000000, 0.6054349545482283768, 1.000000000000000000),
 ( 1.000000000000000000, 0.6533334602781794009, 1.000000000000000000),
 ( 1.000000000000000000, 0.6828746263139577888, 1.000000000000000000),
 ( 1.000000000000000000, 0.7071067811865475727, 1.000000000000000000) ) ) 
 REPRESENTATION_ITEM ( '' )  SURFACE ( )  );
#54895 = CARTESIAN_POINT ( 'NONE',  ( -1.402160292154681736E-14, 8.734375000341403350, 1.575800808251682339 ) ) ;
#54897 = CARTESIAN_POINT ( 'NONE',  ( 2.701700744156261713, 1.353761940859641966, 1.350867010771430676 ) ) ;
#54898 = CARTESIAN_POINT ( 'NONE',  ( -4.634189577772691138, 4.300976017023221409, 1.214306433183764966E-14 ) ) ;
#54899 = CARTESIAN_POINT ( 'NONE',  ( 9.271078113646423091, 9.710679308875986848, 1.040834085586084257E-14 ) ) ;
#54900 = CARTESIAN_POINT ( 'NONE',  ( 6.812946544903684121, -1.603000239855886466, 1.309962327488790157 ) ) ;
#54901 = CARTESIAN_POINT ( 'NONE',  ( 0.6801582343749970061, 0.8385416670080649837, -1.178068619123841643 ) ) ;
#54902 = CARTESIAN_POINT ( 'NONE',  ( 6.339412547452306868, 0.8406370108028878851, -2.024118718474729128 ) ) ;
#54903 = CARTESIAN_POINT ( 'NONE',  ( 4.960800185296459830, 8.075801985472857325, -1.085925974634168290 ) ) ;
#54904 = CARTESIAN_POINT ( 'NONE',  ( -9.367496996292747014, 15.51845925589211106, -7.500000001629759439 ) ) ;
#54905 = ORIENTED_EDGE ( 'NONE', *, *, #77903, .F. ) ;
#54906 = VERTEX_POINT ( 'NONE', #82315 ) ;
#54907 = VECTOR ( 'NONE', #173947, 1000.000000000000000 ) ;
#54908 = CARTESIAN_POINT ( 'NONE',  ( 1.324925973730993745, -1.296446089449550421, 1.500000000000000666 ) ) ;
#54909 = EDGE_CURVE ( 'NONE', #30835, #156842, #63945, .T. ) ;
#54910 = CARTESIAN_POINT ( 'NONE',  ( 3.374138713240721454, -1.116850685118627728, 1.500355210514233262 ) ) ;
#54911 = CARTESIAN_POINT ( 'NONE',  ( -0.02319159430947542039, 0.2540490248266329965, -1.846305437520213477 ) ) ;
#54912 = CARTESIAN_POINT ( 'NONE',  ( 5.234856708652227297, 7.200695141551334721, 1.443375672974065660 ) ) ;
#54913 = CARTESIAN_POINT ( 'NONE',  ( -6.832946231607472498, 9.955225789308602913, 1.082531754730549967 ) ) ;
#54914 = CARTESIAN_POINT ( 'NONE',  ( 4.923546060418115822, 5.773167154356443120, -1.199719254218452047 ) ) ;
#54915 = CARTESIAN_POINT ( 'NONE',  ( 6.684440181240522527, 1.196966437107028547, -1.688953195037292243 ) ) ;
#54916 = CARTESIAN_POINT ( 'NONE',  ( 1.528922965942226986, -1.701935853630029083, 1.081086586856384590 ) ) ;
#54917 = CARTESIAN_POINT ( 'NONE',  ( -9.972185678051314284, 11.59297036493672017, 1.199719254218462483 ) ) ;
#54918 = CARTESIAN_POINT ( 'NONE',  ( 7.289443866002793371, 8.533381260871966134, 1.199719254218452047 ) ) ;
#54919 = DIRECTION ( 'NONE',  ( -0.7592566023652990159, -0.6507913734559659380, 1.175982368226361821E-15 ) ) ;
#54920 = CARTESIAN_POINT ( 'NONE',  ( 1.517799938645987057, -1.219565478727736574, -1.820545776841306029 ) ) ;
#54921 = CARTESIAN_POINT ( 'NONE',  ( 4.828627627824715773, 1.747987318788373656, 0.5269492854979712648 ) ) ;
#54922 = CARTESIAN_POINT ( 'NONE',  ( -2.598358995313378550, 6.183169261174235487, 0.7998128361456341429 ) ) ;
#54923 = CARTESIAN_POINT ( 'NONE',  ( 5.397554552016212703, 8.350878506444006533, 1.082531754730547524 ) ) ;
#54924 = CARTESIAN_POINT ( 'NONE',  ( 8.401248741962376698, 12.95320729893149370, 0.7998128361456462443 ) ) ;
#54925 = CARTESIAN_POINT ( 'NONE',  ( -4.132202957115018727, 8.042930226601317401, 0.000000000000000000 ) ) ;
#54926 = CARTESIAN_POINT ( 'NONE',  ( 4.029797971759831121, 5.724516938518342535, -1.599625672291255185 ) ) ;
#54927 = CARTESIAN_POINT ( 'NONE',  ( 3.607351389687783794, 6.366271167014519783, 1.199719254218451159 ) ) ;
#54928 = EDGE_LOOP ( 'NONE', ( #190275, #95401, #153719, #46724 ) ) ;
#54930 = CARTESIAN_POINT ( 'NONE',  ( 0.7330649400898289203, 1.860844449999502492, 0.7684416140155255759 ) ) ;
#54929 = CARTESIAN_POINT ( 'NONE',  ( 3.755264181858387840, 1.826884192416846631, -0.2291247506851084581 ) ) ;
#54931 = CARTESIAN_POINT ( 'NONE',  ( 1.564254705693722602, 1.878715736396416203, -1.323808166466547087 ) ) ;
#54933 = CARTESIAN_POINT ( 'NONE',  ( 6.754749089495472703, -0.5201146403621333958, -1.891512521893109700 ) ) ;
#54932 = CARTESIAN_POINT ( 'NONE',  ( 4.867013957625893283, 4.780530493426062399, 1.040834085586084257E-14 ) ) ;
#54934 = CARTESIAN_POINT ( 'NONE',  ( -3.418627288940168096, 7.140148937072163804, -0.7998128361456281477 ) ) ;
#54935 = DIRECTION ( 'NONE',  ( -0.000000000000000000, -1.000000000000000000, -0.000000000000000000 ) ) ;
#54936 = CARTESIAN_POINT ( 'NONE',  ( 3.533378866418676711, -0.1359047358975660202, 1.907598245988059826 ) ) ;
#54937 = CARTESIAN_POINT ( 'NONE',  ( -9.484092147959342967, 11.02352791316275216, 1.199719254218462483 ) ) ;
#54938 = CARTESIAN_POINT ( 'NONE',  ( 6.011645680221167076, 7.072102904328817274, -1.053258377668888857 ) ) ;
#54939 = CARTESIAN_POINT ( 'NONE',  ( -3.851398154733808088, 6.650992392901508232, -1.199719254218450271 ) ) ;
#54941 = CARTESIAN_POINT ( 'NONE',  ( 0.8482696660519238874, 0.5391449902514727777, 1.791282564952957124 ) ) ;
#54940 = CARTESIAN_POINT ( 'NONE',  ( 2.208638616728377357, 1.868957087031404285, 0.9372459875717062960 ) ) ;
#54942 = CARTESIAN_POINT ( 'NONE',  ( 1.616564310028177243, 0.5879328921069119085, -1.928455639302439462 ) ) ;
#54943 = CARTESIAN_POINT ( 'NONE',  ( 8.771762198361678031, 9.336070107617867819, 1.040834085586084257E-14 ) ) ;
#54944 = CARTESIAN_POINT ( 'NONE',  ( 1.364683531249988535, 4.176041667008080438, 0.7879004041258499402 ) ) ;
#54945 = CARTESIAN_POINT ( 'NONE',  ( 3.561793593276740388, -1.166016580864630781, 1.292293876973077182 ) ) ;
#54946 = CARTESIAN_POINT ( 'NONE',  ( 4.039439701867726384, 6.800097854565950506, 1.199719254218462483 ) ) ;
#54947 = DIRECTION ( 'NONE',  ( 1.000000000000000000, -0.000000000000000000, -0.000000000000000000 ) ) ;
#54948 = CARTESIAN_POINT ( 'NONE',  ( 3.580403817701179658, -1.662759015092404535, -0.4584509792747801793 ) ) ;
#54949 = CARTESIAN_POINT ( 'NONE',  ( 3.808297599986898430, 1.548825491099754315, -1.550762550882843094 ) ) ;
#54950 = CARTESIAN_POINT ( 'NONE',  ( 5.865903189996044098, 2.174886565178067777, -0.3735607071253948530 ) ) ;
#54951 = CARTESIAN_POINT ( 'NONE',  ( -10.39336823037077195, 4.932734307774878424, -5.330979603150785451 ) ) ;
#54952 =( BOUNDED_CURVE ( )  B_SPLINE_CURVE ( 2, ( #158226, #9816, #60700, #175541, #110596 ),
 .UNSPECIFIED., .F., .T. ) 
 B_SPLINE_CURVE_WITH_KNOTS ( ( 3, 2, 3 ),
 ( 0.000000000000000000, 0.3063186054016480142, 1.000000000000000000 ),
 .UNSPECIFIED. ) 
 CURVE ( )  GEOMETRIC_REPRESENTATION_ITEM ( )  RATIONAL_B_SPLINE_CURVE ( ( 0.9866942343795712667, 0.9929791993688333873, 1.000000000000000000, 0.9841008718140421552, 0.9719753288332495522 ) ) 
 REPRESENTATION_ITEM ( '' )  );
#54953 = PRESENTATION_LAYER_ASSIGNMENT (  '', '', ( #106962 ) ) ;
#54954 = CARTESIAN_POINT ( 'NONE',  ( 3.749033319061449543, -0.4183670367851847205, -2.130223169982926379 ) ) ;
#54955 = CARTESIAN_POINT ( 'NONE',  ( 2.191784710619415044, -0.7813054520266484726, 1.650194661559079456 ) ) ;
#54956 = CARTESIAN_POINT ( 'NONE',  ( -3.511198596259295535, 6.271927390929313617, -1.000000000000001776 ) ) ;
#54957 = CARTESIAN_POINT ( 'NONE',  ( 4.751218706475199838, 0.2043725092088227169, -2.107420708596031922 ) ) ;
#54958 = CARTESIAN_POINT ( 'NONE',  ( 6.609000000000036401, 7.629137130509070275, 2.600000000000000977 ) ) ;
#54959 = EDGE_CURVE ( 'NONE', #184764, #111689, #160222, .T. ) ;
#54960 = ORIENTED_EDGE ( 'NONE', *, *, #128510, .T. ) ;
#54962 = CARTESIAN_POINT ( 'NONE',  ( -0.6823417656250212460, 3.113541667008084879, 1.181850606188767472 ) ) ;
#54961 = CARTESIAN_POINT ( 'NONE',  ( 4.704755546018094314, 1.993839351151542427, 1.131020188671335136 ) ) ;
#54963 = CARTESIAN_POINT ( 'NONE',  ( 6.620655732516627090, 3.711369741872071693, 2.240970959566997323 ) ) ;
#54964 = CARTESIAN_POINT ( 'NONE',  ( 8.367353357928214663, 12.91366268422496688, 1.040834085586084257E-14 ) ) ;
#54965 = CARTESIAN_POINT ( 'NONE',  ( 0.3113914200543760336, 1.760583737686383321, -1.181573663439141830 ) ) ;
#54966 = CARTESIAN_POINT ( 'NONE',  ( -6.073689629242165822, 7.148687991279732756, -1.082531754730544860 ) ) ;
#54967 = CARTESIAN_POINT ( 'NONE',  ( 4.053524740805938720, 3.831459740469437936, 1.214306433183764966E-14 ) ) ;
#54968 = CARTESIAN_POINT ( 'NONE',  ( -6.209271164934474285, 6.346497235286081562, 1.040834085586084257E-14 ) ) ;
#54969 = CIRCLE ( 'NONE', #34238, 0.08000000000000020983 ) ;
#54970 = CARTESIAN_POINT ( 'NONE',  ( -10.99943594186085605, -9.910930717204488261, 0.1113955156350721065 ) ) ;
#54971 = VERTEX_POINT ( 'NONE', #115952 ) ;
#54972 = CARTESIAN_POINT ( 'NONE',  ( 5.186172726741035355, 1.650080556555008293, 1.158690440749516881 ) ) ;
#54974 = CARTESIAN_POINT ( 'NONE',  ( 2.940340207046471921, -1.064325496585982078, 1.766646112275678693 ) ) ;
#54973 = CARTESIAN_POINT ( 'NONE',  ( 3.811813743736467419, 7.598866467667865443, 1.040834085586084257E-14 ) ) ;
#54976 = CARTESIAN_POINT ( 'NONE',  ( 6.883263157960366918, 3.696842586722656865, 2.460469087180997327 ) ) ;
#54975 = CARTESIAN_POINT ( 'NONE',  ( 5.830888582329017744, 8.960397891762626799, -1.199719254218452047 ) ) ;
#54977 = CARTESIAN_POINT ( 'NONE',  ( 5.742760583840166966, 8.857581893525663830, 1.199719254218452047 ) ) ;
#54978 = CARTESIAN_POINT ( 'NONE',  ( 3.285556943750000070, -1.334374999522040861, 0.000000000000000000 ) ) ;
#54979 = DIRECTION ( 'NONE',  ( 1.000000000000000000, -0.000000000000000000, -0.000000000000000000 ) ) ;
#54980 = CARTESIAN_POINT ( 'NONE',  ( 5.841772037242090931, 2.188765561305112683, 0.1107676204459909497 ) ) ;
#54981 = CARTESIAN_POINT ( 'NONE',  ( 5.063125043234593115, -1.117834493326537393, 1.678003986596336761 ) ) ;
#54982 = CARTESIAN_POINT ( 'NONE',  ( 3.175182228840720988, 1.170341537027960843, 1.421418621496411516 ) ) ;
#54983 = EDGE_CURVE ( 'NONE', #28024, #121080, #164648, .T. ) ;
#54984 = CARTESIAN_POINT ( 'NONE',  ( 4.873266149108180123, 7.772895376346490970, 1.199719254218462483 ) ) ;
#54985 = CARTESIAN_POINT ( 'NONE',  ( 1.061059408578250318, 0.3424711756105159877, -1.690240703899626107 ) ) ;
#54986 = PLANE ( 'NONE',  #96209 ) ;
#54987 = CARTESIAN_POINT ( 'NONE',  ( 0.7394344266866456072, 2.295659475925112769, -0.1205738325454289578 ) ) ;
#54988 = CARTESIAN_POINT ( 'NONE',  ( -5.870844209917351009, 6.808071985447069707, -1.199719254218446718 ) ) ;
#54989 = CARTESIAN_POINT ( 'NONE',  ( 0.5798237426192736077, 2.110460337659907371, -0.8156065903286384700 ) ) ;
#54990 = CARTESIAN_POINT ( 'NONE',  ( 3.281953686177707219, 1.336396692706752765, 1.627740544975244008 ) ) ;
#54991 = CARTESIAN_POINT ( 'NONE',  ( -3.962726036944197894, 7.845207153068690431, -0.7998128361456481317 ) ) ;
#54992 = CARTESIAN_POINT ( 'NONE',  ( 6.805303039055573322, 10.02693841461847057, 1.199719254218460707 ) ) ;
#54993 = CARTESIAN_POINT ( 'NONE',  ( 5.343321937117211817, 9.247976336696488886, 0.000000000000000000 ) ) ;
#54994 = CARTESIAN_POINT ( 'NONE',  ( 6.312500000001141309, 1.451031289089316667, 1.451031289060858098 ) ) ;
#54995 = CARTESIAN_POINT ( 'NONE',  ( -6.714312387265696458, 8.856450423275211037, 1.599625672291283607 ) ) ;
#54996 = CARTESIAN_POINT ( 'NONE',  ( 5.599154252319471503, 9.476171027773981237, -0.7216878364870267237 ) ) ;
#54997 = CARTESIAN_POINT ( 'NONE',  ( 5.168313817042160530, 6.667327647676385638, 1.400930397336812572 ) ) ;
#54998 = CARTESIAN_POINT ( 'NONE',  ( -3.750802052474980108, 7.527686161196117887, 1.040834085586084257E-14 ) ) ;
#55000 = CARTESIAN_POINT ( 'NONE',  ( 4.482826657505923684, -1.449732756002309664, 1.683255901693592849 ) ) ;
#54999 = CARTESIAN_POINT ( 'NONE',  ( 2.338272602237463360, -1.224740070204191289, -1.730971256048131401 ) ) ;
#55001 = CARTESIAN_POINT ( 'NONE',  ( 2.625153213768507854, -2.044362554934661791, 0.7897752707372793779 ) ) ;
#55002 = CARTESIAN_POINT ( 'NONE',  ( -6.847031270101295419, 7.946956888995021728, -1.199719254218446718 ) ) ;
#55004 = MECHANICAL_DESIGN_GEOMETRIC_PRESENTATION_REPRESENTATION (  '', ( #61809 ), #210527 ) ;
#55003 = CARTESIAN_POINT ( 'NONE',  ( -5.659602779061863487, 5.567567761852417085, 0.7998128361456281477 ) ) ;
#55005 = CARTESIAN_POINT ( 'NONE',  ( 5.371523934717264304, -0.2895824386080196322, 1.940264742196501802 ) ) ;
#55006 = CARTESIAN_POINT ( 'NONE',  ( 1.364683531249986537, 2.405208333674752286, -0.7879004041258239610 ) ) ;
#55007 = CARTESIAN_POINT ( 'NONE',  ( -4.340018570150322219, 5.196348098997705556, -1.082531754730551743 ) ) ;
#55009 = ORIENTED_EDGE ( 'NONE', *, *, #75599, .T. ) ;
#55008 = CARTESIAN_POINT ( 'NONE',  ( -6.087247782855839340, 6.204136622861004646, 0.000000000000000000 ) ) ;
#55010 = CARTESIAN_POINT ( 'NONE',  ( 4.289387122732970958, -0.003046686910593982868, -2.120778211268215419 ) ) ;
#55011 = CARTESIAN_POINT ( 'NONE',  ( -3.902768115887413014, 5.646591783325653147, -1.599625672291283607 ) ) ;
#55012 = ORIENTED_EDGE ( 'NONE', *, *, #132223, .F. ) ;
#55013 = CARTESIAN_POINT ( 'NONE',  ( 6.034075718726629844, 1.069613854859407631, -1.878468107683453514 ) ) ;
#55014 = CARTESIAN_POINT ( 'NONE',  ( 6.654354466208897811, 6.657835053532175529, 0.7998128361456341429 ) ) ;
#55015 = CARTESIAN_POINT ( 'NONE',  ( 4.968220237687512864, -1.735557695065930606, -0.6152675618510683453 ) ) ;
#55016 = CARTESIAN_POINT ( 'NONE',  ( -5.863297782511878609, 6.029266553239049919, -0.3729355709888391157 ) ) ;
#55017 = CARTESIAN_POINT ( 'NONE',  ( -0.6823417656250212460, 1.613541667008083769, 1.181850606188755259 ) ) ;
#55018 = CARTESIAN_POINT ( 'NONE',  ( 6.720655732516681802, 0.008434553976941013345, 1.726293928996263549 ) ) ;
#55019 = SPHERICAL_SURFACE ( 'NONE', #167184, 0.08000000000000000167 ) ;
#55020 = CARTESIAN_POINT ( 'NONE',  ( -0.04359940615404794828, 3.409091168011650463, 2.082493747991086330 ) ) ;
#55021 = DIRECTION ( 'NONE',  ( 0.000000000000000000, 0.000000000000000000, -1.000000000000000000 ) ) ;
#55022 = CARTESIAN_POINT ( 'NONE',  ( 4.504844740329728481, 1.672958716126593082, -1.369014088531981255 ) ) ;
#55023 = AXIS2_PLACEMENT_3D ( 'NONE', #167253, #18839, #35095 ) ;
#55024 = CARTESIAN_POINT ( 'NONE',  ( -4.086893239515592136, 6.855460315155083251, 1.199719254218464037 ) ) ;
#55025 = CARTESIAN_POINT ( 'NONE',  ( -6.493992390821436977, 10.52014885602626393, 0.7216878364870458196 ) ) ;
#55026 = CARTESIAN_POINT ( 'NONE',  ( 3.362350911093567873, 0.9703303321016673033, 1.931748911306984784 ) ) ;
#55027 = CARTESIAN_POINT ( 'NONE',  ( 4.516842978191152547, 1.801120551983675266, 0.8018027747202867150 ) ) ;
#55028 = CARTESIAN_POINT ( 'NONE',  ( 4.130049176863603400, 0.2125952495928511154, -1.720681531008328768 ) ) ;
#55029 = EDGE_CURVE ( 'NONE', #138277, #160319, #111910, .T. ) ;
#55030 = CARTESIAN_POINT ( 'NONE',  ( 0.6268464039562298140, 0.1668571106153530770, 2.185281662807083691 ) ) ;
#55031 = CARTESIAN_POINT ( 'NONE',  ( 1.712421914926518518, -2.289955115012487052, 0.2841115493098354539 ) ) ;
#55032 = CARTESIAN_POINT ( 'NONE',  ( 3.778635366994155032, -1.985013167256908240, -0.5533215937988352762 ) ) ;
#55033 = CARTESIAN_POINT ( 'NONE',  ( 5.548367435846999207, -1.528527190574509032, 1.197884188273186323 ) ) ;
#55034 = CARTESIAN_POINT ( 'NONE',  ( -7.497295758232724872, 9.769931022736756177, -1.443375672974058777 ) ) ;
#55036 = EDGE_CURVE ( 'NONE', #200044, #61984, #152932, .T. ) ;
#55035 = CARTESIAN_POINT ( 'NONE',  ( -6.089547271193396227, 7.133501900260939443, -1.199719254218453823 ) ) ;
#55037 = CARTESIAN_POINT ( 'NONE',  ( -1.946531837068944615, 3.754233237397059497, -0.4615996190889526951 ) ) ;
#55038 = CARTESIAN_POINT ( 'NONE',  ( -6.792271770322117597, 9.907772251142352715, 1.082531754730549967 ) ) ;
#55039 = CARTESIAN_POINT ( 'NONE',  ( 2.907470687441279455, 1.863611109782586484, 1.181582751932461095 ) ) ;
#55040 = CARTESIAN_POINT ( 'NONE',  ( -3.285556943750000070, -2.996874999522041616, 0.000000000000000000 ) ) ;
#55041 = VERTEX_POINT ( 'NONE', #12677 ) ;
#55042 = CARTESIAN_POINT ( 'NONE',  ( 0.9888277058803507380, 0.1293858107240040412, 1.856492687334237335 ) ) ;
#55043 = CARTESIAN_POINT ( 'NONE',  ( -0.1291982275798911617, 0.2270562610647832436, -2.107042122458637756 ) ) ;
#55044 = CARTESIAN_POINT ( 'NONE',  ( 4.222827212797172436, 7.545785358913557950, -0.9571512059609885714 ) ) ;
#55046 = CARTESIAN_POINT ( 'NONE',  ( -3.673896439623299148, 4.156855427197417185, -2.420000000000000373 ) ) ;
#55045 = CARTESIAN_POINT ( 'NONE',  ( -6.597731880524014159, 6.769412454161013670, -0.2479414380717175903 ) ) ;
#55047 = CARTESIAN_POINT ( 'NONE',  ( 6.439398882927052981, 0.6998097629446423662, -1.703160347957879850 ) ) ;
#55048 = ORIENTED_EDGE ( 'NONE', *, *, #62840, .T. ) ;
#55049 = CARTESIAN_POINT ( 'NONE',  ( 2.676696200465655373, -1.971695749941338560, -0.5996849476793424394 ) ) ;
#55050 = CARTESIAN_POINT ( 'NONE',  ( -1.360316468750023544, 0.8906250003414064587, -2.602085213965210642E-14 ) ) ;
#55051 = CARTESIAN_POINT ( 'NONE',  ( -8.044065211609668253, 8.279164256499745633, 0.7998128361456602331 ) ) ;
#55052 = CARTESIAN_POINT ( 'NONE',  ( -1.177110729581203774, 3.210371626218858410, -0.7749999999999883649 ) ) ;
#55053 =( LENGTH_UNIT ( ) NAMED_UNIT ( * ) SI_UNIT ( .MILLI., .METRE. ) );
#55054 = CARTESIAN_POINT ( 'NONE',  ( 5.332434488876471868, 5.115595079977664383, 0.7998128361456341429 ) ) ;
#55055 = CARTESIAN_POINT ( 'NONE',  ( 1.411086320874027855, 1.817183042272657145, 0.9721812696896633410 ) ) ;
#55057 = CARTESIAN_POINT ( 'NONE',  ( 0.6823417656249969321, 13.02604166700806232, -1.181850606188757036 ) ) ;
#55056 = CARTESIAN_POINT ( 'NONE',  ( -0.4019237886466933696, 12.55133545031537246, 1.500000000000005995 ) ) ;
#55058 = CARTESIAN_POINT ( 'NONE',  ( 7.332262146892202459, 7.448727347662698506, -0.7998128361456281477 ) ) ;
#55059 = CARTESIAN_POINT ( 'NONE',  ( 4.053528829375365738, 3.783736749027409196, 2.445701138906706706 ) ) ;
#55060 = CARTESIAN_POINT ( 'NONE',  ( 6.147136880733683917, -1.866598994669689926, 1.177069016086537356 ) ) ;
#55061 = CARTESIAN_POINT ( 'NONE',  ( 0.8960494714182369869, -0.7788709108395329705, 2.016556642405589184 ) ) ;
#55062 = CIRCLE ( 'NONE', #144930, 0.7499999999999997780 ) ;
#55063 = CARTESIAN_POINT ( 'NONE',  ( -5.422898255786203769, 6.389431388914436738, -1.082531754730544860 ) ) ;
#55064 = CARTESIAN_POINT ( 'NONE',  ( 0.2988868148526523938, -0.2362956723594503705, -1.897694653714178781 ) ) ;
#55065 = CARTESIAN_POINT ( 'NONE',  ( 1.217982839071569012, 0.9896824804975331569, -1.756856037137774162 ) ) ;
#55066 = CARTESIAN_POINT ( 'NONE',  ( 7.363486825553451354, 8.723727730301414240, -1.082531754730548412 ) ) ;
#55067 = CARTESIAN_POINT ( 'NONE',  ( 1.564254705693722602, 1.878715736396416203, -1.323808166466547087 ) ) ;
#55068 = TOROIDAL_SURFACE ( 'NONE', #183232, 6.330000000000000959, 0.08000000000000000167 ) ;
#55069 =( NAMED_UNIT ( * ) PLANE_ANGLE_UNIT ( ) SI_UNIT ( $, .RADIAN. ) );
#55070 = CARTESIAN_POINT ( 'NONE',  ( 6.428373272941257710, -0.9058926715965059939, -1.684108486221975953 ) ) ;
#55071 = CARTESIAN_POINT ( 'NONE',  ( 1.919948509414024951, 8.999999999999998224, -0.7749999999999996891 ) ) ;
#55072 = CARTESIAN_POINT ( 'NONE',  ( 1.797508989346347619, -0.6330400025267440833, 1.760413054629046625 ) ) ;
#55073 = CARTESIAN_POINT ( 'NONE',  ( 3.766814776335784209, -0.2024620155892907503, -2.006371719556559796 ) ) ;
#55075 = DIRECTION ( 'NONE',  ( -1.000000000000000000, 0.000000000000000000, 0.000000000000000000 ) ) ;
#55074 = CARTESIAN_POINT ( 'NONE',  ( 1.364683531249986537, 0.9052083336747533959, -0.7879004041258239610 ) ) ;
#55077 = CARTESIAN_POINT ( 'NONE',  ( 5.496739094006439785, -0.5105849265115348645, -2.043105244204785453 ) ) ;
#55076 = CARTESIAN_POINT ( 'NONE',  ( -8.585337585951595685, 11.03931315507545108, -1.599625672291263179 ) ) ;
#55078 = CARTESIAN_POINT ( 'NONE',  ( 7.365103760721646076, 9.615707025640515937, 1.599625672291281386 ) ) ;
#55080 = CARTESIAN_POINT ( 'NONE',  ( -7.888146445052511169, 8.097259028849730811, 1.040834085586084257E-14 ) ) ;
#55079 = CARTESIAN_POINT ( 'NONE',  ( 4.061549535745618833, 6.896169004081968090, -1.199719254218452047 ) ) ;
#55081 = CARTESIAN_POINT ( 'NONE',  ( 1.264911064067342217, 3.732455999420146053, -0.4999999999999988343 ) ) ;
#55082 = CARTESIAN_POINT ( 'NONE',  ( 3.937764026144819685, -1.931520177269234306, 0.5904599756008358513 ) ) ;
#55083 = CARTESIAN_POINT ( 'NONE',  ( -1.364683531250012516, 4.488541667008090208, -0.7879004041258300672 ) ) ;
#55084 = CARTESIAN_POINT ( 'NONE',  ( 5.986801016505616246, 1.986937900772387078, 0.5535461689152029185 ) ) ;
#55085 = CARTESIAN_POINT ( 'NONE',  ( 8.215877900201359552, 11.56864606933486606, -1.082531754730543083 ) ) ;
#55086 = CARTESIAN_POINT ( 'NONE',  ( 5.097027542433036018, 1.800287743887505343, -1.196142203056582920 ) ) ;
#55087 = CARTESIAN_POINT ( 'NONE',  ( 7.049313524462606395, 7.188896964819984525, 0.000000000000000000 ) ) ;
#55088 = CARTESIAN_POINT ( 'NONE',  ( 1.364683531249984538, -1.032291666325247714, -0.7879004041258309554 ) ) ;
#55090 = DIRECTION ( 'NONE',  ( 5.551115123125764213E-17, 0.000000000000000000, -1.000000000000000000 ) ) ;
#55089 = CARTESIAN_POINT ( 'NONE',  ( 6.475954649182838807, 7.584310507915338562, 1.199719254218452047 ) ) ;
#55091 = CARTESIAN_POINT ( 'NONE',  ( 7.904040366642695048, 9.284097184913720824, 1.082531754730558626 ) ) ;
#55093 = LINE ( 'NONE', #174203, #28039 ) ;
#55092 = CARTESIAN_POINT ( 'NONE',  ( 2.541674676231266083, 1.985806779098505448, -0.8781977400831306735 ) ) ;
#55095 = CARTESIAN_POINT ( 'NONE',  ( 1.628196140939692338, 0.1813696128579282696, 1.832309401408799276 ) ) ;
#55094 = CARTESIAN_POINT ( 'NONE',  ( -6.738039156311804945, 6.963393225226301553, 1.040834085586084257E-14 ) ) ;
#55096 = CARTESIAN_POINT ( 'NONE',  ( 1.364683531249988535, 3.655208333674750509, -0.7879004041258239610 ) ) ;
#55097 = CARTESIAN_POINT ( 'NONE',  ( 3.368858348882136422, 0.05182064297618373117, -2.191103300807801801 ) ) ;
#55098 = CARTESIAN_POINT ( 'NONE',  ( 6.883263157960371359, 1.234153227268469877, 2.265917448979277271 ) ) ;
#55099 = CARTESIAN_POINT ( 'NONE',  ( 3.186655532321683637, -2.228779239134215384, -0.3884498486929898742 ) ) ;
#55100 = CARTESIAN_POINT ( 'NONE',  ( -5.636439174979254396, 7.598931675607687453, -1.599625672291256295 ) ) ;
#55101 = CARTESIAN_POINT ( 'NONE',  ( -11.84668730067608244, 10.09363775091779125, 1.399999999999998357 ) ) ;
#55102 = CARTESIAN_POINT ( 'NONE',  ( 6.465908158583062892, 6.764574590967027845, 0.2795716154820517829 ) ) ;
#55103 = CARTESIAN_POINT ( 'NONE',  ( 1.499999999999993117, 13.85416666666666430, 0.8660254037844409281 ) ) ;
#55104 = CARTESIAN_POINT ( 'NONE',  ( 4.407809338218622308, 8.156544971314787063, 0.000000000000000000 ) ) ;
#55105 = CARTESIAN_POINT ( 'NONE',  ( 5.958207135543601041, 0.7187401461678426529, 1.617382982224302879 ) ) ;
#55107 = CARTESIAN_POINT ( 'NONE',  ( 3.281892451336921201, 1.963554472591656053, -0.4431533499722385416 ) ) ;
#55106 = PRESENTATION_LAYER_ASSIGNMENT (  '', '', ( #27424 ) ) ;
#55108 = CARTESIAN_POINT ( 'NONE',  ( 8.633844893804129228, 8.967240552393299424, -0.7998128361456211532 ) ) ;
#55109 = CARTESIAN_POINT ( 'NONE',  ( 1.641775563537830829, -1.524941811188656127, -1.452692102197229884 ) ) ;
#55111 = CARTESIAN_POINT ( 'NONE',  ( -1.201851678989727383E-14, 2.462500000000023004, 1.732050807568877637 ) ) ;
#55110 = CARTESIAN_POINT ( 'NONE',  ( 1.364683531249996529, 12.21354166700805877, 0.7879004041258405033 ) ) ;
#55112 = CARTESIAN_POINT ( 'NONE',  ( 0.7484202955074462649, -1.954263247020354477, -0.2444711731117015785 ) ) ;
#55113 = CARTESIAN_POINT ( 'NONE',  ( -4.092446641025072829, 3.979529022206003575, 0.4031905389056175126 ) ) ;
#55114 = CARTESIAN_POINT ( 'NONE',  ( -9.340702556249549815, 15.44694763438218033, -7.462845556860568941 ) ) ;
#55116 = ORIENTED_EDGE ( 'NONE', *, *, #105176, .T. ) ;
#55115 = CARTESIAN_POINT ( 'NONE',  ( 6.099861030166984222, 1.256130149795838813, 1.305615287863689078 ) ) ;
#55117 = CARTESIAN_POINT ( 'NONE',  ( 7.131225611108100715, 7.422110755822004968, 0.7216878364870317197 ) ) ;
#55118 = CARTESIAN_POINT ( 'NONE',  ( -1.364683531250000748, -0.9281249996585805295, 0.000000000000000000 ) ) ;
#55119 = CARTESIAN_POINT ( 'NONE',  ( 4.434354141042872399, 1.834536173243521917, 0.3649259964926266364 ) ) ;
#55120 = CARTESIAN_POINT ( 'NONE',  ( 4.054051625686104998, 4.688480637177271149, -1.199719254218446718 ) ) ;
#55121 = CARTESIAN_POINT ( 'NONE',  ( 5.295788417638883416, -1.460108768623759712, -1.467927865959644640 ) ) ;
#55122 = CARTESIAN_POINT ( 'NONE',  ( -0.6124999999999967137, 1.708333333333339477, -1.060881119635938008 ) ) ;
#55123 = CARTESIAN_POINT ( 'NONE',  ( -5.356880090730904875, 7.343055753976412525, 1.443375672974058777 ) ) ;
#55124 = CARTESIAN_POINT ( 'NONE',  ( 2.529878086979381546, -0.9588891237051863081, 2.284325849096846106 ) ) ;
#55125 = CARTESIAN_POINT ( 'NONE',  ( -1.500000000000015099, 0.3791666666666850261, -0.8660254037844383745 ) ) ;
#55126 = CARTESIAN_POINT ( 'NONE',  ( 7.263417608619159083, 9.497073181520933716, -1.599625672291262513 ) ) ;
#55127 = CARTESIAN_POINT ( 'NONE',  ( -8.585337585951595685, 11.03931315507545108, -1.599625672291263179 ) ) ;
#55128 = CARTESIAN_POINT ( 'NONE',  ( 5.006703865196457492, 9.063181286029688977, 0.000000000000000000 ) ) ;
#55129 = CARTESIAN_POINT ( 'NONE',  ( 0.6823417656249882723, 0.09270833367475139752, 1.181850606188755259 ) ) ;
#55130 = CARTESIAN_POINT ( 'NONE',  ( -1.500000000000001332, 0.9000000000000187850, 0.000000000000000000 ) ) ;
#55132 = CARTESIAN_POINT ( 'NONE',  ( 5.834086172582112262, 5.700855377634248100, 1.040834085586084257E-14 ) ) ;
#55131 = CARTESIAN_POINT ( 'NONE',  ( 4.633228507203630997, 0.002057781214020309134, -1.962046631861932067 ) ) ;
#55133 = CARTESIAN_POINT ( 'NONE',  ( 2.442732317853496760, 1.238130588059358717, 1.591075322344523535 ) ) ;
#55134 = CARTESIAN_POINT ( 'NONE',  ( -0.1108833634137009749, 4.092508091048022933, -2.451885048449681470 ) ) ;
#55135 = CARTESIAN_POINT ( 'NONE',  ( -0.05867695357848409787, -1.698172713885632401, -1.384993232510664640 ) ) ;
#55136 = CARTESIAN_POINT ( 'NONE',  ( -11.91292854676714974, 9.985184703269748496, 1.446370920797324100 ) ) ;
#55137 = CARTESIAN_POINT ( 'NONE',  ( 2.372138566722302500, -1.154253592077842727, 1.471842878544210809 ) ) ;
#55138 = CARTESIAN_POINT ( 'NONE',  ( 0.6823417656249899377, 5.176041667008086655, -1.181850606188754593 ) ) ;
#55139 = CARTESIAN_POINT ( 'NONE',  ( 3.920185232657522167, -2.007512044478755531, 0.1524921764288286741 ) ) ;
#55140 = CARTESIAN_POINT ( 'NONE',  ( -6.821723845970312894, 11.11042825360738284, 0.000000000000000000 ) ) ;
#55142 = CARTESIAN_POINT ( 'NONE',  ( 4.446934944069580453, -1.891868754433777555, -0.9506184929228760350 ) ) ;
#55141 = CARTESIAN_POINT ( 'NONE',  ( -5.504247177468192476, 7.444707678511436555, 1.443375672974064550 ) ) ;
#55143 = LINE ( 'NONE', #103900, #35328 ) ;
#55144 = CARTESIAN_POINT ( 'NONE',  ( 5.811005889236001032, -1.634438611397070806, 1.270752202701043609 ) ) ;
#55146 = CARTESIAN_POINT ( 'NONE',  ( 6.620655732516607550, 2.431211045237289703, 2.455576803978098521 ) ) ;
#55145 = CARTESIAN_POINT ( 'NONE',  ( 1.066094891556510271, -1.323660828648763221, 1.618394379614082723 ) ) ;
#55148 = EDGE_LOOP ( 'NONE', ( #67836, #66824, #103105, #88537, #46654 ) ) ;
#55147 = CARTESIAN_POINT ( 'NONE',  ( 6.510779352739587189, 1.350450193652263930, -1.228632259304612839 ) ) ;
#55149 = CARTESIAN_POINT ( 'NONE',  ( 7.751511138711133064, 10.06651563329490529, -1.599625672291262513 ) ) ;
#55150 = CARTESIAN_POINT ( 'NONE',  ( 8.103009739377982967, -6.893137084989842123, -7.439168848974014203 ) ) ;
#55151 = AXIS2_PLACEMENT_3D ( 'NONE', #7899, #57739, #169348 ) ;
#55152 = CARTESIAN_POINT ( 'NONE',  ( -11.16150260363039060, 4.727604019697102977, 6.014961758122009172 ) ) ;
#55153 = CARTESIAN_POINT ( 'NONE',  ( 7.795575137733369075, 9.157554417852841411, -1.082531754730537976 ) ) ;
#55154 = CARTESIAN_POINT ( 'NONE',  ( -0.6823417656250039265, 12.88020833367473017, -1.181850606188755259 ) ) ;
#55155 = CARTESIAN_POINT ( 'NONE',  ( 5.971340724440283410, -1.642497693792897451, -0.9790476769208908969 ) ) ;
#55156 = CARTESIAN_POINT ( 'NONE',  ( -6.320072162264675164, 10.52516795595079557, 0.7998128361456481317 ) ) ;
#55157 = CARTESIAN_POINT ( 'NONE',  ( 5.168682875307768931, 7.053215992657626110, -1.599625672291256295 ) ) ;
#55158 = DIRECTION ( 'NONE',  ( -0.6507913734559640506, -0.7592566023653004592, 0.000000000000000000 ) ) ;
#55159 = CARTESIAN_POINT ( 'NONE',  ( 3.429849674132933846, 5.024577257953626308, -1.443375672974058777 ) ) ;
#55160 = DIRECTION ( 'NONE',  ( 0.000000000000000000, -0.7766560405359869135, 0.6299249119529750640 ) ) ;
#55161 = CARTESIAN_POINT ( 'NONE',  ( 2.496672843210871129, 6.064535417054653266, -0.7998128361456291469 ) ) ;
#55162 = VERTEX_POINT ( 'NONE', #178411 ) ;
#55163 = EDGE_CURVE ( 'NONE', #47720, #120769, #134920, .T. ) ;
#55165 = EDGE_CURVE ( 'NONE', #173308, #42462, #44149, .T. ) ;
#55164 = VECTOR ( 'NONE', #138306, 1000.000000000000000 ) ;
#55166 = CARTESIAN_POINT ( 'NONE',  ( 6.134388704033759687, 0.6352148712998658686, 1.913799669303432927 ) ) ;
#55167 = CARTESIAN_POINT ( 'NONE',  ( 0.7156801077207708417, 1.735845614737155707, 1.217653249118654468 ) ) ;
#55168 = DIRECTION ( 'NONE',  ( 0.6250000000674432732, -1.452638498762078799E-08, 0.7806247497458018714 ) ) ;
#55169 = CARTESIAN_POINT ( 'NONE',  ( -0.1394461523061196473, 5.719344608737997326, -2.874279450258274249 ) ) ;
#55170 = CARTESIAN_POINT ( 'NONE',  ( -4.270455198624581783, 7.926022131796578662, 1.040834085586084257E-14 ) ) ;
#55171 = CARTESIAN_POINT ( 'NONE',  ( 9.408995418203963013, 12.00024729270324286, 1.443375672974076540 ) ) ;
#55172 = CARTESIAN_POINT ( 'NONE',  ( 3.467590214127397541, -0.3886977184213887271, 1.930520482988388631 ) ) ;
#55173 = CARTESIAN_POINT ( 'NONE',  ( 5.062125140741547291, -1.117816439015427044, 1.678017345901124058 ) ) ;
#55174 = CARTESIAN_POINT ( 'NONE',  ( -6.235860587281615075, 9.362588887548838557, -1.199719254218440723 ) ) ;
#55175 = FACE_OUTER_BOUND ( 'NONE', #104521, .T. ) ;
#55176 = CARTESIAN_POINT ( 'NONE',  ( 5.261759291836726860, 1.077959533075742993, 1.907929976554381124 ) ) ;
#55177 = CARTESIAN_POINT ( 'NONE',  ( 3.946537740505224878, 2.817530495244566335, 0.7750000000000135669 ) ) ;
#55178 = CARTESIAN_POINT ( 'NONE',  ( 3.645458630373909159, -1.458056112162182893, -1.259071146193297075 ) ) ;
#55179 = CARTESIAN_POINT ( 'NONE',  ( -7.802881099864745984, 9.062115023719057305, -1.199719254218446718 ) ) ;
#55180 = CARTESIAN_POINT ( 'NONE',  ( -0.1294898018152201291, 4.092224548688067287, -2.481517387982924649 ) ) ;
#55181 = CARTESIAN_POINT ( 'NONE',  ( 0.1709339574563934483, -1.438030690398562239, 1.674123062825278563 ) ) ;
#55182 = CARTESIAN_POINT ( 'NONE',  ( -0.9015567080380649800, 15.51893790258581518, -11.97447543335910503 ) ) ;
#55183 = CARTESIAN_POINT ( 'NONE',  ( -8.784717086998243829, 14.48107293590954825, 8.187136581970905880 ) ) ;
#55184 = VERTEX_POINT ( 'NONE', #161087 ) ;
#55185 = CARTESIAN_POINT ( 'NONE',  ( 5.587368702607580673, 5.691220705896524734, -0.7216878364870458196 ) ) ;
#55186 = CARTESIAN_POINT ( 'NONE',  ( 4.680490344776488065, 1.214988973509235848, -1.549875580164503663 ) ) ;
#55188 = CARTESIAN_POINT ( 'NONE',  ( 4.406893533441514244, -0.4431801161997659944, -1.963548474556547685 ) ) ;
#55187 = CARTESIAN_POINT ( 'NONE',  ( -0.04160512940111232155, -1.735061556407999417, -0.8725848562033207134 ) ) ;
#55189 = CARTESIAN_POINT ( 'NONE',  ( 5.905696578591778767, 0.4397782949263558949, 2.255800006528754675 ) ) ;
#55191 = CARTESIAN_POINT ( 'NONE',  ( 3.696024482597393135, 0.8403398683093143973, -1.660512506883378370 ) ) ;
#55190 =( LENGTH_UNIT ( ) NAMED_UNIT ( * ) SI_UNIT ( .MILLI., .METRE. ) );
#55193 = CARTESIAN_POINT ( 'NONE',  ( 5.203297092594585393, 9.292540051327542017, 0.7998128361456341429 ) ) ;
#55192 = ADVANCED_BREP_SHAPE_REPRESENTATION ( '', ( #19216, #200407 ), #152191 ) ;
#55194 = DIRECTION ( 'NONE',  ( 0.000000000000000000, 0.000000000000000000, -1.000000000000000000 ) ) ;
#55195 = CARTESIAN_POINT ( 'NONE',  ( -7.393273838153706201, 7.519907654134449615, 0.7998128361456341429 ) ) ;
#55196 = CARTESIAN_POINT ( 'NONE',  ( -4.828112100242294424, 5.765790550771681566, -1.082531754730549967 ) ) ;
#55197 = CARTESIAN_POINT ( 'NONE',  ( 6.005435553056907239, -2.074886976054179488, 0.2565860541952763585 ) ) ;
#55198 = CARTESIAN_POINT ( 'NONE',  ( 4.189106276942576201, 7.831115056500907556, 1.040834085586084257E-14 ) ) ;
#55199 = EDGE_LOOP ( 'NONE', ( #187167, #13871, #69767, #64564 ) ) ;
#55200 = ADVANCED_FACE ( 'NONE', ( #176279 ), #77693, .F. ) ;
#55201 = CARTESIAN_POINT ( 'NONE',  ( -0.05544532671888474651, 6.488672696939749684, 3.101758036159037335 ) ) ;
#55202 = CARTESIAN_POINT ( 'NONE',  ( -1.500000000000038636, 7.750000000000000000, -10.64483442802187341 ) ) ;
#55203 = CARTESIAN_POINT ( 'NONE',  ( 1.013953575274041619, -0.8186894766500467657, -1.631917417583013341 ) ) ;
#55204 = CARTESIAN_POINT ( 'NONE',  ( -5.870844209917351009, 6.808071985447069707, -1.199719254218446718 ) ) ;
#55205 = CARTESIAN_POINT ( 'NONE',  ( 2.935853622122220674, -1.419245300609776272, -0.9961633832534546595 ) ) ;
#55206 = CARTESIAN_POINT ( 'NONE',  ( -0.1216878429548682999, 3.463015919485879834, -1.996294584693599994 ) ) ;
#55207 = CARTESIAN_POINT ( 'NONE',  ( -6.082770849258695378, 6.030316128467411829, -0.4441228188259391252 ) ) ;
#55208 = CARTESIAN_POINT ( 'NONE',  ( -5.585069213825653023, 8.603332285183535433, -1.199719254218440723 ) ) ;
#55209 = CARTESIAN_POINT ( 'NONE',  ( -5.815587556173210437, 6.058072081512762885, -0.5160206335057929694 ) ) ;
#55210 = CARTESIAN_POINT ( 'NONE',  ( 6.702019227905350540, 0.8390156466466727192, -2.002601388009570549 ) ) ;
#55211 = CARTESIAN_POINT ( 'NONE',  ( 5.707590141996651489, -0.4392596013848491521, 1.771934311310577659 ) ) ;
#55212 = CARTESIAN_POINT ( 'NONE',  ( 3.432423435979839343, -1.172226468724973936, 1.572839002276872566 ) ) ;
#55213 = CARTESIAN_POINT ( 'NONE',  ( 0.6124999999999550804, -0.02083333265050224536, -1.060881119635993519 ) ) ;
#55214 = CARTESIAN_POINT ( 'NONE',  ( -7.804689982961090955, 12.25722208009664094, 0.7998128361456481317 ) ) ;
#55215 = CARTESIAN_POINT ( 'NONE',  ( 8.098297826064319693, 8.342435640030188893, 0.7998128361456481317 ) ) ;
#55216 = VECTOR ( 'NONE', #96504, 1000.000000000000000 ) ;
#55217 = CARTESIAN_POINT ( 'NONE',  ( 4.072980787186268437, -1.570383936966279981, 1.425070900414181052 ) ) ;
#55218 = CARTESIAN_POINT ( 'NONE',  ( 7.126746022638799971, 8.343567110280638133, 1.199719254218452047 ) ) ;
#55219 = CARTESIAN_POINT ( 'NONE',  ( -9.001723924469462901, 12.58942944760136484, -1.199719254218446718 ) ) ;
#55220 = CARTESIAN_POINT ( 'NONE',  ( 1.252880909328604186, -0.4992908342843911940, -2.009044966204868388 ) ) ;
#55221 = CARTESIAN_POINT ( 'NONE',  ( -1.402160292154681736E-14, 14.59375000068279249, 1.732050807568881190 ) ) ;
#55223 = ORIENTED_EDGE ( 'NONE', *, *, #123377, .T. ) ;
#55222 = CARTESIAN_POINT ( 'NONE',  ( 4.864059028628820336, 0.6975124644323873468, -2.109029365712757897 ) ) ;
#55224 = CARTESIAN_POINT ( 'NONE',  ( 2.286107107991880216, 1.843941258665306115, -1.372366127498450883 ) ) ;
#55226 = CARTESIAN_POINT ( 'NONE',  ( 0.4616703453074429975, -0.5288386019042885522, 1.889040479230045255 ) ) ;
#55225 = CARTESIAN_POINT ( 'NONE',  ( 10.23604278863759909, 11.04439746293979496, 0.000000000000000000 ) ) ;
#55228 = CARTESIAN_POINT ( 'NONE',  ( -1.642778471874998480, -3.551041666188709645, 2.845375778867863303 ) ) ;
#55227 = CARTESIAN_POINT ( 'NONE',  ( 3.390420931869152721, 6.113185632892752075, -1.199719254218452047 ) ) ;
#55229 = CARTESIAN_POINT ( 'NONE',  ( 0.000000000000000000, 13.49999999999999822, 0.000000000000000000 ) ) ;
#55230 = CARTESIAN_POINT ( 'NONE',  ( 4.161989969715272686, 4.726297878971393196, 2.500000000000011102 ) ) ;
#55231 = CARTESIAN_POINT ( 'NONE',  ( -10.91804383151481339, -8.407420853759283830, 0.1905751639681794174 ) ) ;
#55232 = EDGE_CURVE ( 'NONE', #8253, #147564, #32148, .T. ) ;
#55233 = CARTESIAN_POINT ( 'NONE',  ( 2.988426722125224977, -1.135634098421594240, 1.538566774472991616 ) ) ;
#55234 = CARTESIAN_POINT ( 'NONE',  ( -0.5973881975621483376, 6.735339005392440903, -3.613785340523188339 ) ) ;
#55235 = CARTESIAN_POINT ( 'NONE',  ( 4.366008003732903653, 0.8140541678068600184, 1.520548270592293028 ) ) ;
#55236 = CARTESIAN_POINT ( 'NONE',  ( 2.782435679340321322, -0.5899881929209308540, -1.928257399728677379 ) ) ;
#55237 = CARTESIAN_POINT ( 'NONE',  ( 4.307493173298723832, 1.414159744579394307, -1.812179591053430627 ) ) ;
#55238 = CARTESIAN_POINT ( 'NONE',  ( 3.778848203065594102, -2.179170165155080774, -0.6077416658978853636 ) ) ;
#55239 = CARTESIAN_POINT ( 'NONE',  ( 6.692010077984027916, -0.9030311967607449475, 1.901034507416640373 ) ) ;
#55240 = CARTESIAN_POINT ( 'NONE',  ( -4.665414256878287702, 8.457084043084382330, -0.7216878364870338292 ) ) ;
#55241 = ORIENTED_EDGE ( 'NONE', *, *, #177361, .T. ) ;
#55242 = CARTESIAN_POINT ( 'NONE',  ( 4.235448325177215700, -1.219352424245947253, -1.282881785660697771 ) ) ;
#55244 = CARTESIAN_POINT ( 'NONE',  ( 0.9203736287852108955, 1.361359823012283865, -1.844092865855660124 ) ) ;
#55243 = CARTESIAN_POINT ( 'NONE',  ( 7.550965208168244125, 7.774157262476569130, -0.7998128361456341429 ) ) ;
#55245 = CARTESIAN_POINT ( 'NONE',  ( 5.454971364017034752, 0.3553261626877933788, -1.806350769464920569 ) ) ;
#55246 = CARTESIAN_POINT ( 'NONE',  ( -4.406563619641430840, 5.099744630125142564, -1.199719254218446718 ) ) ;
#55247 = CARTESIAN_POINT ( 'NONE',  ( 5.753911783233988331, 0.8852683131516884130, 2.004867968450708915 ) ) ;
#55248 = CARTESIAN_POINT ( 'NONE',  ( -5.842637852846353397, 5.781108681267656202, 0.7998128361456281477 ) ) ;
#55249 = CARTESIAN_POINT ( 'NONE',  ( -4.081167932913447594, 4.720116328942494555, -1.199719254218452047 ) ) ;
#55250 = CARTESIAN_POINT ( 'NONE',  ( -3.505115903893319729, 15.47003409145715480, 11.48545873523604044 ) ) ;
#55251 = EDGE_CURVE ( 'NONE', #201520, #108645, #124635, .T. ) ;
#55252 = CARTESIAN_POINT ( 'NONE',  ( 5.477033855465498924, 1.911541192706748715, 0.7957256658025002594 ) ) ;
#55253 = CARTESIAN_POINT ( 'NONE',  ( 1.745327705122714956, 0.3399549603602426417, -1.987498286102694411 ) ) ;
#55254 = CARTESIAN_POINT ( 'NONE',  ( 1.364683531249988535, 5.655208333674751842, -0.7879004041258300672 ) ) ;
#55255 = CARTESIAN_POINT ( 'NONE',  ( 3.897031312914517098, 1.626875583419360005, -1.031562066982329329 ) ) ;
#55256 = CARTESIAN_POINT ( 'NONE',  ( 1.364683531249996529, 10.71354166700806942, 0.7879004041258405033 ) ) ;
#55257 = CARTESIAN_POINT ( 'NONE',  ( 0.7916362837351547110, -0.06200823681477837107, -2.220726283632424192 ) ) ;
#55259 = ORIENTED_EDGE ( 'NONE', *, *, #123827, .F. ) ;
#55258 = DIRECTION ( 'NONE',  ( -0.000000000000000000, 1.000000000000000000, -0.000000000000000000 ) ) ;
#55261 = FILL_AREA_STYLE_COLOUR ( '', #212363 ) ;
#55260 = CARTESIAN_POINT ( 'NONE',  ( 1.387358672530661030, 7.251968950356647348, -4.302625267142129672 ) ) ;
#55262 = CARTESIAN_POINT ( 'NONE',  ( 4.227444969362701421, 3.826440640544909400, 1.214306433183764966E-14 ) ) ;
#55263 = CARTESIAN_POINT ( 'NONE',  ( -4.586165880992542299, 5.350526861157986147, 2.420000000000010587 ) ) ;
#55264 = CARTESIAN_POINT ( 'NONE',  ( 1.886825320689233809, 2.480000000000016858, 2.459652456995882641 ) ) ;
#55265 = FACE_OUTER_BOUND ( 'NONE', #128906, .T. ) ;
#55266 = CARTESIAN_POINT ( 'NONE',  ( 2.945700582358207864, 1.385421296276163838, 1.389331660621349274 ) ) ;
#55268 = CARTESIAN_POINT ( 'NONE',  ( 1.364683531249988757, 2.196875000341415252, 1.214306433183764966E-14 ) ) ;
#55267 = CARTESIAN_POINT ( 'NONE',  ( 6.159481859310094620, 6.080483678816896109, 1.040834085586084257E-14 ) ) ;
#55269 = CARTESIAN_POINT ( 'NONE',  ( -1.811274280335455122, -3.247629826974540057E-15, 0.2936757779752607878 ) ) ;
#55270 = CARTESIAN_POINT ( 'NONE',  ( 0.2563952634283462872, -2.062181505987520147, -0.05231737696831904177 ) ) ;
#55271 = CARTESIAN_POINT ( 'NONE',  ( -7.808606406466886973, 11.19745900993164511, 1.199719254218453823 ) ) ;
#55272 = CARTESIAN_POINT ( 'NONE',  ( -4.785665035499573783, 5.645992631913323123, 1.082531754730558626 ) ) ;
#55273 = CARTESIAN_POINT ( 'NONE',  ( 0.4095021115802527922, 1.970281763946807541, 1.112102026807944677 ) ) ;
#55275 = ORIENTED_EDGE ( 'NONE', *, *, #178012, .F. ) ;
#55274 = CARTESIAN_POINT ( 'NONE',  ( -5.259673527097670664, 8.223703984000886535, -1.199719254218446718 ) ) ;
#55276 = CARTESIAN_POINT ( 'NONE',  ( 1.364683531249988535, 5.655208333674751842, -0.7879004041258300672 ) ) ;
#55277 = CARTESIAN_POINT ( 'NONE',  ( 1.176777557245082262, -0.04011917365428705612, -1.870279424122413658 ) ) ;
#55278 = CARTESIAN_POINT ( 'NONE',  ( 6.872404467231180369, -0.3655807773644218495, 1.700417682701503841 ) ) ;
#55279 = EDGE_CURVE ( 'NONE', #11451, #150638, #47365, .T. ) ;
#55281 = CARTESIAN_POINT ( 'NONE',  ( 4.739868811304373430, 2.185674081084403753, 0.1610935195608814985 ) ) ;
#55280 = CARTESIAN_POINT ( 'NONE',  ( -2.353626204688216217E-14, 2.453125000341405570, 1.570758158831792262 ) ) ;
#55282 = CARTESIAN_POINT ( 'NONE',  ( 5.631924041214952936, -1.458266564992457104, -1.788428398515107043 ) ) ;
#55283 = CARTESIAN_POINT ( 'NONE',  ( 6.731718603199120743, -1.342629487124985532, -1.563498854789405534 ) ) ;
#55284 = CARTESIAN_POINT ( 'NONE',  ( 2.009616874778739071, -0.9155987108000520625, -1.712560621339030309 ) ) ;
#55285 = CARTESIAN_POINT ( 'NONE',  ( -4.677199806590235376, 7.440188293455128665, 1.082531754730560403 ) ) ;
#55286 = EDGE_CURVE ( 'NONE', #45686, #133641, #146497, .T. ) ;
#55287 = CARTESIAN_POINT ( 'NONE',  ( 4.095971805104285934, 6.832365301713403838, 1.082531754730549078 ) ) ;
#55288 = CARTESIAN_POINT ( 'NONE',  ( -1.360316468749999119, 0.3906250003414130090, -8.673617379884035472E-15 ) ) ;
#55289 = CARTESIAN_POINT ( 'NONE',  ( 3.252577435111691617, 1.966644794889659043, -0.4445022851852917234 ) ) ;
#55290 = CARTESIAN_POINT ( 'NONE',  ( -3.592547517496935683, 6.174760622846296343, -1.082531754730548412 ) ) ;
#55291 = CARTESIAN_POINT ( 'NONE',  ( -7.293360289508603600, 7.473618190706972086, 0.000000000000000000 ) ) ;
#55292 = DIRECTION ( 'NONE',  ( 0.04888523518676889112, 8.339466111204228823E-16, 0.9988044021632737079 ) ) ;
#55294 = CARTESIAN_POINT ( 'NONE',  ( 7.968353659517096510, -5.197284395437338667, -7.583532603600771083 ) ) ;
#55293 = CARTESIAN_POINT ( 'NONE',  ( 0.8733498553583609603, 1.760202786292342170, -0.4843115980177821744 ) ) ;
#55295 = CARTESIAN_POINT ( 'NONE',  ( -3.637330350216213759, 7.465578851886037093, -0.7998128361456481317 ) ) ;
#55296 = DIRECTION ( 'NONE',  ( -0.000000000000000000, -1.000000000000000000, -0.000000000000000000 ) ) ;
#55297 = CARTESIAN_POINT ( 'NONE',  ( -10.73969341588288628, 4.108126672274917013, 4.807887712954548753 ) ) ;
#55298 = VERTEX_POINT ( 'NONE', #201009 ) ;
#55299 = CARTESIAN_POINT ( 'NONE',  ( 6.614142728931415860, -0.9689641062460941923, -1.818880834187324824 ) ) ;
#55300 = CARTESIAN_POINT ( 'NONE',  ( -7.905812970100109638, 8.396072351304486148, 0.7216878364870317197 ) ) ;
#55301 = UNCERTAINTY_MEASURE_WITH_UNIT (LENGTH_MEASURE( 1.000000000000000082E-05 ), #165748, 'distance_accuracy_value', 'NONE');
#55302 = CARTESIAN_POINT ( 'NONE',  ( -3.277320446201389181, 4.846626492033466072, 1.599625672291267398 ) ) ;
#55303 = CARTESIAN_POINT ( 'NONE',  ( -10.64723070543352712, 11.31619066596094392, 0.7998128361456462443 ) ) ;
#55304 = CARTESIAN_POINT ( 'NONE',  ( 5.268225494782738494, 2.017278875131154336, -0.1011536798302767465 ) ) ;
#55306 = ORIENTED_EDGE ( 'NONE', *, *, #42375, .T. ) ;
#55305 = CARTESIAN_POINT ( 'NONE',  ( 5.373765183877965868, 0.4349513647441177744, -2.178143251680577208 ) ) ;
#55307 = CARTESIAN_POINT ( 'NONE',  ( -5.327428015527048366, 5.180030537728460338, -0.7998128361456362523 ) ) ;
#55308 = CARTESIAN_POINT ( 'NONE',  ( 6.979750152936881058, 7.037463354714830643, 0.7998128361456341429 ) ) ;
#55309 =( GEOMETRIC_REPRESENTATION_CONTEXT ( 3 ) GLOBAL_UNCERTAINTY_ASSIGNED_CONTEXT ( ( #129681 ) ) GLOBAL_UNIT_ASSIGNED_CONTEXT ( ( #107100, #142776, #123384 ) ) REPRESENTATION_CONTEXT ( 'NONE', 'WORKASPACE' ) );
#55310 = CARTESIAN_POINT ( 'NONE',  ( 5.664934882792908688, -1.862169278537370465, -0.8832596265169431193 ) ) ;
#55311 = CARTESIAN_POINT ( 'NONE',  ( 4.518204034511161815, -1.842447959940773705, 0.8197716922626956393 ) ) ;
#55312 = EDGE_LOOP ( 'NONE', ( #19136, #133945, #154951, #81296, #20354, #25235, #31625, #75932 ) ) ;
#55313 = SURFACE_STYLE_USAGE ( .BOTH. , #190621 ) ;
#55314 = CARTESIAN_POINT ( 'NONE',  ( 2.517010073631369860, 6.088262185878572375, -0.7998128361456281477 ) ) ;
#55315 = CARTESIAN_POINT ( 'NONE',  ( -8.120407659942227241, 8.438506789546210030, 0.7998128361456341429 ) ) ;
#55316 = CARTESIAN_POINT ( 'NONE',  ( 4.708029738644283313, 8.352945002179891887, -0.6661931671527853149 ) ) ;
#55317 = CARTESIAN_POINT ( 'NONE',  ( 4.112657547701242144, 0.6818919214185631406, -1.897407125352356339 ) ) ;
#55318 = CARTESIAN_POINT ( 'NONE',  ( 3.152128525617302834, -1.393660036906883226, 1.203213496783587910 ) ) ;
#55319 = DIRECTION ( 'NONE',  ( 0.000000000000000000, -1.000000000000000000, 0.000000000000000000 ) ) ;
#55320 = CARTESIAN_POINT ( 'NONE',  ( 1.946342613620454243, 0.8805590942474375016, -2.133279852835685109 ) ) ;
#55321 = CARTESIAN_POINT ( 'NONE',  ( 3.061108821635398769, 6.793320401875094561, -0.7998128361456362523 ) ) ;
#55322 = CARTESIAN_POINT ( 'NONE',  ( 3.884175197147401892, -1.069116497136082700, 1.878640351225938421 ) ) ;
#55323 = CARTESIAN_POINT ( 'NONE',  ( 7.853197290813620945, 10.18514947741448573, 1.599625672291281386 ) ) ;
#55324 = CARTESIAN_POINT ( 'NONE',  ( -4.761938266897808525, 6.578680616179308771, 1.599625672291267398 ) ) ;
#55325 = CIRCLE ( 'NONE', #131441, 6.200000000000000178 ) ;
#55326 = CARTESIAN_POINT ( 'NONE',  ( 3.321888608656462072, -1.742702400767569992, 1.498638621658739511 ) ) ;
#55327 = CARTESIAN_POINT ( 'NONE',  ( 3.834746474454188013E-15, 12.84375000068279782, 1.500000000000001554 ) ) ;
#55328 = CARTESIAN_POINT ( 'NONE',  ( 2.307302758404996545, -0.4121581357655336175, 1.824517092411604979 ) ) ;
#55329 = CARTESIAN_POINT ( 'NONE',  ( 6.455938704688762186, 1.966190342143339764, -0.1448359745850023028 ) ) ;
#55331 = CARTESIAN_POINT ( 'NONE',  ( -7.045397100956844127, 8.248660034984974132, -1.199719254218452047 ) ) ;
#55330 = CARTESIAN_POINT ( 'NONE',  ( 1.364683531249988535, 4.405208333674754506, -0.7879004041258300672 ) ) ;
#55332 = CARTESIAN_POINT ( 'NONE',  ( 1.717678464306471309, -0.2677704892378242607, 2.190511422692428045 ) ) ;
#55333 = ORIENTED_EDGE ( 'NONE', *, *, #69490, .T. ) ;
#55334 = CARTESIAN_POINT ( 'NONE',  ( 5.217190183160311356, 4.981143389975473568, -0.7998128361456211532 ) ) ;
#55335 = CARTESIAN_POINT ( 'NONE',  ( -3.086452525405351643, 6.752611712948207057, 0.7998128361456341429 ) ) ;
#55336 = CARTESIAN_POINT ( 'NONE',  ( -7.836017471263608591, -5.361065518611685121, 7.720011280421910094 ) ) ;
#55337 = CARTESIAN_POINT ( 'NONE',  ( 5.928588038458690868, 1.899881307248694418, 0.5261610973047344819 ) ) ;
#55338 = CARTESIAN_POINT ( 'NONE',  ( 5.584705890799654071, -2.250326009109602232, -0.5107660753775817852 ) ) ;
#55339 = CARTESIAN_POINT ( 'NONE',  ( 6.848144937404742727, -0.7948834574948275833, 1.681425573653466676 ) ) ;
#55340 = CARTESIAN_POINT ( 'NONE',  ( 4.223522562419862680, 0.2575905095270197287, -2.046390306194557418 ) ) ;
#55341 = CARTESIAN_POINT ( 'NONE',  ( 6.995644074971448134, 7.263932296995902149, -0.7216878364870257245 ) ) ;
#55342 = CARTESIAN_POINT ( 'NONE',  ( 5.083381250481017410, 4.895309311841474553, 0.7998128361456352531 ) ) ;
#55343 = CARTESIAN_POINT ( 'NONE',  ( 7.632877294369377452, 8.967740267261513409, -1.082531754730537976 ) ) ;
#55344 = CARTESIAN_POINT ( 'NONE',  ( -1.201851678989727383E-14, 3.759375000341422801, -1.575800808251660134 ) ) ;
#55345 = CARTESIAN_POINT ( 'NONE',  ( -9.756440972247897747, 3.530925782592636342, -6.991133065687681558 ) ) ;
#55346 = CARTESIAN_POINT ( 'NONE',  ( 4.650083499362867911, 6.448183387388563226, 1.443375672974062551 ) ) ;
#55347 = CARTESIAN_POINT ( 'NONE',  ( 6.619587810436369679, 0.3779085275587866777, -2.137903583376862038 ) ) ;
#55349 = CARTESIAN_POINT ( 'NONE',  ( 5.038538826285253514, -1.576363729006284187, 0.9512496309353533075 ) ) ;
#55348 = CARTESIAN_POINT ( 'NONE',  ( 6.539320575229250920, 0.004279804010676861205, 1.996977849922921155 ) ) ;
#55350 = EDGE_CURVE ( 'NONE', #191870, #77536, #104892, .T. ) ;
#55351 = CARTESIAN_POINT ( 'NONE',  ( 6.620655732516652847, 2.468432086671234149, 2.210906647470804565 ) ) ;
#55352 = CARTESIAN_POINT ( 'NONE',  ( 1.898855744251417788, 3.739179606816488199, 0.3999999999999848677 ) ) ;
#55353 = DIRECTION ( 'NONE',  ( 0.000000000000000000, 1.000000000000000000, 0.000000000000000000 ) ) ;
#55354 = CARTESIAN_POINT ( 'NONE',  ( -4.153558989372251986, 7.618438364782146976, 0.8772435784342603737 ) ) ;
#55355 = CARTESIAN_POINT ( 'NONE',  ( 0.1443076407905200254, 2.614873645970688276, 2.074999080605917090 ) ) ;
#55356 = CARTESIAN_POINT ( 'NONE',  ( 5.720439131930858956, 7.397432110343761025, 1.315134405782365956 ) ) ;
#55357 = CARTESIAN_POINT ( 'NONE',  ( 0.5219363917940004205, -1.903054291476031112, 0.1877445768119419822 ) ) ;
#55359 = EDGE_CURVE ( 'NONE', #112763, #40935, #163645, .T. ) ;
#55358 = CARTESIAN_POINT ( 'NONE',  ( 2.254462534575492949, -1.370001101035130509, 1.120467526443365891 ) ) ;
#55360 = CARTESIAN_POINT ( 'NONE',  ( 6.498696042004469930, -1.974701156420979542, -0.3904368389309967324 ) ) ;
#55362 = CARTESIAN_POINT ( 'NONE',  ( 3.901880894453650050, -0.9877729052028583201, -1.641157072818617779 ) ) ;
#55361 = CARTESIAN_POINT ( 'NONE',  ( -9.504429378379839477, 11.04725468198666150, 1.199719254218462483 ) ) ;
#55363 = CARTESIAN_POINT ( 'NONE',  ( -2.193105066167322370, 5.702484939155337607, -2.420000000000000373 ) ) ;
#55364 = CARTESIAN_POINT ( 'NONE',  ( 5.441845355777640059, 1.321472782793672085, 1.460616519443626249 ) ) ;
#55365 = CARTESIAN_POINT ( 'NONE',  ( 6.433853624855537134, -1.958103210868083810, 0.4948410764434567066 ) ) ;
#55366 = CARTESIAN_POINT ( 'NONE',  ( 0.7941172694243576746, -3.057670337906326807, 3.391178412236372175 ) ) ;
#55367 = CARTESIAN_POINT ( 'NONE',  ( 2.992876365407059147, 1.605230647100181596, -0.9602576221170722182 ) ) ;
#55369 = ORIENTED_EDGE ( 'NONE', *, *, #93908, .F. ) ;
#55368 = CARTESIAN_POINT ( 'NONE',  ( 6.586556832619708146, -1.693200007625778492, -0.3281344310326217428 ) ) ;
#55371 = CARTESIAN_POINT ( 'NONE',  ( 2.724825686666657809, 6.122787701178987518, 0.000000000000000000 ) ) ;
#55370 = CARTESIAN_POINT ( 'NONE',  ( 2.051678093609669240, -1.773579625386853875, -1.313098587465796774 ) ) ;
#55372 = CARTESIAN_POINT ( 'NONE',  ( -1.201851678989727383E-14, 4.009375000341416140, -1.575800808251660134 ) ) ;
#55373 = CARTESIAN_POINT ( 'NONE',  ( 0.2388349330707796314, -2.000390574439359526, -0.5026286349697464129 ) ) ;
#55374 = CARTESIAN_POINT ( 'NONE',  ( 6.588372581236919601, 9.773852880496709972, -1.199719254218440723 ) ) ;
#55375 = CARTESIAN_POINT ( 'NONE',  ( -10.66756793585402363, 11.33991743478486391, 0.7998128361456462443 ) ) ;
#55376 = CARTESIAN_POINT ( 'NONE',  ( -1.734723475976807094E-15, 4.000007913748543587, -12.17999999982603399 ) ) ;
#55377 = CARTESIAN_POINT ( 'NONE',  ( -3.066115294984855133, 6.728884944124295053, 0.7998128361456341429 ) ) ;
#55378 = CARTESIAN_POINT ( 'NONE',  ( 0.000000000000000000, 2.800000000000024691, -2.499999999999995115 ) ) ;
#55379 = VERTEX_POINT ( 'NONE', #198878 ) ;
#55380 = CARTESIAN_POINT ( 'NONE',  ( 2.752462066230080495, -2.064650614848703825, -0.1547973748374023295 ) ) ;
#55381 = CARTESIAN_POINT ( 'NONE',  ( -1.001543065824772872E-14, 4.712500000000017231, 1.732050807568877637 ) ) ;
#55382 = CARTESIAN_POINT ( 'NONE',  ( 4.527533231959700366, 7.369540306339926516, 1.199719254218462483 ) ) ;
#55383 = CARTESIAN_POINT ( 'NONE',  ( -6.212075186202199006, 7.030024481103895440, 1.038766164041710738 ) ) ;
#55384 = CARTESIAN_POINT ( 'NONE',  ( 0.5221358870723510348, -2.009748826802790322, 0.2000887155638417791 ) ) ;
#55385 = CARTESIAN_POINT ( 'NONE',  ( -1.364683531250012516, 3.280208333674756727, 0.7879004041258379498 ) ) ;
#55386 = VERTEX_POINT ( 'NONE', #17997 ) ;
#55388 = CARTESIAN_POINT ( 'NONE',  ( 8.432808358020015049, 11.82173160345663376, 1.082531754730546636 ) ) ;
#55387 = CARTESIAN_POINT ( 'NONE',  ( 0.07459516483346911864, 0.7642615113957001993, -1.841455071455591064 ) ) ;
#55389 = CARTESIAN_POINT ( 'NONE',  ( 6.011092252151500226, 2.013677719867816851, 0.1017325769363253418 ) ) ;
#55390 = CARTESIAN_POINT ( 'NONE',  ( 5.647645028696767433, 1.886156043628923529, -0.3343808708002778407 ) ) ;
#55391 = FACE_BOUND ( 'NONE', #179032, .T. ) ;
#55392 = CARTESIAN_POINT ( 'NONE',  ( 3.720431430916489646, 2.081484170424623859, 0.6860852429351402826 ) ) ;
#55393 = CARTESIAN_POINT ( 'NONE',  ( -1.500000000000013101, 2.202083334016153859, 0.8660254037844403729 ) ) ;
#55394 = CARTESIAN_POINT ( 'NONE',  ( 2.707167837304753633, 1.638089068140319071, -0.9866689735503200165 ) ) ;
#55395 = CARTESIAN_POINT ( 'NONE',  ( -6.566226467720086113, 6.555019055295208119, 1.040834085586084257E-14 ) ) ;
#55396 = CARTESIAN_POINT ( 'NONE',  ( 5.639828713160493834, 5.682147708216442439, 1.040834085586084257E-14 ) ) ;
#55398 = CARTESIAN_POINT ( 'NONE',  ( 1.493767781312784981, -2.000855510370867840, 0.2496291452861176263 ) ) ;
#55397 = CARTESIAN_POINT ( 'NONE',  ( 1.727399429735891272E-15, 14.67582449756711149, 11.75119994318007421 ) ) ;
#55399 = CARTESIAN_POINT ( 'NONE',  ( -1.402160292154681736E-14, 10.98437500034139802, 1.575800808251682339 ) ) ;
#55401 = CARTESIAN_POINT ( 'NONE',  ( -5.498713818794216834, 8.572860667638675380, -1.199719254218452047 ) ) ;
#55400 = CARTESIAN_POINT ( 'NONE',  ( 6.163654587501778970, 1.125051486859941718, 1.880622087419632882 ) ) ;
#55403 = ORIENTED_EDGE ( 'NONE', *, *, #94862, .F. ) ;
#55402 = CARTESIAN_POINT ( 'NONE',  ( 3.153030191819999217, -1.409141575680799230, -0.9942448187586181430 ) ) ;
#55404 = CARTESIAN_POINT ( 'NONE',  ( -0.1405533004718754753, 0.003749010675345095921, -1.720146753850452681 ) ) ;
#55405 = CARTESIAN_POINT ( 'NONE',  ( 6.662942426112080874, 9.860851032851066122, 1.199719254218460707 ) ) ;
#55406 = CARTESIAN_POINT ( 'NONE',  ( 4.985647801523278133, 6.839675073242382553, -1.599625672291256295 ) ) ;
#55407 = ADVANCED_FACE ( 'NONE', ( #50525 ), #122286, .T. ) ;
#55408 = CARTESIAN_POINT ( 'NONE',  ( 0.000000000000000000, -0.9841229182759280159, 0.000000000000000000 ) ) ;
#55409 = CARTESIAN_POINT ( 'NONE',  ( 0.3616705494772323726, -0.5269360983083425376, 1.889693748445469224 ) ) ;
#55410 = CARTESIAN_POINT ( 'NONE',  ( 4.469384193999260901, 8.366031992974468423, -0.7998128361456231517 ) ) ;
#55411 = CARTESIAN_POINT ( 'NONE',  ( 0.07536363704235479744, 6.947016338497881804, -2.739277465201896078 ) ) ;
#55412 = ORIENTED_EDGE ( 'NONE', *, *, #208932, .T. ) ;
#55413 = CARTESIAN_POINT ( 'NONE',  ( -1.284279953904152949, 3.171639714193937198, 0.7750000000000152323 ) ) ;
#55414 = VERTEX_POINT ( 'NONE', #97173 ) ;
#55415 = CARTESIAN_POINT ( 'NONE',  ( 3.615680081246709143, -0.5227945197113766929, 1.734396599632443525 ) ) ;
#55416 = ORIENTED_EDGE ( 'NONE', *, *, #68201, .T. ) ;
#55417 = CARTESIAN_POINT ( 'NONE',  ( 8.041957671200231417, 12.53403438304231976, 1.040834085586084257E-14 ) ) ;
#55418 = CARTESIAN_POINT ( 'NONE',  ( 2.911969131885072670, 6.619324097166378706, 0.000000000000000000 ) ) ;
#55419 = CARTESIAN_POINT ( 'NONE',  ( 4.441949062027584993, -1.118158961774197380, -1.425077651336349227 ) ) ;
#55420 = CARTESIAN_POINT ( 'NONE',  ( 0.4153311931458959494, 3.850000000000006306, 0.5000000000000064393 ) ) ;
#55421 = CARTESIAN_POINT ( 'NONE',  ( 1.526556658859590243E-16, 2.000000000000001776, -2.750000000000008438 ) ) ;
#55422 = CARTESIAN_POINT ( 'NONE',  ( 5.757945239960298167, 6.059206896687658883, 0.6045188873357760784 ) ) ;
#55423 = EDGE_CURVE ( 'NONE', #32719, #153422, #69447, .T. ) ;
#55425 = CARTESIAN_POINT ( 'NONE',  ( 1.364683531249996529, 13.96354166700806765, 0.7879004041258405033 ) ) ;
#55424 = CARTESIAN_POINT ( 'NONE',  ( 5.494539847903294749, 1.833519193728103014, 0.3179774322314922741 ) ) ;
#55426 = EDGE_CURVE ( 'NONE', #185672, #57833, #120784, .T. ) ;
#55427 = CARTESIAN_POINT ( 'NONE',  ( 2.935058904569508353, -1.567653816607515127, -1.100626458259999385 ) ) ;
#55428 = CARTESIAN_POINT ( 'NONE',  ( 4.668873160992260019, 8.281730553837055808, 0.5279080060728712498 ) ) ;
#55429 = CARTESIAN_POINT ( 'NONE',  ( -10.45911050446410506, 5.175404930453152197, 5.201426885097844455 ) ) ;
#55430 = DIRECTION ( 'NONE',  ( 0.000000000000000000, 0.000000000000000000, 1.000000000000000000 ) ) ;
#55431 = FACE_OUTER_BOUND ( 'NONE', #211433, .T. ) ;
#55432 = CARTESIAN_POINT ( 'NONE',  ( 6.127922243696800386, 10.09306701771420656, -0.7216878364870267237 ) ) ;
#55433 = CARTESIAN_POINT ( 'NONE',  ( -3.765413976293358278, 5.416068943807445635, 1.599625672291267398 ) ) ;
#55434 = DIRECTION ( 'NONE',  ( 1.276756478318932585E-15, -1.000000000000000000, 1.665334536937738262E-16 ) ) ;
#55435 = CARTESIAN_POINT ( 'NONE',  ( 1.412182186510477777, 1.403042805649477920, -1.550086674462275216 ) ) ;
#55436 = CARTESIAN_POINT ( 'NONE',  ( 6.150558962454855561, 7.204682206732687000, 1.199719254218452047 ) ) ;
#55437 = CARTESIAN_POINT ( 'NONE',  ( 6.809608091213839920, -0.4246860027747687560, 1.886121680295702596 ) ) ;
#55438 = CARTESIAN_POINT ( 'NONE',  ( -5.066996723205291708, 6.934582148538044777, 1.599625672291267398 ) ) ;
#55439 = CARTESIAN_POINT ( 'NONE',  ( 2.801551268311212262, -0.5745519774189576934, 1.732868645247707562 ) ) ;
#55440 = CARTESIAN_POINT ( 'NONE',  ( -4.226925616482887449, 3.500738074553344070, 2.444828727306146199 ) ) ;
#55441 = CARTESIAN_POINT ( 'NONE',  ( 2.021601768330282045, -0.4154675118966509317, 1.866563793090275203 ) ) ;
#55442 = CARTESIAN_POINT ( 'NONE',  ( 1.592182281804704003, 0.9734619808988297374, -1.712098776470400763 ) ) ;
#55443 = CARTESIAN_POINT ( 'NONE',  ( 3.192849282005063127, 1.532776493767808113, 1.192484549457759613 ) ) ;
#55444 = VERTEX_POINT ( 'NONE', #35325 ) ;
#55445 = CARTESIAN_POINT ( 'NONE',  ( -1.284279953904156280, 3.202889714876734573, 0.7750000000000117906 ) ) ;
#55447 = CARTESIAN_POINT ( 'NONE',  ( 6.807467476049567701, -1.494282888040651347, -1.108890849153229441 ) ) ;
#55446 = CARTESIAN_POINT ( 'NONE',  ( -4.899292406491858820, 6.809203455697518947, -1.599625672291271394 ) ) ;
#55449 = CARTESIAN_POINT ( 'NONE',  ( 3.902672080109194752, -2.098000727953463151, -0.3078000538283761078 ) ) ;
#55448 = CARTESIAN_POINT ( 'NONE',  ( 3.088225128862704949, 6.824956093640315302, 0.7998128361456281477 ) ) ;
#55450 = CARTESIAN_POINT ( 'NONE',  ( 6.761775799041450874, -7.009934032699937312, 6.672971353125840999 ) ) ;
#55451 = CARTESIAN_POINT ( 'NONE',  ( 8.062294901620731480, 12.55776115186623620, 1.040834085586084257E-14 ) ) ;
#55452 = CARTESIAN_POINT ( 'NONE',  ( -6.017840079619296567, 8.114175741012878973, -1.599625672291271394 ) ) ;
#55453 = CARTESIAN_POINT ( 'NONE',  ( 3.226477370372305753, 4.787309570232886280, 1.443375672974062551 ) ) ;
#55454 = VERTEX_POINT ( 'NONE', #6018 ) ;
#55455 = CARTESIAN_POINT ( 'NONE',  ( 7.361151057576892143, 7.552707420120024828, 0.7998128361456291469 ) ) ;
#55456 = DIRECTION ( 'NONE',  ( 0.000000000000000000, 0.000000000000000000, -1.000000000000000000 ) ) ;
#55457 = CARTESIAN_POINT ( 'NONE',  ( 4.195794211080963620, -0.6966935528937777677, 1.687730213881050600 ) ) ;
#55458 = CARTESIAN_POINT ( 'NONE',  ( -0.7500000000000179856, 13.07291666734946389, 1.299038105676658228 ) ) ;
#55459 = CARTESIAN_POINT ( 'NONE',  ( -9.978437869977959451, 10.74385839117019614, -0.7216878364870267237 ) ) ;
#55460 = CARTESIAN_POINT ( 'NONE',  ( -5.151759543144467379, 7.884679950488731492, 1.249873765817657079 ) ) ;
#55461 = CARTESIAN_POINT ( 'NONE',  ( 4.080641032480825103, 5.783833874167997102, -1.249999999999999334 ) ) ;
#55462 = CARTESIAN_POINT ( 'NONE',  ( 4.944154083221365070, 1.865701114312174225, 0.1370711555178441010 ) ) ;
#55463 = CARTESIAN_POINT ( 'NONE',  ( 8.751951852821344247, 10.16936423550178503, -1.199719254218446718 ) ) ;
#55464 = CARTESIAN_POINT ( 'NONE',  ( 2.016120517293042536, -0.9081000056256024466, -1.699051532819460197 ) ) ;
#55465 = CARTESIAN_POINT ( 'NONE',  ( 1.010509813927327416, 2.800000000000067768, 1.061904942541237462 ) ) ;
#55466 = CARTESIAN_POINT ( 'NONE',  ( -1.402160292154681736E-14, 8.484375000341403350, 1.575800808251682339 ) ) ;
#55467 = CARTESIAN_POINT ( 'NONE',  ( -5.228640796364566690, 9.251831362400652736, -0.7998128361456231517 ) ) ;
#55468 = CARTESIAN_POINT ( 'NONE',  ( 4.334856428067313416, 6.080418470877079429, -1.599625672291256295 ) ) ;
#55469 = CARTESIAN_POINT ( 'NONE',  ( -4.136646265500958819, 7.840188053144158786, -0.7216878364870458196 ) ) ;
#55470 =( BOUNDED_SURFACE ( )  B_SPLINE_SURFACE ( 3, 2, ( 
 ( #121609, #187579, #53321 ),
 ( #167084, #102074, #133545 ),
 ( #169202, #51197, #34921 ),
 ( #202745, #18675, #151900 ),
 ( #184373, #118385, #168140 ),
 ( #19741, #85821, #119454 ) ),
 .UNSPECIFIED., .F., .F., .T. ) 
 B_SPLINE_SURFACE_WITH_KNOTS ( ( 4, 2, 4 ),
 ( 3, 3 ),
 ( 0.000000000000000000, 0.0003754691837024766985, 0.0007509383674049533971 ),
 ( 0.000000000000000000, 1.000000000000000000 ),
 .UNSPECIFIED. ) 
 GEOMETRIC_REPRESENTATION_ITEM ( )  RATIONAL_B_SPLINE_SURFACE ( (
 ( 1.000000000000000000, 0.6711954675835395401, 1.000000000000000000),
 ( 1.000000000000000000, 0.6709646295267174265, 1.000000000000000000),
 ( 1.000000000000000000, 0.6771840716659688342, 1.000000000000000000),
 ( 1.000000000000000000, 0.6927481755866825575, 1.000000000000000000),
 ( 1.000000000000000000, 0.7017972101310403499, 1.000000000000000000),
 ( 1.000000000000000000, 0.7071067811865475727, 1.000000000000000000) ) ) 
 REPRESENTATION_ITEM ( '' )  SURFACE ( )  );
#55471 = CARTESIAN_POINT ( 'NONE',  ( 1.669685637109643794, 1.462710821638053105, 1.530943346549427320 ) ) ;
#55472 = CARTESIAN_POINT ( 'NONE',  ( 10.05353459973327368, 11.68787744023238417, -1.199719254218440723 ) ) ;
#55474 = ORIENTED_EDGE ( 'NONE', *, *, #165357, .F. ) ;
#55473 = CARTESIAN_POINT ( 'NONE',  ( -3.633221978782304351, 4.301475732409860697, -1.082531754730549967 ) ) ;
#55475 = CARTESIAN_POINT ( 'NONE',  ( 4.944224162298806569, -0.9806570695735459253, 1.823293813017504039 ) ) ;
#55477 = CARTESIAN_POINT ( 'NONE',  ( -1.364683531250012516, 2.342708333674752286, 0.7879004041258379498 ) ) ;
#55476 = CARTESIAN_POINT ( 'NONE',  ( 0.9777802892061361328, -1.796362506263927017, -0.4033719513514141264 ) ) ;
#55478 = ORIENTED_EDGE ( 'NONE', *, *, #12460, .F. ) ;
#55479 = CARTESIAN_POINT ( 'NONE',  ( 5.186298777384058312, 1.878100352198919465, 1.325219426413627000 ) ) ;
#55480 = CARTESIAN_POINT ( 'NONE',  ( 6.805829924380114804, 8.002851668940699881, 1.082531754730558626 ) ) ;
#55482 = DIRECTION ( 'NONE',  ( 1.000000000000000000, 0.000000000000000000, 0.000000000000000000 ) ) ;
#55481 = CARTESIAN_POINT ( 'NONE',  ( 5.587368702607580673, 5.691220705896524734, -0.7216878364870458196 ) ) ;
#55483 = CARTESIAN_POINT ( 'NONE',  ( 1.588225008415785844, -2.281566021618782081, -0.2212011980115625998 ) ) ;
#55484 = CARTESIAN_POINT ( 'NONE',  ( 0.000000000000000000, 11.37999999999999901, 0.000000000000000000 ) ) ;
#55485 = CARTESIAN_POINT ( 'NONE',  ( -6.237633190739009237, 9.434933268240943249, 1.199719254218452047 ) ) ;
#55486 = CARTESIAN_POINT ( 'NONE',  ( 4.945229674018920107, 0.6074099038847360355, -1.844580613826458437 ) ) ;
#55487 = ORIENTED_EDGE ( 'NONE', *, *, #648, .F. ) ;
#55488 = CARTESIAN_POINT ( 'NONE',  ( 6.765155463094740362, 10.83650577367847667, 0.7216878364870438212 ) ) ;
#55489 = EDGE_CURVE ( 'NONE', #195372, #24390, #73798, .T. ) ;
#55490 = ORIENTED_EDGE ( 'NONE', *, *, #122495, .T. ) ;
#55491 = CARTESIAN_POINT ( 'NONE',  ( 5.871340715825057011, -1.643613990083541143, -0.9773822251149253404 ) ) ;
#55492 = CARTESIAN_POINT ( 'NONE',  ( 5.137907791644652278, 2.014008302827663854, -0.1037760698975112861 ) ) ;
#55494 = CARTESIAN_POINT ( 'NONE',  ( -1.423205080756925867, 7.980384757729337863, -10.65537363484301636 ) ) ;
#55493 = CARTESIAN_POINT ( 'NONE',  ( -10.01677656239806247, 10.58066083241955901, 0.7998128361456462443 ) ) ;
#55495 = CARTESIAN_POINT ( 'NONE',  ( 1.642778471875000035, -1.363541666188707646, -2.845375778867859751 ) ) ;
#55497 = CARTESIAN_POINT ( 'NONE',  ( 0.8656337812406755816, 0.8672032905003168590, 1.542741919674812223 ) ) ;
#55496 = CARTESIAN_POINT ( 'NONE',  ( 3.292999148915674468, 1.648261854606505983, 1.285964787075925431 ) ) ;
#55498 = CARTESIAN_POINT ( 'NONE',  ( -0.2834499351972725179, -6.554910260573307390, -9.477100694337659448 ) ) ;
#55500 = CARTESIAN_POINT ( 'NONE',  ( 4.752058238528302780, 0.8743775744927633209, 2.119134945200305431 ) ) ;
#55499 = CARTESIAN_POINT ( 'NONE',  ( 5.259637247458703868, 5.100941308315409373, 0.000000000000000000 ) ) ;
#55501 = CARTESIAN_POINT ( 'NONE',  ( 2.185155941524752787, -0.7450687668543712894, 1.572906677108532936 ) ) ;
#55502 = CARTESIAN_POINT ( 'NONE',  ( 2.530568227245037605, 6.104080031761181857, 0.000000000000000000 ) ) ;
#55503 = CIRCLE ( 'NONE', #20992, 0.08000000000000020983 ) ;
#55504 = DIRECTION ( 'NONE',  ( 0.9667316390278627436, -0.2557927639760400607, 0.000000000000000000 ) ) ;
#55505 = CARTESIAN_POINT ( 'NONE',  ( 1.827078023146003760, -1.230200505038709036, 1.222094307470813934 ) ) ;
#55506 = CARTESIAN_POINT ( 'NONE',  ( 2.541674676231266083, 1.985806779098505448, -0.8781977400831306735 ) ) ;
#55507 = CARTESIAN_POINT ( 'NONE',  ( 5.606460214450851964, 6.499623990736163037, 1.199719254218462483 ) ) ;
#55508 = CARTESIAN_POINT ( 'NONE',  ( 4.065638850954083061, 1.320825628876612479, 1.523796413913918846 ) ) ;
#55509 = CARTESIAN_POINT ( 'NONE',  ( 3.218750000000001776, -0.7852924748298164559, 1.895863743164153847 ) ) ;
#55510 = CARTESIAN_POINT ( 'NONE',  ( -0.7500000000000215383, 3.472916667349487785, 1.299038105676671107 ) ) ;
#55511 = CARTESIAN_POINT ( 'NONE',  ( 0.6219390430294257088, -1.027834010343916749, -1.629101698904901863 ) ) ;
#55512 = CARTESIAN_POINT ( 'NONE',  ( -1.364683531250000748, 14.10937500034140157, 0.000000000000000000 ) ) ;
#55513 = CARTESIAN_POINT ( 'NONE',  ( 4.219114570843409240, 1.715941675311336123, -1.410698622648777434 ) ) ;
#55514 = ORIENTED_EDGE ( 'NONE', *, *, #71209, .F. ) ;
#55515 = CARTESIAN_POINT ( 'NONE',  ( 6.883263157960393563, 1.268976584491373183, 2.060807272249213451 ) ) ;
#55516 = CARTESIAN_POINT ( 'NONE',  ( 1.499999999999985123, 0.2958333333333566517, -0.8660254037844323793 ) ) ;
#55517 = CARTESIAN_POINT ( 'NONE',  ( 8.125414133291656071, 8.374071331795406081, -0.7998128361456291469 ) ) ;
#55518 = CARTESIAN_POINT ( 'NONE',  ( 4.785665035499516051, 8.527100274817353665, -0.7216878364870207285 ) ) ;
#55519 = CARTESIAN_POINT ( 'NONE',  ( -3.285556943750000514, -1.538541666188708357, -1.896917185911906722 ) ) ;
#55520 = CARTESIAN_POINT ( 'NONE',  ( 0.4873737393681918384, -2.093643541511390538, -0.7425801828774351021 ) ) ;
#55522 = CARTESIAN_POINT ( 'NONE',  ( 6.232861002365865488, -1.862453515449840724, -0.6167318247369477646 ) ) ;
#55521 = AXIS2_PLACEMENT_3D ( 'NONE', #109874, #45891, #46959 ) ;
#55523 = CARTESIAN_POINT ( 'NONE',  ( 9.490344339885973923, 12.09515436799890331, -1.443375672974057666 ) ) ;
#55524 = CARTESIAN_POINT ( 'NONE',  ( -1.390311220213877652, 4.148202468850559654, -0.5641062960582055030 ) ) ;
#55525 = CARTESIAN_POINT ( 'NONE',  ( 6.450461099754450700, 0.7004171410973459855, 2.151357330220986963 ) ) ;
#55526 = CARTESIAN_POINT ( 'NONE',  ( -4.773879485787619892, 7.623257595843924150, 1.082531754730549967 ) ) ;
#55527 = CARTESIAN_POINT ( 'NONE',  ( 3.086439574430835275, 1.148074821921121647, -1.713452782031915200 ) ) ;
#55528 = CARTESIAN_POINT ( 'NONE',  ( -6.175902666224832416, 7.163973517805802160, -1.199719254218446718 ) ) ;
#55529 = CARTESIAN_POINT ( 'NONE',  ( -0.7500000000000215383, 3.222916667349487341, 1.299038105676671107 ) ) ;
#55530 = CARTESIAN_POINT ( 'NONE',  ( -0.6823417656250212460, 5.113541667008086655, 1.181850606188767472 ) ) ;
#55531 = CARTESIAN_POINT ( 'NONE',  ( 4.745289220334846902, -1.444806058459674691, -1.188008360142885245 ) ) ;
#55532 = CARTESIAN_POINT ( 'NONE',  ( 4.060950141605116137, -0.9941625748171744048, 1.420652921118512602 ) ) ;
#55533 = CARTESIAN_POINT ( 'NONE',  ( 3.421201824283449877, -1.039729455425863147, -1.395559870880677789 ) ) ;
#55534 = EDGE_CURVE ( 'NONE', #183045, #202980, #66788, .T. ) ;
#55535 = CARTESIAN_POINT ( 'NONE',  ( 0.4160993436025617886, -1.233022138464324291, -1.932370275504050827 ) ) ;
#55536 = CARTESIAN_POINT ( 'NONE',  ( 0.6823417656249917140, 3.905208333674754950, 1.181850606188765695 ) ) ;
#55537 = CARTESIAN_POINT ( 'NONE',  ( 4.599217410553211316, -0.5561919879800735211, 2.015351296096360656 ) ) ;
#55538 = CARTESIAN_POINT ( 'NONE',  ( 6.474560584146490605, -0.09798994077552795889, -1.939597741719009338 ) ) ;
#55540 = VERTEX_POINT ( 'NONE', #153367 ) ;
#55539 = CARTESIAN_POINT ( 'NONE',  ( -11.33772463945037146, 13.39999999999998259, 3.599999999999999201 ) ) ;
#55541 =( NAMED_UNIT ( * ) SI_UNIT ( $, .STERADIAN. ) SOLID_ANGLE_UNIT ( ) );
#55542 = CARTESIAN_POINT ( 'NONE',  ( 0.2115648487451895210, 1.930418618556551946, 0.5826528611774861588 ) ) ;
#55543 = CARTESIAN_POINT ( 'NONE',  ( 0.7387272492362946252, 1.258454933865692293, -1.706699550108881080 ) ) ;
#55544 = DIRECTION ( 'NONE',  ( 0.000000000000000000, 1.000000000000000000, 0.000000000000000000 ) ) ;
#55545 = FACE_OUTER_BOUND ( 'NONE', #85232, .T. ) ;
#55546 = CARTESIAN_POINT ( 'NONE',  ( -6.367525699912501835, 10.58053041653993098, -0.7998128361456291469 ) ) ;
#55547 = CARTESIAN_POINT ( 'NONE',  ( 6.277588818327314080, 7.282607361925381717, 1.199719254218462483 ) ) ;
#55548 = CARTESIAN_POINT ( 'NONE',  ( 2.666775373343560407, 0.7166976873529753433, 1.995817185486338019 ) ) ;
#55549 = CARTESIAN_POINT ( 'NONE',  ( 0.5773502691896124084, -4.295408888568413630, -0.9999999999999991118 ) ) ;
#55551 = EDGE_CURVE ( 'NONE', #132973, #2109, #8061, .T. ) ;
#55550 = CARTESIAN_POINT ( 'NONE',  ( 4.266095019097836172, 0.8626762044917112293, 1.609013669381313294 ) ) ;
#55552 = VERTEX_POINT ( 'NONE', #57996 ) ;
#55553 = CARTESIAN_POINT ( 'NONE',  ( -3.811250578772981346, 6.500190537660166079, -1.082531754730546636 ) ) ;
#55554 = CARTESIAN_POINT ( 'NONE',  ( 0.000000000000000000, 19.00000000000000000, 0.000000000000000000 ) ) ;
#55555 = CARTESIAN_POINT ( 'NONE',  ( 3.285556943749998737, -0.6927083328553748087, -1.896917185911906500 ) ) ;
#55556 = CARTESIAN_POINT ( 'NONE',  ( -7.531718027591449705, 8.745758106066849891, 1.199719254218462483 ) ) ;
#55557 = CARTESIAN_POINT ( 'NONE',  ( 2.619404093423041591, 1.708565301817746018, 1.076861402434741821 ) ) ;
#55558 = CARTESIAN_POINT ( 'NONE',  ( 5.684669477433477169, -2.151827843693389308, -0.4886931181809702207 ) ) ;
#55559 = CARTESIAN_POINT ( 'NONE',  ( -4.447956913735107598, 7.346977611736363656, 1.199719254218452935 ) ) ;
#55560 = CARTESIAN_POINT ( 'NONE',  ( 3.414761196407948063, -1.412042937968212231, 1.212274210779472394 ) ) ;
#55561 = CARTESIAN_POINT ( 'NONE',  ( 3.216308754939877446, 4.775446185561722956, -1.599625672291262513 ) ) ;
#55562 = FACE_OUTER_BOUND ( 'NONE', #148433, .T. ) ;
#55563 = CARTESIAN_POINT ( 'NONE',  ( -4.334856428067329404, 6.080418470877079429, -1.599625672291256295 ) ) ;
#55564 =( BOUNDED_SURFACE ( )  B_SPLINE_SURFACE ( 3, 3, ( 
 ( #13814, #114599, #179541, #62570, #31161, #82019, #79886, #131887, #63648, #198945, #83076, #181642, #178474, #32213, #116713, #97234 ),
 ( #162227, #80959, #180590, #98287, #128733, #50589, #164348, #182713, #148109, #161155, #214112, #194707, #197895, #46347, #733, #65739 ),
 ( #49524, #115646, #30085, #33269, #99354, #17001, #149154, #6084, #85219, #200022, #117795, #151306, #104694, #136126, #86294, #102542 ),
 ( #204277, #2875, #5007, #51674, #137198, #38617, #35395, #68945, #101472, #36468, #118854, #183787, #185907, #21261, #168606, #100406 ),
 ( #52721, #1810, #72155, #122088, #55933, #34331, #167543, #88445, #203222, #20207, #54866, #184837, #154506, #71081, #18066, #166474 ),
 ( #201080, #152364, #67868, #3942, #70010, #202140, #121019, #19143, #135067, #37542, #103621, #53800, #138264, #119931, #84154, #169674 ),
 ( #87367, #153436, #186985, #150241, #170745, #134015, #22330, #155573, #27699, #173983, #140422, #25555, #158773, #142553, #143631, #77511 ) ),
 .UNSPECIFIED., .T., .F., .T. ) 
 B_SPLINE_SURFACE_WITH_KNOTS ( ( 4, 3, 4 ),
 ( 4, 2, 2, 2, 2, 2, 2, 4 ),
 ( 0.000000000000000000, 0.5000000000000000000, 1.000000000000000000 ),
 ( 0.6095821870314059865, 0.6120980958896804491, 0.6146140047479549118, 0.6196458224645037260, 0.6297094578976014656, 0.6397880689092279027, 0.6448273744150412323, 0.6498666799208544509 ),
 .UNSPECIFIED. ) 
 GEOMETRIC_REPRESENTATION_ITEM ( )  RATIONAL_B_SPLINE_SURFACE ( (
 ( 1.000000000000000000, 1.000000000000000000, 1.000000000000000000, 1.000000000000000000, 1.000000000000000000, 1.000000000000000000, 1.000000000000000000, 1.000000000000000000, 1.000000000000000000, 1.000000000000000000, 1.000000000000000000, 1.000000000000000000, 1.000000000000000000, 1.000000000000000000, 1.000000000000000000, 1.000000000000000000),
 ( 0.3333333333333333703, 0.3333333333333333703, 0.3333333333333333703, 0.3333333333333333703, 0.3333333333333333703, 0.3333333333333333703, 0.3333333333333333703, 0.3333333333333333703, 0.3333333333333333703, 0.3333333333333333703, 0.3333333333333333703, 0.3333333333333333703, 0.3333333333333333703, 0.3333333333333333703, 0.3333333333333333703, 0.3333333333333333703),
 ( 0.3333333333333333703, 0.3333333333333333703, 0.3333333333333333703, 0.3333333333333333703, 0.3333333333333333703, 0.3333333333333333703, 0.3333333333333333703, 0.3333333333333333703, 0.3333333333333333703, 0.3333333333333333703, 0.3333333333333333703, 0.3333333333333333703, 0.3333333333333333703, 0.3333333333333333703, 0.3333333333333333703, 0.3333333333333333703),
 ( 1.000000000000000000, 1.000000000000000000, 1.000000000000000000, 1.000000000000000000, 1.000000000000000000, 1.000000000000000000, 1.000000000000000000, 1.000000000000000000, 1.000000000000000000, 1.000000000000000000, 1.000000000000000000, 1.000000000000000000, 1.000000000000000000, 1.000000000000000000, 1.000000000000000000, 1.000000000000000000),
 ( 0.3333333333333333703, 0.3333333333333333703, 0.3333333333333333703, 0.3333333333333333703, 0.3333333333333333703, 0.3333333333333333703, 0.3333333333333333703, 0.3333333333333333703, 0.3333333333333333703, 0.3333333333333333703, 0.3333333333333333703, 0.3333333333333333703, 0.3333333333333333703, 0.3333333333333333703, 0.3333333333333333703, 0.3333333333333333703),
 ( 0.3333333333333333703, 0.3333333333333333703, 0.3333333333333333703, 0.3333333333333333703, 0.3333333333333333703, 0.3333333333333333703, 0.3333333333333333703, 0.3333333333333333703, 0.3333333333333333703, 0.3333333333333333703, 0.3333333333333333703, 0.3333333333333333703, 0.3333333333333333703, 0.3333333333333333703, 0.3333333333333333703, 0.3333333333333333703),
 ( 1.000000000000000000, 1.000000000000000000, 1.000000000000000000, 1.000000000000000000, 1.000000000000000000, 1.000000000000000000, 1.000000000000000000, 1.000000000000000000, 1.000000000000000000, 1.000000000000000000, 1.000000000000000000, 1.000000000000000000, 1.000000000000000000, 1.000000000000000000, 1.000000000000000000, 1.000000000000000000) ) ) 
 REPRESENTATION_ITEM ( '' )  SURFACE ( )  );
#55565 = CARTESIAN_POINT ( 'NONE',  ( -9.982881178363895103, 10.54111621771303753, 1.040834085586084257E-14 ) ) ;
#55566 = CARTESIAN_POINT ( 'NONE',  ( 4.652862234063231739, -1.464609733205827879, 1.089778014065109657 ) ) ;
#55568 = CARTESIAN_POINT ( 'NONE',  ( -4.144866890078757748, 7.628995377423835045, -0.8586628004631415845 ) ) ;
#55567 = CARTESIAN_POINT ( 'NONE',  ( -4.411198876399886615, 6.239761003923544713, -1.599625672291271394 ) ) ;
#55569 = CARTESIAN_POINT ( 'NONE',  ( 5.316739912341137853, 7.735632174496787528, -1.307268462668280673 ) ) ;
#55570 = CARTESIAN_POINT ( 'NONE',  ( 0.2097273702015931829, -1.334265282896981208, -1.107180986369905362 ) ) ;
#55571 = CARTESIAN_POINT ( 'NONE',  ( 6.544863656343847147, -1.481929198830441274, -1.092355128777318107 ) ) ;
#55572 = CARTESIAN_POINT ( 'NONE',  ( 5.813149116883928436, 2.032396105517704221, 1.093072976444838362 ) ) ;
#55573 = CARTESIAN_POINT ( 'NONE',  ( 3.867818961648523235, 7.734482231890414283, 1.040834085586084257E-14 ) ) ;
#55574 = CARTESIAN_POINT ( 'NONE',  ( 0.1751657365761209451, 0.002452341591326848407, -2.044164811867712483 ) ) ;
#55575 = CARTESIAN_POINT ( 'NONE',  ( 6.494519276145969577, 7.535692896047149425, -1.199719254218446718 ) ) ;
#55576 = CARTESIAN_POINT ( 'NONE',  ( 5.835437120055854798, -1.464435618476932488, 1.771446943145409847 ) ) ;
#55577 = CARTESIAN_POINT ( 'NONE',  ( -5.641074431737709283, 8.738948049406083385, -1.199719254218452047 ) ) ;
#55578 = EDGE_CURVE ( 'NONE', #66472, #187417, #145313, .T. ) ;
#55579 = CARTESIAN_POINT ( 'NONE',  ( 5.629731426258720361, -1.187751674602673058, -1.445209747047627946 ) ) ;
#55581 = CARTESIAN_POINT ( 'NONE',  ( -5.334207092333882017, 5.187939460669764635, 0.7998128361456281477 ) ) ;
#55580 = CARTESIAN_POINT ( 'NONE',  ( 3.761887187967042134, 0.6396200178584460216, -1.802413552503052463 ) ) ;
#55582 = CARTESIAN_POINT ( 'NONE',  ( 5.303435803989668074, 1.802500012205746183, 1.273053691228965389 ) ) ;
#55583 = CARTESIAN_POINT ( 'NONE',  ( 0.6125000000000019318, 1.229166667349464115, -1.060881119635941339 ) ) ;
#55584 = CARTESIAN_POINT ( 'NONE',  ( -7.444835747235459600, 8.818634805597074688, 1.082531754730549078 ) ) ;
#55585 = CARTESIAN_POINT ( 'NONE',  ( 4.543390873910906791, 6.393985001019784953, 1.443375672974065660 ) ) ;
#55586 = CARTESIAN_POINT ( 'NONE',  ( -4.109529958273628658, 7.808552361378938045, 0.7216878364870338292 ) ) ;
#55587 = CARTESIAN_POINT ( 'NONE',  ( 5.637388408723053246, -0.05200288984260474645, 2.120005899716829401 ) ) ;
#55588 = CARTESIAN_POINT ( 'NONE',  ( 2.415413485888187495, 2.061215426621319402, 1.037632957015870661 ) ) ;
#55589 = CARTESIAN_POINT ( 'NONE',  ( 4.053139552913617827, 1.658577106941661272, -1.047563642765911185 ) ) ;
#55590 = CARTESIAN_POINT ( 'NONE',  ( 0.2682999959267086676, -0.8333247372044670920, -1.774235371720728649 ) ) ;
#55591 = CARTESIAN_POINT ( 'NONE',  ( 4.216222584169931231, 4.021273891060765493, 1.214306433183764966E-14 ) ) ;
#55592 = CARTESIAN_POINT ( 'NONE',  ( 4.146814880933355596, 5.931313009212638931, 1.599625672291261402 ) ) ;
#55593 = ORIENTED_EDGE ( 'NONE', *, *, #208559, .T. ) ;
#55594 = CARTESIAN_POINT ( 'NONE',  ( 5.981657729715996297, -0.6748525008196132324, 1.900413905137773529 ) ) ;
#55595 = CARTESIAN_POINT ( 'NONE',  ( -8.809047120577080392, 11.30030761213851953, 1.599625672291269396 ) ) ;
#55596 = DIRECTION ( 'NONE',  ( 0.6507913734559640506, -0.7592566023653004592, 0.000000000000000000 ) ) ;
#55597 = CARTESIAN_POINT ( 'NONE',  ( 5.912764389335556814, 6.070849007079178072, -0.7216878364870512597 ) ) ;
#55598 = CARTESIAN_POINT ( 'NONE',  ( 3.502934933135398055, 0.5226102428602089622, 2.107139934106997181 ) ) ;
#55599 = CARTESIAN_POINT ( 'NONE',  ( 5.391302360089590628, 6.318882837306503575, -1.199719254218452047 ) ) ;
#55600 = CARTESIAN_POINT ( 'NONE',  ( 0.7562902151678205787, 0.8540304730459827853, -1.941197329821432227 ) ) ;
#55601 = CARTESIAN_POINT ( 'NONE',  ( 0.7499999999999885647, 1.097916667349485564, -1.299038105676652899 ) ) ;
#55602 = CARTESIAN_POINT ( 'NONE',  ( 9.622536337397022521, 12.24937836509514710, 1.599625672291281386 ) ) ;
#55603 = CARTESIAN_POINT ( 'NONE',  ( -3.128199800776549466, 2.800000000000122835, 2.480560084996058734 ) ) ;
#55604 = CARTESIAN_POINT ( 'NONE',  ( 5.568688238291347403, 7.519645578322940338, 1.337618216391135428 ) ) ;
#55605 = CARTESIAN_POINT ( 'NONE',  ( 1.370465108300226609, -1.309671233245520483, 1.591056919209728138 ) ) ;
#55607 = DIRECTION ( 'NONE',  ( -0.6249999999996199707, 4.211139888037421403E-14, -0.7806247498001041007 ) ) ;
#55606 = CARTESIAN_POINT ( 'NONE',  ( -10.16591625214838679, 10.75465713712827487, 1.040834085586084257E-14 ) ) ;
#55608 = CARTESIAN_POINT ( 'NONE',  ( 0.6823417656249899377, 1.092708333674752286, 1.181850606188755259 ) ) ;
#55609 = SURFACE_STYLE_USAGE ( .BOTH. , #137941 ) ;
#55610 = ORIENTED_EDGE ( 'NONE', *, *, #3649, .T. ) ;
#55611 = CARTESIAN_POINT ( 'NONE',  ( 3.650944405621194377, 0.2833616294029631111, 1.891055170903446658 ) ) ;
#55612 = CARTESIAN_POINT ( 'NONE',  ( 5.735142062806906083, -1.598577407953686746, 0.7598067823499834450 ) ) ;
#55613 = CARTESIAN_POINT ( 'NONE',  ( 5.365994935958575240, 9.482354201918870018, 0.7998128361456341429 ) ) ;
#55614 = CARTESIAN_POINT ( 'NONE',  ( -5.037017762676898158, 5.835274463666530131, -1.199719254218446718 ) ) ;
#55615 = CARTESIAN_POINT ( 'NONE',  ( 0.3690327605676722023, -1.530577755691145958, -0.9687459989127805704 ) ) ;
#55617 = CARTESIAN_POINT ( 'NONE',  ( 1.393601161502202590, -1.900819510297278025, 0.2380969459827488588 ) ) ;
#55616 = CARTESIAN_POINT ( 'NONE',  ( 1.445103857048099405, 8.688264192037886247, -2.625611233228245300 ) ) ;
#55618 = CARTESIAN_POINT ( 'NONE',  ( 1.926316106172959230, 1.062450747350886848, 1.776810178100460824 ) ) ;
#55619 = CARTESIAN_POINT ( 'NONE',  ( -1.364683531250014514, -0.4072916663252447167, 0.7879004041258379498 ) ) ;
#55620 = CARTESIAN_POINT ( 'NONE',  ( 6.473518811298506925, 1.789458955665638618, -0.5451884755478533240 ) ) ;
#55621 = CARTESIAN_POINT ( 'NONE',  ( 2.736711336054332921, 0.2235625380298221498, 1.811883384933578256 ) ) ;
#55623 = CARTESIAN_POINT ( 'NONE',  ( 6.198956711081595294, 6.941498593865138567, 0.8670033951987624610 ) ) ;
#55622 = CARTESIAN_POINT ( 'NONE',  ( 6.656857027519620829, -1.708965229049699053, 1.396003577074665714 ) ) ;
#55624 = CARTESIAN_POINT ( 'NONE',  ( 0.6823417656249899377, 0.8427083336747520637, 1.181850606188755259 ) ) ;
#55625 = CARTESIAN_POINT ( 'NONE',  ( 4.598127328184369311, 0.8849438138122868169, -1.863347811608778271 ) ) ;
#55626 = CARTESIAN_POINT ( 'NONE',  ( -6.958359152311683893, 9.141171649162195934, -1.599625672291263179 ) ) ;
#55627 = CARTESIAN_POINT ( 'NONE',  ( 8.378048858240820351, 11.86180853700128601, -1.199719254218446718 ) ) ;
#55628 = CARTESIAN_POINT ( 'NONE',  ( 5.854423403002611437, 5.724582146458163656, 1.040834085586084257E-14 ) ) ;
#55629 = PRESENTATION_LAYER_ASSIGNMENT (  '', '', ( #239 ) ) ;
#55630 = DIRECTION ( 'NONE',  ( -1.000000000000000000, 7.047314121155791443E-15, -8.638326563840826660E-31 ) ) ;
#55631 = CARTESIAN_POINT ( 'NONE',  ( 0.2741912710782665741, -2.129148944087058126, 0.4243047986705119068 ) ) ;
#55632 = CARTESIAN_POINT ( 'NONE',  ( -1.364683531250014514, 1.301041667008083325, -0.7879004041258289570 ) ) ;
#55633 = CARTESIAN_POINT ( 'NONE',  ( 4.218171724704827596, -1.107204882465680607, -1.856345114869990320 ) ) ;
#55634 = CARTESIAN_POINT ( 'NONE',  ( 4.424476369979273294, -0.8654530498428643082, -1.825003331238822746 ) ) ;
#55635 = CARTESIAN_POINT ( 'NONE',  ( 6.620655732516649294, 0.5674144795907026806, 2.226195167976598110 ) ) ;
#55638 = CARTESIAN_POINT ( 'NONE',  ( 5.612712406377503349, 8.531619659873665995, -1.082531754730543083 ) ) ;
#55637 = CARTESIAN_POINT ( 'NONE',  ( -3.285556943749998737, -3.580208332855374653, 1.896917185911908499 ) ) ;
#55636 = CARTESIAN_POINT ( 'NONE',  ( -15.75000000000000000, 12.69999999999999929, -3.600000000000000977 ) ) ;
#55639 = CARTESIAN_POINT ( 'NONE',  ( -4.945692173934974178, 8.992000979557944973, 0.000000000000000000 ) ) ;
#55640 = CARTESIAN_POINT ( 'NONE',  ( 2.255092540634635156, 0.09411513195021348199, -2.014433103604281960 ) ) ;
#55641 = CARTESIAN_POINT ( 'NONE',  ( -7.711890448074853133, 7.891627032375787998, -0.7998128361456291469 ) ) ;
#55643 = DIRECTION ( 'NONE',  ( -1.000000000000000000, 0.000000000000000000, 0.000000000000000000 ) ) ;
#55642 = CARTESIAN_POINT ( 'NONE',  ( -5.088387723830502196, 4.830873854090670605, -0.7998128361456221525 ) ) ;
#55644 = CYLINDRICAL_SURFACE ( 'NONE', #66941, 1.250000000000000000 ) ;
#55645 = CARTESIAN_POINT ( 'NONE',  ( 5.361546783204238942, -1.511448857895525855, -1.171587532507123441 ) ) ;
#55646 = CARTESIAN_POINT ( 'NONE',  ( -2.927671105547157371, 5.503034492191895666, 1.199719254218462483 ) ) ;
#55647 = CARTESIAN_POINT ( 'NONE',  ( 5.056828107772846082, 6.922718763866881453, -1.443375672974051449 ) ) ;
#55649 = CARTESIAN_POINT ( 'NONE',  ( 3.954703970953522774, -1.882481274494081980, -0.7231244775810635739 ) ) ;
#55648 = CARTESIAN_POINT ( 'NONE',  ( -8.798878505144665851, 9.367705798864669475, -0.7216878364870267237 ) ) ;
#55650 = CARTESIAN_POINT ( 'NONE',  ( 0.7499999999999902300, 3.983333333333352488, 1.299038105676669330 ) ) ;
#55651 = CARTESIAN_POINT ( 'NONE',  ( 0.6823417656249934904, 8.442708333674733723, 1.181850606188764807 ) ) ;
#55652 = CARTESIAN_POINT ( 'NONE',  ( 6.352575194690796678, 0.5466354793271388512, 1.635951794362877187 ) ) ;
#55653 = CARTESIAN_POINT ( 'NONE',  ( 4.875038752565570732, 7.845239757038595663, -1.199719254218452047 ) ) ;
#55654 = CARTESIAN_POINT ( 'NONE',  ( 7.280365300858406385, 11.43758391773608984, 1.040834085586084257E-14 ) ) ;
#55655 = DIRECTION ( 'NONE',  ( 0.000000000000000000, 0.000000000000000000, 1.000000000000000000 ) ) ;
#55656 = CARTESIAN_POINT ( 'NONE',  ( 5.360568611784803927, -1.355617963529401893, 1.289147430649554948 ) ) ;
#55657 = DIRECTION ( 'NONE',  ( 0.000000000000000000, 1.000000000000000000, 0.000000000000000000 ) ) ;
#55658 = CARTESIAN_POINT ( 'NONE',  ( 2.008725816923035978, 0.6454906730102347723, 1.967154155859623055 ) ) ;
#55659 = CARTESIAN_POINT ( 'NONE',  ( -6.360183458142173230, 9.473945563590925545, 1.082531754730549967 ) ) ;
#55660 = ORIENTED_EDGE ( 'NONE', *, *, #31289, .T. ) ;
#55661 = CARTESIAN_POINT ( 'NONE',  ( 0.9664229901367870079, -1.967894173845801120, -0.4390061282484732930 ) ) ;
#55662 = CARTESIAN_POINT ( 'NONE',  ( 1.581973821214562204, 0.9331543445117953528, 1.552620351220496353 ) ) ;
#55663 = CARTESIAN_POINT ( 'NONE',  ( 5.194182247366881278, 5.232503174782402233, 0.7216878364870328300 ) ) ;
#55664 = DIRECTION ( 'NONE',  ( 0.000000000000000000, 0.000000000000000000, 1.000000000000000000 ) ) ;
#55665 = EDGE_CURVE ( 'NONE', #114168, #127442, #150243, .T. ) ;
#55666 = CARTESIAN_POINT ( 'NONE',  ( 7.822691444960700125, 10.14955932391940330, -1.443375672974058777 ) ) ;
#55667 = CARTESIAN_POINT ( 'NONE',  ( 7.588813295347141441, 9.876701482703580837, -1.599625672291262513 ) ) ;
#55669 = CARTESIAN_POINT ( 'NONE',  ( 5.958580499074456860, -1.820587016788511647, -0.5960958187592230173 ) ) ;
#55668 = CARTESIAN_POINT ( 'NONE',  ( -5.693534442735004752, 8.729875052244421951, 1.199719254218452047 ) ) ;
#55670 = CARTESIAN_POINT ( 'NONE',  ( 0.07499057489264349119, 0.002531239327734788758, -1.955573237620360061 ) ) ;
#55671 = CARTESIAN_POINT ( 'NONE',  ( -4.052968920965120958, 3.984128252961195216, -0.5207863488562065601 ) ) ;
#55672 = CARTESIAN_POINT ( 'NONE',  ( -0.6823417656250246877, -0.6364583329919113464, 1.181850606188755259 ) ) ;
#55674 = ORIENTED_EDGE ( 'NONE', *, *, #77512, .F. ) ;
#55673 = CARTESIAN_POINT ( 'NONE',  ( 3.063779527008304360, 6.518233848244248563, 0.7216878364870317197 ) ) ;
#55675 = CARTESIAN_POINT ( 'NONE',  ( -7.944714827928056167, 10.29191993738131927, 1.443375672974090751 ) ) ;
#55676 = CARTESIAN_POINT ( 'NONE',  ( 3.151412294154242844, -1.766339975446712174, -1.245920677233211649 ) ) ;
#55677 = CARTESIAN_POINT ( 'NONE',  ( -2.959422669532919326, 6.674686557755516780, 0.7998128361456352531 ) ) ;
#55678 = CARTESIAN_POINT ( 'NONE',  ( 5.343321937561575474, 8.287607122913563273, -1.082531754730548412 ) ) ;
#55679 = CARTESIAN_POINT ( 'NONE',  ( 1.248456593208754795, 1.040400552670465162, -1.847740296886036582 ) ) ;
#55680 = CARTESIAN_POINT ( 'NONE',  ( 6.018537349360657984, 1.224031959697377658, -1.354583942311540667 ) ) ;
#55681 = EDGE_CURVE ( 'NONE', #211051, #127758, #1097, .T. ) ;
#55682 = CARTESIAN_POINT ( 'NONE',  ( 2.389859445797080095, -0.8464594663768022498, 1.780534303499915927 ) ) ;
#55683 = CARTESIAN_POINT ( 'NONE',  ( 4.113462262696740979, 1.539102623358613586, 1.134910093507961237 ) ) ;
#55684 = ORIENTED_EDGE ( 'NONE', *, *, #142758, .T. ) ;
#55685 = CARTESIAN_POINT ( 'NONE',  ( -9.086263084862915562, 14.48154074114212797, -7.851261044451125493 ) ) ;
#55686 = CARTESIAN_POINT ( 'NONE',  ( 4.685976223243822680, -1.210123887884282601, -1.553869430650482997 ) ) ;
#55687 = CARTESIAN_POINT ( 'NONE',  ( 6.603083112279575673, -0.4245024861969335928, 1.902271653767301007 ) ) ;
#55688 = VERTEX_POINT ( 'NONE', #203156 ) ;
#55689 = CARTESIAN_POINT ( 'NONE',  ( -4.423703259808839938, 8.383013913077441259, 0.7998128361456352531 ) ) ;
#55691 = CARTESIAN_POINT ( 'NONE',  ( 6.781144757626056396, -7.161464053357567749, -6.776370306708062508 ) ) ;
#55690 = CARTESIAN_POINT ( 'NONE',  ( -5.966997003790217136, 9.975597247814986801, -0.7216878364870338292 ) ) ;
#55693 = CARTESIAN_POINT ( 'NONE',  ( 6.658462837642799670, 7.901199744405670522, 1.082531754730549967 ) ) ;
#55692 = CARTESIAN_POINT ( 'NONE',  ( 6.123478934866503742, 10.29580919065294431, 0.7998128361456462443 ) ) ;
#55695 = VERTEX_POINT ( 'NONE', #38550 ) ;
#55694 = CARTESIAN_POINT ( 'NONE',  ( 5.408822929737922003, -0.4686924282312036061, -1.853821656156897646 ) ) ;
#55696 = CARTESIAN_POINT ( 'NONE',  ( 0.6224627697807673110, -1.182292326766160251, -1.863150505713020211 ) ) ;
#55697 = CARTESIAN_POINT ( 'NONE',  ( 9.601861708076905089, 3.883749503203147047, -7.121442012218629714 ) ) ;
#55698 = CARTESIAN_POINT ( 'NONE',  ( 5.883453010584854148, 0.1459518013421389204, -2.007843741401983184 ) ) ;
#55699 = CARTESIAN_POINT ( 'NONE',  ( -0.02319159430947542386, 1.394398620246390275, -2.068318759734718792 ) ) ;
#55700 = FACE_OUTER_BOUND ( 'NONE', #13591, .T. ) ;
#55701 = CARTESIAN_POINT ( 'NONE',  ( -0.08000000000000194456, -9.999999999999994671, -10.91970695577494865 ) ) ;
#55702 = CARTESIAN_POINT ( 'NONE',  ( -6.770610912236891821, -7.154544010627095219, -6.663994888585869525 ) ) ;
#55703 = CARTESIAN_POINT ( 'NONE',  ( 2.506376218629560171, 2.069854378281150709, 0.05321039126485183068 ) ) ;
#55704 = CARTESIAN_POINT ( 'NONE',  ( -4.740547266272593596, 8.682388910626682943, -0.7998128361456281477 ) ) ;
#55705 = CIRCLE ( 'NONE', #118089, 3.000000000000010214 ) ;
#55706 = CARTESIAN_POINT ( 'NONE',  ( -4.662190612263335865, 8.310640895677696705, -0.4745246276153299858 ) ) ;
#55708 = CARTESIAN_POINT ( 'NONE',  ( 0.6905621207787122628, -2.145541755201633372, -0.2633910710312590275 ) ) ;
#55707 = CARTESIAN_POINT ( 'NONE',  ( -5.148345644887285744, 7.029489223833707001, -1.599625672291256295 ) ) ;
#55709 = COLOUR_RGB ( '', 0.72549020, 0.75294118, 0.79215686) ;
#55710 = CARTESIAN_POINT ( 'NONE',  ( -11.75936552431323179, 8.614003048789559358, 2.408008290394755058 ) ) ;
#55711 = CARTESIAN_POINT ( 'NONE',  ( 3.770576118376296471, 7.413106214832098750, 0.7216878364870257245 ) ) ;
#55712 = CARTESIAN_POINT ( 'NONE',  ( 4.232369794311310053E-13, -9.350066838357705024, 9.500000000000001776 ) ) ;
#55713 = CARTESIAN_POINT ( 'NONE',  ( -1.402160292154681736E-14, 13.23437500034139980, 1.575800808251682339 ) ) ;
#55715 = CARTESIAN_POINT ( 'NONE',  ( -4.769436176957319695, 8.786368983084006601, 0.7998128361456281477 ) ) ;
#55714 = CARTESIAN_POINT ( 'NONE',  ( 6.925078400183559246, 1.280611897634201357, 1.970548662192173284 ) ) ;
#55716 = CARTESIAN_POINT ( 'NONE',  ( 5.273917847569165929, 1.525789468548454986, -0.8241785451228255122 ) ) ;
#55717 = CARTESIAN_POINT ( 'NONE',  ( -2.740719608256871442, 6.349256642941639051, 0.7998128361456341429 ) ) ;
#55718 = CARTESIAN_POINT ( 'NONE',  ( 2.272408084759574454, -0.9721198248324285363, -1.827787434591138238 ) ) ;
#55719 = CARTESIAN_POINT ( 'NONE',  ( 4.868830934094980911, -0.2605620880507720227, -2.101091820269097354 ) ) ;
#55720 = CARTESIAN_POINT ( 'NONE',  ( 7.772902139336337335, 7.962807338847539107, 0.7998128361456341429 ) ) ;
#55721 = CARTESIAN_POINT ( 'NONE',  ( -0.9486429539237333231, 3.292910930033766892, 1.028101543438982635 ) ) ;
#55722 = CARTESIAN_POINT ( 'NONE',  ( 1.569134323820881027, 1.734487354001874371, 0.9329377246683704383 ) ) ;
#55723 = CARTESIAN_POINT ( 'NONE',  ( 6.093061176370408560, 6.029359313278345844, 0.2718797729955486631 ) ) ;
#55724 = CARTESIAN_POINT ( 'NONE',  ( 0.7207899753199145110, 1.446443371814851941, -1.251069288267861346 ) ) ;
#55725 = CARTESIAN_POINT ( 'NONE',  ( 4.787240309336779909, 1.696446081987776022, 1.541789747812449818 ) ) ;
#55726 = CARTESIAN_POINT ( 'NONE',  ( 1.857752496991037061, 1.820901040755190214, -0.1330985588276211995 ) ) ;
#55727 = CARTESIAN_POINT ( 'NONE',  ( 5.903649544107831382, 5.852288987739402870, -0.7998128361456481317 ) ) ;
#55728 = CARTESIAN_POINT ( 'NONE',  ( 6.290620086616457662, 6.441404310581745563, 1.040834085586084257E-14 ) ) ;
#55729 = CARTESIAN_POINT ( 'NONE',  ( -9.006694118179950692, 9.402231314165087284, 1.040834085586084257E-14 ) ) ;
#55730 =( BOUNDED_CURVE ( )  B_SPLINE_CURVE ( 3, ( #66649, #82934, #67715, #131744 ),
 .UNSPECIFIED., .F., .T. ) 
 B_SPLINE_CURVE_WITH_KNOTS ( ( 4, 4 ),
 ( 0.000000000000000000, 0.4999999999999967248 ),
 .UNSPECIFIED. ) 
 CURVE ( )  GEOMETRIC_REPRESENTATION_ITEM ( )  RATIONAL_B_SPLINE_CURVE ( ( 1.000000000000000222, 0.3333333333333378112, 0.3333333333333334259, 0.9999999999999958922 ) ) 
 REPRESENTATION_ITEM ( '' )  );
#55731 = CARTESIAN_POINT ( 'NONE',  ( 2.883067256526872235, -1.861736025891271407, -0.7665772676846579481 ) ) ;
#55732 = CARTESIAN_POINT ( 'NONE',  ( 3.362109073961420780, -1.959717995770013932, 0.09162775335717905645 ) ) ;
#55733 = CARTESIAN_POINT ( 'NONE',  ( -9.332089804907933939, 9.781859615347734405, 1.040834085586084257E-14 ) ) ;
#55734 = CARTESIAN_POINT ( 'NONE',  ( -6.087774667736030487, 7.061157519568837415, 1.199719254218450271 ) ) ;
#55735 = CARTESIAN_POINT ( 'NONE',  ( 0.07536363704233051131, 7.629137130509080045, -2.744199452819145790 ) ) ;
#55737 = CARTESIAN_POINT ( 'NONE',  ( 5.137463350450376609, -1.253266684191740810, -1.249936613051380485 ) ) ;
#55736 = CARTESIAN_POINT ( 'NONE',  ( 6.474567623737461197, -0.1010770918629246007, -2.088323083193554641 ) ) ;
#55738 = CARTESIAN_POINT ( 'NONE',  ( -0.7499999999999972244, 3.389583334016149863, -1.299038105676652011 ) ) ;
#55739 = CARTESIAN_POINT ( 'NONE',  ( 0.2522424171345696298, 0.8426718423822797677, 2.023156535103701970 ) ) ;
#55740 = CARTESIAN_POINT ( 'NONE',  ( 0.1513755341013711675, 0.6631104863988640519, 1.609371435944781936 ) ) ;
#55741 = CARTESIAN_POINT ( 'NONE',  ( 6.425674737872927089, 9.584038729905381970, -1.199719254218440723 ) ) ;
#55742 = CARTESIAN_POINT ( 'NONE',  ( 0.1333692844072802142, 2.017199222642913625, -2.468757726274827036 ) ) ;
#55743 = CARTESIAN_POINT ( 'NONE',  ( 6.170549959107765936, 1.581869261771509994, 1.668023173554062266 ) ) ;
#55744 = CARTESIAN_POINT ( 'NONE',  ( 3.006787879153326681, 6.373552747333731006, -0.4818892653130519843 ) ) ;
#55745 = CARTESIAN_POINT ( 'NONE',  ( 5.958250847983307175, 1.314789979124462382, 1.130330842948763514 ) ) ;
#55746 = CARTESIAN_POINT ( 'NONE',  ( 1.664966938652842954, -1.558911317520403239, 1.562347339584921002 ) ) ;
#55747 = CARTESIAN_POINT ( 'NONE',  ( 0.5675212215028536678, 1.888217155380923939, 1.071465276393630539 ) ) ;
#55748 = CARTESIAN_POINT ( 'NONE',  ( 0.3999999999999758193, 3.000000000000047518, 2.023857702507768419 ) ) ;
#55749 = CARTESIAN_POINT ( 'NONE',  ( 1.411481693167576434, -1.991701369327549154, 0.7188087792022596068 ) ) ;
#55750 = CARTESIAN_POINT ( 'NONE',  ( 2.875000000000002220, 2.052068128417948056, -1.638482584539516883E-13 ) ) ;
#55751 = CARTESIAN_POINT ( 'NONE',  ( 6.827182134110192813, 3.687242579989722824, 2.603029107617850002 ) ) ;
#55752 = CARTESIAN_POINT ( 'NONE',  ( 4.418917755230268085, 1.760988537516799068, 0.7813691060932350663 ) ) ;
#55753 = CARTESIAN_POINT ( 'NONE',  ( 1.137687779795238052, -0.04954009815814026940, 2.220905934856795216 ) ) ;
#55754 = ORIENTED_EDGE ( 'NONE', *, *, #98691, .F. ) ;
#55756 = CARTESIAN_POINT ( 'NONE',  ( 1.499999999999989120, 5.004166666666691299, 0.8660254037844524744 ) ) ;
#55755 = CARTESIAN_POINT ( 'NONE',  ( 1.664052950329899971, 1.182993008014191938, 1.963431667052175422 ) ) ;
#55757 = CARTESIAN_POINT ( 'NONE',  ( 4.955668840994886359, 5.740367388370866131, 1.199719254218462483 ) ) ;
#55758 = CARTESIAN_POINT ( 'NONE',  ( 4.659198344590585350, 8.587481835331020719, 0.7998128361456462443 ) ) ;
#55759 = CARTESIAN_POINT ( 'NONE',  ( 3.897323497890590627, -0.2185073706607517652, -2.210542651646169698 ) ) ;
#55760 = CARTESIAN_POINT ( 'NONE',  ( -7.212574532790087645, 11.35849468832304154, -0.7216878364870267237 ) ) ;
#55761 =( NAMED_UNIT ( * ) PLANE_ANGLE_UNIT ( ) SI_UNIT ( $, .RADIAN. ) );
#55762 = CARTESIAN_POINT ( 'NONE',  ( 5.314433026876846711, 9.143996264757578984, -0.7216878364870267237 ) ) ;
#55763 = CARTESIAN_POINT ( 'NONE',  ( -9.951321562306267410, 10.71222269888655987, 1.040834085586084257E-14 ) ) ;
#55764 = CARTESIAN_POINT ( 'NONE',  ( 5.221298555038576872, 9.105615724271411082, 0.000000000000000000 ) ) ;
#55765 = CARTESIAN_POINT ( 'NONE',  ( 1.301407962653992501, 1.352153127569672098, -1.496052916918483522 ) ) ;
#55767 = CARTESIAN_POINT ( 'NONE',  ( 6.250444628687981563, -2.052375444028589957, -0.2060817263721328174 ) ) ;
#55766 = CARTESIAN_POINT ( 'NONE',  ( 8.076906825439115423, 10.44614393447756129, -1.599625672291262513 ) ) ;
#55768 = CARTESIAN_POINT ( 'NONE',  ( 11.94105721237523277, 10.19999999999999929, -1.187919463087249827 ) ) ;
#55769 = CARTESIAN_POINT ( 'NONE',  ( 7.363486825553451354, 8.723727730301414240, -1.082531754730548412 ) ) ;
#55770 = CARTESIAN_POINT ( 'NONE',  ( 0.08126746489400815676, -0.8690269180096841239, 1.623235155968821841 ) ) ;
#55771 = CARTESIAN_POINT ( 'NONE',  ( -2.298420387838187473, 5.509269730139584986, -0.7346435760097105305 ) ) ;
#55772 = CARTESIAN_POINT ( 'NONE',  ( -1.201851678989727383E-14, 2.946875000341419248, -1.575800808251660134 ) ) ;
#55773 = CARTESIAN_POINT ( 'NONE',  ( 1.633702333402654361, 0.8778187100713531477, -1.536624053347920071 ) ) ;
#55774 = CARTESIAN_POINT ( 'NONE',  ( 6.434187037261335007, -1.398866626055271123, -1.024706079042293938 ) ) ;
#55775 = CARTESIAN_POINT ( 'NONE',  ( 6.216323138650166058, 1.627425874425829200, 0.6175015193602851893 ) ) ;
#55776 = CARTESIAN_POINT ( 'NONE',  ( 3.702894494004336678, 1.966553232070525237, 1.177740060511106135 ) ) ;
#55777 = CARTESIAN_POINT ( 'NONE',  ( 3.187279605439637287, -0.7454021820463945236, 1.683677988101241141 ) ) ;
#55778 = CARTESIAN_POINT ( 'NONE',  ( 6.909851844459134362, 11.21324425184434936, -0.7998128361456291469 ) ) ;
#55779 = CARTESIAN_POINT ( 'NONE',  ( 1.469576158976823947E-15, 15.00000000000000000, 12.00000000000000178 ) ) ;
#55780 = CARTESIAN_POINT ( 'NONE',  ( 3.100428009929767637, -0.5284298666012043899, -1.747434388548900541 ) ) ;
#55781 = CARTESIAN_POINT ( 'NONE',  ( 3.762342404062005041, 1.897698010425369786, -0.6819954029829021769 ) ) ;
#55782 = CARTESIAN_POINT ( 'NONE',  ( -9.775592450653132204, 11.36361159963886891, -1.199719254218441611 ) ) ;
#55784 = CARTESIAN_POINT ( 'NONE',  ( -7.944151662964566540, 8.232874793072271657, 0.000000000000000000 ) ) ;
#55783 = CARTESIAN_POINT ( 'NONE',  ( 2.993345543732395697, 1.941157005910049138, -1.162047774482692697 ) ) ;
#55785 = CARTESIAN_POINT ( 'NONE',  ( 5.930723256393157783, 2.028624516890007445, 0.5651790528119063906 ) ) ;
#55786 = CARTESIAN_POINT ( 'NONE',  ( 10.12955225396220271, 13.73833855058678743, 7.326689838346525541 ) ) ;
#55787 = CARTESIAN_POINT ( 'NONE',  ( 3.859880467719906783, -0.6038372105774907350, 1.980330894321411517 ) ) ;
#55788 = CARTESIAN_POINT ( 'NONE',  ( 10.71502147350184231, 11.39527989537399755, 0.000000000000000000 ) ) ;
#55789 = CARTESIAN_POINT ( 'NONE',  ( -0.6801582343750386395, 2.380208333674735499, -1.178068619123869398 ) ) ;
#55790 = CARTESIAN_POINT ( 'NONE',  ( 6.024112365460934981, -2.104525519549589330, 0.2592714029671301934 ) ) ;
#55791 = ITEM_DEFINED_TRANSFORMATION ( 'NONE', 'NONE', #59109,  #200407 ) ;
#55794 = EDGE_CURVE ( 'NONE', #138769, #148041, #40699, .T. ) ;
#55793 = CARTESIAN_POINT ( 'NONE',  ( 1.330555237386946255, 1.856516968354186892, 0.5143259067744552215 ) ) ;
#55792 = CARTESIAN_POINT ( 'NONE',  ( -8.317037166979361018, 11.79062823052953668, 1.199719254218453823 ) ) ;
#55795 = CARTESIAN_POINT ( 'NONE',  ( -3.283337425626721373, -0.1112512837626866702, -0.1207467602163218856 ) ) ;
#55796 = CARTESIAN_POINT ( 'NONE',  ( 8.289920859751990889, 11.75899253876431416, 1.199719254218450271 ) ) ;
#55797 = CARTESIAN_POINT ( 'NONE',  ( 5.045042557616584489, 5.058506870073687267, 0.000000000000000000 ) ) ;
#55798 = CARTESIAN_POINT ( 'NONE',  ( 5.530423754462008290, 6.204488192500752675, 0.9375459734879583173 ) ) ;
#55799 = CARTESIAN_POINT ( 'NONE',  ( -1.127943160727153060, 2.800000000000024691, -0.7749999999999935829 ) ) ;
#55800 = CARTESIAN_POINT ( 'NONE',  ( -2.916975605234527702, 6.554888639415577423, 1.040834085586084257E-14 ) ) ;
#55801 = CARTESIAN_POINT ( 'NONE',  ( 0.7740458967449159733, 0.4260312260581029520, -2.180030009307607042 ) ) ;
#55802 = CARTESIAN_POINT ( 'NONE',  ( 2.467921950875014314, 2.065534160692492627, -0.4097329821706324204 ) ) ;
#55804 = CARTESIAN_POINT ( 'NONE',  ( -4.516801452008150086, 5.298631777878131111, 1.199719254218452935 ) ) ;
#55803 = AXIS2_PLACEMENT_3D ( 'NONE', #167300, #2626, #103362 ) ;
#55805 = CARTESIAN_POINT ( 'NONE',  ( 6.916630921265960019, 11.22115317478565188, 0.7998128361456462443 ) ) ;
#55806 = CARTESIAN_POINT ( 'NONE',  ( 0.1505322013598429098, -0.3980627942141829467, -1.824191605747552014 ) ) ;
#55807 = CARTESIAN_POINT ( 'NONE',  ( 7.772902139336337335, 7.962807338847539107, 0.7998128361456341429 ) ) ;
#55808 = CARTESIAN_POINT ( 'NONE',  ( 11.97929049433705551, 9.799999999999997158, 0.7046979865771803020 ) ) ;
#55809 = CARTESIAN_POINT ( 'NONE',  ( -5.628043163448566588, 9.580151100749725757, 0.000000000000000000 ) ) ;
#55810 = CARTESIAN_POINT ( 'NONE',  ( -9.164948653158003111, 9.794787638213568570, -0.7216878364870267237 ) ) ;
#55811 = CARTESIAN_POINT ( 'NONE',  ( 0.8617730121942971389, -1.675286201960282995, -1.300076073212981242 ) ) ;
#55812 = CARTESIAN_POINT ( 'NONE',  ( -5.399890319992785237, 9.521898816625391504, 0.7998128361456291469 ) ) ;
#55814 = CARTESIAN_POINT ( 'NONE',  ( 3.560947883890089649, 1.548132398191165882, -1.204989647596923508 ) ) ;
#55813 = CARTESIAN_POINT ( 'NONE',  ( 1.225000000000008971, -0.6250000000000005551, -1.561251128379126385E-14 ) ) ;
#55815 = CARTESIAN_POINT ( 'NONE',  ( 1.762795743007524063, -1.528684080660724920, 1.528680807790387286 ) ) ;
#55816 = CARTESIAN_POINT ( 'NONE',  ( 1.786409390178132162, 1.601450680722369846, -0.9084932335857234253 ) ) ;
#55818 = CARTESIAN_POINT ( 'NONE',  ( -4.567562471335953944, 6.984949105684680859, -1.180336305634868577 ) ) ;
#55817 = CARTESIAN_POINT ( 'NONE',  ( -5.659602779061863487, 5.567567761852417085, 0.7998128361456281477 ) ) ;
#55819 = CARTESIAN_POINT ( 'NONE',  ( 3.855166295008194410, 1.726882014201753801, -0.2153026951989250037 ) ) ;
#55820 = CARTESIAN_POINT ( 'NONE',  ( 7.321039761699430493, 7.643560598178549270, -0.7216878364870257245 ) ) ;
#55821 = CARTESIAN_POINT ( 'NONE',  ( -11.36817070414822695, 5.406007704794011381, -5.610921796774237968 ) ) ;
#55822 = COLOUR_RGB ( '', 0.31764706, 0.68627451, 0.89019608) ;
#55823 = CARTESIAN_POINT ( 'NONE',  ( 1.059701713109785670, 0.4209238396889224965, -2.120155868012041811 ) ) ;
#55824 = CARTESIAN_POINT ( 'NONE',  ( 3.040388574052850235, 1.915307028720541371, -0.6297779509270851062 ) ) ;
#55825 = CARTESIAN_POINT ( 'NONE',  ( 6.825078400183582694, 6.033236438919748146, 2.839236806905225841 ) ) ;
#55826 = CARTESIAN_POINT ( 'NONE',  ( 0.1632417891470130944, -1.931755829615459996, -0.9703963252955111196 ) ) ;
#55827 = ADVANCED_FACE ( 'NONE', ( #72087 ), #202073, .T. ) ;
#55828 = CARTESIAN_POINT ( 'NONE',  ( 2.518385046665332361, 1.288922565979855994, -1.491834565112426070 ) ) ;
#55829 = CARTESIAN_POINT ( 'NONE',  ( 6.609000000000047947, 7.053019707385148607, 2.498153760597703332 ) ) ;
#55830 = CARTESIAN_POINT ( 'NONE',  ( 2.595178948467924851, -0.6067665810922833192, 1.844924317596825070 ) ) ;
#55833 = ORIENTED_EDGE ( 'NONE', *, *, #18887, .F. ) ;
#55832 = CARTESIAN_POINT ( 'NONE',  ( -3.851925040058333582, 7.508013290127760087, -0.7216878364870458196 ) ) ;
#55831 = SURFACE_STYLE_USAGE ( .BOTH. , #22228 ) ;
#55834 = CARTESIAN_POINT ( 'NONE',  ( -4.787437638956935082, 6.678706226906775179, -1.443375672974066548 ) ) ;
#55835 = CARTESIAN_POINT ( 'NONE',  ( -0.1106856583840877956, 1.350702755748961481, -2.249207804202685956 ) ) ;
#55836 = CARTESIAN_POINT ( 'NONE',  ( 5.143339171537801846, 7.093924681584509173, 1.599625672291269396 ) ) ;
#55837 = CARTESIAN_POINT ( 'NONE',  ( -6.143779885648060102, 7.196773283791382703, 1.199719254218452047 ) ) ;
#55838 = CARTESIAN_POINT ( 'NONE',  ( -7.065734331377342414, 8.272386803808890576, -1.199719254218452047 ) ) ;
#55839 = CARTESIAN_POINT ( 'NONE',  ( -6.337068562759858636, 6.936200024879327408, -0.9492287992594623525 ) ) ;
#55840 = CARTESIAN_POINT ( 'NONE',  ( 6.370204010553460527, 1.178711257604664109, 1.983722394024198143 ) ) ;
#55841 = LINE ( 'NONE', #172809, #136039 ) ;
#55842 = CARTESIAN_POINT ( 'NONE',  ( 3.678520109711844732, 1.247982904293298168, -1.513573691770610186 ) ) ;
#55843 = CARTESIAN_POINT ( 'NONE',  ( 7.609150525767641504, 9.900428251527500834, -1.599625672291262513 ) ) ;
#55844 = CARTESIAN_POINT ( 'NONE',  ( 1.037732671793228700, -1.587836052788630381, 1.242728777923551187 ) ) ;
#55845 = EDGE_LOOP ( 'NONE', ( #33638, #199869, #73402, #157347, #185354, #80881, #21665, #101202 ) ) ;
#55846 = CARTESIAN_POINT ( 'NONE',  ( 2.571616345043222118, 1.500848072127154653, 1.493768111954131284 ) ) ;
#55847 = CARTESIAN_POINT ( 'NONE',  ( -1.402160292154681736E-14, 1.368750000682821710, -1.732050807568863648 ) ) ;
#55848 = CARTESIAN_POINT ( 'NONE',  ( -6.693975156845199059, 8.832723654451292816, 1.599625672291283607 ) ) ;
#55849 = CARTESIAN_POINT ( 'NONE',  ( 3.134520880496122874, -1.623366475481220261, 0.8686021547102339424 ) ) ;
#55850 = ORIENTED_EDGE ( 'NONE', *, *, #131846, .F. ) ;
#55851 = CARTESIAN_POINT ( 'NONE',  ( -8.350932551013499960, 11.83017284523606172, -1.199719254218446718 ) ) ;
#55852 = DIRECTION ( 'NONE',  ( 0.000000000000000000, 1.000000000000000000, 0.000000000000000000 ) ) ;
#55853 = CARTESIAN_POINT ( 'NONE',  ( 4.482752736079084421, -1.382999391253452615, 1.607682512923855445 ) ) ;
#55854 = CARTESIAN_POINT ( 'NONE',  ( 0.2867153840934755782, 1.362228626754984573, 1.238794746348782505 ) ) ;
#55855 = CARTESIAN_POINT ( 'NONE',  ( 0.000000000000000000, 5.000000000000000888, -10.25000000000000000 ) ) ;
#55856 = CARTESIAN_POINT ( 'NONE',  ( 6.908042961362778733, 8.018137195466769285, 1.199719254218462483 ) ) ;
#55857 = CARTESIAN_POINT ( 'NONE',  ( 5.027041095616958444, 9.086908054853605421, 0.000000000000000000 ) ) ;
#55858 = CARTESIAN_POINT ( 'NONE',  ( 4.833308404897187494, -1.885807738700072678, 0.8313965460460555068 ) ) ;
#55860 = CARTESIAN_POINT ( 'NONE',  ( 0.9777802892061361328, -1.796362506263927017, -0.4033719513514141264 ) ) ;
#55859 = CARTESIAN_POINT ( 'NONE',  ( -5.716734326456539783, 9.821273814174633188, -0.7998128361456231517 ) ) ;
#55861 = CARTESIAN_POINT ( 'NONE',  ( 5.549815083142378924, 6.383051840172381475, -1.247766374558601399 ) ) ;
#55862 = CARTESIAN_POINT ( 'NONE',  ( -2.974142338115852269, 6.685868392857900133, 0.1038623869373533903 ) ) ;
#55863 = CARTESIAN_POINT ( 'NONE',  ( 10.94305301526625840, -8.100264386820958507, -0.2223449190352319027 ) ) ;
#55864 = VECTOR ( 'NONE', #65917, 1000.000000000000000 ) ;
#55865 = CARTESIAN_POINT ( 'NONE',  ( 1.471597369358583318, 0.1596246592955492538, -2.201166978212334424 ) ) ;
#55866 = CARTESIAN_POINT ( 'NONE',  ( 3.567884397833466892, 2.208229897964437249, -0.4915367949662046154 ) ) ;
#55867 = CIRCLE ( 'NONE', #176938, 0.08000000000000040412 ) ;
#55868 = CARTESIAN_POINT ( 'NONE',  ( -8.690413276679693766, 9.241163032322203819, 1.040834085586084257E-14 ) ) ;
#55869 = CARTESIAN_POINT ( 'NONE',  ( 4.148556159002002808, 1.777816924242316299, 0.3471830323657533746 ) ) ;
#55870 = CARTESIAN_POINT ( 'NONE',  ( 3.801880972252824176, -0.9895533254376009946, -1.640229128645746215 ) ) ;
#55871 = CARTESIAN_POINT ( 'NONE',  ( 5.213363469605923228, -1.747142239327776903, -1.110534646669825376 ) ) ;
#55872 = CARTESIAN_POINT ( 'NONE',  ( -0.6823417656249969321, 3.780208333674754506, -1.181850606188749264 ) ) ;
#55873 = CARTESIAN_POINT ( 'NONE',  ( 2.571113415349820297, 0.09854779587974149546, -1.969128565948689458 ) ) ;
#55874 = CARTESIAN_POINT ( 'NONE',  ( 0.9910896068104644296, 1.700257414060426964, -0.9055851426933002601 ) ) ;
#55875 = CARTESIAN_POINT ( 'NONE',  ( 4.153091690245942047, -1.555063956268587066, -1.039456662654779207 ) ) ;
#55876 = CARTESIAN_POINT ( 'NONE',  ( 3.528207577792912719, -1.374008478127983546, -1.853924954965507466 ) ) ;
#55877 = CARTESIAN_POINT ( 'NONE',  ( 3.666312420855986520, -0.7522870471967492145, -1.702408540065254883 ) ) ;
#55878 = CARTESIAN_POINT ( 'NONE',  ( -0.6823417656250212460, 4.301041667008085767, 1.181850606188767472 ) ) ;
#55879 = CARTESIAN_POINT ( 'NONE',  ( 6.343235766347262938, 8.493804042195527870, -1.599625672291281386 ) ) ;
#55880 = DIRECTION ( 'NONE',  ( 0.000000000000000000, 1.000000000000000000, 0.000000000000000000 ) ) ;
#55881 = CARTESIAN_POINT ( 'NONE',  ( 0.7156196601619690956, -0.3068708111382661974, 2.083463767009658962 ) ) ;
#55882 = CARTESIAN_POINT ( 'NONE',  ( 2.968872451268290913, 5.447139712246216625, -1.082531754730543971 ) ) ;
#55884 = CARTESIAN_POINT ( 'NONE',  ( 5.066970889784239596, 4.909229436870949925, 0.2438227144904350496 ) ) ;
#55883 = CARTESIAN_POINT ( 'NONE',  ( -0.6823417656249969321, 5.530208333674756283, -1.181850606188749264 ) ) ;
#55885 = CARTESIAN_POINT ( 'NONE',  ( -1.930226670627066099, 8.999999999999998224, -0.7749999999999996891 ) ) ;
#55886 = CARTESIAN_POINT ( 'NONE',  ( 3.041385797112206912, 0.05609166564453024750, 2.120036961950934273 ) ) ;
#55887 = CARTESIAN_POINT ( 'NONE',  ( 2.987253516826691158, 6.445425535883942736, -0.5244392418292821434 ) ) ;
#55888 = CARTESIAN_POINT ( 'NONE',  ( 0.8440173190735723585, -1.284739210308597723, -1.558479848626155961 ) ) ;
#55889 = CARTESIAN_POINT ( 'NONE',  ( 1.364683531249986537, 1.155208333674754728, -0.7879004041258239610 ) ) ;
#55890 = CARTESIAN_POINT ( 'NONE',  ( -3.551873057100300990, 5.166937871415542283, 1.443375672974064550 ) ) ;
#55891 = CARTESIAN_POINT ( 'NONE',  ( 5.443762371086860341, 6.309809840144842141, 1.199719254218462483 ) ) ;
#55892 = VERTEX_POINT ( 'NONE', #39612 ) ;
#55893 = CARTESIAN_POINT ( 'NONE',  ( 0.7026770610618977564, -0.7276074859871293210, -2.035605373553108777 ) ) ;
#55894 = CARTESIAN_POINT ( 'NONE',  ( 6.610000000000037623, 2.481806704560181043, 2.105257736569548399 ) ) ;
#55897 = CARTESIAN_POINT ( 'NONE',  ( 4.121315508874254796, 5.831287398485176077, -1.443375672974051449 ) ) ;
#55896 = CARTESIAN_POINT ( 'NONE',  ( 6.825078400183526739, -0.0002198122173602961866, 1.955566246027613531 ) ) ;
#55895 = CARTESIAN_POINT ( 'NONE',  ( 4.386945222473598527, 7.275797305264619652, -1.199719254218452047 ) ) ;
#55898 = CARTESIAN_POINT ( 'NONE',  ( 4.370663978927065152, 5.060324124126027279, 2.420000000000000373 ) ) ;
#55899 = CARTESIAN_POINT ( 'NONE',  ( 5.471888747823221877, -0.9023485654677811940, 1.803414228490702209 ) ) ;
#55900 = CARTESIAN_POINT ( 'NONE',  ( -8.703971430293361067, 9.256980878204810637, 0.7216878364870438212 ) ) ;
#55901 = CARTESIAN_POINT ( 'NONE',  ( 0.2577194443907256383, 2.166829308800602316, -0.3276212646995610989 ) ) ;
#55902 = CARTESIAN_POINT ( 'NONE',  ( 0.000000000000000000, -0.02379966007286238305, 0.000000000000000000 ) ) ;
#55904 = CARTESIAN_POINT ( 'NONE',  ( 0.6823417656249934904, 10.94270833367473550, 1.181850606188764807 ) ) ;
#55903 = CARTESIAN_POINT ( 'NONE',  ( 0.2864612384333536932, -1.063250325806489149, 1.997138572869002537 ) ) ;
#55905 = CARTESIAN_POINT ( 'NONE',  ( -7.160677686311960777, 11.50587440067263678, -0.7998128361456291469 ) ) ;
#55907 = CARTESIAN_POINT ( 'NONE',  ( 1.511203358410578179, -1.803099835331838818, 0.6471475864035965975 ) ) ;
#55906 = CARTESIAN_POINT ( 'NONE',  ( -4.731432421044873493, 7.503459676985569260, -1.082531754730548412 ) ) ;
#55908 = CARTESIAN_POINT ( 'NONE',  ( -0.6823417656250212460, 2.613541667008084879, 1.181850606188767472 ) ) ;
#55909 = CARTESIAN_POINT ( 'NONE',  ( 0.7499999999999920064, 4.483333333333352932, 1.299038105676669330 ) ) ;
#55910 = CARTESIAN_POINT ( 'NONE',  ( -1.500000000000001110, 9.520833333333333925, 0.8660254037844419273 ) ) ;
#55911 = CARTESIAN_POINT ( 'NONE',  ( 2.859633459980165160, 1.716568739768107532, -0.1690650336269062803 ) ) ;
#55912 = CARTESIAN_POINT ( 'NONE',  ( 5.903649544107831382, 5.852288987739402870, -0.7998128361456481317 ) ) ;
#55913 = CARTESIAN_POINT ( 'NONE',  ( 2.248939020346378381, -1.418119551073221851, -1.058484587410456701 ) ) ;
#55914 = CARTESIAN_POINT ( 'NONE',  ( 2.508449741805112154, -2.007837557984166299, -0.1460343770829114485 ) ) ;
#55915 = CARTESIAN_POINT ( 'NONE',  ( 10.58621901417202515, 11.24501035948919991, -0.7998128361456281477 ) ) ;
#55916 = CARTESIAN_POINT ( 'NONE',  ( 5.034293675167554660, 1.138177661764948834, -1.890478833441497031 ) ) ;
#55917 = EDGE_LOOP ( 'NONE', ( #26101, #203870, #112865 ) ) ;
#55918 = CARTESIAN_POINT ( 'NONE',  ( 4.711197416960428264, 1.676919581237258372, -1.125501318796730876 ) ) ;
#55919 = CARTESIAN_POINT ( 'NONE',  ( -7.910256278930404505, 8.193330178365746619, -0.7998128361456362523 ) ) ;
#55921 = CARTESIAN_POINT ( 'NONE',  ( 3.726185550002871327, 2.006962945745351945, 0.1948219989877792713 ) ) ;
#55920 = CARTESIAN_POINT ( 'NONE',  ( 4.828832153679845973, 1.461785933843419150, -1.536352341152541046 ) ) ;
#55923 = ORIENTED_EDGE ( 'NONE', *, *, #161480, .T. ) ;
#55922 = CARTESIAN_POINT ( 'NONE',  ( 4.236430684147264536, 1.109505083903281619, -1.432011362939947574 ) ) ;
#55924 = B_SPLINE_CURVE_WITH_KNOTS ( 'NONE', 3,
 ( #27509, #195356, #113104, #14443, #11251, #77329 ),
 .UNSPECIFIED., .F., .F.,
 ( 4, 2, 4 ),
 ( 0.000000000000000000, 0.0003258677429877275783, 0.0006517354859754551566 ),
 .UNSPECIFIED. ) ;
#55925 = CARTESIAN_POINT ( 'NONE',  ( 4.603875680292229156, 7.528882839386387360, 1.199719254218452047 ) ) ;
#55926 = EDGE_LOOP ( 'NONE', ( #139321, #78127, #71442, #3600 ) ) ;
#55927 = ADVANCED_FACE ( 'NONE', ( #156580, #90515, #171743, #86230, #23340, #8173, #155502, #74257 ), #53733, .F. ) ;
#55928 = CARTESIAN_POINT ( 'NONE',  ( 1.270139834521961886, -1.189467451172643964, 1.443775233441677130 ) ) ;
#55929 = AXIS2_PLACEMENT_3D ( 'NONE', #25266, #175810, #131106 ) ;
#55930 = CARTESIAN_POINT ( 'NONE',  ( -10.91805698906626887, -9.914767083041231999, 0.1897524941850696201 ) ) ;
#55931 = CARTESIAN_POINT ( 'NONE',  ( 6.094382945298186804, -0.9628849012233617888, 1.534170072110131899 ) ) ;
#55932 = CARTESIAN_POINT ( 'NONE',  ( -3.440018289565379028, 5.036440642624797626, 1.599625672291267398 ) ) ;
#55933 = CARTESIAN_POINT ( 'NONE',  ( -11.66942904513850543, 4.336835040752899495, -5.185078083676367910 ) ) ;
#55934 = CARTESIAN_POINT ( 'NONE',  ( 3.834746474454188013E-15, 8.593750000682796042, 1.500000000000001554 ) ) ;
#55935 = CARTESIAN_POINT ( 'NONE',  ( 1.364683531249986537, 2.467708333674753174, -0.7879004041258239610 ) ) ;
#55936 = CARTESIAN_POINT ( 'NONE',  ( 2.467126471220339567, 3.603011019375355062, -11.63837686854860998 ) ) ;
#55937 = ORIENTED_EDGE ( 'NONE', *, *, #167677, .T. ) ;
#55938 = CARTESIAN_POINT ( 'NONE',  ( 4.206267736153862735, 1.236801365491456028, -1.592660703826812352 ) ) ;
#55939 = CARTESIAN_POINT ( 'NONE',  ( 6.048345925472178308, 9.110135108809304327, 1.082531754730549967 ) ) ;
#55940 = CARTESIAN_POINT ( 'NONE',  ( -2.875737979874388284, 6.369128386579808954, -0.7216878364870458196 ) ) ;
#55941 = CARTESIAN_POINT ( 'NONE',  ( -6.961185525973791144, 7.086080966583015339, 0.7998128361456341429 ) ) ;
#55942 = CARTESIAN_POINT ( 'NONE',  ( 4.623349522974431025, 1.846400237221163865, 1.042759738753673338 ) ) ;
#55944 = CARTESIAN_POINT ( 'NONE',  ( -10.45911201557330195, 5.175391108250987138, -5.201428006079835242 ) ) ;
#55943 = CARTESIAN_POINT ( 'NONE',  ( -5.808742468812186033, 5.741564066561132940, 0.000000000000000000 ) ) ;
#55945 = CARTESIAN_POINT ( 'NONE',  ( 5.975845355540164938, 1.172130763738386650, 1.584922449839619052 ) ) ;
#55946 = CARTESIAN_POINT ( 'NONE',  ( 1.364683531249988757, 0.6343750003414208027, 0.000000000000000000 ) ) ;
#55947 = CARTESIAN_POINT ( 'NONE',  ( 0.4572897223803442102, -1.724499148370229218, 1.038616540587710357 ) ) ;
#55948 = ORIENTED_EDGE ( 'NONE', *, *, #115096, .F. ) ;
#55949 = CARTESIAN_POINT ( 'NONE',  ( 0.4744016597374626221, -2.101792896462660210, -0.2546084012580717704 ) ) ;
#55950 = CARTESIAN_POINT ( 'NONE',  ( 8.989385892795640487, 12.33334389077627335, 7.952349317847390076 ) ) ;
#55951 = CARTESIAN_POINT ( 'NONE',  ( 1.381394743813993964, -0.05274132383669553892, 2.069866178704109938 ) ) ;
#55952 = ORIENTED_EDGE ( 'NONE', *, *, #119448, .F. ) ;
#55953 = CARTESIAN_POINT ( 'NONE',  ( 4.529305835417093640, 7.441884687032027657, -1.199719254218450271 ) ) ;
#55954 = CARTESIAN_POINT ( 'NONE',  ( 5.061990249855835344, 6.999017606288844284, -1.599625672291273171 ) ) ;
#55956 = CARTESIAN_POINT ( 'NONE',  ( 5.087333953625774008, 6.958308917361963886, 1.599625672291267398 ) ) ;
#55955 = CARTESIAN_POINT ( 'NONE',  ( 4.927721519287828755, 1.075078395752477878, -1.792878403059654513 ) ) ;
#55957 = CARTESIAN_POINT ( 'NONE',  ( 7.212011367826596242, 7.378711115411311638, 0.000000000000000000 ) ) ;
#55960 = ORIENTED_EDGE ( 'NONE', *, *, #106666, .F. ) ;
#55959 = CARTESIAN_POINT ( 'NONE',  ( 1.242487904981701252, 1.745646600027310980, 0.4836494453460266074 ) ) ;
#55958 = CARTESIAN_POINT ( 'NONE',  ( 2.801551268311212262, -0.5745519774189576934, 1.732868645247707562 ) ) ;
#55961 = CARTESIAN_POINT ( 'NONE',  ( 10.70146331988817323, 11.37946204949139251, 0.7998128361456341429 ) ) ;
#55962 = LINE ( 'NONE', #57031, #95710 ) ;
#55963 = CIRCLE ( 'NONE', #183974, 0.04999999999999969746 ) ;
#55964 = CARTESIAN_POINT ( 'NONE',  ( 3.909358855915114006, 1.891329263188616938, 1.136761501516952766 ) ) ;
#55965 = CARTESIAN_POINT ( 'NONE',  ( 7.609150525767641504, 9.900428251527500834, -1.599625672291262513 ) ) ;
#55966 = CARTESIAN_POINT ( 'NONE',  ( 1.364683531249996529, 9.026041667008060543, 0.7879004041258403923 ) ) ;
#55967 = CARTESIAN_POINT ( 'NONE',  ( 3.123589223026546957, -0.3706944625661895976, 1.875830702792554483 ) ) ;
#55968 = CARTESIAN_POINT ( 'NONE',  ( 8.932124273304774320, 9.315233161810734686, 0.7998128361456462443 ) ) ;
#55969 = CARTESIAN_POINT ( 'NONE',  ( 6.021949436824264978, 2.040384406434097464, -0.3501103912618847014 ) ) ;
#55970 = CARTESIAN_POINT ( 'NONE',  ( 1.360316468749989571, 0.8177083336747339448, -0.7853790794159001276 ) ) ;
#55971 = CARTESIAN_POINT ( 'NONE',  ( 5.407841436338867602, -0.9846607899807978681, -1.957994596084790206 ) ) ;
#55972 = CARTESIAN_POINT ( 'NONE',  ( 6.038137670975392446, 7.156622065392123311, -1.170913047369964710 ) ) ;
#55973 = CARTESIAN_POINT ( 'NONE',  ( -9.367496997192910513, 15.46908218390266043, -7.500000000505454345 ) ) ;
#55974 = ORIENTED_EDGE ( 'NONE', *, *, #98818, .T. ) ;
#55975 = AXIS2_PLACEMENT_3D ( 'NONE', #9350, #89556, #75422 ) ;
#55976 = CARTESIAN_POINT ( 'NONE',  ( 1.237941840314000785, -1.374772708486730943, 1.500000000000001332 ) ) ;
#55977 = CARTESIAN_POINT ( 'NONE',  ( 4.923546060418115822, 5.773167154356443120, -1.199719254218452047 ) ) ;
#55978 = CARTESIAN_POINT ( 'NONE',  ( 3.285556943750000070, -1.771874999522041083, 0.000000000000000000 ) ) ;
#55979 = CARTESIAN_POINT ( 'NONE',  ( -0.2409995289980038091, -0.004801160710915519658, -2.000252362011435636 ) ) ;
#55980 = CARTESIAN_POINT ( 'NONE',  ( -7.212574532790100079, 9.437756259720353924, -1.443375672974059665 ) ) ;
#55981 = CARTESIAN_POINT ( 'NONE',  ( 4.085803189671889157, 5.860132702740892263, -1.599625672291273171 ) ) ;
#55982 = CARTESIAN_POINT ( 'NONE',  ( 5.594608825991118195, 2.038665915018455177, 0.3594684214384344378 ) ) ;
#55983 = ADVANCED_FACE ( 'NONE', ( #11364 ), #4642, .F. ) ;
#55984 = CARTESIAN_POINT ( 'NONE',  ( 1.124625310196948558, 0.3961260723950796314, 1.976952190469769111 ) ) ;
#55985 = CARTESIAN_POINT ( 'NONE',  ( -9.134442807305063639, 11.67993591332117376, 1.599625672291281386 ) ) ;
#55986 = CARTESIAN_POINT ( 'NONE',  ( 6.535912570239620578, 9.782925877658371405, 1.199719254218452047 ) ) ;
#55987 = CARTESIAN_POINT ( 'NONE',  ( 2.231648340698067834, 5.547414130882294181, -0.2706067644340047207 ) ) ;
#55988 = CARTESIAN_POINT ( 'NONE',  ( 1.711130781365449716, -0.2659051965858104660, 2.175189728913041964 ) ) ;
#55989 = CARTESIAN_POINT ( 'NONE',  ( 5.426323838365305186, 1.084245000580752238, -1.468710674947353745 ) ) ;
#55990 = CARTESIAN_POINT ( 'NONE',  ( -3.750802052474980108, 7.527686161196117887, 1.040834085586084257E-14 ) ) ;
#55991 = CARTESIAN_POINT ( 'NONE',  ( 4.407809338218622308, 8.156544971314787063, 0.000000000000000000 ) ) ;
#55992 = CARTESIAN_POINT ( 'NONE',  ( 9.748476143425788720, 11.33197590787365172, -1.199719254218440723 ) ) ;
#55993 = CARTESIAN_POINT ( 'NONE',  ( -4.630991987519598396, 7.560518531151607213, 1.199719254218452935 ) ) ;
#55994 = CARTESIAN_POINT ( 'NONE',  ( 3.832150974156964818, 7.622593236491780999, 1.040834085586084257E-14 ) ) ;
#55995 = CARTESIAN_POINT ( 'NONE',  ( 3.217027588192558074, 6.975225629525113824, -1.734723475976807094E-15 ) ) ;
#55996 = EDGE_LOOP ( 'NONE', ( #71832, #195603, #174526, #86847 ) ) ;
#55998 = CARTESIAN_POINT ( 'NONE',  ( 6.504166875733549347, -0.8557802559411722410, 1.820156917002911712 ) ) ;
#55997 = CARTESIAN_POINT ( 'NONE',  ( 2.735704033801298785, 1.827604811068459956, 0.2230458208379028362 ) ) ;
#55999 = CARTESIAN_POINT ( 'NONE',  ( 1.511505665106587459, 2.295766583369537095, 0.1122837871174054425 ) ) ;
#56001 = CARTESIAN_POINT ( 'NONE',  ( 6.825062041929172985, -1.792332737533608666, -0.7979697884207545000 ) ) ;
#56000 = CARTESIAN_POINT ( 'NONE',  ( 4.039966587192259873, 5.736380323189513852, 1.443375672974062551 ) ) ;
#56002 = CARTESIAN_POINT ( 'NONE',  ( -4.985647801523292344, 6.839675073242382553, -1.599625672291256295 ) ) ;
#56003 = CARTESIAN_POINT ( 'NONE',  ( 0.3713344243775092424, 2.999999999999998668, -0.3713344243776030007 ) ) ;
#56004 = CARTESIAN_POINT ( 'NONE',  ( 3.146637304467227558, 1.866760668956708447, 0.4145885930168375921 ) ) ;
#56005 = CARTESIAN_POINT ( 'NONE',  ( -9.134442807305063639, 11.67993591332117376, 1.599625672291281386 ) ) ;
#56006 = CARTESIAN_POINT ( 'NONE',  ( 0.6782873735513493818, -1.106163567672680204, -1.749894625276714688 ) ) ;
#56007 = CARTESIAN_POINT ( 'NONE',  ( -7.783789588021474692, 8.253711738879413673, 0.7216878364870317197 ) ) ;
#56009 = CARTESIAN_POINT ( 'NONE',  ( 0.6900581440293825919, -1.856003987442723657, -0.2331820809091043056 ) ) ;
#56008 = CARTESIAN_POINT ( 'NONE',  ( 2.173483749353939842, 1.288726691912587041, 1.646222326975780526 ) ) ;
#56010 = CARTESIAN_POINT ( 'NONE',  ( 2.073592080879012478, 1.495823877299466087, -1.351946161731142126 ) ) ;
#56011 = CARTESIAN_POINT ( 'NONE',  ( 8.270110514656026979, 10.67154823856396817, 1.443375672974076540 ) ) ;
#56012 = CARTESIAN_POINT ( 'NONE',  ( -0.6823417656250212460, 4.363541667008085767, 1.181850606188767472 ) ) ;
#56013 = CARTESIAN_POINT ( 'NONE',  ( 2.682838027602444164, 1.232319236757819292, 1.229298679657732762 ) ) ;
#56014 = CARTESIAN_POINT ( 'NONE',  ( 4.955668840994886359, 5.740367388370866131, 1.199719254218462483 ) ) ;
#56016 = CARTESIAN_POINT ( 'NONE',  ( 0.1250758119425495474, 3.478658522888401716, -1.998845934954712966 ) ) ;
#56015 = CARTESIAN_POINT ( 'NONE',  ( -0.5000000000000056621, 3.172938907704293765, -0.4000000000000305533 ) ) ;
#56017 = CARTESIAN_POINT ( 'NONE',  ( 2.947548438991169473, 0.6205982292267105960, -1.609554129922322163 ) ) ;
#56018 = CARTESIAN_POINT ( 'NONE',  ( 3.316156725143477146, 1.388770557483296697, -1.695381604771596606 ) ) ;
#56019 = CARTESIAN_POINT ( 'NONE',  ( 5.162800556355915838, -1.600310254184673431, 1.519886962452212664 ) ) ;
#56020 = CARTESIAN_POINT ( 'NONE',  ( -9.912197829101469182, 5.385002637010017246, -6.113573717307969169 ) ) ;
#56021 = VECTOR ( 'NONE', #124616, 1000.000000000000000 ) ;
#56022 = CARTESIAN_POINT ( 'NONE',  ( 3.204148022151423802, 0.7856563700287253482, -2.024084340642897661 ) ) ;
#56023 = CARTESIAN_POINT ( 'NONE',  ( 2.701551412915685457, -0.5726843992823158480, 1.733614832724015731 ) ) ;
#56024 = LINE ( 'NONE', #185998, #176593 ) ;
#56025 = CARTESIAN_POINT ( 'NONE',  ( 4.153586450535729391, 2.052860580235102095, -0.5180077198428371110 ) ) ;
#56026 = TOROIDAL_SURFACE ( 'NONE', #627, 0.4800000000000000933, 0.08000000000000000167 ) ;
#56027 = CARTESIAN_POINT ( 'NONE',  ( 6.639320575229290533, 2.050619746573784763, 2.302922995531462291 ) ) ;
#56028 = ORIENTED_EDGE ( 'NONE', *, *, #167754, .F. ) ;
#56030 = CARTESIAN_POINT ( 'NONE',  ( -1.364683531250014514, 2.051041667008086655, -0.7879004041258289570 ) ) ;
#56029 = CARTESIAN_POINT ( 'NONE',  ( 4.441175045773351648, -1.771670475836329306, -1.454733398674179945 ) ) ;
#56031 = CARTESIAN_POINT ( 'NONE',  ( 11.89942855770814312, 13.88000000000000078, -0.7000000000000009548 ) ) ;
#56032 = CARTESIAN_POINT ( 'NONE',  ( 8.757677159423465696, 12.30470822171437284, 1.199719254218450271 ) ) ;
#56033 = CARTESIAN_POINT ( 'NONE',  ( -0.05774110376318035420, -1.308430771297010908, -1.669371405835825550 ) ) ;
#56034 = CARTESIAN_POINT ( 'NONE',  ( -5.097502569058210753, 7.930541516334467467, -1.082531754730549967 ) ) ;
#56035 = CARTESIAN_POINT ( 'NONE',  ( 4.867013957625893283, 4.780530493426062399, 1.040834085586084257E-14 ) ) ;
#56036 = CARTESIAN_POINT ( 'NONE',  ( -6.683806541412780078, 6.900121841177441873, -0.7216878364870267237 ) ) ;
#56037 = CARTESIAN_POINT ( 'NONE',  ( -11.09999999999959996, -2.077690541055267462E-15, -0.2598076211376263434 ) ) ;
#56038 = VERTEX_POINT ( 'NONE', #178161 ) ;
#56039 = CARTESIAN_POINT ( 'NONE',  ( 5.432267593368638181, -1.591316862017605471, -1.238322901282742805 ) ) ;
#56041 = CARTESIAN_POINT ( 'NONE',  ( 3.661030488878083577, 1.629037084659604728, -1.265030972029494993 ) ) ;
#56040 = CARTESIAN_POINT ( 'NONE',  ( 5.335297142177534369, 6.183267073083954735, -1.199719254218452047 ) ) ;
#56043 = CARTESIAN_POINT ( 'NONE',  ( -0.2409995289980038091, 6.947781193150415646, -2.595509233728268583 ) ) ;
#56042 = CARTESIAN_POINT ( 'NONE',  ( 8.167861197590044142, 8.493869250135347215, 0.000000000000000000 ) ) ;
#56044 = CARTESIAN_POINT ( 'NONE',  ( 6.119526231721748033, 8.232809585132461194, 1.599625672291269396 ) ) ;
#56045 = CARTESIAN_POINT ( 'NONE',  ( -1.642778471875000035, -1.567708332855376252, -2.845375778867859751 ) ) ;
#56046 = PRESENTATION_STYLE_ASSIGNMENT (( #205478 ) ) ;
#56047 = CARTESIAN_POINT ( 'NONE',  ( 6.714806894218784628, -0.1628439675423892508, 2.155775914164249407 ) ) ;
#56048 = CARTESIAN_POINT ( 'NONE',  ( 3.797500137148449362, 1.423962148579031917, -1.427936706820939872 ) ) ;
#56049 = CARTESIAN_POINT ( 'NONE',  ( 3.755264181858387840, 1.826884192416846631, -0.2291247506851084581 ) ) ;
#56050 = CARTESIAN_POINT ( 'NONE',  ( 6.494519276145969577, 7.535692896047149425, -1.199719254218446718 ) ) ;
#56051 = CARTESIAN_POINT ( 'NONE',  ( 0.3227381541650706787, -0.09231566880639123507, 1.722440863776145692 ) ) ;
#56052 = CARTESIAN_POINT ( 'NONE',  ( -5.204170427930421283E-15, -5.907420853759282053, 10.91970695577496997 ) ) ;
#56053 = CARTESIAN_POINT ( 'NONE',  ( 0.4582085974003520801, -2.167260061518965664, -0.7665384626166712456 ) ) ;
#56054 = CARTESIAN_POINT ( 'NONE',  ( -6.795661308947694934, 8.951357498570873261, -1.599625672291263179 ) ) ;
#56055 = CARTESIAN_POINT ( 'NONE',  ( 0.2634263733268344398, -2.021796075192600295, -1.015562799429880814 ) ) ;
#56056 = CARTESIAN_POINT ( 'NONE',  ( 2.543703448412675261, -1.561038821359970408, -1.413940773279374508 ) ) ;
#56057 = CARTESIAN_POINT ( 'NONE',  ( -5.641074431737709283, 8.738948049406083385, -1.199719254218452047 ) ) ;
#56058 = CARTESIAN_POINT ( 'NONE',  ( 8.599949509769960088, 8.927695937686774386, 1.040834085586084257E-14 ) ) ;
#56059 = CARTESIAN_POINT ( 'NONE',  ( 7.173672674962134899, 7.541908673643526129, -0.7216878364870317197 ) ) ;
#56061 = EDGE_CURVE ( 'NONE', #113311, #7325, #171956, .T. ) ;
#56060 = CARTESIAN_POINT ( 'NONE',  ( -5.201524489137236529, 9.220195670635433771, 0.7998128361456481317 ) ) ;
#56062 = CARTESIAN_POINT ( 'NONE',  ( 6.358410854684775515, 8.441231968597481483, -1.443375672974058777 ) ) ;
#56063 = CARTESIAN_POINT ( 'NONE',  ( 5.274334856052985465, 6.586744271544701768, 1.367809967355391398 ) ) ;
#56064 = CARTESIAN_POINT ( 'NONE',  ( -3.978428010606240850, 6.728917548094202949, -1.199719254218452047 ) ) ;
#56066 = CARTESIAN_POINT ( 'NONE',  ( 3.410577425615939795, -2.218986280728425076, -0.1058077642441344057 ) ) ;
#56065 = CARTESIAN_POINT ( 'NONE',  ( 2.320699612028754188, -0.8158636990020677882, -1.957571985684476212 ) ) ;
#56067 = CARTESIAN_POINT ( 'NONE',  ( 2.537292984272555785, -1.624655320356691801, -1.470880813658273389 ) ) ;
#56068 = CARTESIAN_POINT ( 'NONE',  ( -5.930802130974132780, 9.006687355190106103, -1.199719254218440723 ) ) ;
#56069 = AXIS2_PLACEMENT_3D ( 'NONE', #8511, #77777, #173176 ) ;
#56070 = CARTESIAN_POINT ( 'NONE',  ( 6.883263157960366030, 3.696842586722657309, 2.460469087180996883 ) ) ;
#56071 = CARTESIAN_POINT ( 'NONE',  ( -4.125423880308188629, 8.035021303660014880, -0.7998128361456481317 ) ) ;
#56072 = CARTESIAN_POINT ( 'NONE',  ( 5.670351692713981429, -0.8806477319739226539, -1.753155087565357428 ) ) ;
#56073 = CARTESIAN_POINT ( 'NONE',  ( 4.081882008079450230, 3.980588341361369853, -0.7346435760097060896 ) ) ;
#56074 = CARTESIAN_POINT ( 'NONE',  ( -1.364683531250012516, 1.280208333674755172, 0.7879004041258379498 ) ) ;
#56075 = CARTESIAN_POINT ( 'NONE',  ( -4.340018570150318666, 6.156717313299049366, -1.443375672974066548 ) ) ;
#56076 = CARTESIAN_POINT ( 'NONE',  ( -5.260200412422196159, 9.080724881227137502, -0.7216878364870207285 ) ) ;
#56077 = CARTESIAN_POINT ( 'NONE',  ( 4.148766697842418694, 2.080301416381886703, 0.4105806053946169376 ) ) ;
#56078 = CARTESIAN_POINT ( 'NONE',  ( -2.959422669532919326, 6.674686557755516780, 0.7998128361456352531 ) ) ;
#56079 = ORIENTED_EDGE ( 'NONE', *, *, #87069, .F. ) ;
#56080 = CARTESIAN_POINT ( 'NONE',  ( 5.014612968065254250, 1.493337269798940881, -1.563205770552501761 ) ) ;
#56081 = CARTESIAN_POINT ( 'NONE',  ( 6.667912619822566000, 6.673652899414787676, 1.040834085586084257E-14 ) ) ;
#56082 = CARTESIAN_POINT ( 'NONE',  ( 4.634224865634020141, 0.3196297827482602605, 1.813140464320086354 ) ) ;
#56083 = CARTESIAN_POINT ( 'NONE',  ( -5.910693218230258061, 6.000975156485434781, -0.07073762994192281384 ) ) ;
#56084 = CARTESIAN_POINT ( 'NONE',  ( -0.6823417656250003738, 1.780208333674752952, -1.181850606188749264 ) ) ;
#56085 = CARTESIAN_POINT ( 'NONE',  ( 6.632745071352946553, -1.550850273991890127, 0.7898216520882040959 ) ) ;
#56086 = CARTESIAN_POINT ( 'NONE',  ( 6.827182134110172385, 0.001020705822878456353, 1.910856149448317165 ) ) ;
#56087 = CARTESIAN_POINT ( 'NONE',  ( -0.5631007116328591300, 7.823254984196720940, 1.919102855466193303 ) ) ;
#56088 = DIRECTION ( 'NONE',  ( -0.9999980456341537316, 0.000000000000000000, -0.001977050295949902767 ) ) ;
#56089 = CARTESIAN_POINT ( 'NONE',  ( 4.100566281481184738, -0.6756360485904688851, -2.053482476349233643 ) ) ;
#56090 = CARTESIAN_POINT ( 'NONE',  ( -3.924195396151603177, 6.665646164563756138, 1.199719254218464037 ) ) ;
#56091 = CIRCLE ( 'NONE', #173771, 0.1000000000000000472 ) ;
#56092 = CARTESIAN_POINT ( 'NONE',  ( -8.663296969008007054, 9.209527340038563992, 0.7216878364870438212 ) ) ;
#56093 = CARTESIAN_POINT ( 'NONE',  ( 3.555696680978126079, 0.5271953485486252644, -2.096301903996622862 ) ) ;
#56094 = CARTESIAN_POINT ( 'NONE',  ( 4.762937738300905721, -1.759534068222264436, -0.8891730789123506451 ) ) ;
#56095 = CARTESIAN_POINT ( 'NONE',  ( 4.323420094722703944, -1.284794005617446278, 1.164475704859231131 ) ) ;
#56096 = CARTESIAN_POINT ( 'NONE',  ( 0.3280006606478855224, 1.121390616443746602, -1.882787531365101685 ) ) ;
#56097 = CARTESIAN_POINT ( 'NONE',  ( 0.8335961714901140018, 0.1734020439737720132, 2.301109984577158762 ) ) ;
#56098 = CARTESIAN_POINT ( 'NONE',  ( 3.936836037902153418, 0.2985264485904081111, 2.038899620686930536 ) ) ;
#56099 = CARTESIAN_POINT ( 'NONE',  ( 5.864781425808283544, 0.1387459415673809593, -1.937151248970377271 ) ) ;
#56100 = CARTESIAN_POINT ( 'NONE',  ( -8.310784975052685652, 9.758632561392040827, -1.082531754730543083 ) ) ;
#56101 = CARTESIAN_POINT ( 'NONE',  ( -6.303615075710993665, 6.318915441276411471, -0.7998128361456362523 ) ) ;
#56102 = CARTESIAN_POINT ( 'NONE',  ( 0.000000000000000000, 0.000000000000000000, 0.000000000000000000 ) ) ;
#56104 = EDGE_LOOP ( 'NONE', ( #124913, #213896, #180129, #23233 ) ) ;
#56103 = CARTESIAN_POINT ( 'NONE',  ( 1.409462824231155764E-15, 2.018041202053853400, -12.16970660573436014 ) ) ;
#56105 = CARTESIAN_POINT ( 'NONE',  ( -6.033015167956794933, 9.982342096017511324, -0.7216878364870267237 ) ) ;
#56106 = CARTESIAN_POINT ( 'NONE',  ( 3.135963548190400019, -1.480894843444351849, -1.636267651353009223 ) ) ;
#56107 = CARTESIAN_POINT ( 'NONE',  ( -1.642778471875000035, -3.405208332855375275, -2.845375778867859751 ) ) ;
#56108 = ORIENTED_EDGE ( 'NONE', *, *, #44491, .F. ) ;
#56109 = CARTESIAN_POINT ( 'NONE',  ( 0.3208626164478335374, -1.658663274457260473, -0.8439677346868018626 ) ) ;
#56110 = CARTESIAN_POINT ( 'NONE',  ( -0.02919842301642854021, 4.085261895051949921, -2.628472738367752637 ) ) ;
#56111 = CARTESIAN_POINT ( 'NONE',  ( -1.500000000000011324, 5.202083334016151639, 0.8660254037844403729 ) ) ;
#56112 = CARTESIAN_POINT ( 'NONE',  ( 4.470816497852414528, 7.277750640693428252, -1.251308411505752671 ) ) ;
#56114 = CARTESIAN_POINT ( 'NONE',  ( 6.620655732516646630, 0.01042156863438315970, 1.726407961933307700 ) ) ;
#56113 = DIRECTION ( 'NONE',  ( 1.000000000000000000, 0.000000000000000000, 0.000000000000000000 ) ) ;
#56115 = CARTESIAN_POINT ( 'NONE',  ( 6.650350966976619205, -1.419654684173769166, 1.172063944840713523 ) ) ;
#56116 = VERTEX_POINT ( 'NONE', #141432 ) ;
#56117 = CARTESIAN_POINT ( 'NONE',  ( 1.956002958106726419, 2.055451868484101219, -0.1503645474096800549 ) ) ;
#56118 = CARTESIAN_POINT ( 'NONE',  ( -0.6801582343750022241, -0.1510416663252633906, -1.178068619123841643 ) ) ;
#56119 = CARTESIAN_POINT ( 'NONE',  ( -5.910464900553636269, 8.982960586366182554, -1.199719254218440723 ) ) ;
#56120 = CARTESIAN_POINT ( 'NONE',  ( 0.07680821025391608436, 6.948789780205374633, -2.405840108717867132 ) ) ;
#56121 = CARTESIAN_POINT ( 'NONE',  ( 3.876741858503734761, 6.610283703974623393, 1.199719254218462483 ) ) ;
#56122 = CARTESIAN_POINT ( 'NONE',  ( 1.059529560858112340, 0.4028119719261863962, -2.020956803572224736 ) ) ;
#56124 = CARTESIAN_POINT ( 'NONE',  ( 5.319803798718575116, 1.092037692397327620, -1.482314076171886708 ) ) ;
#56123 = CARTESIAN_POINT ( 'NONE',  ( -4.036671995544492297, 7.285761072467114019, 0.7944190476826870073 ) ) ;
#56125 = CARTESIAN_POINT ( 'NONE',  ( 4.957477724091233995, 8.935474444748447098, -0.7998128361456281477 ) ) ;
#56126 = CARTESIAN_POINT ( 'NONE',  ( -4.685224601974262271, 7.623789914682047808, -1.199719254218453823 ) ) ;
#56127 = SURFACE_SIDE_STYLE ('',( #5201 ) ) ;
#56128 = CARTESIAN_POINT ( 'NONE',  ( 4.037865812933420173, -1.521084700717803884, -1.599171214764223636 ) ) ;
#56129 = CARTESIAN_POINT ( 'NONE',  ( 0.8784639925019833706, -1.201575844224999301, 1.796657101444132154 ) ) ;
#56130 = CARTESIAN_POINT ( 'NONE',  ( -3.606105671554953318, 7.150947683548662503, 0.7216878364870317197 ) ) ;
#56131 = CARTESIAN_POINT ( 'NONE',  ( 6.539320575229251808, 0.01001626003939220556, 1.796977979958065852 ) ) ;
#56132 = CARTESIAN_POINT ( 'NONE',  ( 1.094935803221647186, 1.780670018850015079, 0.9462964651613046119 ) ) ;
#56133 = CARTESIAN_POINT ( 'NONE',  ( 7.661766205054107992, 8.111351125417501251, -0.7216878364870317197 ) ) ;
#56134 = DIRECTION ( 'NONE',  ( 0.000000000000000000, 0.000000000000000000, 1.000000000000000000 ) ) ;
#56135 = CARTESIAN_POINT ( 'NONE',  ( 6.270165159132718102, 1.906809857242173223, -0.1455798257045255450 ) ) ;
#56136 = SURFACE_SIDE_STYLE ('',( #142760 ) ) ;
#56137 = CARTESIAN_POINT ( 'NONE',  ( 1.779943879855113709, -1.003247456797161652, 1.578688272967261996 ) ) ;
#56138 = CARTESIAN_POINT ( 'NONE',  ( 2.940638933469359895, -1.523795050681177710, 1.320827213682006285 ) ) ;
#56140 = CARTESIAN_POINT ( 'NONE',  ( 11.78331023100045627, 12.21999999999998288, 1.799999999999999600 ) ) ;
#56139 = CARTESIAN_POINT ( 'NONE',  ( 1.364683531249986537, 0.4052083336747511200, -0.7879004041258309554 ) ) ;
#56142 = CARTESIAN_POINT ( 'NONE',  ( 5.584633104594088238, -2.054432100182907561, -0.4627632117069883089 ) ) ;
#56141 = CARTESIAN_POINT ( 'NONE',  ( -9.677822722056413696, 10.18521468535430685, 1.040834085586084257E-14 ) ) ;
#56143 = CARTESIAN_POINT ( 'NONE',  ( 7.313733799568044702, 10.62010763521636214, 1.199719254218460707 ) ) ;
#56145 = CARTESIAN_POINT ( 'NONE',  ( -8.148614017013223076, 9.465470093725620870, -1.199719254218446718 ) ) ;
#56144 = CARTESIAN_POINT ( 'NONE',  ( 5.061990249855835344, 6.999017606288844284, -1.599625672291273171 ) ) ;
#56146 = CARTESIAN_POINT ( 'NONE',  ( -0.01424860406280193531, -7.025535116234850719, -9.597801448745755692 ) ) ;
#56147 = CARTESIAN_POINT ( 'NONE',  ( 4.201429114599513959, 1.802380596022877368, -0.9117778440167979559 ) ) ;
#56148 = CARTESIAN_POINT ( 'NONE',  ( -1.364683531250010295, 4.780208333674755394, 0.7879004041258379498 ) ) ;
#56149 = CARTESIAN_POINT ( 'NONE',  ( 6.689892334039674537, -1.344252178338888992, -1.564594595144116695 ) ) ;
#56150 = CARTESIAN_POINT ( 'NONE',  ( 9.788623719386617239, 11.48277776311499387, -1.082531754730537088 ) ) ;
#56151 = CARTESIAN_POINT ( 'NONE',  ( 4.165412764819938829, 0.2691229397190370576, -2.144731622849817221 ) ) ;
#56152 = CARTESIAN_POINT ( 'NONE',  ( 5.352436782344940802, 9.466536356036257871, 0.000000000000000000 ) ) ;
#56153 = CARTESIAN_POINT ( 'NONE',  ( -1.402160292154681736E-14, -1.115624999658584082, 1.575800808251672791 ) ) ;
#56154 = CARTESIAN_POINT ( 'NONE',  ( 4.857564175446106525, 8.889184981320973122, 0.7998128361456331437 ) ) ;
#56155 = CARTESIAN_POINT ( 'NONE',  ( 7.090551149822735155, 9.295395646258437949, 1.443375672974076540 ) ) ;
#56157 = CARTESIAN_POINT ( 'NONE',  ( 1.123270288250308280, 2.922697346350005887, 0.7749999999993786304 ) ) ;
#56156 = CARTESIAN_POINT ( 'NONE',  ( 2.049520782779357120, 1.889653518395111753, -1.069053457954100006 ) ) ;
#56159 = CARTESIAN_POINT ( 'NONE',  ( 1.399689850468607277, -0.6632477835330424787, -1.717811453623831808 ) ) ;
#56158 = CARTESIAN_POINT ( 'NONE',  ( -5.585596099150193616, 6.579245539505756746, -1.082531754730544860 ) ) ;
#56160 = CARTESIAN_POINT ( 'NONE',  ( -0.6823417656250212460, 2.801041667008084879, 1.181850606188767472 ) ) ;
#56161 = CARTESIAN_POINT ( 'NONE',  ( 2.718528139169604341, 2.064530135181973591, 0.7356957861901700646 ) ) ;
#56162 = CARTESIAN_POINT ( 'NONE',  ( 3.643696890507712283, -1.711652922788420739, -1.479685619365896265 ) ) ;
#56163 = CARTESIAN_POINT ( 'NONE',  ( -6.905180308061733996, 6.950465202360470052, 0.7998128361456341429 ) ) ;
#56164 = CARTESIAN_POINT ( 'NONE',  ( 0.000000000000000000, -7.154544010627095219, 0.000000000000000000 ) ) ;
#56165 = CARTESIAN_POINT ( 'NONE',  ( 6.477827756726281194, 6.756902019748111776, -0.2091553196570776485 ) ) ;
#56166 = CARTESIAN_POINT ( 'NONE',  ( -1.500000000000008216, 13.24999999999999822, 3.469446951953614189E-15 ) ) ;
#56167 = CARTESIAN_POINT ( 'NONE',  ( 5.017926250833595780, 7.907978821730911712, -1.082531754730548412 ) ) ;
#56168 =( BOUNDED_SURFACE ( )  B_SPLINE_SURFACE ( 3, 2, ( 
 ( #181549, #96077, #16901 ),
 ( #113439, #180500, #210854 ),
 ( #149055, #193549, #111306 ),
 ( #32117, #49433, #162130 ) ),
 .UNSPECIFIED., .F., .F., .T. ) 
 B_SPLINE_SURFACE_WITH_KNOTS ( ( 4, 4 ),
 ( 3, 3 ),
 ( 0.06089844177390838637, 0.06334004522945697879 ),
 ( 0.000000000000000000, 1.000000000000000000 ),
 .UNSPECIFIED. ) 
 GEOMETRIC_REPRESENTATION_ITEM ( )  RATIONAL_B_SPLINE_SURFACE ( (
 ( 1.000000000000000000, 0.7169884966214687960, 1.000000000000000000),
 ( 1.000000000000000000, 0.7174883642159475272, 1.000000000000000000),
 ( 1.000000000000000000, 0.7180610417775422638, 1.000000000000000000),
 ( 1.000000000000000000, 0.7187540717311187155, 1.000000000000000000) ) ) 
 REPRESENTATION_ITEM ( '' )  SURFACE ( )  );
#56169 = CARTESIAN_POINT ( 'NONE',  ( 5.571497546025357295, 1.705283197966761310, -0.4730582879079441305 ) ) ;
#56170 = AXIS2_PLACEMENT_3D ( 'NONE', #90539, #188006, #41799 ) ;
#56171 = CARTESIAN_POINT ( 'NONE',  ( 3.510405448560415032, -2.010878083398774052, -0.09666398930169986525 ) ) ;
#56172 = CARTESIAN_POINT ( 'NONE',  ( 9.094822116668764167, 9.505047312402055582, 0.7998128361456462443 ) ) ;
#56173 = CARTESIAN_POINT ( 'NONE',  ( 1.624194961551369776, -1.169474557214383870, -1.751182684644275289 ) ) ;
#56174 = VECTOR ( 'NONE', #144385, 1000.000000000000000 ) ;
#56175 = CARTESIAN_POINT ( 'NONE',  ( -1.364683531250000748, 11.10937500034139802, 0.000000000000000000 ) ) ;
#56177 = ADVANCED_FACE ( 'NONE', ( #60126 ), #77340, .T. ) ;
#56176 = CARTESIAN_POINT ( 'NONE',  ( 1.170285302187854981, -0.8824026946198880728, -1.760880109839728647 ) ) ;
#56178 = DIRECTION ( 'NONE',  ( 0.000000000000000000, 0.000000000000000000, -1.000000000000000000 ) ) ;
#56179 = CARTESIAN_POINT ( 'NONE',  ( 2.449293598294706414E-16, -1.500000000000001332, -2.000000000000000000 ) ) ;
#56181 = ORIENTED_EDGE ( 'NONE', *, *, #198981, .T. ) ;
#56180 = CARTESIAN_POINT ( 'NONE',  ( 6.029554192727712980, -0.2124046070472781211, 1.799012333733180702 ) ) ;
#56182 = CARTESIAN_POINT ( 'NONE',  ( 6.480434237652132445, 7.623223367758051872, 1.082531754730558626 ) ) ;
#56183 = CARTESIAN_POINT ( 'NONE',  ( -1.364683531250014514, -0.1572916663252435232, 0.7879004041258379498 ) ) ;
#56184 = ADVANCED_FACE ( 'NONE', ( #93725 ), #152349, .F. ) ;
#56185 = CARTESIAN_POINT ( 'NONE',  ( 4.891396039733495016, 1.386484060982313249, 1.255958711209571810 ) ) ;
#56186 = VERTEX_POINT ( 'NONE', #162980 ) ;
#56187 = CARTESIAN_POINT ( 'NONE',  ( 5.893440691016273547, -1.874049447596724427, 0.8799615681738190975 ) ) ;
#56188 = CARTESIAN_POINT ( 'NONE',  ( -1.225000000000045386, 2.250000000000001776, -4.683753385137379155E-14 ) ) ;
#56189 = CARTESIAN_POINT ( 'NONE',  ( -6.102578539482539810, 6.292298848917299736, 0.000000000000000000 ) ) ;
#56190 = CARTESIAN_POINT ( 'NONE',  ( 7.130698725783555680, 10.40656671580112658, 1.199719254218460707 ) ) ;
#56191 = CARTESIAN_POINT ( 'NONE',  ( -9.612894607289142357, 11.17379744904754801, -1.199719254218441611 ) ) ;
#56192 = CARTESIAN_POINT ( 'NONE',  ( 7.614839552730775729, 8.913009562054615031, 1.199719254218452047 ) ) ;
#56193 = CARTESIAN_POINT ( 'NONE',  ( 0.6823417656249882723, -0.1572916663252488245, 1.181850606188755259 ) ) ;
#56195 = EDGE_CURVE ( 'NONE', #95365, #210028, #28965, .T. ) ;
#56194 = CARTESIAN_POINT ( 'NONE',  ( 1.499999999999989120, 1.275000000000019229, 0.000000000000000000 ) ) ;
#56197 = CARTESIAN_POINT ( 'NONE',  ( 4.123651276850781144, 7.962676922967908411, -0.7998128361456221525 ) ) ;
#56196 = CARTESIAN_POINT ( 'NONE',  ( 5.125427350195786325, 0.1941421753944693185, -1.952251141935714696 ) ) ;
#56198 = CARTESIAN_POINT ( 'NONE',  ( 1.845077155533506374, -1.080901620906085547, 1.701686244941137183 ) ) ;
#56199 = LINE ( 'NONE', #169938, #93384 ) ;
#56200 = CARTESIAN_POINT ( 'NONE',  ( 0.1698123575781598782, 1.266975945507025081, 1.788028528876134393 ) ) ;
#56201 = SURFACE_STYLE_FILL_AREA ( #124488 ) ;
#56202 = CARTESIAN_POINT ( 'NONE',  ( 1.792056902697708454, -1.861051795492570049, -0.1884349046137670514 ) ) ;
#56203 = CARTESIAN_POINT ( 'NONE',  ( 1.364683531249990311, 4.634375000341417916, 1.214306433183764966E-14 ) ) ;
#56204 = CARTESIAN_POINT ( 'NONE',  ( -7.147119532698295252, 11.49005655479003174, 0.000000000000000000 ) ) ;
#56206 = CARTESIAN_POINT ( 'NONE',  ( 3.075892445452293344, -0.8556518723831849638, 1.936791289764336010 ) ) ;
#56205 = CARTESIAN_POINT ( 'NONE',  ( -3.782361668532609134, 7.356579680022602652, 1.040834085586084257E-14 ) ) ;
#56207 = CARTESIAN_POINT ( 'NONE',  ( -0.04536344973642384565, -10.00000000000004796, -9.579592128873146706 ) ) ;
#56208 = CARTESIAN_POINT ( 'NONE',  ( 4.545415791725802457, 1.850806902094417783, -0.9279678557222792445 ) ) ;
#56209 = CARTESIAN_POINT ( 'NONE',  ( 5.180097208873055692, 8.201141289397330780, -1.199719254218450271 ) ) ;
#56211 = CARTESIAN_POINT ( 'NONE',  ( 6.620655732516645742, 7.051964633898824886, 2.771890290588132189 ) ) ;
#56210 = CARTESIAN_POINT ( 'NONE',  ( 1.575843314401915496, -1.115566239278027671, 1.768056137498266844 ) ) ;
#56213 = VERTEX_POINT ( 'NONE', #49226 ) ;
#56212 = CARTESIAN_POINT ( 'NONE',  ( 6.493173258741942178, 1.586635928914212013, -0.9027890188317910791 ) ) ;
#56214 = CARTESIAN_POINT ( 'NONE',  ( 7.130698725783555680, 10.40656671580112658, 1.199719254218460707 ) ) ;
#56215 = CARTESIAN_POINT ( 'NONE',  ( -3.958617665510272943, 6.601842462195195438, -1.082531754730549967 ) ) ;
#56217 = VECTOR ( 'NONE', #173740, 1000.000000000000000 ) ;
#56216 = CARTESIAN_POINT ( 'NONE',  ( 5.355107487273504496, 6.310342158982962246, -1.082531754730543083 ) ) ;
#56218 = CARTESIAN_POINT ( 'NONE',  ( -10.83925572545687999, 5.627432043407305962, 6.488667418600654102 ) ) ;
#56219 = CARTESIAN_POINT ( 'NONE',  ( 7.171900071504736296, 9.390302721554109056, -1.443375672974058777 ) ) ;
#56220 = CARTESIAN_POINT ( 'NONE',  ( -1.402160292154681736E-14, 13.23437500034139980, 1.575800808251682339 ) ) ;
#56221 = CARTESIAN_POINT ( 'NONE',  ( 6.358066468859800757, 0.7272683628555456359, -1.768788954293845528 ) ) ;
#56222 = CARTESIAN_POINT ( 'NONE',  ( -6.835281999583978418, 11.12624609948998966, -0.7998128361456291469 ) ) ;
#56223 =( BOUNDED_SURFACE ( )  B_SPLINE_SURFACE ( 1, 2, ( 
 ( #109520, #27117, #74821, #93223, #159255, #210123, #156072, #40187, #7658, #205867, #91087, #76929, #143055, #172321, #192807, #58564, #44466, #123660, #196037, #12993, #96423, #63889, #114835, #178723, #81208, #33519, #113782, #97478, #95359, #112711, #128978, #163534, #49771, #197083, #62817, #45533, #46593, #211192, #131094, #161409, #14047, #99591, #193884, #181882, #48720, #165657, #989, #180833, #17244, #32458, #98528, #162474, #80135, #115897, #83320, #111647, #149408, #177659, #145186, #194957, #179784, #31404, #65981, #214351, #164589, #127932, #132132, #30338, #146238, #29267, #212255, #79068, #130044, #47671, #15119, #16175, #82259, #213319, #147287, #148351, #31757, #197428, #182239, #16529, #200609, #150839, #148696, #83675, #33864, #17591, #133544, #52256, #163893, #51195, #117317, #49070, #66336, #15469, #183313, #50129, #115189, #116251, #100992, #18673, #84752, #2400, #118383, #30692, #14401, #64248, #130390, #196381, #32809, #98884, #40006, #108266, #88763, #8552, #125596, #172138, #188366, #74631, #109337, #42151, #122408, #105014, #106116, #56251, #190493, #6404, #73556, #159077, #38931, #26927, #174287, #10674, #60498, #25862, #93035, #91972, #158030, #155886, #7474, #175347, #76745, #171054, #142867, #22651, #204599, #23732, #173217, #24796, #191556, #59439, #9618, #184371, #43220, #89837, #139658, #208868, #205678, #154819, #57315, #123479, #90900, #75694, #141807, #58380, #189442, #72476, #41085, #107192, #124536, #156960, #138576, #140738, #206750, #207811, #13868, #79946, #129858, #130905, #127740, #47482, #163348, #45341, #211001, #193697, #126657, #44276, #160145, #77817, #209934, #177466, #29080, #95164, #161213, #12800, #78873, #144996, #207458, #56951, #59077, #156598, #172850, #26574, #7103, #125237, #43924, #158723, #61218, #91615, #193347, #174989, #155522, #143580, #127375, #189082, #191196, #25506, #74275, #108970, #157665, #209573, #73175, #77462, #139283, #205313, #8190, #10320, #9263, #105734, #92678, #140368, #42862, #76394, #173934, #123123, #206386, #41794, #142503, #58012, #208511, #11384, #75334, #60145, #40715, #124177, #126303, #171763, #192262, #110039, #24421, #90534, #190140, #176051, #27644, #93744, #107907, #23359, #89469, #194413, #114308, #78527, #145717, #16705, #111100, #99058, #180306, #148864, #44991, #31928, #165113, #98009, #15643, #13526, #79598, #181356, #438, #177106, #28722, #94808, #112176, #178181, #30870, #96948, #32982, #131600, #164064, #160857, #12449, #29796, #95880, #144644, #161935, #210660, #211715, #63352, #130563, #81731, #147813, #213832, #129510, #195491, #47126, #113242, #65450, #179246, #154204, #104389, #184543, #37244, #201847, #119628, #135822, #22024, #51371, #169377, #20961, #167252, #36163, #117494, #87059, #102242, #151011, #168314, #153131, #53491, #4704, #70778, #118559, #88133, #5773, #19911, #85996, #149941, #152070, #35094, #183485, #185613, #100113, #3640, #136892, #103315, #71852, #69719, #198653, #202919, #34040, #50302, #116420, #67575, #54563, #120709, #18838, #186684, #38312, #182411, #166174, #170436, #17763, #83851, #101165, #1509, #133720, #199725, #84923, #2580, #68650, #134773, #52433, #200781, #106567, #74018, #124984, #189894, #76145, #10069, #207206, #137960, #142248, #72929, #205059, #175798, #122868, #93490, #188829, #90276, #41536, #190944, #141195, #9007, #155270, #208261, #139035, #24173, #75082, #123926, #159529, #43672, #107647, #42608, #58830, #108716, #174743, #27390, #56701, #26317, #92429, #172595, #173679, #40464, #158469, #25254, #156345, #91355, #59894, #126045, #192007, #109790, #57765, #11128, #203980, #157416, #55627, #89218, #121784, #7930, #140108, #187751, #39380, #105476, #171509, #23102, #6851, #206135, #209317, #146514, #193090, #115114, #32728, #160599, #162752, #14324, #45806, #80416, #212533, #110846, #144400, #210401, #128198, #145469, #64173, #130316, #196304, #47950, #114064, #15392, #200273, #2061, #116976, #148363, #17255, #199203, #101729, #999, #68133, #20463, #34589, #18329, #16186, #67063, #133200, #150500, #36717, #118049, #198148, #98538, #50850, #132141, #167800 ),
 ( #102803, #86547, #114844, #152612, #164600, #65992, #182973, #19396, #85476, #151563, #3130, #48731, #69200, #119110, #4197, #214362, #39942, #137450, #170991, #138512, #189378, #22590, #155823, #108204, #73489, #57253, #55120, #187240, #6340, #123414, #54053, #41021, #107129, #173152, #24734, #90836, #206687, #207505, #63132, #148654, #25551, #16487, #15424, #221, #173978, #81514, #82567, #131388, #197384, #145499, #211496, #98843, #66293, #91661, #132439, #9310, #194191, #45835, #162780, #49026, #115144, #181141, #32763, #157713, #164893, #177958, #29572, #198440, #161715, #75383, #13307, #129295, #141497, #59125, #125282, #95663, #79380, #113020, #51148, #2360, #53277, #102030, #71634, #21805, #168100, #169157, #119409, #103098, #185398, #153984, #183270, #86845, #152911, #84709, #19699, #34874, #4488, #85777, #68436, #3434, #70559, #20750, #136678, #202703, #35952, #5552, #137747, #69501, #135609, #67356, #201629, #167035, #100948, #54353, #17547, #120492, #186465, #38101, #203766, #104173, #116208, #170221, #165962, #182194, #99901, #199505, #87911, #149718, #150796, #1297, #133501, #117272, #18630, #134565, #200567, #52213, #118343, #184327, #206981, #27167, #23960, #92212, #142030, #39165, #25032, #105249, #122642, #121564, #57549, #156125, #173452, #58611, #208044, #158263, #9852, #75927, #10903, #123707, #90063, #93272, #7707, #40237, #59672, #188605, #125830, #205915, #191791, #73790, #204830, #108498, #189668, #107427, #124766, #55410, #6636, #41318, #43449, #91132, #56482, #139885, #157190, #8786, #74867, #140972, #190725, #109572, #42389, #106348, #174522, #175576, #172370, #159305, #26098, #138811, #88997, #76980, #72715, #143106, #187536, #171290, #22881, #155050, #48766, #193932, #13038, #210171, #209099, #192855, #62864, #64984, #131140, #44514, #197128, #79118, #11980, #14094, #61811, #114881, #147334, #129030, #126898, #195005, #45579, #78054, #180881, #111695, #211238, #97528, #127979, #160378, #213363, #177702, #161459, #110631, #176632, #29313, #32502, #98576, #60734, #196084, #95407, #145233, #144178, #46639, #94337, #179830, #112761, #178774, #30386, #164638, #130089, #80184, #82305, #28243, #96473, #162521, #146289, #212301, #63934, #47716, #113832, #31450, #16222, #163585, #15167, #81255, #119144, #4231, #120225, #37833, #103910, #148400, #67098, #49818, #17291, #117009, #199239, #50886, #68170, #105820, #204308, #171846, #90619, #123200, #156676, #206468, #39711, #9344, #75417, #23439, #7186, #71113, #73258, #170774, #38648, #40800, #21293, #155601, #58095, #172931, #119962, #89550, #185937, #189161, #169703, #157747, #37572, #203251, #57033, #106906, #88475, #24508, #8269, #87398, #137230, #91694, #121048, #104726, #22363, #124256, #190214, #154534, #41874, #6114, #107985, #174012, #188082, #55965, #122117, #25583, #46135, #110118, #144725, #179329, #45073, #28801, #92756, #176130, #192341, #160938, #47207, #128523, #208588, #191274, #27729, #93824, #194492, #158801, #159865, #30950, #125315, #113322, #112251, #97024, #146841, #178262, #163078, #29875, #95959, #11467, #77540, #14660, #59157, #42940, #109049, #10398, #143662, #209656, #210737, #162013, #211795, #63432, #79676, #61297, #127458, #193429, #52252, #22923, #184367, #155094, #35990, #151895, #103138, #186509, #202742, #70602, #2397, #71673, #134603, #85816, #136716, #185436, #37056, #89038, #100986, #171328, #34913, #167076, #102070, #38140, #119449, #72756, #104212, #168135, #54392, #152952, #53316, #84747, #19737, #135646, #170259, #3470, #4527, #105292, #169197, #20790, #18667, #69539, #200605, #86885, #121603, #120530, #118379, #117311, #201669, #68476, #21844, #150835, #87952, #6679, #51188, #39200, #154026, #199546, #183307, #5593, #137786, #203805, #55451, #187575, #107474, #60784, #192900, #204870, #44556, #188648, #156168, #7749, #124808, #190769, #77021, #10947, #208087, #138853, #143151, #73836, #205959, #176672, #123749, #94379, #189710, #91177, #42431, #125874, #142073, #9893, #139932, #209145, #57592, #25074, #75970, #108537, #160419, #110672, #174567, #191833, #59715, #43496, #109616, #28284, #41363 ) ),
 .UNSPECIFIED., .F., .F., .T. ) 
 B_SPLINE_SURFACE_WITH_KNOTS ( ( 2, 2 ),
 ( 3, 2, 2, 2, 2, 2, 2, 2, 2, 2, 2, 2, 2, 2, 2, 2, 2, 2, 2, 2, 2, 2, 2, 2, 2, 2, 2, 2, 2, 2, 2, 2, 2, 2, 2, 2, 2, 2, 2, 2, 2, 2, 2, 2, 2, 2, 2, 2, 2, 2, 2, 2, 2, 2, 2, 2, 2, 2, 2, 2, 2, 2, 2, 2, 2, 2, 2, 2, 2, 2, 2, 2, 2, 2, 2, 2, 2, 2, 2, 2, 2, 2, 2, 2, 2, 2, 2, 2, 2, 2, 2, 2, 2, 2, 2, 2, 2, 2, 2, 2, 2, 2, 2, 2, 2, 2, 2, 2, 2, 2, 2, 2, 2, 2, 2, 2, 2, 2, 2, 2, 2, 2, 2, 2, 2, 2, 2, 2, 2, 2, 2, 2, 2, 2, 2, 2, 2, 2, 2, 2, 2, 2, 2, 2, 2, 2, 2, 2, 2, 2, 2, 2, 2, 2, 2, 2, 2, 2, 2, 2, 2, 2, 2, 2, 2, 2, 2, 2, 2, 2, 2, 2, 2, 2, 2, 2, 2, 2, 2, 2, 2, 2, 2, 2, 2, 2, 2, 2, 2, 2, 2, 2, 2, 2, 2, 2, 2, 2, 2, 2, 2, 2, 2, 2, 2, 2, 2, 2, 2, 2, 2, 2, 2, 2, 2, 2, 2, 2, 2, 2, 2, 2, 2, 2, 2, 2, 2, 2, 2, 2, 2, 2, 2, 2, 2, 2, 2, 2, 2, 2, 3 ),
 ( 0.000000000000000000, 1.000000000000000000 ),
 ( 0.000000000000000000, 0.004166666666666666609, 0.008333333333333333218, 0.01250000000000000069, 0.01666666666666666644, 0.02083333333333333218, 0.02500000000000000139, 0.02916666666666666713, 0.03333333333333333287, 0.03749999999999999861, 0.04166666666666666435, 0.04583333333333333010, 0.05000000000000000278, 0.05416666666666666852, 0.05833333333333333426, 0.06250000000000000000, 0.06666666666666666574, 0.07083333333333333148, 0.07499999999999999722, 0.07916666666666666297, 0.08333333333333332871, 0.08749999999999999445, 0.09166666666666666019, 0.09583333333333333981, 0.1000000000000000056, 0.1041666666666666713, 0.1083333333333333370, 0.1125000000000000028, 0.1166666666666666685, 0.1208333333333333343, 0.1250000000000000000, 0.1291666666666666796, 0.1333333333333333315, 0.1375000000000000111, 0.1416666666666666630, 0.1458333333333333426, 0.1499999999999999944, 0.1541666666666666741, 0.1583333333333333259, 0.1625000000000000056, 0.1666666666666666574, 0.1708333333333333370, 0.1749999999999999889, 0.1791666666666666685, 0.1833333333333333204, 0.1875000000000000000, 0.1916666666666666796, 0.1958333333333333315, 0.2000000000000000111, 0.2041666666666666630, 0.2083333333333333426, 0.2124999999999999944, 0.2166666666666666741, 0.2208333333333333259, 0.2250000000000000056, 0.2291666666666666574, 0.2333333333333333370, 0.2374999999999999889, 0.2416666666666666685, 0.2458333333333333204, 0.2500000000000000000, 0.2541666666666666519, 0.2583333333333333592, 0.2625000000000000111, 0.2666666666666666630, 0.2708333333333333148, 0.2750000000000000222, 0.2791666666666666741, 0.2833333333333333259, 0.2874999999999999778, 0.2916666666666666852, 0.2958333333333333370, 0.2999999999999999889, 0.3041666666666666408, 0.3083333333333333481, 0.3125000000000000000, 0.3166666666666666519, 0.3208333333333333592, 0.3250000000000000111, 0.3291666666666666630, 0.3333333333333333148, 0.3375000000000000222, 0.3416666666666666741, 0.3458333333333333259, 0.3499999999999999778, 0.3541666666666666852, 0.3583333333333333370, 0.3624999999999999889, 0.3666666666666666408, 0.3708333333333333481, 0.3750000000000000000, 0.3791666666666666519, 0.3833333333333333592, 0.3875000000000000111, 0.3916666666666666630, 0.3958333333333333148, 0.4000000000000000222, 0.4041666666666666741, 0.4083333333333333259, 0.4124999999999999778, 0.4166666666666666852, 0.4208333333333333370, 0.4249999999999999889, 0.4291666666666666408, 0.4333333333333333481, 0.4375000000000000000, 0.4416666666666666519, 0.4458333333333333592, 0.4500000000000000111, 0.4541666666666666630, 0.4583333333333333148, 0.4625000000000000222, 0.4666666666666666741, 0.4708333333333333259, 0.4749999999999999778, 0.4791666666666666852, 0.4833333333333333370, 0.4874999999999999889, 0.4916666666666666408, 0.4958333333333333481, 0.5000000000000000000, 0.5041666666666666519, 0.5083333333333333037, 0.5124999999999999556, 0.5166666666666667185, 0.5208333333333333703, 0.5250000000000000222, 0.5291666666666666741, 0.5333333333333333259, 0.5374999999999999778, 0.5416666666666666297, 0.5458333333333332815, 0.5500000000000000444, 0.5541666666666666963, 0.5583333333333333481, 0.5625000000000000000, 0.5666666666666666519, 0.5708333333333333037, 0.5749999999999999556, 0.5791666666666667185, 0.5833333333333333703, 0.5875000000000000222, 0.5916666666666666741, 0.5958333333333333259, 0.5999999999999999778, 0.6041666666666666297, 0.6083333333333332815, 0.6125000000000000444, 0.6166666666666666963, 0.6208333333333333481, 0.6250000000000000000, 0.6291666666666666519, 0.6333333333333333037, 0.6374999999999999556, 0.6416666666666667185, 0.6458333333333333703, 0.6500000000000000222, 0.6541666666666666741, 0.6583333333333333259, 0.6624999999999999778, 0.6666666666666666297, 0.6708333333333332815, 0.6750000000000000444, 0.6791666666666666963, 0.6833333333333333481, 0.6875000000000000000, 0.6916666666666666519, 0.6958333333333333037, 0.6999999999999999556, 0.7041666666666667185, 0.7083333333333333703, 0.7125000000000000222, 0.7166666666666666741, 0.7208333333333333259, 0.7249999999999999778, 0.7291666666666666297, 0.7333333333333332815, 0.7375000000000000444, 0.7416666666666666963, 0.7458333333333333481, 0.7500000000000000000, 0.7541666666666666519, 0.7583333333333333037, 0.7624999999999999556, 0.7666666666666667185, 0.7708333333333333703, 0.7750000000000000222, 0.7791666666666666741, 0.7833333333333333259, 0.7874999999999999778, 0.7916666666666666297, 0.7958333333333332815, 0.8000000000000000444, 0.8041666666666666963, 0.8083333333333333481, 0.8125000000000000000, 0.8166666666666666519, 0.8208333333333333037, 0.8249999999999999556, 0.8291666666666667185, 0.8333333333333333703, 0.8375000000000000222, 0.8416666666666666741, 0.8458333333333333259, 0.8499999999999999778, 0.8541666666666666297, 0.8583333333333332815, 0.8625000000000000444, 0.8666666666666666963, 0.8708333333333333481, 0.8750000000000000000, 0.8791666666666666519, 0.8833333333333333037, 0.8874999999999999556, 0.8916666666666667185, 0.8958333333333333703, 0.9000000000000000222, 0.9041666666666666741, 0.9083333333333333259, 0.9124999999999999778, 0.9166666666666666297, 0.9208333333333332815, 0.9250000000000000444, 0.9291666666666666963, 0.9333333333333333481, 0.9375000000000000000, 0.9416666666666666519, 0.9458333333333333037, 0.9499999999999999556, 0.9541666666666667185, 0.9583333333333333703, 0.9625000000000000222, 0.9666666666666666741, 0.9708333333333333259, 0.9749999999999999778, 0.9791666666666666297, 0.9833333333333332815, 0.9875000000000000444, 0.9916666666666666963, 0.9958333333333333481, 1.000000000000000000 ),
 .UNSPECIFIED. ) 
 GEOMETRIC_REPRESENTATION_ITEM ( )  RATIONAL_B_SPLINE_SURFACE ( (
 ( 1.000000000000000000, 0.8660254037844387076, 1.000000000000000000, 0.8660254037844387076, 1.000000000000000000, 0.8660254037844387076, 1.000000000000000000, 0.8660254037844387076, 1.000000000000000000, 0.8660254037844387076, 1.000000000000000000, 0.8660254037844387076, 1.000000000000000000, 0.8660254037844387076, 1.000000000000000000, 0.8660254037844387076, 1.000000000000000000, 0.8660254037844387076, 1.000000000000000000, 0.8660254037844387076, 1.000000000000000000, 0.8660254037844387076, 1.000000000000000000, 0.8660254037844387076, 1.000000000000000000, 0.8660254037844387076, 1.000000000000000000, 0.8660254037844387076, 1.000000000000000000, 0.8660254037844387076, 1.000000000000000000, 0.8660254037844387076, 1.000000000000000000, 0.8660254037844387076, 1.000000000000000000, 0.8660254037844387076, 1.000000000000000000, 0.8660254037844387076, 1.000000000000000000, 0.8660254037844387076, 1.000000000000000000, 0.8660254037844387076, 1.000000000000000000, 0.8660254037844387076, 1.000000000000000000, 0.8660254037844387076, 1.000000000000000000, 0.8660254037844387076, 1.000000000000000000, 0.8660254037844387076, 1.000000000000000000, 0.8660254037844387076, 1.000000000000000000, 0.8660254037844387076, 1.000000000000000000, 0.8660254037844387076, 1.000000000000000000, 0.8660254037844387076, 1.000000000000000000, 0.8660254037844387076, 1.000000000000000000, 0.8660254037844387076, 1.000000000000000000, 0.8660254037844387076, 1.000000000000000000, 0.8660254037844387076, 1.000000000000000000, 0.8660254037844387076, 1.000000000000000000, 0.8660254037844387076, 1.000000000000000000, 0.8660254037844387076, 1.000000000000000000, 0.8660254037844387076, 1.000000000000000000, 0.8660254037844387076, 1.000000000000000000, 0.8660254037844387076, 1.000000000000000000, 0.8660254037844387076, 1.000000000000000000, 0.8660254037844387076, 1.000000000000000000, 0.8660254037844387076, 1.000000000000000000, 0.8660254037844387076, 1.000000000000000000, 0.8660254037844387076, 1.000000000000000000, 0.8660254037844387076, 1.000000000000000000, 0.8660254037844387076, 1.000000000000000000, 0.8660254037844387076, 1.000000000000000000, 0.8660254037844387076, 1.000000000000000000, 0.8660254037844387076, 1.000000000000000000, 0.8660254037844387076, 1.000000000000000000, 0.8660254037844387076, 1.000000000000000000, 0.8660254037844387076, 1.000000000000000000, 0.8660254037844387076, 1.000000000000000000, 0.8660254037844387076, 1.000000000000000000, 0.8660254037844387076, 1.000000000000000000, 0.8660254037844387076, 1.000000000000000000, 0.8660254037844387076, 1.000000000000000000, 0.8660254037844387076, 1.000000000000000000, 0.8660254037844387076, 1.000000000000000000, 0.8660254037844387076, 1.000000000000000000, 0.8660254037844387076, 1.000000000000000000, 0.8660254037844387076, 1.000000000000000000, 0.8660254037844387076, 1.000000000000000000, 0.8660254037844387076, 1.000000000000000000, 0.8660254037844387076, 1.000000000000000000, 0.8660254037844387076, 1.000000000000000000, 0.8660254037844387076, 1.000000000000000000, 0.8660254037844387076, 1.000000000000000000, 0.8660254037844387076, 1.000000000000000000, 0.8660254037844387076, 1.000000000000000000, 0.8660254037844387076, 1.000000000000000000, 0.8660254037844387076, 1.000000000000000000, 0.8660254037844387076, 1.000000000000000000, 0.8660254037844387076, 1.000000000000000000, 0.8660254037844387076, 1.000000000000000000, 0.8660254037844387076, 1.000000000000000000, 0.8660254037844387076, 1.000000000000000000, 0.8660254037844387076, 1.000000000000000000, 0.8660254037844387076, 1.000000000000000000, 0.8660254037844387076, 1.000000000000000000, 0.8660254037844387076, 1.000000000000000000, 0.8660254037844387076, 1.000000000000000000, 0.8660254037844387076, 1.000000000000000000, 0.8660254037844387076, 1.000000000000000000, 0.8660254037844387076, 1.000000000000000000, 0.8660254037844387076, 1.000000000000000000, 0.8660254037844387076, 1.000000000000000000, 0.8660254037844387076, 1.000000000000000000, 0.8660254037844387076, 1.000000000000000000, 0.8660254037844387076, 1.000000000000000000, 0.8660254037844387076, 1.000000000000000000, 0.8660254037844387076, 1.000000000000000000, 0.8660254037844387076, 1.000000000000000000, 0.8660254037844387076, 1.000000000000000000, 0.8660254037844387076, 1.000000000000000000, 0.8660254037844387076, 1.000000000000000000, 0.8660254037844387076, 1.000000000000000000, 0.8660254037844387076, 1.000000000000000000, 0.8660254037844387076, 1.000000000000000000, 0.8660254037844387076, 1.000000000000000000, 0.8660254037844387076, 1.000000000000000000, 0.8660254037844387076, 1.000000000000000000, 0.8660254037844387076, 1.000000000000000000, 0.8660254037844387076, 1.000000000000000000, 0.8660254037844387076, 1.000000000000000000, 0.8660254037844387076, 1.000000000000000000, 0.8660254037844387076, 1.000000000000000000, 0.8660254037844387076, 1.000000000000000000, 0.8660254037844387076, 1.000000000000000000, 0.8660254037844387076, 1.000000000000000000, 0.8660254037844387076, 1.000000000000000000, 0.8660254037844387076, 1.000000000000000000, 0.8660254037844387076, 1.000000000000000000, 0.8660254037844387076, 1.000000000000000000, 0.8660254037844387076, 1.000000000000000000, 0.8660254037844387076, 1.000000000000000000, 0.8660254037844387076, 1.000000000000000000, 0.8660254037844387076, 1.000000000000000000, 0.8660254037844387076, 1.000000000000000000, 0.8660254037844387076, 1.000000000000000000, 0.8660254037844387076, 1.000000000000000000, 0.8660254037844387076, 1.000000000000000000, 0.8660254037844387076, 1.000000000000000000, 0.8660254037844387076, 1.000000000000000000, 0.8660254037844387076, 1.000000000000000000, 0.8660254037844387076, 1.000000000000000000, 0.8660254037844387076, 1.000000000000000000, 0.8660254037844387076, 1.000000000000000000, 0.8660254037844387076, 1.000000000000000000, 0.8660254037844387076, 1.000000000000000000, 0.8660254037844387076, 1.000000000000000000, 0.8660254037844387076, 1.000000000000000000, 0.8660254037844387076, 1.000000000000000000, 0.8660254037844387076, 1.000000000000000000, 0.8660254037844387076, 1.000000000000000000, 0.8660254037844387076, 1.000000000000000000, 0.8660254037844387076, 1.000000000000000000, 0.8660254037844387076, 1.000000000000000000, 0.8660254037844387076, 1.000000000000000000, 0.8660254037844387076, 1.000000000000000000, 0.8660254037844387076, 1.000000000000000000, 0.8660254037844387076, 1.000000000000000000, 0.8660254037844387076, 1.000000000000000000, 0.8660254037844387076, 1.000000000000000000, 0.8660254037844387076, 1.000000000000000000, 0.8660254037844387076, 1.000000000000000000, 0.8660254037844387076, 1.000000000000000000, 0.8660254037844387076, 1.000000000000000000, 0.8660254037844387076, 1.000000000000000000, 0.8660254037844387076, 1.000000000000000000, 0.8660254037844387076, 1.000000000000000000, 0.8660254037844387076, 1.000000000000000000, 0.8660254037844387076, 1.000000000000000000, 0.8660254037844387076, 1.000000000000000000, 0.8660254037844387076, 1.000000000000000000, 0.8660254037844387076, 1.000000000000000000, 0.8660254037844387076, 1.000000000000000000, 0.8660254037844387076, 1.000000000000000000, 0.8660254037844387076, 1.000000000000000000, 0.8660254037844387076, 1.000000000000000000, 0.8660254037844387076, 1.000000000000000000, 0.8660254037844387076, 1.000000000000000000, 0.8660254037844387076, 1.000000000000000000, 0.8660254037844387076, 1.000000000000000000, 0.8660254037844387076, 1.000000000000000000, 0.8660254037844387076, 1.000000000000000000, 0.8660254037844387076, 1.000000000000000000, 0.8660254037844387076, 1.000000000000000000, 0.8660254037844387076, 1.000000000000000000, 0.8660254037844387076, 1.000000000000000000, 0.8660254037844387076, 1.000000000000000000, 0.8660254037844387076, 1.000000000000000000, 0.8660254037844387076, 1.000000000000000000, 0.8660254037844387076, 1.000000000000000000, 0.8660254037844387076, 1.000000000000000000, 0.8660254037844387076, 1.000000000000000000, 0.8660254037844387076, 1.000000000000000000, 0.8660254037844387076, 1.000000000000000000, 0.8660254037844387076, 1.000000000000000000, 0.8660254037844387076, 1.000000000000000000, 0.8660254037844387076, 1.000000000000000000, 0.8660254037844387076, 1.000000000000000000, 0.8660254037844387076, 1.000000000000000000, 0.8660254037844387076, 1.000000000000000000, 0.8660254037844387076, 1.000000000000000000, 0.8660254037844387076, 1.000000000000000000, 0.8660254037844387076, 1.000000000000000000, 0.8660254037844387076, 1.000000000000000000, 0.8660254037844387076, 1.000000000000000000, 0.8660254037844387076, 1.000000000000000000, 0.8660254037844387076, 1.000000000000000000, 0.8660254037844387076, 1.000000000000000000, 0.8660254037844387076, 1.000000000000000000, 0.8660254037844387076, 1.000000000000000000, 0.8660254037844387076, 1.000000000000000000, 0.8660254037844387076, 1.000000000000000000, 0.8660254037844387076, 1.000000000000000000, 0.8660254037844387076, 1.000000000000000000, 0.8660254037844387076, 1.000000000000000000, 0.8660254037844387076, 1.000000000000000000, 0.8660254037844387076, 1.000000000000000000, 0.8660254037844387076, 1.000000000000000000, 0.8660254037844387076, 1.000000000000000000, 0.8660254037844387076, 1.000000000000000000, 0.8660254037844387076, 1.000000000000000000, 0.8660254037844387076, 1.000000000000000000, 0.8660254037844387076, 1.000000000000000000, 0.8660254037844387076, 1.000000000000000000, 0.8660254037844387076, 1.000000000000000000, 0.8660254037844387076, 1.000000000000000000, 0.8660254037844387076, 1.000000000000000000, 0.8660254037844387076, 1.000000000000000000, 0.8660254037844387076, 1.000000000000000000, 0.8660254037844387076, 1.000000000000000000, 0.8660254037844387076, 1.000000000000000000, 0.8660254037844387076, 1.000000000000000000, 0.8660254037844387076, 1.000000000000000000, 0.8660254037844387076, 1.000000000000000000, 0.8660254037844387076, 1.000000000000000000, 0.8660254037844387076, 1.000000000000000000, 0.8660254037844387076, 1.000000000000000000, 0.8660254037844387076, 1.000000000000000000, 0.8660254037844387076, 1.000000000000000000, 0.8660254037844387076, 1.000000000000000000, 0.8660254037844387076, 1.000000000000000000, 0.8660254037844387076, 1.000000000000000000, 0.8660254037844387076, 1.000000000000000000, 0.8660254037844387076, 1.000000000000000000, 0.8660254037844387076, 1.000000000000000000, 0.8660254037844387076, 1.000000000000000000, 0.8660254037844387076, 1.000000000000000000, 0.8660254037844387076, 1.000000000000000000, 0.8660254037844387076, 1.000000000000000000, 0.8660254037844387076, 1.000000000000000000, 0.8660254037844387076, 1.000000000000000000, 0.8660254037844387076, 1.000000000000000000, 0.8660254037844387076, 1.000000000000000000, 0.8660254037844387076, 1.000000000000000000, 0.8660254037844387076, 1.000000000000000000, 0.8660254037844387076, 1.000000000000000000),
 ( 1.000000000000000000, 0.8660254037844387076, 1.000000000000000000, 0.8660254037844387076, 1.000000000000000000, 0.8660254037844387076, 1.000000000000000000, 0.8660254037844387076, 1.000000000000000000, 0.8660254037844387076, 1.000000000000000000, 0.8660254037844387076, 1.000000000000000000, 0.8660254037844387076, 1.000000000000000000, 0.8660254037844387076, 1.000000000000000000, 0.8660254037844387076, 1.000000000000000000, 0.8660254037844387076, 1.000000000000000000, 0.8660254037844387076, 1.000000000000000000, 0.8660254037844387076, 1.000000000000000000, 0.8660254037844387076, 1.000000000000000000, 0.8660254037844387076, 1.000000000000000000, 0.8660254037844387076, 1.000000000000000000, 0.8660254037844387076, 1.000000000000000000, 0.8660254037844387076, 1.000000000000000000, 0.8660254037844387076, 1.000000000000000000, 0.8660254037844387076, 1.000000000000000000, 0.8660254037844387076, 1.000000000000000000, 0.8660254037844387076, 1.000000000000000000, 0.8660254037844387076, 1.000000000000000000, 0.8660254037844387076, 1.000000000000000000, 0.8660254037844387076, 1.000000000000000000, 0.8660254037844387076, 1.000000000000000000, 0.8660254037844387076, 1.000000000000000000, 0.8660254037844387076, 1.000000000000000000, 0.8660254037844387076, 1.000000000000000000, 0.8660254037844387076, 1.000000000000000000, 0.8660254037844387076, 1.000000000000000000, 0.8660254037844387076, 1.000000000000000000, 0.8660254037844387076, 1.000000000000000000, 0.8660254037844387076, 1.000000000000000000, 0.8660254037844387076, 1.000000000000000000, 0.8660254037844387076, 1.000000000000000000, 0.8660254037844387076, 1.000000000000000000, 0.8660254037844387076, 1.000000000000000000, 0.8660254037844387076, 1.000000000000000000, 0.8660254037844387076, 1.000000000000000000, 0.8660254037844387076, 1.000000000000000000, 0.8660254037844387076, 1.000000000000000000, 0.8660254037844387076, 1.000000000000000000, 0.8660254037844387076, 1.000000000000000000, 0.8660254037844387076, 1.000000000000000000, 0.8660254037844387076, 1.000000000000000000, 0.8660254037844387076, 1.000000000000000000, 0.8660254037844387076, 1.000000000000000000, 0.8660254037844387076, 1.000000000000000000, 0.8660254037844387076, 1.000000000000000000, 0.8660254037844387076, 1.000000000000000000, 0.8660254037844387076, 1.000000000000000000, 0.8660254037844387076, 1.000000000000000000, 0.8660254037844387076, 1.000000000000000000, 0.8660254037844387076, 1.000000000000000000, 0.8660254037844387076, 1.000000000000000000, 0.8660254037844387076, 1.000000000000000000, 0.8660254037844387076, 1.000000000000000000, 0.8660254037844387076, 1.000000000000000000, 0.8660254037844387076, 1.000000000000000000, 0.8660254037844387076, 1.000000000000000000, 0.8660254037844387076, 1.000000000000000000, 0.8660254037844387076, 1.000000000000000000, 0.8660254037844387076, 1.000000000000000000, 0.8660254037844387076, 1.000000000000000000, 0.8660254037844387076, 1.000000000000000000, 0.8660254037844387076, 1.000000000000000000, 0.8660254037844387076, 1.000000000000000000, 0.8660254037844387076, 1.000000000000000000, 0.8660254037844387076, 1.000000000000000000, 0.8660254037844387076, 1.000000000000000000, 0.8660254037844387076, 1.000000000000000000, 0.8660254037844387076, 1.000000000000000000, 0.8660254037844387076, 1.000000000000000000, 0.8660254037844387076, 1.000000000000000000, 0.8660254037844387076, 1.000000000000000000, 0.8660254037844387076, 1.000000000000000000, 0.8660254037844387076, 1.000000000000000000, 0.8660254037844387076, 1.000000000000000000, 0.8660254037844387076, 1.000000000000000000, 0.8660254037844387076, 1.000000000000000000, 0.8660254037844387076, 1.000000000000000000, 0.8660254037844387076, 1.000000000000000000, 0.8660254037844387076, 1.000000000000000000, 0.8660254037844387076, 1.000000000000000000, 0.8660254037844387076, 1.000000000000000000, 0.8660254037844387076, 1.000000000000000000, 0.8660254037844387076, 1.000000000000000000, 0.8660254037844387076, 1.000000000000000000, 0.8660254037844387076, 1.000000000000000000, 0.8660254037844387076, 1.000000000000000000, 0.8660254037844387076, 1.000000000000000000, 0.8660254037844387076, 1.000000000000000000, 0.8660254037844387076, 1.000000000000000000, 0.8660254037844387076, 1.000000000000000000, 0.8660254037844387076, 1.000000000000000000, 0.8660254037844387076, 1.000000000000000000, 0.8660254037844387076, 1.000000000000000000, 0.8660254037844387076, 1.000000000000000000, 0.8660254037844387076, 1.000000000000000000, 0.8660254037844387076, 1.000000000000000000, 0.8660254037844387076, 1.000000000000000000, 0.8660254037844387076, 1.000000000000000000, 0.8660254037844387076, 1.000000000000000000, 0.8660254037844387076, 1.000000000000000000, 0.8660254037844387076, 1.000000000000000000, 0.8660254037844387076, 1.000000000000000000, 0.8660254037844387076, 1.000000000000000000, 0.8660254037844387076, 1.000000000000000000, 0.8660254037844387076, 1.000000000000000000, 0.8660254037844387076, 1.000000000000000000, 0.8660254037844387076, 1.000000000000000000, 0.8660254037844387076, 1.000000000000000000, 0.8660254037844387076, 1.000000000000000000, 0.8660254037844387076, 1.000000000000000000, 0.8660254037844387076, 1.000000000000000000, 0.8660254037844387076, 1.000000000000000000, 0.8660254037844387076, 1.000000000000000000, 0.8660254037844387076, 1.000000000000000000, 0.8660254037844387076, 1.000000000000000000, 0.8660254037844387076, 1.000000000000000000, 0.8660254037844387076, 1.000000000000000000, 0.8660254037844387076, 1.000000000000000000, 0.8660254037844387076, 1.000000000000000000, 0.8660254037844387076, 1.000000000000000000, 0.8660254037844387076, 1.000000000000000000, 0.8660254037844387076, 1.000000000000000000, 0.8660254037844387076, 1.000000000000000000, 0.8660254037844387076, 1.000000000000000000, 0.8660254037844387076, 1.000000000000000000, 0.8660254037844387076, 1.000000000000000000, 0.8660254037844387076, 1.000000000000000000, 0.8660254037844387076, 1.000000000000000000, 0.8660254037844387076, 1.000000000000000000, 0.8660254037844387076, 1.000000000000000000, 0.8660254037844387076, 1.000000000000000000, 0.8660254037844387076, 1.000000000000000000, 0.8660254037844387076, 1.000000000000000000, 0.8660254037844387076, 1.000000000000000000, 0.8660254037844387076, 1.000000000000000000, 0.8660254037844387076, 1.000000000000000000, 0.8660254037844387076, 1.000000000000000000, 0.8660254037844387076, 1.000000000000000000, 0.8660254037844387076, 1.000000000000000000, 0.8660254037844387076, 1.000000000000000000, 0.8660254037844387076, 1.000000000000000000, 0.8660254037844387076, 1.000000000000000000, 0.8660254037844387076, 1.000000000000000000, 0.8660254037844387076, 1.000000000000000000, 0.8660254037844387076, 1.000000000000000000, 0.8660254037844387076, 1.000000000000000000, 0.8660254037844387076, 1.000000000000000000, 0.8660254037844387076, 1.000000000000000000, 0.8660254037844387076, 1.000000000000000000, 0.8660254037844387076, 1.000000000000000000, 0.8660254037844387076, 1.000000000000000000, 0.8660254037844387076, 1.000000000000000000, 0.8660254037844387076, 1.000000000000000000, 0.8660254037844387076, 1.000000000000000000, 0.8660254037844387076, 1.000000000000000000, 0.8660254037844387076, 1.000000000000000000, 0.8660254037844387076, 1.000000000000000000, 0.8660254037844387076, 1.000000000000000000, 0.8660254037844387076, 1.000000000000000000, 0.8660254037844387076, 1.000000000000000000, 0.8660254037844387076, 1.000000000000000000, 0.8660254037844387076, 1.000000000000000000, 0.8660254037844387076, 1.000000000000000000, 0.8660254037844387076, 1.000000000000000000, 0.8660254037844387076, 1.000000000000000000, 0.8660254037844387076, 1.000000000000000000, 0.8660254037844387076, 1.000000000000000000, 0.8660254037844387076, 1.000000000000000000, 0.8660254037844387076, 1.000000000000000000, 0.8660254037844387076, 1.000000000000000000, 0.8660254037844387076, 1.000000000000000000, 0.8660254037844387076, 1.000000000000000000, 0.8660254037844387076, 1.000000000000000000, 0.8660254037844387076, 1.000000000000000000, 0.8660254037844387076, 1.000000000000000000, 0.8660254037844387076, 1.000000000000000000, 0.8660254037844387076, 1.000000000000000000, 0.8660254037844387076, 1.000000000000000000, 0.8660254037844387076, 1.000000000000000000, 0.8660254037844387076, 1.000000000000000000, 0.8660254037844387076, 1.000000000000000000, 0.8660254037844387076, 1.000000000000000000, 0.8660254037844387076, 1.000000000000000000, 0.8660254037844387076, 1.000000000000000000, 0.8660254037844387076, 1.000000000000000000, 0.8660254037844387076, 1.000000000000000000, 0.8660254037844387076, 1.000000000000000000, 0.8660254037844387076, 1.000000000000000000, 0.8660254037844387076, 1.000000000000000000, 0.8660254037844387076, 1.000000000000000000, 0.8660254037844387076, 1.000000000000000000, 0.8660254037844387076, 1.000000000000000000, 0.8660254037844387076, 1.000000000000000000, 0.8660254037844387076, 1.000000000000000000, 0.8660254037844387076, 1.000000000000000000, 0.8660254037844387076, 1.000000000000000000, 0.8660254037844387076, 1.000000000000000000, 0.8660254037844387076, 1.000000000000000000, 0.8660254037844387076, 1.000000000000000000, 0.8660254037844387076, 1.000000000000000000, 0.8660254037844387076, 1.000000000000000000, 0.8660254037844387076, 1.000000000000000000, 0.8660254037844387076, 1.000000000000000000, 0.8660254037844387076, 1.000000000000000000, 0.8660254037844387076, 1.000000000000000000, 0.8660254037844387076, 1.000000000000000000, 0.8660254037844387076, 1.000000000000000000, 0.8660254037844387076, 1.000000000000000000, 0.8660254037844387076, 1.000000000000000000, 0.8660254037844387076, 1.000000000000000000, 0.8660254037844387076, 1.000000000000000000, 0.8660254037844387076, 1.000000000000000000, 0.8660254037844387076, 1.000000000000000000, 0.8660254037844387076, 1.000000000000000000, 0.8660254037844387076, 1.000000000000000000, 0.8660254037844387076, 1.000000000000000000, 0.8660254037844387076, 1.000000000000000000, 0.8660254037844387076, 1.000000000000000000, 0.8660254037844387076, 1.000000000000000000, 0.8660254037844387076, 1.000000000000000000, 0.8660254037844387076, 1.000000000000000000, 0.8660254037844387076, 1.000000000000000000, 0.8660254037844387076, 1.000000000000000000, 0.8660254037844387076, 1.000000000000000000, 0.8660254037844387076, 1.000000000000000000, 0.8660254037844387076, 1.000000000000000000, 0.8660254037844387076, 1.000000000000000000, 0.8660254037844387076, 1.000000000000000000, 0.8660254037844387076, 1.000000000000000000, 0.8660254037844387076, 1.000000000000000000, 0.8660254037844387076, 1.000000000000000000, 0.8660254037844387076, 1.000000000000000000, 0.8660254037844387076, 1.000000000000000000, 0.8660254037844387076, 1.000000000000000000, 0.8660254037844387076, 1.000000000000000000, 0.8660254037844387076, 1.000000000000000000) ) ) 
 REPRESENTATION_ITEM ( '' )  SURFACE ( )  );
#56224 = CARTESIAN_POINT ( 'NONE',  ( 6.030679399980265920, 5.930214142932100252, -0.7998128361456281477 ) ) ;
#56225 = CARTESIAN_POINT ( 'NONE',  ( -0.04006801626467436372, -6.479296433800352695, 11.00029612940780410 ) ) ;
#56226 = EDGE_CURVE ( 'NONE', #142172, #108790, #82771, .T. ) ;
#56227 = DIRECTION ( 'NONE',  ( -3.330669073875472579E-16, 1.665334536937734318E-16, 1.000000000000000000 ) ) ;
#56228 = CARTESIAN_POINT ( 'NONE',  ( 3.979481780810941949, 4.601482484822914998, 1.199719254218464037 ) ) ;
#56229 = VERTEX_POINT ( 'NONE', #67556 ) ;
#56230 = CARTESIAN_POINT ( 'NONE',  ( -0.1353477234830356701, -0.1462924468558861324, -1.883848219957585446 ) ) ;
#56231 = PLANE ( 'NONE',  #35128 ) ;
#56232 = CARTESIAN_POINT ( 'NONE',  ( 1.872871967411074756, 3.299999999999997158, -0.4000000000000131783 ) ) ;
#56233 = VECTOR ( 'NONE', #64652, 1000.000000000000000 ) ;
#56234 = CARTESIAN_POINT ( 'NONE',  ( -6.486760921661624657, 6.767311426390788753, 0.2083394120615672529 ) ) ;
#56235 = CARTESIAN_POINT ( 'NONE',  ( -3.768803514918943609, 7.340761834139994058, 0.7216878364870317197 ) ) ;
#56236 = CARTESIAN_POINT ( 'NONE',  ( 3.871016551901614200, 4.474939717762034697, -1.199719254218446718 ) ) ;
#56237 = CARTESIAN_POINT ( 'NONE',  ( 3.151173496672290852, 1.691593242058259783, -1.008282029756089493 ) ) ;
#56238 = EDGE_CURVE ( 'NONE', #78671, #42462, #91647, .T. ) ;
#56239 = CARTESIAN_POINT ( 'NONE',  ( 4.622672832840883039, 0.3474877929729481840, 1.986098205159859909 ) ) ;
#56240 = CARTESIAN_POINT ( 'NONE',  ( -6.663996196316808174, 7.733415969579778171, -1.199719254218446718 ) ) ;
#56241 = CARTESIAN_POINT ( 'NONE',  ( -3.076612070176407698, 6.450603142078709773, -0.6987248798898172408 ) ) ;
#56242 = CARTESIAN_POINT ( 'NONE',  ( 4.435597005726048536, 0.9382243502508281763, -1.980580373504265301 ) ) ;
#56243 = CARTESIAN_POINT ( 'NONE',  ( 1.324887192667550062, 1.296481010641095777, 1.500000000000000888 ) ) ;
#56244 = CARTESIAN_POINT ( 'NONE',  ( 3.241151106802504511, -1.699520814979482264, 0.9069582849330155572 ) ) ;
#56245 = CARTESIAN_POINT ( 'NONE',  ( -9.657485491635913633, 10.16148791653038330, 1.040834085586084257E-14 ) ) ;
#56246 = ADVANCED_FACE ( 'NONE', ( #169358 ), #2557, .F. ) ;
#56247 = CARTESIAN_POINT ( 'NONE',  ( -0.1296875068448125057, 0.2507808023153486054, -1.861542470327881560 ) ) ;
#56248 = CARTESIAN_POINT ( 'NONE',  ( 0.000000000000000000, 15.50000000000019362, 0.000000000000000000 ) ) ;
#56249 = CARTESIAN_POINT ( 'NONE',  ( -6.748402495618347707, 15.51952511201470841, -9.932705302265116387 ) ) ;
#56250 = CARTESIAN_POINT ( 'NONE',  ( -4.796985430826090635, 14.48151950780699693, 11.00853662041797598 ) ) ;
#56251 = CARTESIAN_POINT ( 'NONE',  ( 3.825371897350130723, 7.614684313550482031, 0.7998128361456321445 ) ) ;
#56252 = EDGE_LOOP ( 'NONE', ( #122776, #87016, #193789, #87725 ) ) ;
#56253 = CARTESIAN_POINT ( 'NONE',  ( 4.367134877377630175, 7.148722219365612141, -1.082531754730548412 ) ) ;
#56254 = ORIENTED_EDGE ( 'NONE', *, *, #80870, .F. ) ;
#56256 = CARTESIAN_POINT ( 'NONE',  ( 3.246742594617262334, 1.964541544574874621, 0.4388061624774098890 ) ) ;
#56255 = CARTESIAN_POINT ( 'NONE',  ( 6.620655732516645742, 0.007553340620044741646, 1.826407896915737794 ) ) ;
#56257 = CARTESIAN_POINT ( 'NONE',  ( 4.974093195743899187, 1.996273031041963408, 1.139003188958290780 ) ) ;
#56259 = CARTESIAN_POINT ( 'NONE',  ( 3.151044791815108770, 1.598572158793242659, -0.9524303787414812872 ) ) ;
#56258 = DIRECTION ( 'NONE',  ( 0.3162277660168373861, -0.9486832980505139901, 0.000000000000000000 ) ) ;
#56260 = CARTESIAN_POINT ( 'NONE',  ( -1.642778471875000035, -0.1677083328553742592, -2.845375778867859751 ) ) ;
#56261 = CARTESIAN_POINT ( 'NONE',  ( 4.000000000000001776, 5.499999999999998224, -2.024999999999999023 ) ) ;
#56262 = CYLINDRICAL_SURFACE ( 'NONE', #33226, 0.3999999999999996336 ) ;
#56263 = CARTESIAN_POINT ( 'NONE',  ( -7.152089726408780379, 8.302858421353754181, -1.199719254218446718 ) ) ;
#56264 = CARTESIAN_POINT ( 'NONE',  ( -3.512971199716682591, 7.112567143062499930, 0.000000000000000000 ) ) ;
#56265 = CARTESIAN_POINT ( 'NONE',  ( 6.146049400653379458, 0.6566722887273982456, 1.984991666494940743 ) ) ;
#56266 = CARTESIAN_POINT ( 'NONE',  ( 4.636525346193557162, 7.392734756325715750, -1.082531754730549078 ) ) ;
#56267 = EDGE_LOOP ( 'NONE', ( #91338, #203666, #21572, #80382 ) ) ;
#56268 = AXIS2_PLACEMENT_3D ( 'NONE', #50126, #116247, #117313 ) ;
#56269 = FILL_AREA_STYLE_COLOUR ( '', #81137 ) ;
#56270 = CARTESIAN_POINT ( 'NONE',  ( 0.4465194593917913846, 3.080450244942120719, -0.4155024747329958412 ) ) ;
#56271 = CARTESIAN_POINT ( 'NONE',  ( 0.9964003531478006215, -0.4411313887022934033, -1.771462291394958255 ) ) ;
#56272 = CARTESIAN_POINT ( 'NONE',  ( -5.949330478298285207, 5.835307067636438028, 0.7998128361456341429 ) ) ;
#56273 = CARTESIAN_POINT ( 'NONE',  ( 2.144752260294139568, 0.7423094788623717522, 1.567400511497107018 ) ) ;
#56274 = CARTESIAN_POINT ( 'NONE',  ( 6.724721492623498165, -6.244189044378178011, 7.341412881700131621 ) ) ;
#56275 = CARTESIAN_POINT ( 'NONE',  ( -7.217017841176048165, 7.314275657660511243, 1.040834085586084257E-14 ) ) ;
#56276 = CARTESIAN_POINT ( 'NONE',  ( -3.239364772909965661E-16, -5.511313137147274333, -11.00000000000000178 ) ) ;
#56277 = CARTESIAN_POINT ( 'NONE',  ( 6.930535145478218695, -1.343193056793217988, 1.706537673033242664 ) ) ;
#56278 = CARTESIAN_POINT ( 'NONE',  ( 5.690036971771410101, -0.8169618954828453683, 1.632782195682795257 ) ) ;
#56279 = CARTESIAN_POINT ( 'NONE',  ( 3.678520109711844732, 1.247982904293298168, -1.513573691770610186 ) ) ;
#56280 = CARTESIAN_POINT ( 'NONE',  ( 0.6125000000000019318, -1.020833332650530778, -1.060881119635948444 ) ) ;
#56281 = CARTESIAN_POINT ( 'NONE',  ( -7.655550293210764856, 12.08322577538792331, 0.000000000000000000 ) ) ;
#56282 = CARTESIAN_POINT ( 'NONE',  ( 7.786460292950004636, 7.978625184730144149, 1.040834085586084257E-14 ) ) ;
#56283 = CARTESIAN_POINT ( 'NONE',  ( 3.492942606646631809, -2.044086983709763050, -0.5638711869686771072 ) ) ;
#56284 = CARTESIAN_POINT ( 'NONE',  ( -3.470524135418306511, 5.072030796119872953, -1.443375672974053447 ) ) ;
#56285 = CARTESIAN_POINT ( 'NONE',  ( -8.622095623286845978, 12.14652976288826913, 1.199719254218462483 ) ) ;
#56286 = CARTESIAN_POINT ( 'NONE',  ( 1.920843890195075510, -1.466934385316904565, 1.461102248941518855 ) ) ;
#56288 = CARTESIAN_POINT ( 'NONE',  ( -1.500000000000015099, 15.26041666734946745, -0.8660254037844309360 ) ) ;
#56287 = DIRECTION ( 'NONE',  ( 0.2684563758389304500, -5.821219718043054220E-15, -0.9632918427306581544 ) ) ;
#56290 = VERTEX_POINT ( 'NONE', #70760 ) ;
#56289 = CARTESIAN_POINT ( 'NONE',  ( 4.899211331842913353, -0.2710981195956448375, -2.204650271698949116 ) ) ;
#56291 = CARTESIAN_POINT ( 'NONE',  ( 1.881834863725037277, -0.6175646290925532744, -2.214118314682656852 ) ) ;
#56293 = CARTESIAN_POINT ( 'NONE',  ( 0.3210474040165818277, -1.749687966165301312, -0.8873976775175674847 ) ) ;
#56292 = CARTESIAN_POINT ( 'NONE',  ( 8.419250204406344196, 12.76628297187536809, 1.040834085586084257E-14 ) ) ;
#56295 = CARTESIAN_POINT ( 'NONE',  ( -3.285556943749998737, -3.580208332855374653, 1.896917185911908499 ) ) ;
#56294 = CARTESIAN_POINT ( 'NONE',  ( 5.551137550152489553, 5.441024994791534120, 0.7998128361456352531 ) ) ;
#56296 = CARTESIAN_POINT ( 'NONE',  ( 1.474311205794113012E-15, 15.00000000000000355, 11.68000000000000504 ) ) ;
#56297 = CARTESIAN_POINT ( 'NONE',  ( 6.251489360189885325, 1.835807759842246423, -0.1425652098738516838 ) ) ;
#56298 = DIRECTION ( 'NONE',  ( 1.224646799147353454E-16, 0.000000000000000000, -1.000000000000000000 ) ) ;
#56299 = CARTESIAN_POINT ( 'NONE',  ( 2.970861089138316036, -1.445268511421276214, 1.252435071843561731 ) ) ;
#56300 = CARTESIAN_POINT ( 'NONE',  ( -0.2104748580754166321, -0.006608320950486632102, -2.103482951484026309 ) ) ;
#56301 = CARTESIAN_POINT ( 'NONE',  ( 4.489066604428880503, 1.540008836363685241, -0.7767696631951895858 ) ) ;
#56302 = CARTESIAN_POINT ( 'NONE',  ( 2.290250256651988892, -0.7762311197250795214, -1.861343989391924358 ) ) ;
#56303 = CARTESIAN_POINT ( 'NONE',  ( 3.498943719384327355, -2.264459259401516267, 0.3945650996091658591 ) ) ;
#56304 = CARTESIAN_POINT ( 'NONE',  ( 3.427297576727184047, 0.05164501975941707818, 2.261966552586023749 ) ) ;
#56305 = CARTESIAN_POINT ( 'NONE',  ( 5.988920713192999123, -0.3073026951427524356, -2.083404400164515113 ) ) ;
#56306 = CARTESIAN_POINT ( 'NONE',  ( -5.153507786970267013, 8.066157280557016307, -1.082531754730549967 ) ) ;
#56307 = EDGE_LOOP ( 'NONE', ( #170664, #200986, #75474, #162678 ) ) ;
#56308 = CARTESIAN_POINT ( 'NONE',  ( 4.674921082483953327, 0.0007207667814621705445, -1.769921774705035755 ) ) ;
#56310 = CARTESIAN_POINT ( 'NONE',  ( 0.7445458516137266614, 0.6704725750066173884, 2.192023251310899923 ) ) ;
#56309 = CARTESIAN_POINT ( 'NONE',  ( 8.025500584646550806, 8.327781868367935658, 0.000000000000000000 ) ) ;
#56311 = CARTESIAN_POINT ( 'NONE',  ( 5.402248404572855378, 1.391679675130308880, -1.205515946264820615 ) ) ;
#56312 = CARTESIAN_POINT ( 'NONE',  ( -2.948008335967658322, 5.526761261015804116, 1.199719254218462483 ) ) ;
#56313 = CARTESIAN_POINT ( 'NONE',  ( 5.402338782601353806, 1.661146971675907524, -1.429436781345946095 ) ) ;
#56314 = CARTESIAN_POINT ( 'NONE',  ( -4.647747731386360215, 4.316793862905830892, 0.7998128361456341429 ) ) ;
#56315 = CARTESIAN_POINT ( 'NONE',  ( -11.84668730067608600, 19.00000000000000000, 1.319999999999998286 ) ) ;
#56316 = CARTESIAN_POINT ( 'NONE',  ( 6.074686117427479992, 1.393331124738606652, -1.531503843499823381 ) ) ;
#56317 = CARTESIAN_POINT ( 'NONE',  ( -11.33772463945036968, 13.40000000000000036, -3.600000000000002309 ) ) ;
#56318 = AXIS2_PLACEMENT_3D ( 'NONE', #100769, #70377, #151675 ) ;
#56319 = CARTESIAN_POINT ( 'NONE',  ( -1.402160292154681736E-14, -1.006249999317181620, 1.732050807568877637 ) ) ;
#56320 = CARTESIAN_POINT ( 'NONE',  ( 4.266181944680371707, 0.9094715277466745018, 1.698315803094905041 ) ) ;
#56321 = CARTESIAN_POINT ( 'NONE',  ( -1.364683531250010295, 10.38020833367473195, 0.7879004041258445001 ) ) ;
#56322 = CARTESIAN_POINT ( 'NONE',  ( -3.307826292054316664, 4.882216645528547616, -1.443375672974059665 ) ) ;
#56323 = CARTESIAN_POINT ( 'NONE',  ( 1.143189493912871280, 2.142763695547444058, 0.5857495978145771387 ) ) ;
#56325 = ORIENTED_EDGE ( 'NONE', *, *, #183211, .F. ) ;
#56324 = CARTESIAN_POINT ( 'NONE',  ( 2.905190055078214595, 6.611415174225076186, 0.7998128361456271485 ) ) ;
#56328 = VECTOR ( 'NONE', #148632, 1000.000000000000000 ) ;
#56327 = CARTESIAN_POINT ( 'NONE',  ( 4.757850744675321764, 8.278777181968248300, -0.9081679900534248562 ) ) ;
#56326 = CARTESIAN_POINT ( 'NONE',  ( 1.255262969126037044E-15, -1.000000000000000888, -10.24999999999999822 ) ) ;
#56329 = CARTESIAN_POINT ( 'NONE',  ( 10.55232363013785246, 11.20546574478267132, 0.000000000000000000 ) ) ;
#56330 = CARTESIAN_POINT ( 'NONE',  ( -1.737500000000000266, -2.508333333333334636, -3.009438278150923907 ) ) ;
#56331 = CARTESIAN_POINT ( 'NONE',  ( -1.930226670627066099, 8.999999999999998224, 0.7750000000000013545 ) ) ;
#56332 = CARTESIAN_POINT ( 'NONE',  ( 11.57674487772738914, 8.193752454921764183, 2.992692998337922461 ) ) ;
#56333 = CARTESIAN_POINT ( 'NONE',  ( 9.205623113554615600, 11.76297960394566466, 1.443375672974076540 ) ) ;
#56334 = CARTESIAN_POINT ( 'NONE',  ( 1.557006721180295150, 1.605793932651664813, -1.126831546849601740 ) ) ;
#56335 = CARTESIAN_POINT ( 'NONE',  ( -0.6823417656250212460, 2.113541667008083991, 1.181850606188767472 ) ) ;
#56336 = FACE_OUTER_BOUND ( 'NONE', #145384, .T. ) ;
#56337 = CARTESIAN_POINT ( 'NONE',  ( 6.637165056451467038, -0.09505199798197358496, -1.959668910398344233 ) ) ;
#56338 = CARTESIAN_POINT ( 'NONE',  ( -7.133561379084627063, 11.47423870890741782, 0.7998128361456481317 ) ) ;
#56339 = CARTESIAN_POINT ( 'NONE',  ( -3.402733366905605905, 6.913679994791092298, 0.7216878364870317197 ) ) ;
#56340 = CARTESIAN_POINT ( 'NONE',  ( 0.2161854901324336276, -2.218109922327567318, 0.4452641707137113825 ) ) ;
#56342 = ORIENTED_EDGE ( 'NONE', *, *, #67389, .T. ) ;
#56341 = CARTESIAN_POINT ( 'NONE',  ( -7.040761844198392794, 7.108643661186573759, -0.7998128361456291469 ) ) ;
#56343 = CARTESIAN_POINT ( 'NONE',  ( 1.364683531249990311, 5.613541667008087543, 0.7879004041258500513 ) ) ;
#56344 = CARTESIAN_POINT ( 'NONE',  ( 1.071320448993583918, 1.804315561281001123, -0.4931735697189034151 ) ) ;
#56345 = CARTESIAN_POINT ( 'NONE',  ( 6.802075984838630518, -1.546572159107060251, 0.7837757703139431875 ) ) ;
#56347 = CARTESIAN_POINT ( 'NONE',  ( 4.195009555701286530, 1.760677850468267414, 1.304791629949946019 ) ) ;
#56346 = CARTESIAN_POINT ( 'NONE',  ( -1.360316468750007779, 2.390625000341400685, -1.734723475976807094E-15 ) ) ;
#56348 = CARTESIAN_POINT ( 'NONE',  ( 4.208297055918253093, -2.301676378859803584, 0.1658454734064350733 ) ) ;
#56349 = CARTESIAN_POINT ( 'NONE',  ( 0.3036813079041804087, -0.5503025168475895734, 1.985974332091578809 ) ) ;
#56350 = CARTESIAN_POINT ( 'NONE',  ( 2.624863168539525393, -1.811862388431908721, 0.6992392096202125762 ) ) ;
#56351 = CARTESIAN_POINT ( 'NONE',  ( -4.731432421044873493, 7.503459676985569260, -1.082531754730548412 ) ) ;
#56352 = CARTESIAN_POINT ( 'NONE',  ( 4.992489932941452935, -1.175987964647656536, 1.764448611491518548 ) ) ;
#56353 = CARTESIAN_POINT ( 'NONE',  ( 1.360316468749949825, 0.2447916670081152490, 0.7853790794158739264 ) ) ;
#56354 = CARTESIAN_POINT ( 'NONE',  ( 3.850232551101365086, 0.2440307281281335616, -2.001511205109906655 ) ) ;
#56355 = CARTESIAN_POINT ( 'NONE',  ( -5.219525951136856357, 6.152163700156858539, -1.082531754730543971 ) ) ;
#56356 = CARTESIAN_POINT ( 'NONE',  ( -5.420227550413282636, 9.545625585449309725, 0.7998128361456291469 ) ) ;
#56357 = CARTESIAN_POINT ( 'NONE',  ( 10.42352117080803708, 11.05519620889787724, -0.7998128361456281477 ) ) ;
#56358 = CARTESIAN_POINT ( 'NONE',  ( 0.5569169099325711469, -1.540613122784354916, -0.9793164655157863274 ) ) ;
#56359 = CARTESIAN_POINT ( 'NONE',  ( -6.720001414228860881, 7.869031733802326123, -1.199719254218452047 ) ) ;
#56360 = CARTESIAN_POINT ( 'NONE',  ( -6.168033539574335755, 6.160736982450306876, 0.7998128361456282587 ) ) ;
#56361 = CARTESIAN_POINT ( 'NONE',  ( -11.27970626620888517, 5.059847508428347851, 5.788342990380983544 ) ) ;
#56362 = VERTEX_POINT ( 'NONE', #134754 ) ;
#56363 = CARTESIAN_POINT ( 'NONE',  ( 5.770404196412942888, -1.309395467888567754, 1.591445708773833401 ) ) ;
#56364 = CARTESIAN_POINT ( 'NONE',  ( -5.872089928050201024, 8.904503111816948646, 1.082531754730550855 ) ) ;
#56365 = CARTESIAN_POINT ( 'NONE',  ( 3.199361063144932960, 6.676412307070378915, -0.7216878364870045193 ) ) ;
#56366 = CARTESIAN_POINT ( 'NONE',  ( -3.228813138348844536, 6.918699094715619502, 0.7998128361456341429 ) ) ;
#56368 = CARTESIAN_POINT ( 'NONE',  ( -10.62011439820619429, 11.28455497419572318, -0.7998128361456221525 ) ) ;
#56367 = B_SPLINE_CURVE_WITH_KNOTS ( 'NONE', 3,
 ( #193402, #33034, #13578, #30924 ),
 .UNSPECIFIED., .F., .F.,
 ( 4, 4 ),
 ( 0.000000000000000000, 1.000000000000000000 ),
 .UNSPECIFIED. ) ;
#56369 = CARTESIAN_POINT ( 'NONE',  ( 5.602215259268515268, -0.9060462314097734726, 1.805096023085197121 ) ) ;
#56370 = CARTESIAN_POINT ( 'NONE',  ( 5.795613637301100241, 2.053263797698097637, -0.8479724704701059323 ) ) ;
#56371 = CARTESIAN_POINT ( 'NONE',  ( -5.164730172163054966, 4.990216387137135889, -0.7998128361456362523 ) ) ;
#56372 = VECTOR ( 'NONE', #126403, 1000.000000000000000 ) ;
#56373 = CARTESIAN_POINT ( 'NONE',  ( 4.821896187954575197, 8.777295985922343391, 0.7998128361456462443 ) ) ;
#56374 = CARTESIAN_POINT ( 'NONE',  ( 3.713790661510278923, -2.030684131657393365, 0.3505542424454102246 ) ) ;
#56375 = CARTESIAN_POINT ( 'NONE',  ( 3.568982563115063122, -0.9913999084223243941, 1.755768870528085834 ) ) ;
#56376 = ORIENTED_EDGE ( 'NONE', *, *, #108076, .T. ) ;
#56377 = CARTESIAN_POINT ( 'NONE',  ( 6.471393748265540147, 5.229711127717882491, 2.420000000000010587 ) ) ;
#56378 = CARTESIAN_POINT ( 'NONE',  ( 2.218730694130720771, 5.740269576461138890, 0.7998128361456462443 ) ) ;
#56380 = VERTEX_POINT ( 'NONE', #38293 ) ;
#56379 = CARTESIAN_POINT ( 'NONE',  ( -7.767895665986912057, 8.027242796598338614, -0.7998128361456362523 ) ) ;
#56381 = CARTESIAN_POINT ( 'NONE',  ( 4.985841187518467166, 7.931359929992748192, -1.059499378661461710 ) ) ;
#56382 = CARTESIAN_POINT ( 'NONE',  ( 4.341172599035714619, -1.163090190446917083, 1.646587424817484324 ) ) ;
#56383 = CARTESIAN_POINT ( 'NONE',  ( 3.538839456958355889, -1.395042877683351890, -1.201619466480362108 ) ) ;
#56384 = DIRECTION ( 'NONE',  ( 0.000000000000000000, -1.000000000000000000, 0.000000000000000000 ) ) ;
#56385 = CARTESIAN_POINT ( 'NONE',  ( 1.770602872417438967, 1.189155993293121716, 1.977591576486624314 ) ) ;
#56386 = CARTESIAN_POINT ( 'NONE',  ( 4.085803189671889157, 5.860132702740892263, -1.599625672291273171 ) ) ;
#56387 = CARTESIAN_POINT ( 'NONE',  ( 3.268983376858981327, -1.995845357749256976, -0.8305886511386084692 ) ) ;
#56388 = CARTESIAN_POINT ( 'NONE',  ( 9.447334110624092673, 9.916311305349925220, -0.7998128361456281477 ) ) ;
#56389 = CARTESIAN_POINT ( 'NONE',  ( -4.401593425930945713, 8.286942763561420122, 1.040834085586084257E-14 ) ) ;
#56390 = EDGE_CURVE ( 'NONE', #53890, #197321, #21958, .T. ) ;
#56391 = CARTESIAN_POINT ( 'NONE',  ( 3.286738001609066817, -2.216000729425780413, 0.6097190577039524051 ) ) ;
#56392 = CARTESIAN_POINT ( 'NONE',  ( 0.4999999999999622524, 2.999999999999960920, -0.4000000000000305533 ) ) ;
#56393 =( GEOMETRIC_REPRESENTATION_CONTEXT ( 3 ) GLOBAL_UNCERTAINTY_ASSIGNED_CONTEXT ( ( #188434 ) ) GLOBAL_UNIT_ASSIGNED_CONTEXT ( ( #137934, #42585, #71824 ) ) REPRESENTATION_CONTEXT ( 'NONE', 'WORKASPACE' ) );
#56394 = CARTESIAN_POINT ( 'NONE',  ( 2.834663617355744680, 0.2272019944037397543, 1.856728029318695627 ) ) ;
#56395 = AXIS2_PLACEMENT_3D ( 'NONE', #126151, #209424, #187849 ) ;
#56396 = CARTESIAN_POINT ( 'NONE',  ( 0.3331948752925878998, -1.804169345717737238, 0.7948754592718260126 ) ) ;
#56398 = CARTESIAN_POINT ( 'NONE',  ( -5.413448473606448985, 9.537716662508005427, 0.000000000000000000 ) ) ;
#56397 = CARTESIAN_POINT ( 'NONE',  ( -1.364683531250012516, 4.238541667008090208, -0.7879004041258300672 ) ) ;
#56400 = CARTESIAN_POINT ( 'NONE',  ( 2.139570144280181108, -1.970530345926827742, 0.9937953903183869286 ) ) ;
#56399 = CARTESIAN_POINT ( 'NONE',  ( -4.388035272317281077, 8.271124917678806199, 0.7998128361456481317 ) ) ;
#56401 = DIRECTION ( 'NONE',  ( 0.000000000000000000, -1.000000000000000000, 0.000000000000000000 ) ) ;
#56402 = CARTESIAN_POINT ( 'NONE',  ( 5.840865249388943248, 5.708764300575555062, 0.7998128361456341429 ) ) ;
#56403 = CARTESIAN_POINT ( 'NONE',  ( -4.252453736180621391, 8.112946458852704268, -0.7998128361456281477 ) ) ;
#56404 = CARTESIAN_POINT ( 'NONE',  ( 11.86145017354087372, 13.50485634456124551, 1.099999999999996980 ) ) ;
#56405 = CARTESIAN_POINT ( 'NONE',  ( 5.840691970153715218, 0.3840316513750040572, 1.933538979438324867 ) ) ;
#56406 = CARTESIAN_POINT ( 'NONE',  ( 6.041700318104039624, -1.667111694969125368, -1.595929347687746747 ) ) ;
#56407 = CARTESIAN_POINT ( 'NONE',  ( 0.3968290921660848070, 0.3316028935436679537, 1.933473477243151439 ) ) ;
#56408 = CARTESIAN_POINT ( 'NONE',  ( 3.362228078103552953, -2.060403055893737623, 0.09660672959950138139 ) ) ;
#56409 = CARTESIAN_POINT ( 'NONE',  ( 6.643132081016117851, 8.773406732650713025, 1.443375672974076540 ) ) ;
#56410 = VECTOR ( 'NONE', #15625, 1000.000000000000000 ) ;
#56411 = CARTESIAN_POINT ( 'NONE',  ( 7.075376061485196821, 9.347967719856493218, 1.599625672291268286 ) ) ;
#56412 = CARTESIAN_POINT ( 'NONE',  ( 6.602457619730756733, 9.686322408785807525, 1.082531754730558626 ) ) ;
#56413 = CARTESIAN_POINT ( 'NONE',  ( -1.364683531249997417, 3.321875000341423245, 1.214306433183764966E-14 ) ) ;
#56414 = CARTESIAN_POINT ( 'NONE',  ( -9.333041836230018262, 14.55305236562984383, 7.472413793098201751 ) ) ;
#56415 = CARTESIAN_POINT ( 'NONE',  ( 3.484082288587588838, 7.008587070086755411, -0.7216878364870267237 ) ) ;
#56416 = CARTESIAN_POINT ( 'NONE',  ( 5.723135995274492238, -1.960344405425541670, -0.9336216343173405763 ) ) ;
#56418 = CARTESIAN_POINT ( 'NONE',  ( 5.565905774130330386, -1.163279849954502287, 1.427249551226833502 ) ) ;
#56417 = FACE_OUTER_BOUND ( 'NONE', #142024, .T. ) ;
#56419 = FACE_OUTER_BOUND ( 'NONE', #46715, .T. ) ;
#56421 = CARTESIAN_POINT ( 'NONE',  ( 4.560489089606875268, 8.500000000000003553, -0.2119548090071901036 ) ) ;
#56420 = B_SPLINE_CURVE_WITH_KNOTS ( 'NONE', 3,
 ( #8175, #108953, #142484, #172832, #197326, #112960, #174973, #26554, #46846, #41777 ),
 .UNSPECIFIED., .F., .F.,
 ( 4, 3, 3, 4 ),
 ( 8.603168645141783524E-16, 3.125222853364259014E-05, 6.323671013787866575E-05, 9.524404753373414908E-05 ),
 .UNSPECIFIED. ) ;
#56422 = CARTESIAN_POINT ( 'NONE',  ( 0.5615140978009087736, 1.851110617189118734, -0.2680550677405246773 ) ) ;
#56423 = CARTESIAN_POINT ( 'NONE',  ( 0.8962371694669484246, -0.8134219682564158838, 2.111273946446708738 ) ) ;
#56424 = EDGE_CURVE ( 'NONE', #33823, #200465, #143113, .T. ) ;
#56426 = CARTESIAN_POINT ( 'NONE',  ( -4.095724654357025152, 7.689947244493171574, 0.7385042830605083042 ) ) ;
#56425 = AXIS2_PLACEMENT_3D ( 'NONE', #78190, #94472, #162661 ) ;
#56427 = CARTESIAN_POINT ( 'NONE',  ( 1.220146605508150803E-14, 11.43749999999999822, -1.499999999999998446 ) ) ;
#56428 = CARTESIAN_POINT ( 'NONE',  ( 5.678247172832384670, 7.430942480705488684, 1.324022058552588366 ) ) ;
#56429 = CARTESIAN_POINT ( 'NONE',  ( -1.115562610750309283E-14, 9.312500000000001776, 1.500000000000001554 ) ) ;
#56430 = CARTESIAN_POINT ( 'NONE',  ( 2.061070876156974041, 0.3059375065844106012, -1.743026645166842803 ) ) ;
#56431 = CARTESIAN_POINT ( 'NONE',  ( -0.07574839183086683192, -0.8175154495408327726, -1.727131953450977253 ) ) ;
#56433 = CARTESIAN_POINT ( 'NONE',  ( 2.987788816292748173, -1.913300742920095221, 0.09679331860494060080 ) ) ;
#56432 = CARTESIAN_POINT ( 'NONE',  ( -7.967387826325084355, 12.44703623068796361, 0.7998128361456481317 ) ) ;
#56434 = CARTESIAN_POINT ( 'NONE',  ( -5.586581854188635177, 5.810800913040471194, -0.4357733342581562863 ) ) ;
#56435 = CARTESIAN_POINT ( 'NONE',  ( 3.965261034597372891, 1.688065314258681893, 1.014448032605998584 ) ) ;
#56436 = CARTESIAN_POINT ( 'NONE',  ( 6.486581104273712484, -1.239329707167437622, 1.595369898402546838 ) ) ;
#56437 = CARTESIAN_POINT ( 'NONE',  ( -1.500000000000001110, 11.02083333333333393, 0.8660254037844418162 ) ) ;
#56438 = CARTESIAN_POINT ( 'NONE',  ( 2.817106861211693847, -0.1851908181382568019, 1.861470920997858380 ) ) ;
#56440 = EDGE_LOOP ( 'NONE', ( #27689, #115790, #199539, #92442, #96911 ) ) ;
#56439 = CARTESIAN_POINT ( 'NONE',  ( 0.01192831195480706721, -0.7772932952810689411, -1.650495136788888040 ) ) ;
#56442 = CARTESIAN_POINT ( 'NONE',  ( 2.901081683644312736, 6.328419697652925002, 0.7216878364870338292 ) ) ;
#56441 = CARTESIAN_POINT ( 'NONE',  ( 2.227434312139275896, 0.001603268854937638837, 2.207063162490217056 ) ) ;
#56443 = CARTESIAN_POINT ( 'NONE',  ( 1.364683531249990311, 3.696875000341416584, 1.214306433183764966E-14 ) ) ;
#56444 = CARTESIAN_POINT ( 'NONE',  ( 6.496542546517183325, 1.940334402339534581, 0.2891159199209930031 ) ) ;
#56445 = CARTESIAN_POINT ( 'NONE',  ( 7.456094412511537151, 10.78619501698377370, 1.199719254218460707 ) ) ;
#56446 = CARTESIAN_POINT ( 'NONE',  ( -7.769310276573702545, -5.221243112839676570, 7.769310276573728302 ) ) ;
#56447 = CARTESIAN_POINT ( 'NONE',  ( 9.695354081530210166, -7.357813805514500594, 9.269928574751062911E-15 ) ) ;
#56448 = CARTESIAN_POINT ( 'NONE',  ( 0.1747926744264677867, 2.047238405490480861, -2.272669950590770149 ) ) ;
#56449 = CARTESIAN_POINT ( 'NONE',  ( 1.734723475976807094E-15, 1.000000000000000888, 0.000000000000000000 ) ) ;
#56450 = ORIENTED_EDGE ( 'NONE', *, *, #2314, .T. ) ;
#56451 = CARTESIAN_POINT ( 'NONE',  ( 3.156751980976373329, -0.5984545454679365273, -1.982000093670479135 ) ) ;
#56452 = CARTESIAN_POINT ( 'NONE',  ( 1.499999999999987121, 3.795833333333356929, -0.8660254037844262731 ) ) ;
#56453 = CARTESIAN_POINT ( 'NONE',  ( 5.660692828905515839, 6.562895374266609849, -1.199719254218445830 ) ) ;
#56454 = CARTESIAN_POINT ( 'NONE',  ( -6.449404147558570166, 6.867377544759197150, 0.7074503392771516186 ) ) ;
#56455 = CARTESIAN_POINT ( 'NONE',  ( 0.8209702097039422997, 1.527776094787479444, -1.321057435245088341 ) ) ;
#56456 = CARTESIAN_POINT ( 'NONE',  ( 1.445103857048099627, 8.688264192037895128, 2.625611233228258179 ) ) ;
#56457 = CARTESIAN_POINT ( 'NONE',  ( -1.364683531250010295, 4.530208333674754506, 0.7879004041258379498 ) ) ;
#56459 = CARTESIAN_POINT ( 'NONE',  ( 8.839552966430002101, 11.33589776563360019, -1.443375672974052559 ) ) ;
#56458 = CARTESIAN_POINT ( 'NONE',  ( 0.07459516483345089710, 0.2549822845471191868, -1.790622017744479155 ) ) ;
#56460 = CARTESIAN_POINT ( 'NONE',  ( 4.886092203009785528, -0.1017338195800701617, 2.013677658187912556 ) ) ;
#56461 = CARTESIAN_POINT ( 'NONE',  ( 5.401554078093819378, -1.867474805896391032, 0.4264384668619321528 ) ) ;
#56462 = CARTESIAN_POINT ( 'NONE',  ( 6.539320575229233157, 0.001224430076711413356, 2.103502572931112091 ) ) ;
#56463 = CARTESIAN_POINT ( 'NONE',  ( 4.230150181147958044, 2.149441460308566754, 0.4267382380854707336 ) ) ;
#56464 = CARTESIAN_POINT ( 'NONE',  ( -0.7500000000000215383, 1.972916667349486453, 1.299038105676659116 ) ) ;
#56465 = CARTESIAN_POINT ( 'NONE',  ( 2.953266587970606594, -1.684550232849800544, 0.9053361341156559439 ) ) ;
#56466 = CARTESIAN_POINT ( 'NONE',  ( -6.403528624356093601, 6.365204904703887223, 1.040834085586084257E-14 ) ) ;
#56467 = CARTESIAN_POINT ( 'NONE',  ( 5.477130869796502211, 5.492333557625114437, 1.040834085586084257E-14 ) ) ;
#56469 = CARTESIAN_POINT ( 'NONE',  ( 0.1050925082292548940, -0.09611335402343046397, 2.014234898253919326 ) ) ;
#56468 = CARTESIAN_POINT ( 'NONE',  ( 6.825078400183573812, 0.002648415797040087893, 1.855566311045192540 ) ) ;
#56470 = CARTESIAN_POINT ( 'NONE',  ( 1.364683531249997417, 11.54687500034139802, 2.602085213965210642E-15 ) ) ;
#56472 = CARTESIAN_POINT ( 'NONE',  ( -6.631873415740034083, 7.766215735565355160, 1.199719254218452047 ) ) ;
#56471 = CARTESIAN_POINT ( 'NONE',  ( 6.356982542327763497, 0.3766756592470664744, -2.158781491689326426 ) ) ;
#56474 = VERTEX_POINT ( 'NONE', #136873 ) ;
#56473 = CARTESIAN_POINT ( 'NONE',  ( 2.502614896622682661, 1.386922750403916105, -1.025098202461205865 ) ) ;
#56475 = CARTESIAN_POINT ( 'NONE',  ( 1.734723475976807094E-15, 0.7598076211376200151, 3.469446951953614189E-15 ) ) ;
#56476 = CARTESIAN_POINT ( 'NONE',  ( 5.960781091502512119, 10.10599504006161986, 0.7998128361456462443 ) ) ;
#56477 = CARTESIAN_POINT ( 'NONE',  ( 6.173040012923759257, 6.096301524699504704, -0.7998128361456281477 ) ) ;
#56478 = LINE ( 'NONE', #155047, #147494 ) ;
#56479 = CARTESIAN_POINT ( 'NONE',  ( 0.5374593765826127800, 1.831924746014142791, -0.7026076897959919743 ) ) ;
#56480 = EDGE_CURVE ( 'NONE', #29860, #156791, #18650, .T. ) ;
#56481 = DIRECTION ( 'NONE',  ( -0.000000000000000000, 1.000000000000000000, 9.023263958591317418E-17 ) ) ;
#56482 = CARTESIAN_POINT ( 'NONE',  ( 6.114890974963323345, 7.092793211334054604, 1.199719254218462483 ) ) ;
#56483 = CARTESIAN_POINT ( 'NONE',  ( -0.7500000000000006661, 10.70833333333333393, -1.299038105676657340 ) ) ;
#56484 = ORIENTED_EDGE ( 'NONE', *, *, #160843, .F. ) ;
#56486 = CIRCLE ( 'NONE', #163795, 11.00000000000000000 ) ;
#56485 = CARTESIAN_POINT ( 'NONE',  ( 0.4366904681730480742, -5.787668213791780758, 10.40319425600974235 ) ) ;
#56487 = ORIENTED_EDGE ( 'NONE', *, *, #46380, .F. ) ;
#56488 = CARTESIAN_POINT ( 'NONE',  ( 2.279683508022036342, 1.776238746767303978, -0.3545518163566608871 ) ) ;
#56489 = ORIENTED_EDGE ( 'NONE', *, *, #10791, .T. ) ;
#56490 = CARTESIAN_POINT ( 'NONE',  ( 9.028840231696797503, 12.62106513936658203, -1.199719254218446718 ) ) ;
#56491 = AXIS2_PLACEMENT_3D ( 'NONE', #36403, #169613, #187986 ) ;
#56492 = CARTESIAN_POINT ( 'NONE',  ( 4.037295881819344956, 7.932205305423046582, -0.7998128361456362523 ) ) ;
#56493 = CARTESIAN_POINT ( 'NONE',  ( 3.527799351415283002, -1.784095038623861651, 0.3127521441018704107 ) ) ;
#56494 = CARTESIAN_POINT ( 'NONE',  ( 7.797347741190739256, 8.269529584243604958, 0.7216878364870267237 ) ) ;
#56495 = CARTESIAN_POINT ( 'NONE',  ( -1.214306433183764966E-14, 3.299999999999969624, -3.122502256758252770E-14 ) ) ;
#56496 = CARTESIAN_POINT ( 'NONE',  ( 5.086710258240730198, 6.515995995190169587, 1.216687342998038934 ) ) ;
#56498 = CARTESIAN_POINT ( 'NONE',  ( 1.364683531249997417, 14.48437500034140157, 2.602085213965210642E-15 ) ) ;
#56497 = CARTESIAN_POINT ( 'NONE',  ( 5.230833165924736683, -1.752262279689630553, -0.6273003976000991466 ) ) ;
#56499 = CARTESIAN_POINT ( 'NONE',  ( 3.181152667880298157, 1.511915621606011007, 1.176196041047285812 ) ) ;
#56500 = CARTESIAN_POINT ( 'NONE',  ( -10.96033999287893224, 4.843182460328104177, 4.379153535238802242 ) ) ;
#56501 = CARTESIAN_POINT ( 'NONE',  ( 6.174897528274166270, 6.957956273452501783, 0.8961316764096085574 ) ) ;
#56502 = CARTESIAN_POINT ( 'NONE',  ( 7.825489347732291989, 14.97139610117899444, 9.977962224420885207 ) ) ;
#56503 = CARTESIAN_POINT ( 'NONE',  ( 6.720112740279237329, -7.154544010627095219, -6.827626583076776612 ) ) ;
#56504 = CARTESIAN_POINT ( 'NONE',  ( 0.9311234436981525864, -2.653119629485602537, 3.474999999999998757 ) ) ;
#56505 = CARTESIAN_POINT ( 'NONE',  ( 7.809133291791403586, 8.213003049952529722, -0.7216878364870257245 ) ) ;
#56506 = ADVANCED_FACE ( 'NONE', ( #3621 ), #200763, .F. ) ;
#56507 = CARTESIAN_POINT ( 'NONE',  ( -3.079673448598517549, 6.744702790006905424, 1.040834085586084257E-14 ) ) ;
#56508 = DIRECTION ( 'NONE',  ( 0.5773502691896272854, 0.000000000000000000, -0.8164965809277250353 ) ) ;
#56509 = CARTESIAN_POINT ( 'NONE',  ( 1.658266814308974268, -1.477475772113973740, 1.479395487768909501 ) ) ;
#56510 = CARTESIAN_POINT ( 'NONE',  ( 6.405299695295086693, 1.602013123205116019, 1.069544239394400797 ) ) ;
#56511 = CARTESIAN_POINT ( 'NONE',  ( -4.069418662396130593, 7.899405539437467816, -0.7998128361456281477 ) ) ;
#56512 = EDGE_CURVE ( 'NONE', #40754, #88097, #46295, .T. ) ;
#56513 = CARTESIAN_POINT ( 'NONE',  ( 1.975362765405625609, 1.747911882041437659, -0.5268472171036930884 ) ) ;
#56514 = CARTESIAN_POINT ( 'NONE',  ( 3.475398437264758389, 0.05438942809191969763, -2.206374867412825402 ) ) ;
#56515 = CARTESIAN_POINT ( 'NONE',  ( 1.500000000000001332, 10.37499999999999467, 0.000000000000000000 ) ) ;
#56516 = CARTESIAN_POINT ( 'NONE',  ( 0.9668906521006037647, -1.505869814250645478, 1.178657042999963878 ) ) ;
#56517 = CARTESIAN_POINT ( 'NONE',  ( 1.187880472884972560, -1.246972491003460748, -1.524547227783664249 ) ) ;
#56518 = CARTESIAN_POINT ( 'NONE',  ( 3.597155123818120082, -0.5607282099057244729, 1.859368625674643782 ) ) ;
#56519 = ORIENTED_EDGE ( 'NONE', *, *, #151772, .T. ) ;
#56520 = DIRECTION ( 'NONE',  ( 0.000000000000000000, 8.546850786086437571E-32, 1.000000000000000000 ) ) ;
#56522 = CARTESIAN_POINT ( 'NONE',  ( 6.842638030098166624, -1.824918384715786823, -0.3633994975895912805 ) ) ;
#56521 = CARTESIAN_POINT ( 'NONE',  ( -3.494969737272722643, 7.299491470118629088, -0.7998128361456481317 ) ) ;
#56523 = CARTESIAN_POINT ( 'NONE',  ( 3.874598038455354665, 7.742391154831717692, -0.7998128361456362523 ) ) ;
#56524 = CARTESIAN_POINT ( 'NONE',  ( 6.558483974469879740, -6.776276029125230416, 6.864213375410075813 ) ) ;
#56525 = CARTESIAN_POINT ( 'NONE',  ( -7.834948825496938163, -5.823938088759704534, -7.720982897393569466 ) ) ;
#56526 = CARTESIAN_POINT ( 'NONE',  ( -5.611095471209320174, 7.639640364534566075, 1.599625672291263179 ) ) ;
#56527 = CARTESIAN_POINT ( 'NONE',  ( 3.052458795248469414, -1.657928338269051505, 1.433322580492613296 ) ) ;
#56528 = CARTESIAN_POINT ( 'NONE',  ( 2.738383840280328663, 5.178236332760252303, 1.082531754730548412 ) ) ;
#56529 = CARTESIAN_POINT ( 'NONE',  ( 7.550965208168244125, 7.774157262476569130, -0.7998128361456341429 ) ) ;
#56530 = CARTESIAN_POINT ( 'NONE',  ( -3.399419719642636117, 0.06547992991065912372, 0.000000000000000000 ) ) ;
#56531 = CARTESIAN_POINT ( 'NONE',  ( 3.334410585898534674, 1.781380905032422746, 0.3990451814587444024 ) ) ;
#56532 = SURFACE_STYLE_FILL_AREA ( #72763 ) ;
#56533 = CARTESIAN_POINT ( 'NONE',  ( -10.16825202056928390, 10.96530823352674133, 0.7216878364870438212 ) ) ;
#56534 = CARTESIAN_POINT ( 'NONE',  ( -4.601933621211449221, 8.477299672830683974, 0.2703350597391823706 ) ) ;
#56535 = CARTESIAN_POINT ( 'NONE',  ( 0.4350687514514690046, -5.166862915010145052, 10.91132967064558024 ) ) ;
#56536 = CARTESIAN_POINT ( 'NONE',  ( 4.047608660086319254, 0.6306619223146043840, -1.761260876548931709 ) ) ;
#56537 = CARTESIAN_POINT ( 'NONE',  ( 9.576136569953906275, 10.06658084123472641, 0.000000000000000000 ) ) ;
#56538 = CARTESIAN_POINT ( 'NONE',  ( 1.594233254470639238, -1.917152233794093164, -0.1895178900164773139 ) ) ;
#56539 = CARTESIAN_POINT ( 'NONE',  ( 6.649272889308863732, 1.708415183241232205, -0.9640671636572254455 ) ) ;
#56540 = CARTESIAN_POINT ( 'NONE',  ( -1.364683531250014514, 9.401041667008062319, -0.7879004041258335089 ) ) ;
#56541 = CARTESIAN_POINT ( 'NONE',  ( -6.358937740009323214, 7.377514437221045718, -1.199719254218446718 ) ) ;
#56542 = CARTESIAN_POINT ( 'NONE',  ( 4.578903193113299963, 6.365139696764064325, 1.599625672291267398 ) ) ;
#56543 = CARTESIAN_POINT ( 'NONE',  ( -5.953438849732214599, 6.118302544208584770, 0.7216878364870257245 ) ) ;
#56544 = AXIS2_PLACEMENT_3D ( 'NONE', #39496, #138078, #172714 ) ;
#56545 = TOROIDAL_SURFACE ( 'NONE', #194914, 11.92000000000000171, 0.08000000000000000167 ) ;
#56546 = CARTESIAN_POINT ( 'NONE',  ( 0.4392562211190715882, -1.791127875450468920, -1.128673114062600957 ) ) ;
#56547 = CARTESIAN_POINT ( 'NONE',  ( -0.6125000000000383471, 0.6041666673494219264, 1.060881119635901593 ) ) ;
#56548 = CARTESIAN_POINT ( 'NONE',  ( 0.9311234436981525864, -2.346869630441518861, 3.474999999999998757 ) ) ;
#56549 = CARTESIAN_POINT ( 'NONE',  ( 4.627825472248149552, 2.009385113269086087, -0.4979276649561757417 ) ) ;
#56551 = CARTESIAN_POINT ( 'NONE',  ( 0.6823417656249882723, 2.238541667008084435, -1.181850606188749264 ) ) ;
#56550 = CARTESIAN_POINT ( 'NONE',  ( -0.006632162239710717895, -1.840811702136424088, -0.04651623371411393176 ) ) ;
#56553 = ORIENTED_EDGE ( 'NONE', *, *, #18226, .T. ) ;
#56552 = CIRCLE ( 'NONE', #18493, 1.850000000000000089 ) ;
#56554 = CARTESIAN_POINT ( 'NONE',  ( 5.572921396849181974, -1.036564899910274784, 2.051751470549934453 ) ) ;
#56555 = CARTESIAN_POINT ( 'NONE',  ( 6.643132081016117851, 8.773406732650713025, 1.443375672974076540 ) ) ;
#56557 = CARTESIAN_POINT ( 'NONE',  ( 1.224999999999982991, 1.395833333333318826, -0.7072540797572817173 ) ) ;
#56556 = CARTESIAN_POINT ( 'NONE',  ( 5.072158865288245444, 5.090142562357324429, 0.7216878364870338292 ) ) ;
#56558 = CARTESIAN_POINT ( 'NONE',  ( 0.2524361811976470471, 0.8832210619409311958, 2.115471854006613750 ) ) ;
#56559 = CARTESIAN_POINT ( 'NONE',  ( -0.06712503953322571104, -9.995102581657556939, -9.579544693637531694 ) ) ;
#56560 = CARTESIAN_POINT ( 'NONE',  ( -5.725286006720766707, 9.901527117808042178, 0.7998128361456291469 ) ) ;
#56561 = CARTESIAN_POINT ( 'NONE',  ( 4.874914055504836696, 1.811399353594527639, -0.7004420144864877962 ) ) ;
#56562 = ORIENTED_EDGE ( 'NONE', *, *, #57451, .F. ) ;
#56563 = CARTESIAN_POINT ( 'NONE',  ( 8.229436053370658755, 12.54483312900040026, 0.7216878364870438212 ) ) ;
#56564 = CIRCLE ( 'NONE', #156768, 7.426656976154414558 ) ;
#56565 = ORIENTED_EDGE ( 'NONE', *, *, #84212, .F. ) ;
#56566 = CARTESIAN_POINT ( 'NONE',  ( 0.05298979808228323346, 0.3483158054882686261, 1.982706882182909025 ) ) ;
#56567 = B_SPLINE_CURVE_WITH_KNOTS ( 'NONE', 3,
 ( #75548, #9475, #203643, #52095, #26783, #53157, #119286, #92888, #102977, #158933 ),
 .UNSPECIFIED., .F., .F.,
 ( 4, 3, 3, 4 ),
 ( 0.000000000000000000, 8.893179197954857176E-05, 0.0001334007970840202239, 0.0001778705873658964021 ),
 .UNSPECIFIED. ) ;
#56568 = CARTESIAN_POINT ( 'NONE',  ( 5.928922775424462444, -1.700964743930567513, 1.082835439959836776 ) ) ;
#56569 = CARTESIAN_POINT ( 'NONE',  ( -8.157201976916404362, 12.66848607304450702, -0.7998128361456281477 ) ) ;
#56570 = CARTESIAN_POINT ( 'NONE',  ( -1.642778471874998480, -0.8385416661887100664, 2.845375778867863303 ) ) ;
#56572 = CARTESIAN_POINT ( 'NONE',  ( 1.041466456679561059, 0.7221788661597589032, -1.615996624379830493 ) ) ;
#56571 = CARTESIAN_POINT ( 'NONE',  ( 3.117214558520535306, -2.014654392230078805, 0.5582205872023697779 ) ) ;
#56573 = CARTESIAN_POINT ( 'NONE',  ( 6.399064592084179992, -0.9530083391863402031, -1.777013033299412292 ) ) ;
#56575 = CARTESIAN_POINT ( 'NONE',  ( 4.154423454741348110, -1.699848520643287175, 1.538017723768041023 ) ) ;
#56574 =( NAMED_UNIT ( * ) PLANE_ANGLE_UNIT ( ) SI_UNIT ( $, .RADIAN. ) );
#56576 = CARTESIAN_POINT ( 'NONE',  ( 2.220290661370280638, -0.001068742171999540608, 1.740516466435287235 ) ) ;
#56577 = CARTESIAN_POINT ( 'NONE',  ( 5.190073875932979419, 4.949507698210251938, 0.7998128361456341429 ) ) ;
#56578 = CARTESIAN_POINT ( 'NONE',  ( 0.4640311867334303564, 2.877219473291478646, 2.027578619373314073 ) ) ;
#56579 = CARTESIAN_POINT ( 'NONE',  ( 1.704000572024838123, -1.251590786289292101, -1.200144391261132482 ) ) ;
#56580 = CARTESIAN_POINT ( 'NONE',  ( 0.6801582343749761339, 1.838541667008058988, -1.178068619123876282 ) ) ;
#56581 = CARTESIAN_POINT ( 'NONE',  ( 1.574410529035878969, 1.253355123444719998, -1.375888611855519583 ) ) ;
#56582 = CARTESIAN_POINT ( 'NONE',  ( 2.260437933566094681, -2.170709518246512815, 0.05174924654302060639 ) ) ;
#56583 = CARTESIAN_POINT ( 'NONE',  ( 4.299907273828439180, 8.168308919441841454, 1.040834085586084257E-14 ) ) ;
#56584 = CARTESIAN_POINT ( 'NONE',  ( 3.257046257486408969, 0.04465439498414420366, -2.016188763087948033 ) ) ;
#56585 = CARTESIAN_POINT ( 'NONE',  ( 1.906250000000001332, 1.895863743164044823, -0.7852924748300882385 ) ) ;
#56586 = CARTESIAN_POINT ( 'NONE',  ( 1.499999999999987121, 3.327083334016150751, -0.8660254037844262731 ) ) ;
#56587 = CARTESIAN_POINT ( 'NONE',  ( 0.4813100693330485957, 1.798698175156054457, -0.6901501906162701427 ) ) ;
#56588 = CARTESIAN_POINT ( 'NONE',  ( -1.402160292154681736E-14, 14.67187500034139980, 1.575800808251682339 ) ) ;
#56589 = CARTESIAN_POINT ( 'NONE',  ( 4.746434557108095476, 1.141014917558682340, -1.905822037654863133 ) ) ;
#56590 = VERTEX_POINT ( 'NONE', #104371 ) ;
#56591 = CARTESIAN_POINT ( 'NONE',  ( 1.499999999999989120, 0.5250000000000185629, 0.000000000000000000 ) ) ;
#56592 = CARTESIAN_POINT ( 'NONE',  ( 8.423693512792301163, 8.722063941212843119, 0.7998128361456481317 ) ) ;
#56593 = CARTESIAN_POINT ( 'NONE',  ( -1.402160292154681736E-14, -0.05312499965857903073, -1.575800808251665908 ) ) ;
#56594 = CARTESIAN_POINT ( 'NONE',  ( 0.6807244054014843782, 1.099941690210548106, 1.929793933578232146 ) ) ;
#56595 = CARTESIAN_POINT ( 'NONE',  ( 5.723093114104088386, -1.772945450647535948, -0.8403097561825513262 ) ) ;
#56596 = CARTESIAN_POINT ( 'NONE',  ( 9.910647101909615841, 10.66476916175714607, 0.000000000000000000 ) ) ;
#56597 = CARTESIAN_POINT ( 'NONE',  ( -1.378728738066232307, 3.613591550242559070, -0.5908528300941753297 ) ) ;
#56598 = CARTESIAN_POINT ( 'NONE',  ( 5.852851842114176861, -1.788828801601877849, 1.385077142625196434 ) ) ;
#56599 = CARTESIAN_POINT ( 'NONE',  ( -4.828112100242291760, 6.726159765073026264, -1.443375672974066548 ) ) ;
#56600 = CARTESIAN_POINT ( 'NONE',  ( 3.191897189531978096, -1.383228714077057830, -1.530316362279722231 ) ) ;
#56601 = CARTESIAN_POINT ( 'NONE',  ( -6.067437437315529536, 7.037430750744921859, 1.199719254218450271 ) ) ;
#56602 = CARTESIAN_POINT ( 'NONE',  ( -1.201851678989727383E-14, 2.243750000682818158, 1.732050807568877637 ) ) ;
#56603 = CARTESIAN_POINT ( 'NONE',  ( 1.364683531249990311, 5.176041667008085767, 0.7879004041258500513 ) ) ;
#56604 = CARTESIAN_POINT ( 'NONE',  ( 5.255093269098372488, -1.579555527043162488, -1.001684657140684775 ) ) ;
#56605 = CARTESIAN_POINT ( 'NONE',  ( 3.340171489122942816, 0.4179119503955433523, -1.682892220811042616 ) ) ;
#56606 = CARTESIAN_POINT ( 'NONE',  ( 3.122313433385078607, 0.04571620936353942150, 1.740018996352102443 ) ) ;
#56607 = CARTESIAN_POINT ( 'NONE',  ( 0.2402843302407534631, 2.286812847775396840, 0.1605059593563825382 ) ) ;
#56608 = CARTESIAN_POINT ( 'NONE',  ( 0.6823417656249899377, 4.238541667008085767, -1.181850606188754593 ) ) ;
#56609 = CARTESIAN_POINT ( 'NONE',  ( 4.616787868375789472, -0.1008748965102136408, 2.088423895528898733 ) ) ;
#56610 = CARTESIAN_POINT ( 'NONE',  ( 5.912047867262844925, 1.302452500554865722, -1.440575834569270519 ) ) ;
#56611 = DIRECTION ( 'NONE',  ( -1.000000000000000000, -0.000000000000000000, -0.000000000000000000 ) ) ;
#56612 = SURFACE_SIDE_STYLE ('',( #121695 ) ) ;
#56613 = CARTESIAN_POINT ( 'NONE',  ( 0.4928148368598186946, -2.006445878461552645, 0.2004378712678403507 ) ) ;
#56614 = CARTESIAN_POINT ( 'NONE',  ( 0.3695850531008069706, -1.794773754367712693, -1.129184308951653781 ) ) ;
#56615 = PRESENTATION_STYLE_ASSIGNMENT (( #173596 ) ) ;
#56616 = CARTESIAN_POINT ( 'NONE',  ( -8.208571938070008400, 11.66408546346865016, -1.199719254218446718 ) ) ;
#56617 = CARTESIAN_POINT ( 'NONE',  ( 7.630541526392844887, 7.796719957080126662, 0.7998128361456341429 ) ) ;
#56618 = DIRECTION ( 'NONE',  ( -0.000000000000000000, 1.000000000000000000, -0.000000000000000000 ) ) ;
#56619 = CARTESIAN_POINT ( 'NONE',  ( 4.617693566336190436, -1.789886777702164089, 0.3589094947460610974 ) ) ;
#56620 = VERTEX_POINT ( 'NONE', #56683 ) ;
#56621 = CARTESIAN_POINT ( 'NONE',  ( -6.933015448541747006, 9.181880338089085214, 1.599625672291269396 ) ) ;
#56622 = CARTESIAN_POINT ( 'NONE',  ( -2.830620210203090181, 6.524417021870718258, 0.000000000000000000 ) ) ;
#56623 = CARTESIAN_POINT ( 'NONE',  ( -3.285556943749998737, -2.967708332855377051, 1.896917185911908499 ) ) ;
#56624 = CARTESIAN_POINT ( 'NONE',  ( -6.008234629150358330, 10.16135750065076060, 0.000000000000000000 ) ) ;
#56625 = CARTESIAN_POINT ( 'NONE',  ( 2.302995500392619022, -0.3493979467522835836, -1.989178256620740548 ) ) ;
#56626 = CARTESIAN_POINT ( 'NONE',  ( 5.508869005905306260, 1.674340917344345536, -1.437622030140395912 ) ) ;
#56627 = ADVANCED_FACE ( 'NONE', ( #23083 ), #155251, .T. ) ;
#56628 = CARTESIAN_POINT ( 'NONE',  ( -3.284818356260900796, 7.054314858938165678, 0.7998128361456352531 ) ) ;
#56629 = CARTESIAN_POINT ( 'NONE',  ( 2.940123752802700885, -0.9609217279343595930, 1.593531096896059873 ) ) ;
#56630 = CARTESIAN_POINT ( 'NONE',  ( 4.539282502477016479, 4.190251095844947926, 0.7998128361456341429 ) ) ;
#56631 = CYLINDRICAL_SURFACE ( 'NONE', #53897, 0.7499999999999997780 ) ;
#56632 = CARTESIAN_POINT ( 'NONE',  ( -5.416646063859567484, 6.278174148379618735, 1.199719254218450271 ) ) ;
#56633 = AXIS2_PLACEMENT_3D ( 'NONE', #68457, #35972, #165981 ) ;
#56634 = CARTESIAN_POINT ( 'NONE',  ( -8.941766003412679353, 10.39081407785832845, -1.199719254218446718 ) ) ;
#56635 = CARTESIAN_POINT ( 'NONE',  ( 4.688025921862073453, -0.8580590012943272171, 1.611482198803436905 ) ) ;
#56636 = CIRCLE ( 'NONE', #8227, 12.00000000000000178 ) ;
#56638 = CARTESIAN_POINT ( 'NONE',  ( -4.074744958279661766, 7.716589449174610316, -0.6783282581392232613 ) ) ;
#56637 = CARTESIAN_POINT ( 'NONE',  ( -5.004894982100124068, 5.868074229652107121, 1.199719254218452935 ) ) ;
#56639 = CARTESIAN_POINT ( 'NONE',  ( 6.170730229783032428, 7.061345527190763249, -1.063955632616358615 ) ) ;
#56640 = CARTESIAN_POINT ( 'NONE',  ( 0.2800716429562755683, -1.702078881456047688, 0.3292984779095942116 ) ) ;
#56641 = CARTESIAN_POINT ( 'NONE',  ( 0.4447213192238759771, 0.5506589691408066978, -1.650998906686143464 ) ) ;
#56642 = CARTESIAN_POINT ( 'NONE',  ( 5.619831112054756161, -2.252673335196005766, 0.5002786026085581650 ) ) ;
#56643 = CARTESIAN_POINT ( 'NONE',  ( 3.878514461961128479, 6.682628084666728085, -1.199719254218448494 ) ) ;
#56644 = CARTESIAN_POINT ( 'NONE',  ( 0.8431279278494309137, -1.768909939683245058, 1.056965710194081920 ) ) ;
#56645 = CARTESIAN_POINT ( 'NONE',  ( 4.496500501226593727, 8.397667684739696270, 0.7998128361456462443 ) ) ;
#56646 = EDGE_CURVE ( 'NONE', #109221, #197571, #113836, .T. ) ;
#56647 = EDGE_CURVE ( 'NONE', #172448, #169017, #31320, .T. ) ;
#56648 = CARTESIAN_POINT ( 'NONE',  ( 6.222043071159490957, -1.966323047081437014, -1.189884408624383383 ) ) ;
#56649 = CARTESIAN_POINT ( 'NONE',  ( 5.381422217466650615, 4.322449550048924394, 2.440471613107408011 ) ) ;
#56650 = CARTESIAN_POINT ( 'NONE',  ( -6.587282531393266360, 8.778525268082516320, 1.599625672291269396 ) ) ;
#56651 = VECTOR ( 'NONE', #35831, 1000.000000000000000 ) ;
#56652 = CARTESIAN_POINT ( 'NONE',  ( 6.086763352761943580, -0.2763008855245497331, -1.850001521387992565 ) ) ;
#56654 = CARTESIAN_POINT ( 'NONE',  ( -3.959863383643135393, 6.777535159962392086, 1.199719254218452935 ) ) ;
#56653 = CARTESIAN_POINT ( 'NONE',  ( 3.797043250571481732, -0.1924442655423033721, -1.902711443722324258 ) ) ;
#56655 = CARTESIAN_POINT ( 'NONE',  ( 5.549527019956425278, -1.737703232767298545, -1.360318885177333570 ) ) ;
#56656 = CARTESIAN_POINT ( 'NONE',  ( 4.452435347768154195, -1.380274204828018991, 1.605734313660161172 ) ) ;
#56657 = CARTESIAN_POINT ( 'NONE',  ( -1.225000000000030065, 0.3333333340161495628, 0.7072540797572656190 ) ) ;
#56658 = CARTESIAN_POINT ( 'NONE',  ( 6.883263157960335832, 6.035928496661214560, 2.641088654967935323 ) ) ;
#56659 = CARTESIAN_POINT ( 'NONE',  ( 5.573810548549551491, 6.635772073796838200, -1.082531754730548412 ) ) ;
#56660 = CARTESIAN_POINT ( 'NONE',  ( -4.299344108864949554, 8.030002203735486788, -0.7216878364870338292 ) ) ;
#56661 = CARTESIAN_POINT ( 'NONE',  ( 5.865915527372128402, 0.6157079936559420874, -2.029145397309819021 ) ) ;
#56662 = CARTESIAN_POINT ( 'NONE',  ( 2.099037836983450589, -0.6160640708386398989, -2.223778577795953115 ) ) ;
#56663 = CARTESIAN_POINT ( 'NONE',  ( 3.719154087244529894, -1.729071306366702698, -0.9269775827704658244 ) ) ;
#56664 = CARTESIAN_POINT ( 'NONE',  ( 6.937452841262716774, -7.242250812743806776, 6.937452841262695458 ) ) ;
#56665 = CARTESIAN_POINT ( 'NONE',  ( 6.578975509608026684, 1.922407110116808981, 0.7477742492353837145 ) ) ;
#56666 = CARTESIAN_POINT ( 'NONE',  ( 3.470524135418292300, 5.072030796119872953, -1.443375672974057666 ) ) ;
#56667 = CARTESIAN_POINT ( 'NONE',  ( 4.095444919779759552, 6.935713618788495793, 1.199719254218451159 ) ) ;
#56668 = VERTEX_POINT ( 'NONE', #184522 ) ;
#56669 = CARTESIAN_POINT ( 'NONE',  ( 5.401577436481666439, -1.966305606708594667, 0.4464985920552416720 ) ) ;
#56670 = CARTESIAN_POINT ( 'NONE',  ( -7.784352752540590004, 12.23349531127272094, 0.7998128361456481317 ) ) ;
#56671 =( NAMED_UNIT ( * ) SI_UNIT ( $, .STERADIAN. ) SOLID_ANGLE_UNIT ( ) );
#56672 = CARTESIAN_POINT ( 'NONE',  ( -10.99878419127389684, 6.872217442641685103, 3.961452310287494338 ) ) ;
#56673 = CARTESIAN_POINT ( 'NONE',  ( 2.887734989934476193, -2.027295339332426227, 0.7774125151447373039 ) ) ;
#56674 = CARTESIAN_POINT ( 'NONE',  ( 5.662465432362883355, 6.635239754958710989, 1.199719254218451159 ) ) ;
#56675 = CARTESIAN_POINT ( 'NONE',  ( 0.2289750728588327566, 1.457791096766167360, -1.540313549178488284 ) ) ;
#56676 = CARTESIAN_POINT ( 'NONE',  ( -0.7500000000000006661, 1.389583334016154748, -1.299038105676652011 ) ) ;
#56677 = CARTESIAN_POINT ( 'NONE',  ( -8.803107927929307408, 14.53091780748839490, -8.204921721742058693 ) ) ;
#56678 = CARTESIAN_POINT ( 'NONE',  ( 4.797842130449009090, 8.250315290282747682, 0.8618622828703215166 ) ) ;
#56679 = CARTESIAN_POINT ( 'NONE',  ( 1.194684731684968693, -0.4980721920408748282, -1.999570191575838818 ) ) ;
#56681 = CARTESIAN_POINT ( 'NONE',  ( 0.7500000000000006661, 8.364583334016128191, 1.299038105676657340 ) ) ;
#56680 = DIRECTION ( 'NONE',  ( 0.000000000000000000, 1.000000000000000000, 0.000000000000000000 ) ) ;
#56682 = CARTESIAN_POINT ( 'NONE',  ( 1.364683531249986537, 0.8635416670080893198, 0.7879004041258500513 ) ) ;
#56683 = CARTESIAN_POINT ( 'NONE',  ( 11.84668730067608600, 12.69999999999998153, 1.399999999999998579 ) ) ;
#56684 = EDGE_LOOP ( 'NONE', ( #61919, #40395, #81230, #38076 ) ) ;
#56685 = CARTESIAN_POINT ( 'NONE',  ( 3.598220562318912741, -0.9401235635465958751, 1.665135908046413871 ) ) ;
#56686 = CARTESIAN_POINT ( 'NONE',  ( 5.365971031753679732, 0.8746336007162245352, 1.538519630229380875 ) ) ;
#56687 = CARTESIAN_POINT ( 'NONE',  ( 6.723917837734620484, 6.809268663637336516, 0.000000000000000000 ) ) ;
#56688 = CARTESIAN_POINT ( 'NONE',  ( -3.307299406729781399, 5.945934176904983381, -1.199719254218452935 ) ) ;
#56689 = CARTESIAN_POINT ( 'NONE',  ( 0.1053163366912619470, 1.342294115999270510, 1.216805694454982767 ) ) ;
#56691 = CARTESIAN_POINT ( 'NONE',  ( 6.187116780671887639, 1.595606285689795678, 1.059669358585461962 ) ) ;
#56690 = CARTESIAN_POINT ( 'NONE',  ( 0.000000000000000000, 6.487495393664096888, -3.100011470320000573 ) ) ;
#56692 = CARTESIAN_POINT ( 'NONE',  ( 0.5903903138861701372, 1.065687334306382184, -1.774900233272216798 ) ) ;
#56693 = CARTESIAN_POINT ( 'NONE',  ( -1.364683531250000748, 0.5718750003414208027, 0.000000000000000000 ) ) ;
#56694 = CARTESIAN_POINT ( 'NONE',  ( 5.893391625361731556, 1.417579469995243091, 1.220656814419220249 ) ) ;
#56695 = CARTESIAN_POINT ( 'NONE',  ( 2.842213963582499670, 1.811911227886909614, 0.2232855069103783507 ) ) ;
#56697 = CARTESIAN_POINT ( 'NONE',  ( 6.266472554743693912, 6.895788939045927712, 0.7740814723603481884 ) ) ;
#56696 = CARTESIAN_POINT ( 'NONE',  ( 5.777994779145079640, 1.311685685134782231, 1.774619457157788904 ) ) ;
#56698 = CARTESIAN_POINT ( 'NONE',  ( 1.364683531249986537, 0.8635416670080893198, 0.7879004041258500513 ) ) ;
#56699 = CARTESIAN_POINT ( 'NONE',  ( 3.596185909054748553, 0.9300860933913506212, -1.841171126807969349 ) ) ;
#56700 = CARTESIAN_POINT ( 'NONE',  ( -8.064402442030170093, 8.302891025323665630, 0.7998128361456602331 ) ) ;
#56701 = CARTESIAN_POINT ( 'NONE',  ( 9.185812768458653466, 10.67553530374532045, 1.199719254218453823 ) ) ;
#56702 = CARTESIAN_POINT ( 'NONE',  ( 1.430889623655247744, 4.024647178788855584, -0.4691377289697504227 ) ) ;
#56703 = CARTESIAN_POINT ( 'NONE',  ( 0.8257154465432202661, -2.052837714267462754, 0.6772920067378007669 ) ) ;
#56704 = CARTESIAN_POINT ( 'NONE',  ( 0.2566020104313873618, -2.170709068928804886, -0.05254486697847670501 ) ) ;
#56705 = CARTESIAN_POINT ( 'NONE',  ( -1.402160292154681736E-14, 1.259375000341419248, -1.575800808251659024 ) ) ;
#56706 = CARTESIAN_POINT ( 'NONE',  ( 3.690839692606663558, -0.4176960054509891163, -2.120685484085436112 ) ) ;
#56708 = CARTESIAN_POINT ( 'NONE',  ( 2.646866301197240645, -0.3325320220872363675, -1.933311746529025266 ) ) ;
#56707 = CARTESIAN_POINT ( 'NONE',  ( 4.477216424163804831, -1.805109318760585779, -0.9060198856494814379 ) ) ;
#56709 = CARTESIAN_POINT ( 'NONE',  ( 6.620655732516651071, 2.021119449029490589, 2.477762541108457839 ) ) ;
#56710 = EDGE_CURVE ( 'NONE', #96482, #65271, #105044, .T. ) ;
#56713 = CARTESIAN_POINT ( 'NONE',  ( 6.317736394288135493, 8.393778431468064127, 1.443375672974076540 ) ) ;
#56712 = CARTESIAN_POINT ( 'NONE',  ( -3.285556943750000514, -3.288541666188709023, -1.896917185911906500 ) ) ;
#56711 = DIRECTION ( 'NONE',  ( 0.000000000000000000, 0.000000000000000000, -1.000000000000000000 ) ) ;
#56714 = CARTESIAN_POINT ( 'NONE',  ( -6.363572996767778100, 8.517530811019446091, -1.599625672291271394 ) ) ;
#56715 = CARTESIAN_POINT ( 'NONE',  ( 2.501185699981960830, -0.1928336239410358699, 2.007256303757164240 ) ) ;
#56717 =( LENGTH_UNIT ( ) NAMED_UNIT ( * ) SI_UNIT ( .MILLI., .METRE. ) );
#56716 = CARTESIAN_POINT ( 'NONE',  ( -4.172158584703340445, 5.890604320285754980, -1.599625672291256295 ) ) ;
#56718 = DIRECTION ( 'NONE',  ( -0.000000000000000000, -1.000000000000000000, -0.000000000000000000 ) ) ;
#56719 = CARTESIAN_POINT ( 'NONE',  ( 6.258066496116281741, 0.7254575739856858885, -1.769658340881982816 ) ) ;
#56720 = CARTESIAN_POINT ( 'NONE',  ( -4.370663978927101567, 5.060324124126029943, -1.009771797811724214 ) ) ;
#56721 = CARTESIAN_POINT ( 'NONE',  ( 4.487385655998873624, 7.218738451098584363, 1.082531754730558626 ) ) ;
#56723 = CARTESIAN_POINT ( 'NONE',  ( 4.710564641745673242, 1.930423983604495630, 0.5826390268678026674 ) ) ;
#56722 = CARTESIAN_POINT ( 'NONE',  ( -8.148087131688692253, 9.568818410800712826, -1.082531754730543083 ) ) ;
#56724 = CARTESIAN_POINT ( 'NONE',  ( 1.499999999999990896, 4.025000000000021672, 1.214306433183764966E-14 ) ) ;
#56725 = CARTESIAN_POINT ( 'NONE',  ( -0.6823417656250003738, 14.71354166700806410, 1.181850606188754593 ) ) ;
#56726 = CARTESIAN_POINT ( 'NONE',  ( 6.668995740727024391, -1.579612310505887685, -0.6930582901118372829 ) ) ;
#56727 = CARTESIAN_POINT ( 'NONE',  ( 6.068156270568149324, 9.237210194708310951, 1.199719254218452047 ) ) ;
#56728 = CARTESIAN_POINT ( 'NONE',  ( 8.107412671292022921, 12.40247251657532956, 0.7216878364870438212 ) ) ;
#56729 = CARTESIAN_POINT ( 'NONE',  ( -11.55950211276791251, 11.37999999999999901, -3.221476510067115662 ) ) ;
#56730 = CARTESIAN_POINT ( 'NONE',  ( 4.921099816907485547, -0.09337705715995943401, 1.868355541605345671 ) ) ;
#56731 = PLANE ( 'NONE',  #109450 ) ;
#56732 = CARTESIAN_POINT ( 'NONE',  ( 1.780221101387355009, -1.146701191353172611, -1.723467693327894068 ) ) ;
#56733 = CARTESIAN_POINT ( 'NONE',  ( -2.253107639696438902E-15, -7.721243112841103873, -10.98746396341378251 ) ) ;
#56734 = ORIENTED_EDGE ( 'NONE', *, *, #27310, .T. ) ;
#56735 = CARTESIAN_POINT ( 'NONE',  ( 5.239300017038202917, 5.077214539491492928, 0.000000000000000000 ) ) ;
#56736 = CARTESIAN_POINT ( 'NONE',  ( 0.2984541275833849094, 1.388471424577278235, -1.462460896543740674 ) ) ;
#56737 = CARTESIAN_POINT ( 'NONE',  ( 0.7381712907078247232, 1.078401568856072412, -1.455492281976622504 ) ) ;
#56738 = CARTESIAN_POINT ( 'NONE',  ( 4.787437638956922648, 6.678706226906775179, -1.443375672974068769 ) ) ;
#56739 = CARTESIAN_POINT ( 'NONE',  ( -2.476786429007699297, 5.182949722010740778, -0.9424847539492169357 ) ) ;
#56740 = CARTESIAN_POINT ( 'NONE',  ( 7.741342523278698096, 10.05465224862374285, 1.443375672974076540 ) ) ;
#56741 = CARTESIAN_POINT ( 'NONE',  ( 6.740374924288304648, 11.01552117831172062, 1.040834085586084257E-14 ) ) ;
#56743 = CARTESIAN_POINT ( 'NONE',  ( 6.187116780671887639, 1.595606285689795678, 1.059669358585461962 ) ) ;
#56742 = CARTESIAN_POINT ( 'NONE',  ( -4.693093728624763372, 8.627026450037540428, 0.7998128361456481317 ) ) ;
#56744 = DIRECTION ( 'NONE',  ( -0.000000000000000000, -0.000000000000000000, 1.000000000000000000 ) ) ;
#56745 = CARTESIAN_POINT ( 'NONE',  ( 11.84668730067608600, 10.19999999999999929, -1.400000000000001910 ) ) ;
#56746 =( BOUNDED_CURVE ( )  B_SPLINE_CURVE ( 2, ( #205179, #124048, #126173, #11260, #25380, #155387, #142379, #10196, #190014 ),
 .UNSPECIFIED., .F., .T. ) 
 B_SPLINE_CURVE_WITH_KNOTS ( ( 3, 2, 2, 2, 3 ),
 ( 0.5982142857142856984, 0.6011904761904761640, 0.6071428571428570953, 0.6130952380952381375, 0.6160714285714286031 ),
 .UNSPECIFIED. ) 
 CURVE ( )  GEOMETRIC_REPRESENTATION_ITEM ( )  RATIONAL_B_SPLINE_CURVE ( ( 0.9330127018922194093, 0.9330127018922194093, 1.000000000000000000, 0.8660254037844387076, 1.000000000000000000, 0.8660254037844387076, 1.000000000000000000, 0.9330127018922194093, 0.9330127018922194093 ) ) 
 REPRESENTATION_ITEM ( '' )  );
#56747 = AXIS2_PLACEMENT_3D ( 'NONE', #112620, #11834, #95262 ) ;
#56748 = CARTESIAN_POINT ( 'NONE',  ( 1.225000000000000977, 0.6458333333333310389, -0.7072540797572937077 ) ) ;
#56750 = ORIENTED_EDGE ( 'NONE', *, *, #183643, .F. ) ;
#56749 = CARTESIAN_POINT ( 'NONE',  ( 4.039966587192257208, 6.696749537490852333, 1.082531754730558626 ) ) ;
#56751 = ADVANCED_FACE ( 'NONE', ( #205038 ), #37223, .T. ) ;
#56752 = CARTESIAN_POINT ( 'NONE',  ( -8.866669273657352690, 9.446795028796142191, 0.7216878364870438212 ) ) ;
#56753 = CARTESIAN_POINT ( 'NONE',  ( 2.887745953747706373, 1.527789104365802286, 1.529575784674996886 ) ) ;
#56754 = CARTESIAN_POINT ( 'NONE',  ( -5.777182853198894463, 9.754147405458438058, 0.7216878364870267237 ) ) ;
#56755 = CARTESIAN_POINT ( 'NONE',  ( 7.024532985656128936, 9.288650798055913427, 1.443375672974065660 ) ) ;
#56756 = CARTESIAN_POINT ( 'NONE',  ( 1.283610819548046011, 0.1505422781087061845, -2.115291873224629082 ) ) ;
#56757 = EDGE_CURVE ( 'NONE', #198330, #151228, #56636, .T. ) ;
#56758 = CARTESIAN_POINT ( 'NONE',  ( 6.141596500199405284, -1.324292569296809052, -1.256812384211228428 ) ) ;
#56759 = CARTESIAN_POINT ( 'NONE',  ( 1.018749824907847934, 1.819822117139553885, 0.7584178161138422913 ) ) ;
#56760 = CARTESIAN_POINT ( 'NONE',  ( 3.322422747544371280, -0.7792853099402965444, -1.746611395919236642 ) ) ;
#56761 = CARTESIAN_POINT ( 'NONE',  ( 0.3817069231124412543, 4.000000000000008882, 1.007084182327167454 ) ) ;
#56762 = CARTESIAN_POINT ( 'NONE',  ( 5.019951571474082996, 1.948400538373602497, -0.2868881896359152806 ) ) ;
#56763 = CARTESIAN_POINT ( 'NONE',  ( 0.2341854262303414147, 0.3310631332954366290, 1.913375037591731775 ) ) ;
#56764 = ORIENTED_EDGE ( 'NONE', *, *, #209073, .F. ) ;
#56765 = CARTESIAN_POINT ( 'NONE',  ( -4.098307573080856692, 8.003385611894792362, 0.7998128361456352531 ) ) ;
#56767 = CARTESIAN_POINT ( 'NONE',  ( 4.067155351693835485E-15, 1.250000000682825130, -1.225000000000013411 ) ) ;
#56766 = CARTESIAN_POINT ( 'NONE',  ( -4.502189528189771472, 7.410248995266807803, -1.199719254218453823 ) ) ;
#56768 = CARTESIAN_POINT ( 'NONE',  ( 5.600926855776875435, 7.627776979863398310, -1.443375672974078761 ) ) ;
#56770 = ORIENTED_EDGE ( 'NONE', *, *, #182687, .F. ) ;
#56769 = CARTESIAN_POINT ( 'NONE',  ( 5.250612361737760025, 1.884661702551674534, 0.3228764834103393100 ) ) ;
#56771 = CARTESIAN_POINT ( 'NONE',  ( 0.7278961316968115547, -2.094849050945537972, 0.6941159686642894844 ) ) ;
#56772 = EDGE_CURVE ( 'NONE', #85578, #59844, #177711, .T. ) ;
#56773 = CARTESIAN_POINT ( 'NONE',  ( -3.432849766368863964, -0.02876672507445138249, 0.000000000000000000 ) ) ;
#56774 = CARTESIAN_POINT ( 'NONE',  ( 0.01216826571975513152, -1.911853497171299265, -0.04704278909201110859 ) ) ;
#56775 = CARTESIAN_POINT ( 'NONE',  ( 3.929058411375439874, 4.999999999999997335, -0.7500000000000006661 ) ) ;
#56776 = CARTESIAN_POINT ( 'NONE',  ( 6.727182134110220701, 0.005875948494733078051, 1.810970247402940103 ) ) ;
#56777 = CARTESIAN_POINT ( 'NONE',  ( 2.436061438456170958, 1.271862942251865691, 1.633573898902056731 ) ) ;
#56778 = CARTESIAN_POINT ( 'NONE',  ( -5.551173829791513192, 8.563787670477010394, 1.199719254218452047 ) ) ;
#56779 = CARTESIAN_POINT ( 'NONE',  ( -4.611386515133914621, 8.374621496872018511, -0.1785149356163841239 ) ) ;
#56780 = CARTESIAN_POINT ( 'NONE',  ( 0.2511322555047851290, -1.735185354305257110, 1.289038484408123963 ) ) ;
#56781 = CARTESIAN_POINT ( 'NONE',  ( -11.07041934583884313, 7.106884258450539171, -4.635831715794138219 ) ) ;
#56782 = CARTESIAN_POINT ( 'NONE',  ( 5.899206235721897507, 6.055031161196562373, 0.000000000000000000 ) ) ;
#56783 = CARTESIAN_POINT ( 'NONE',  ( -6.999862025036992286, -6.532648833121171172, 6.392587740394332307 ) ) ;
#56784 = CARTESIAN_POINT ( 'NONE',  ( -1.364683531250014514, 12.40104166700806054, -0.7879004041258335089 ) ) ;
#56786 = CARTESIAN_POINT ( 'NONE',  ( -5.932574734431526942, 9.079031735882207244, 1.199719254218454489 ) ) ;
#56785 = CARTESIAN_POINT ( 'NONE',  ( 6.925078400183593885, 7.629137130509070275, 2.455651831298297338 ) ) ;
#56787 = CARTESIAN_POINT ( 'NONE',  ( 4.465268017702548775, -1.683484418668965921, -0.4155383358091616075 ) ) ;
#56788 = EDGE_CURVE ( 'NONE', #179865, #15325, #195015, .T. ) ;
#56789 = CARTESIAN_POINT ( 'NONE',  ( -2.927671105547157371, 5.503034492191895666, 1.199719254218462483 ) ) ;
#56790 = CARTESIAN_POINT ( 'NONE',  ( 2.114207291064807759, 2.064986537539798661, -0.1480984254652456533 ) ) ;
#56791 = CARTESIAN_POINT ( 'NONE',  ( 3.269268187362909028, 1.912946029434154038, -0.9076713616091285353 ) ) ;
#56792 = CARTESIAN_POINT ( 'NONE',  ( 7.287671262545424966, 8.461036880179857889, -1.199719254218451159 ) ) ;
#56793 = CARTESIAN_POINT ( 'NONE',  ( -1.201851678989727383E-14, 3.696875000341422801, -1.575800808251660134 ) ) ;
#56794 = CARTESIAN_POINT ( 'NONE',  ( 2.272252165359678333, -0.9238012212633615050, -1.739302338446031548 ) ) ;
#56795 = CARTESIAN_POINT ( 'NONE',  ( 6.082781304119575516, 6.035783188292461077, -0.3281998023207943760 ) ) ;
#56796 = CARTESIAN_POINT ( 'NONE',  ( -0.2108831679770960255, -0.001785917861228669690, -1.896958272444612792 ) ) ;
#56797 = CARTESIAN_POINT ( 'NONE',  ( 4.242302733825270344, 0.6093012942862492398, 2.209731468575569124 ) ) ;
#56798 = CARTESIAN_POINT ( 'NONE',  ( 2.367563199519676420, 1.790531440309536926, -0.3556685536310541518 ) ) ;
#56799 = CARTESIAN_POINT ( 'NONE',  ( 4.342354338126830804, 8.288106837781779035, -0.7998128361456381397 ) ) ;
#56800 = CARTESIAN_POINT ( 'NONE',  ( 5.788968402910802169, 8.737251655829183505, 1.082531754730558626 ) ) ;
#56801 = CARTESIAN_POINT ( 'NONE',  ( -8.857554428429624593, 9.228235009456373206, 0.7998128361456462443 ) ) ;
#56802 = CARTESIAN_POINT ( 'NONE',  ( 2.900642264033539863, -1.984120583840060625, -0.3400495124021261084 ) ) ;
#56803 = CARTESIAN_POINT ( 'NONE',  ( 3.291801117278610800, -1.314073873198824627, -1.456807609480186061 ) ) ;
#56804 = CARTESIAN_POINT ( 'NONE',  ( -9.155833807930273238, 9.576227618873799585, -0.7998128361456291469 ) ) ;
#56805 = CARTESIAN_POINT ( 'NONE',  ( -5.605406444246153974, 8.627059054007450101, -1.199719254218440723 ) ) ;
#56806 = DIRECTION ( 'NONE',  ( -0.000000000000000000, -1.000000000000000000, 0.000000000000000000 ) ) ;
#56808 = CARTESIAN_POINT ( 'NONE',  ( 4.610057705051894494, -0.7578761767026606089, -1.599493228202266470 ) ) ;
#56807 = CARTESIAN_POINT ( 'NONE',  ( 6.140588758375521650, -1.766823853066697536, 1.117321708369632516 ) ) ;
#56809 = CARTESIAN_POINT ( 'NONE',  ( 0.7499999999999885647, 3.347916667349487341, -1.299038105676658228 ) ) ;
#56810 = CARTESIAN_POINT ( 'NONE',  ( 0.9377431681640016059, 0.8850447378907433382, -2.004962588275795543 ) ) ;
#56811 = EDGE_CURVE ( 'NONE', #204988, #195372, #108696, .T. ) ;
#56812 = CARTESIAN_POINT ( 'NONE',  ( 5.156098626313831090, -1.256936769724174674, 1.203943403725541206 ) ) ;
#56813 = CARTESIAN_POINT ( 'NONE',  ( 7.564559641420864899, 10.91273778404466199, -1.199719254218446718 ) ) ;
#56814 = CARTESIAN_POINT ( 'NONE',  ( 0.000000000000000000, 5.499999999999998224, 0.000000000000000000 ) ) ;
#56815 = CARTESIAN_POINT ( 'NONE',  ( 0.1932713599902321500, -1.417659354009516148, -1.810318517150938389 ) ) ;
#56816 = CARTESIAN_POINT ( 'NONE',  ( -1.737500000000000266, -1.414583332377417735, -3.009438278150923907 ) ) ;
#56817 = CARTESIAN_POINT ( 'NONE',  ( 5.923113090906284128, 0.7054357044574584013, 1.584025686543149680 ) ) ;
#56818 = CARTESIAN_POINT ( 'NONE',  ( 1.541937560865791479, -1.600244427420342896, -1.519961040588948986 ) ) ;
#56819 =( BOUNDED_SURFACE ( )  B_SPLINE_SURFACE ( 3, 2, ( 
 ( #180561, #98259, #65710 ),
 ( #52691, #84125, #150211 ),
 ( #164316, #1783, #67840 ),
 ( #133986, #81989, #148077 ),
 ( #199993, #51642, #117766 ),
 ( #118820, #131858, #197865 ) ),
 .UNSPECIFIED., .F., .F., .T. ) 
 B_SPLINE_SURFACE_WITH_KNOTS ( ( 4, 2, 4 ),
 ( 3, 3 ),
 ( 0.000000000000000000, 0.0003754691837024766985, 0.0007509383674049533971 ),
 ( 0.000000000000000000, 1.000000000000000000 ),
 .UNSPECIFIED. ) 
 GEOMETRIC_REPRESENTATION_ITEM ( )  RATIONAL_B_SPLINE_SURFACE ( (
 ( 1.000000000000000000, 0.6711954675835395401, 1.000000000000000000),
 ( 1.000000000000000000, 0.6709646295267174265, 1.000000000000000000),
 ( 1.000000000000000000, 0.6771840716659688342, 1.000000000000000000),
 ( 1.000000000000000000, 0.6927481755866825575, 1.000000000000000000),
 ( 1.000000000000000000, 0.7017972101310361310, 1.000000000000000000),
 ( 1.000000000000000000, 0.7071067811865475727, 1.000000000000000000) ) ) 
 REPRESENTATION_ITEM ( '' )  SURFACE ( )  );
#56820 = CARTESIAN_POINT ( 'NONE',  ( 5.775877569751362017, -2.119564319632438743, 0.4699819441058172842 ) ) ;
#56821 = CARTESIAN_POINT ( 'NONE',  ( -1.224999999999995204, 3.000000000000002665, -1.387778780781445676E-14 ) ) ;
#56822 = CARTESIAN_POINT ( 'NONE',  ( 0.7435476276109568294, 0.4067398897551637305, -2.077755800567067546 ) ) ;
#56823 = CARTESIAN_POINT ( 'NONE',  ( 2.656250000000001332, -1.895863743164027504, 0.7852924748301256530 ) ) ;
#56824 = CARTESIAN_POINT ( 'NONE',  ( 6.727182134110196721, 7.629137130509074716, 2.689055895399253160 ) ) ;
#56825 = CARTESIAN_POINT ( 'NONE',  ( 4.295867091898570855, -0.7379356464434319030, 1.779637345161827922 ) ) ;
#56826 = CARTESIAN_POINT ( 'NONE',  ( 1.348599501924132804, 1.090831829848055046, -1.934932191954039427 ) ) ;
#56827 = ORIENTED_EDGE ( 'NONE', *, *, #48815, .T. ) ;
#56828 = CARTESIAN_POINT ( 'NONE',  ( 0.7499999999999902300, 4.566666666666691299, -1.299038105676658228 ) ) ;
#56829 = CARTESIAN_POINT ( 'NONE',  ( 4.416205349749311004, 6.175325546172740765, 1.599625672291267398 ) ) ;
#56830 = CARTESIAN_POINT ( 'NONE',  ( 5.309989718046547402, 9.346738437696316737, 0.7998128361456462443 ) ) ;
#56831 = CARTESIAN_POINT ( 'NONE',  ( 3.422728177422405871, -0.9015832817733639981, -2.030284994954335787 ) ) ;
#56832 = CARTESIAN_POINT ( 'NONE',  ( -8.351459436338037889, 10.76645531385962862, -1.443375672974059665 ) ) ;
#56833 = CARTESIAN_POINT ( 'NONE',  ( -0.5773502691960585853, -4.295408888567775918, 1.000000000000000888 ) ) ;
#56834 = CARTESIAN_POINT ( 'NONE',  ( 5.666945020832167224, 8.594891043404107478, 1.082531754730558626 ) ) ;
#56835 = CARTESIAN_POINT ( 'NONE',  ( -9.449669878600623463, 11.08733161553131197, -1.082531754730537976 ) ) ;
#56836 = AXIS2_PLACEMENT_3D ( 'NONE', #189972, #12280, #42695 ) ;
#56837 = CARTESIAN_POINT ( 'NONE',  ( 5.045042558060919724, 8.899983727797476263, -0.7216878364870458196 ) ) ;
#56838 = CARTESIAN_POINT ( 'NONE',  ( 1.863907939170056149, -0.1017519224979606118, -2.013985838549677609 ) ) ;
#56840 = CARTESIAN_POINT ( 'NONE',  ( 6.092244811693771744, 1.020019244021443727, -1.792768071708307431 ) ) ;
#56839 = CARTESIAN_POINT ( 'NONE',  ( 7.401861798056875053, 10.72292363345333399, -1.199719254218441611 ) ) ;
#56841 = DIRECTION ( 'NONE',  ( 0.000000000000000000, 1.000000000000000000, 0.000000000000000000 ) ) ;
#56842 = CARTESIAN_POINT ( 'NONE',  ( 6.875393295461478260, 8.154285278527437342, -1.082531754730548412 ) ) ;
#56843 = CIRCLE ( 'NONE', #177933, 0.09999999999999982514 ) ;
#56844 = CARTESIAN_POINT ( 'NONE',  ( 6.286628787680052177, 1.509496725765889114, -0.8662470760552234417 ) ) ;
#56845 = SURFACE_STYLE_USAGE ( .BOTH. , #172742 ) ;
#56846 = CARTESIAN_POINT ( 'NONE',  ( 1.364683531249990311, 2.884375000341422801, 1.214306433183764966E-14 ) ) ;
#56847 = CARTESIAN_POINT ( 'NONE',  ( 1.756752346989236768, -1.514669478205426190, -0.9150583790542564655 ) ) ;
#56848 = CARTESIAN_POINT ( 'NONE',  ( 0.1764080092822375156, 1.496053712750060383, 1.352152247781977179 ) ) ;
#56849 = CARTESIAN_POINT ( 'NONE',  ( 0.2922019606856861018, 1.531309713818730822, -1.022077305420886040 ) ) ;
#56850 = CARTESIAN_POINT ( 'NONE',  ( 4.388395349243869425, -0.5016406811718626679, -2.236657869423730460 ) ) ;
#56851 = CARTESIAN_POINT ( 'NONE',  ( 2.097363409947244683, -1.840767647902554982, 0.04455809990146220728 ) ) ;
#56852 = CARTESIAN_POINT ( 'NONE',  ( 7.899597058256738968, 12.36794700127490820, 1.040834085586084257E-14 ) ) ;
#56853 = CARTESIAN_POINT ( 'NONE',  ( 3.416849837094409370, 1.649954109374281996, 0.7815844185870900462 ) ) ;
#56854 = CARTESIAN_POINT ( 'NONE',  ( 3.744767666119628746, 2.000857235306313875, -0.2496062519145719194 ) ) ;
#56855 = CARTESIAN_POINT ( 'NONE',  ( -9.073431116043565225, 11.60875560684942265, -1.599625672291263179 ) ) ;
#56857 = FACE_OUTER_BOUND ( 'NONE', #15459, .T. ) ;
#56856 = CARTESIAN_POINT ( 'NONE',  ( 3.731548843211284439, -2.091483890824384684, 0.8634027215336376182 ) ) ;
#56858 = CARTESIAN_POINT ( 'NONE',  ( 5.051841681570322429, 0.6635009534815727861, -1.998768678292896839 ) ) ;
#56859 = CARTESIAN_POINT ( 'NONE',  ( 7.292702578216013976, 15.96614424547465205, 9.125377228003427987 ) ) ;
#56860 = CARTESIAN_POINT ( 'NONE',  ( 2.963400493335893948, 1.747644659881589568, 1.109742091278065113 ) ) ;
#56861 = CARTESIAN_POINT ( 'NONE',  ( 2.693266070609028784, 6.293894182352508970, 0.000000000000000000 ) ) ;
#56862 = CARTESIAN_POINT ( 'NONE',  ( 1.360316468749955598, 0.5260416670081085044, 0.7853790794158820310 ) ) ;
#56863 = CARTESIAN_POINT ( 'NONE',  ( 6.305353446217972113, 1.845220813986702124, -1.044706065825385943 ) ) ;
#56865 = CARTESIAN_POINT ( 'NONE',  ( 0.8735101492000696410, 1.856966920605634508, -0.5126664406217595893 ) ) ;
#56864 = CARTESIAN_POINT ( 'NONE',  ( -8.045874094706015001, 11.47427131287732927, -1.199719254218446718 ) ) ;
#56866 = CARTESIAN_POINT ( 'NONE',  ( -5.666381855868691808, 5.575476684793721383, 0.000000000000000000 ) ) ;
#56867 = CARTESIAN_POINT ( 'NONE',  ( 7.099665995050449041, 11.43469409420089455, 0.7998128361456462443 ) ) ;
#56868 = CARTESIAN_POINT ( 'NONE',  ( 5.763624699140868834, 7.817591130454727200, -1.443375672974078761 ) ) ;
#56869 = CARTESIAN_POINT ( 'NONE',  ( 4.215071147998584955, 7.318223152490296535, 0.8720340548805920466 ) ) ;
#56870 = CARTESIAN_POINT ( 'NONE',  ( -0.4019237886467001974, 9.582585450998170273, 1.500000000000001998 ) ) ;
#56871 = CARTESIAN_POINT ( 'NONE',  ( -3.632695093457760649, 6.325562478087638496, -1.199719254218452047 ) ) ;
#56872 = CARTESIAN_POINT ( 'NONE',  ( 1.055278351191447639, 0.4402236684300055991, 2.177206957374391738 ) ) ;
#56873 = CARTESIAN_POINT ( 'NONE',  ( 1.905437291041052195, 1.750494195096408800, 1.170504954829422850 ) ) ;
#56874 = CARTESIAN_POINT ( 'NONE',  ( -4.950662367645459305, 5.804802846121667415, -1.199719254218453823 ) ) ;
#56875 = CARTESIAN_POINT ( 'NONE',  ( 8.046927864910717432, 9.346836249606042202, 1.199719254218462483 ) ) ;
#56876 = CARTESIAN_POINT ( 'NONE',  ( 6.139480533765972581, 1.719935631569947221, -0.7110793932548589158 ) ) ;
#56877 = CARTESIAN_POINT ( 'NONE',  ( 5.777746017718023097, 9.892454120646377191, 0.7998128361456462443 ) ) ;
#56878 = CARTESIAN_POINT ( 'NONE',  ( 11.88237264505823987, 9.843229615316822390, 0.9087825512662162097 ) ) ;
#56879 = CARTESIAN_POINT ( 'NONE',  ( -5.153507786970262572, 9.026526494858359229, -0.7216878364870338292 ) ) ;
#56880 = CARTESIAN_POINT ( 'NONE',  ( -7.687109909268394325, 11.91211929421440097, 0.000000000000000000 ) ) ;
#56881 = CARTESIAN_POINT ( 'NONE',  ( 0.4398875993102538962, -2.011672884243600024, 0.6710486789910232730 ) ) ;
#56882 = CARTESIAN_POINT ( 'NONE',  ( -7.747558435566414659, 8.003516027774422170, -0.7998128361456362523 ) ) ;
#56884 = CARTESIAN_POINT ( 'NONE',  ( 2.963279974173158138, 1.655882904019840840, 1.051842618152734499 ) ) ;
#56883 = CARTESIAN_POINT ( 'NONE',  ( -1.225000000000036060, 0.02083333333335212617, 0.7072540797572677285 ) ) ;
#56885 = CARTESIAN_POINT ( 'NONE',  ( 1.991316529349271836, 1.880942973025516940, -1.065213018539921563 ) ) ;
#56886 = CARTESIAN_POINT ( 'NONE',  ( 1.065666191918061445, -1.167978014494171823, 1.423405568861765946 ) ) ;
#56888 = CARTESIAN_POINT ( 'NONE',  ( -4.512490679940424521, 7.037946173918820492, -1.151410311177623935 ) ) ;
#56887 = CARTESIAN_POINT ( 'NONE',  ( -4.472210567661380587, 6.310941310395290493, 1.599625672291270506 ) ) ;
#56889 = CARTESIAN_POINT ( 'NONE',  ( 1.364683531249986537, 1.655208333674748955, -0.7879004041258239610 ) ) ;
#56890 = CARTESIAN_POINT ( 'NONE',  ( 3.398151218454207090, 1.370964323331394397, -1.071876607410700677 ) ) ;
#56891 = CARTESIAN_POINT ( 'NONE',  ( 6.697364695470787943, 7.876308901879812474, -1.082531754730543083 ) ) ;
#56892 = CARTESIAN_POINT ( 'NONE',  ( -12.46228870304231329, 8.331136472732479703, -2.451782011337487965 ) ) ;
#56893 = ADVANCED_FACE ( 'NONE', ( #57747 ), #162880, .T. ) ;
#56894 = CARTESIAN_POINT ( 'NONE',  ( 0.7257156204387126275, -2.052300050329861847, 0.6792298617422781737 ) ) ;
#56895 = CARTESIAN_POINT ( 'NONE',  ( 2.477888549845189470, 1.799646572043178683, 0.9090068759892779848 ) ) ;
#56896 = CARTESIAN_POINT ( 'NONE',  ( -0.08641082498352903318, -9.914243671626374876, -10.99966068378000728 ) ) ;
#56897 = CARTESIAN_POINT ( 'NONE',  ( 0.5675189469334164238, 0.2105291993744831114, -2.151437729447757796 ) ) ;
#56898 = CARTESIAN_POINT ( 'NONE',  ( 2.254701366666445939, -1.525215070022269082, 1.249173565255176976 ) ) ;
#56899 = CARTESIAN_POINT ( 'NONE',  ( -11.00023875073173762, -5.574346042903139953, -0.04317804960739271558 ) ) ;
#56902 = ORIENTED_EDGE ( 'NONE', *, *, #120283, .F. ) ;
#56901 = CARTESIAN_POINT ( 'NONE',  ( -4.665414256878293031, 7.496714828783040296, -1.082531754730549967 ) ) ;
#56900 = CARTESIAN_POINT ( 'NONE',  ( -2.788906526875773208E-15, 10.71875000068279604, -1.499999999999998446 ) ) ;
#56903 = CARTESIAN_POINT ( 'NONE',  ( -5.519577934094894722, 7.532869904567736974, 1.443375672974058777 ) ) ;
#56904 = CARTESIAN_POINT ( 'NONE',  ( -0.2108831679771168421, 6.948330828014878335, -2.492181822431015270 ) ) ;
#56905 = CARTESIAN_POINT ( 'NONE',  ( 6.008198349511364000, 7.038594824965278995, 1.199719254218453823 ) ) ;
#56906 = CARTESIAN_POINT ( 'NONE',  ( -6.252245114557387851, 7.323316050852266557, -1.199719254218453823 ) ) ;
#56907 = CARTESIAN_POINT ( 'NONE',  ( 2.192062543670767027, 1.244387780127395482, 1.590672870423719187 ) ) ;
#56908 = DIRECTION ( 'NONE',  ( -1.000000000000000000, -0.000000000000000000, -0.000000000000000000 ) ) ;
#56909 = CARTESIAN_POINT ( 'NONE',  ( 6.071339422564090427, 0.1780416842499404351, -2.300786051158403733 ) ) ;
#56910 = DIRECTION ( 'NONE',  ( 0.06086575749407437119, 0.9962285034897238045, -0.06183953750876716726 ) ) ;
#56911 = ADVANCED_FACE ( 'NONE', ( #76127 ), #157395, .T. ) ;
#56912 = CARTESIAN_POINT ( 'NONE',  ( 3.819154011256303161, -1.728040176127441985, -0.9287006429716244682 ) ) ;
#56913 = CARTESIAN_POINT ( 'NONE',  ( 8.880754312151170282, 10.31963377138658089, 1.199719254218453823 ) ) ;
#56914 = CARTESIAN_POINT ( 'NONE',  ( 1.090470458312575053, -0.4872005951904456733, 1.956561897242928172 ) ) ;
#56915 = ORIENTED_EDGE ( 'NONE', *, *, #3142, .T. ) ;
#56916 = CARTESIAN_POINT ( 'NONE',  ( 2.518900147204519158, 0.2643050731806431686, 2.100751150841919657 ) ) ;
#56918 = CARTESIAN_POINT ( 'NONE',  ( -7.691553217654356622, 7.867900263551875994, -0.7998128361456291469 ) ) ;
#56917 = CARTESIAN_POINT ( 'NONE',  ( -2.300079615812729905, 5.835176651756807331, -0.7998128361456281477 ) ) ;
#56919 = CARTESIAN_POINT ( 'NONE',  ( 1.886409237429786279, 1.602333580200336671, -0.9066872629178088783 ) ) ;
#56920 = ORIENTED_EDGE ( 'NONE', *, *, #32633, .T. ) ;
#56921 = CARTESIAN_POINT ( 'NONE',  ( -9.297140650669053485, 11.86975006391249643, 1.599625672291281386 ) ) ;
#56922 = CARTESIAN_POINT ( 'NONE',  ( 6.189669738297051360, 5.317594965474103041, 2.438128856460785698 ) ) ;
#56923 = CARTESIAN_POINT ( 'NONE',  ( 4.131183091185314460, 1.940096312829143299, 0.8565103500411813675 ) ) ;
#56924 = CARTESIAN_POINT ( 'NONE',  ( 0.5504183687293667804, -1.553892155338543191, -0.9872222399871022347 ) ) ;
#56925 = CARTESIAN_POINT ( 'NONE',  ( 0.7499999999999920064, 5.264583334016151639, 1.299038105676669330 ) ) ;
#56926 = CARTESIAN_POINT ( 'NONE',  ( 7.401861798056875053, 10.72292363345333399, -1.199719254218441611 ) ) ;
#56927 = CARTESIAN_POINT ( 'NONE',  ( 6.851666526859736983, 9.086973262793417661, -1.599625672291269396 ) ) ;
#56928 = CARTESIAN_POINT ( 'NONE',  ( 3.954412886046823949, 0.7382688757093980314, 1.924196998259326996 ) ) ;
#56930 = CARTESIAN_POINT ( 'NONE',  ( 1.733694375844633706, 1.821329977863223926, 0.2691589665217360983 ) ) ;
#56929 = CARTESIAN_POINT ( 'NONE',  ( -5.930802130974132780, 9.006687355190106103, -1.199719254218440723 ) ) ;
#56931 = CARTESIAN_POINT ( 'NONE',  ( 1.364683531249990311, 5.113541667008084879, 0.7879004041258500513 ) ) ;
#56932 = CARTESIAN_POINT ( 'NONE',  ( 0.000000000000000000, 12.29999999999998295, 0.000000000000000000 ) ) ;
#56933 = CARTESIAN_POINT ( 'NONE',  ( -5.436182321379713578, 6.108390213082993903, 1.083092214668917919 ) ) ;
#56934 = LINE ( 'NONE', #184779, #177314 ) ;
#56935 = CARTESIAN_POINT ( 'NONE',  ( 0.5927436934281338221, -2.190715567557582677, -0.2661302102612560505 ) ) ;
#56936 = CARTESIAN_POINT ( 'NONE',  ( 3.726065177040696952, -1.343991584994163269, -1.819822530443465425 ) ) ;
#56938 = CARTESIAN_POINT ( 'NONE',  ( -8.188761592974051595, 9.616271948966963024, -1.082531754730543971 ) ) ;
#56937 = B_SPLINE_CURVE_WITH_KNOTS ( 'NONE', 3,
 ( #95020, #46265, #175204, #59291, #60354, #161070 ),
 .UNSPECIFIED., .F., .F.,
 ( 4, 2, 4 ),
 ( 0.000000000000000000, 0.0003779448103413555527, 0.0007558896206827111055 ),
 .UNSPECIFIED. ) ;
#56939 = CARTESIAN_POINT ( 'NONE',  ( 4.025510356283497515, -0.3035946714039591265, 1.785781755087331391 ) ) ;
#56940 = CARTESIAN_POINT ( 'NONE',  ( 3.696418550083080401, 1.350829783741511969, -1.358666786172907592 ) ) ;
#56941 = CARTESIAN_POINT ( 'NONE',  ( 5.125469573878929097, 0.2063957376101481500, -2.060066405364005426 ) ) ;
#56942 = CARTESIAN_POINT ( 'NONE',  ( 0.6823417656249917140, 3.655208333674754506, 1.181850606188765695 ) ) ;
#56943 = CARTESIAN_POINT ( 'NONE',  ( 2.659003877371171942, -1.714407010456520108, -0.9732827283935908680 ) ) ;
#56944 = CARTESIAN_POINT ( 'NONE',  ( 0.7098319175448050133, -1.917404841279496397, 0.1857973779731073583 ) ) ;
#56945 = CARTESIAN_POINT ( 'NONE',  ( 4.311305935566238645, -0.3199438451688824125, 1.842931056080451935 ) ) ;
#56946 = CARTESIAN_POINT ( 'NONE',  ( 1.928779914882609914, 1.326332282235458848, -1.888294200376864573 ) ) ;
#56947 = CARTESIAN_POINT ( 'NONE',  ( 3.244433657958167849, -1.833057675465451730, -0.3206290368645177136 ) ) ;
#56948 = CARTESIAN_POINT ( 'NONE',  ( -1.201851678989727383E-14, 3.821875000341423689, 1.575800808251672791 ) ) ;
#56949 = CLOSED_SHELL ( 'NONE', ( #178480, #60355, #94887, #170365, #5670, #77216, #94031, #197373, #115976, #99975 ) ) ;
#56950 = CARTESIAN_POINT ( 'NONE',  ( -3.815730167242251003, 6.539103397502874948, -1.199719254218452047 ) ) ;
#56951 = CARTESIAN_POINT ( 'NONE',  ( 5.880485940025228508, 7.883652901494672349, 1.599625672291267398 ) ) ;
#56952 = CARTESIAN_POINT ( 'NONE',  ( -2.788906526875773208E-15, 8.968750000682797818, -1.499999999999998446 ) ) ;
#56953 = CARTESIAN_POINT ( 'NONE',  ( 1.049603877184020373, -1.661282181752096410, -1.294363288650403732 ) ) ;
#56954 = CARTESIAN_POINT ( 'NONE',  ( 4.812781342726870193, 4.717259109377208048, 0.7216878364870317197 ) ) ;
#56956 = CARTESIAN_POINT ( 'NONE',  ( 5.081368137764759041, 4.913552992540472175, 0.1930038310255646206 ) ) ;
#56955 = CARTESIAN_POINT ( 'NONE',  ( 1.364683531249990311, 5.196875000341417916, 1.214306433183764966E-14 ) ) ;
#56957 = CARTESIAN_POINT ( 'NONE',  ( 1.310129046446480094, 4.152766000979581484, -0.4142140226951018245 ) ) ;
#56958 = CARTESIAN_POINT ( 'NONE',  ( 1.687894460584405731, 2.027760172737497424, -0.6205009303206151516 ) ) ;
#56959 = CARTESIAN_POINT ( 'NONE',  ( 0.7385429019767172365, 1.199765550694283478, -1.624703887242204825 ) ) ;
#56960 = CARTESIAN_POINT ( 'NONE',  ( -1.364683531250012516, 1.280208333674755172, 0.7879004041258379498 ) ) ;
#56961 = CARTESIAN_POINT ( 'NONE',  ( 4.635998460869027227, 7.496083073400806818, -1.199719254218452047 ) ) ;
#56962 = CARTESIAN_POINT ( 'NONE',  ( 1.440939128517594758, 0.4201678954103040819, 2.120193794684998245 ) ) ;
#56963 = CARTESIAN_POINT ( 'NONE',  ( 6.610000000000042952, 1.321253023796984172, 1.840686448008920229 ) ) ;
#56964 = EDGE_CURVE ( 'NONE', #96430, #33125, #54324, .T. ) ;
#56967 = CARTESIAN_POINT ( 'NONE',  ( 3.334942599281629949, 5.874221551595115720, -1.082531754730543083 ) ) ;
#56966 = FACE_OUTER_BOUND ( 'NONE', #57681, .T. ) ;
#56965 = CARTESIAN_POINT ( 'NONE',  ( 5.550083779947807550, 7.568460058062819407, -1.599625672291283607 ) ) ;
#56968 = CARTESIAN_POINT ( 'NONE',  ( -5.490125858891038213, 5.369844688319787451, -0.7998128361456362523 ) ) ;
#56969 = CARTESIAN_POINT ( 'NONE',  ( 6.139861302770143858, 2.010801613648224961, -0.1531635369260639090 ) ) ;
#56970 = CARTESIAN_POINT ( 'NONE',  ( -7.375272376154077492, 11.54830883891436422, -0.7216878364870267237 ) ) ;
#56971 = CARTESIAN_POINT ( 'NONE',  ( 0.1522426329377546128, 0.8445714516599597266, 2.022489037641273857 ) ) ;
#56972 = CARTESIAN_POINT ( 'NONE',  ( 1.500000000000009104, 5.004166666666691299, 0.8660254037844407060 ) ) ;
#56974 = CARTESIAN_POINT ( 'NONE',  ( 0.6823417656249934904, 10.69270833367473550, 1.181850606188764807 ) ) ;
#56973 = CARTESIAN_POINT ( 'NONE',  ( 0.2337813496832439053, -2.066932786716439541, 0.9205801711329018033 ) ) ;
#56975 = CARTESIAN_POINT ( 'NONE',  ( -8.676328237741483207, 12.20980114641871062, -1.199719254218446718 ) ) ;
#56977 = CARTESIAN_POINT ( 'NONE',  ( 0.8432031700210621539, 0.3724620109286616576, -1.878856871602401224 ) ) ;
#56976 = CARTESIAN_POINT ( 'NONE',  ( -6.209271164934474285, 6.346497235286081562, 1.040834085586084257E-14 ) ) ;
#56978 = CARTESIAN_POINT ( 'NONE',  ( -1.402160292154681736E-14, 1.259375000341419248, -1.575800808251659024 ) ) ;
#56979 = DIRECTION ( 'NONE',  ( 8.638326563840814399E-31, 0.000000000000000000, 1.000000000000000000 ) ) ;
#56980 = DIRECTION ( 'NONE',  ( 0.6507913734559640506, 0.7592566023653005702, 0.000000000000000000 ) ) ;
#56981 = CARTESIAN_POINT ( 'NONE',  ( 2.719059632816126282, -0.1691219839104734501, 1.716555610488319505 ) ) ;
#56982 = CARTESIAN_POINT ( 'NONE',  ( 5.716698046817569434, 6.698511138489155137, -1.199719254218452047 ) ) ;
#56983 = CARTESIAN_POINT ( 'NONE',  ( 0.5261445748756715668, 1.690971295752751624, 0.5220769596525741685 ) ) ;
#56984 = CARTESIAN_POINT ( 'NONE',  ( 1.647136526480545982, 0.1996500767776411833, 2.003181903140099696 ) ) ;
#56985 = CARTESIAN_POINT ( 'NONE',  ( 4.577303723630254062, 0.003709267837189236805, -2.206952907291927168 ) ) ;
#56986 = EDGE_LOOP ( 'NONE', ( #61819, #122721, #187159, #199682 ) ) ;
#56987 = CARTESIAN_POINT ( 'NONE',  ( 8.609064354553323639, 10.10662517080946543, -1.082531754730543083 ) ) ;
#56988 = CARTESIAN_POINT ( 'NONE',  ( -6.400331034103001748, 9.624747418832267698, 1.199719254218452935 ) ) ;
#56990 = CARTESIAN_POINT ( 'NONE',  ( 3.778922869151004171, 1.701937167235707982, -1.081084515101193633 ) ) ;
#56989 = CARTESIAN_POINT ( 'NONE',  ( 4.740951199079581180, 2.029406658027664623, 0.6148427566107574904 ) ) ;
#56991 = ORIENTED_EDGE ( 'NONE', *, *, #161090, .F. ) ;
#56992 = CARTESIAN_POINT ( 'NONE',  ( 4.362691568547328202, 8.311833606605697256, -0.7998128361456381397 ) ) ;
#56993 = ORIENTED_EDGE ( 'NONE', *, *, #129837, .F. ) ;
#56994 = CARTESIAN_POINT ( 'NONE',  ( 1.041631754505952134, 0.7616270086890539748, -1.708776438048253077 ) ) ;
#56995 = VECTOR ( 'NONE', #201680, 1000.000000000000000 ) ;
#56996 = CARTESIAN_POINT ( 'NONE',  ( 6.471393748265519719, 5.229711127717882491, -2.499999999999995115 ) ) ;
#56997 = CARTESIAN_POINT ( 'NONE',  ( -2.266184231778562541, 5.795632037050281404, 1.040834085586084257E-14 ) ) ;
#56998 = DIRECTION ( 'NONE',  ( 0.000000000000000000, -1.000000000000000000, 0.000000000000000000 ) ) ;
#56999 = CARTESIAN_POINT ( 'NONE',  ( -3.914243274428899966, 2.801588762746444417, 0.7750000000000135669 ) ) ;
#57000 = AXIS2_PLACEMENT_3D ( 'NONE', #204789, #53238, #104131 ) ;
#57001 = CARTESIAN_POINT ( 'NONE',  ( 1.364683531249988535, 2.926041667008082658, 0.7879004041258500513 ) ) ;
#57002 = DIRECTION ( 'NONE',  ( -0.000000000000000000, 1.000000000000000000, -0.000000000000000000 ) ) ;
#57003 = EDGE_CURVE ( 'NONE', #19657, #97605, #10706, .T. ) ;
#57004 = CARTESIAN_POINT ( 'NONE',  ( 7.241463443474815520, 8.581367117876336437, -1.082531754730548412 ) ) ;
#57005 = CARTESIAN_POINT ( 'NONE',  ( -3.526529353330355221, 6.168015774643768268, -1.082531754730546636 ) ) ;
#57006 = CARTESIAN_POINT ( 'NONE',  ( -7.096767062110449942, 7.244259425409119046, -0.7998128361456362523 ) ) ;
#57007 = CARTESIAN_POINT ( 'NONE',  ( 4.324552338190708056, -0.9094542848507057853, -1.915842285305848991 ) ) ;
#57009 = CARTESIAN_POINT ( 'NONE',  ( -10.01587959479698320, 5.734125918284786572, -5.906598880481439551 ) ) ;
#57008 = CARTESIAN_POINT ( 'NONE',  ( -0.1294898018152383368, 5.723764454335155349, -2.520545915250469893 ) ) ;
#57010 =( BOUNDED_SURFACE ( )  B_SPLINE_SURFACE ( 3, 3, ( 
 ( #10549, #178410, #142736, #208745, #95036, #108136, #207691, #110269, #143813, #59310, #79821, #144875, #91846, #128672, #125467, #43096, #109209, #175221, #27880, #112399, #96106, #26806, #127612, #162161, #145933, #209810, #28952, #211944, #160018, #92908, #63580, #60372, #126535, #192496, #44148, #61444, #129737, #193577, #176278, #93977, #45220, #161086, #12676, #111335, #78751, #210882, #183716, #100338, #35324, #132875, #32147, #149085, #66731, #65674, #198877, #148039, #97171, #80899, #33206, #665, #113470, #117727, #49462, #150174, #164279, #197830, #179475, #81954, #67799, #163226, #131821, #2806, #47355, #15869, #84086, #151237, #115582, #214047, #146988, #134998, #68878, #14808, #101402, #181576, #199956, #99289, #165337, #16930, #83010, #31099, #1741, #213007, #64643, #130783, #196776, #50524, #133948, #167477, #48419, #116648, #51602, #19072, #182644, #34264, #85153, #166403, #114531, #180524, #98227, #17996, #37466, #20136, #170667, #123096, #6008, #189053, #156569, #154430, #55853, #39602, #40690, #168538, #4930, #106793, #105706, #172821, #72078, #185835, #88364, #138189, #71006, #204198, #87290, #36394, #86222, #186910, #122009, #52653, #56923, #203148, #89440, #103544, #137119, #118782, #21187, #7075, #102472, #54791, #8164, #201008, #169605, #23331, #90505, #120937, #153359, #152293, #74248, #184768, #3867, #24393, #38542, #139253, #104619, #22254, #187976, #171734, #69940, #136052, #155492, #73147, #205285, #202064, #53724, #119857, #174963, #95852, #92653, #160828, #128419, #46029, #9236, #44964, #206360, #173904, #161908, #78500, #13495, #110011, #77435, #209546, #107878, #41765, #12420, #75308, #190111, #108942, #176024, #25479, #192234, #140342, #29767, #194386, #60118, #43897, #27616, #191169, #210632, #26545, #158695, #127349, #57987, #91586, #142474, #93716, #157638, #112150, #177078, #124150, #28694, #178152, #10293, #76367, #208482, #159757, #141424, #61189, #126277, #207430, #59049, #125207, #42836, #11354, #143552, #193318, #111072, #94780, #144617, #62258, #167223, #130536, #81703, #32957, #147785, #213801, #166146, #67547, #145689, #115338, #116392, #179218, #14551, #80647, #148836, #83821, #99032, #79570, #65424, #131573, #164039, #17732, #211687, #197574, #15614, #146739, #162971, #149914, #117465, #31903, #196527, #49218, #100085, #34010, #180279, #199695, #181329, #212757, #182380, #63323, #64392, #1481, #129484, #30843, #96920, #113213, #195466, #165087, #48170, #133691, #408, #114283, #198626, #16678, #47097, #51340, #97980, #82763, #66480, #132619, #50273, #101135, #183458, #35064, #169349, #136863, #205029, #200754, #203952, #52403, #139007, #38284, #118530, #135794, #134745, #102217, #137931, #202888, #54534, #186658, #104361, #184513, #188800, #39351, #69690, #5744, #68622, #187723, #153102, #170406, #84895, #37213, #55600, #6823, #105447, #120680, #3612, #71821, #201818, #168285, #36134, #20934, #53463, #85967, #152042, #23074, #19883, #121755, #119600, #185584, #103287, #87030, #4677, #70751, #21995, #89190, #88105, #122839, #171483, #72902, #154176, #155241, #56675, #40437, #106538, #18809, #150983, #2547, #60657, #27088, #209021, #61733, #160299, #127901, #77976, #76902, #176554, #177630, #48691, #11902, #29238, #128948, #95330, #161379, #47642, #163505, #93196, #211161, #212226 ),
 ( #172563, #12963, #45502, #28164, #44435, #113753, #213290, #193852, #144099, #79040, #196007, #130016, #111618, #81179, #145155, #110552, #63860, #159227, #94260, #179757, #10828, #126820, #192777, #210094, #143026, #62785, #194926, #31374, #96392, #46563, #80105, #112683, #178693, #147258, #30307, #162443, #14018, #146209, #97450, #197053, #15089, #64916, #131065, #18287, #86507, #82231, #85437, #148322, #20425, #134225, #214321, #17215, #16146, #198111, #19357, #84373, #150461, #68091, #200235, #65953, #70229, #135281, #165627, #101689, #164561, #69161, #34550, #51885, #180805, #133161, #151522, #102766, #201295, #2022, #99562, #3090, #116934, #32431, #152572, #132102, #118008, #183997, #49741, #115868, #136341, #182934, #35611, #50807, #167758, #4159, #181853, #52936, #33490, #202361, #119072, #83291, #149376, #959, #67025, #185053, #36678, #168821, #114806, #98497, #199162, #100621, #166696, #104913, #40982, #103834, #8449, #188266, #139552, #120150, #72375, #173115, #42053, #140636, #172037, #38829, #107093, #170954, #137408, #87581, #204497, #22553, #121231, #187201, #58282, #71296, #157933, #156863, #108166, #88659, #56147, #138475, #89737, #75598, #123376, #154719, #9526, #153652, #186127, #5221, #6300, #122308, #39906, #106016, #169882, #55082, #23630, #141710, #155786, #7371, #73448, #205579, #57216, #206649, #174193, #37761, #189342, #90799, #203427, #24696, #74536, #124438, #190396, #25765, #54011, #91877, #21472, #77723, #145962, #207720, #61476, #143845, #208774, #76654, #79853, #31128, #160047, #110300, #45248, #13778, #162191, #94008, #113499, #209838, #142769, #96139, #80927, #126565, #211972, #59344, #158983, #10580, #26836, #125497, #111365, #60403, #63611, #128700, #27911, #78782, #176308, #177370, #129767, #195750, #11651, #179507, #127641, #192526, #47387, #191460, #44180, #97202, #43126, #193606, #28984, #92939, #109240, #95070, #161118, #163255, #194668, #12705, #112429, #144903, #175250, #14837, #210911, #62538, #46313, #178442, #30049, #168566, #149116, #166438, #83042, #50553, #118813, #114563, #117758, #180555, #52683, #18029, #32177, #49491, #48449, #15899, #51633, #116675, #182673, #100368, #84116, #98253, #102503, #167506, #197859, #133978, #196806, #101433, #66762, #150203, #213040, #165368, #183748, #135026, #19104, #34295, #131851, #199986, #115612, #81983, #164310, #697, #181607, #214077, #65703, #151266, #148071, #36427, #35358, #201040, #33235, #132903, #16961, #1775, #20166, #67831, #99317, #147017, #198908, #64670, #85182, #2838, #68907, #184798, #130816, #202099, #87323, #88398, #173941, #137154, #154465, #39636, #6043, #72114, #172860, #74282, #152323, #122045, #123132, #185867, #21219, #153391, #155532, #90543, #105745, #86253, #138223, #204236, #170699, #24431, #3900, #55888, #22285, #4962, #190148, #37502, #53758, #56959, #119890, #206394, #171771, #103578, #203179, #169636, #71040, #205321, #188009, #23368, #89477, #7112, #54826, #41802, #106830, #120976, #73185, #136082, #40724, #139291, #189090, #69971, #104652, #156607, #140376, #8197, #58021, #186944, #124185, #38577, #107915, #59084, #176056, #76399, #92683, #158728, #29801, #42869, #129516, #128451, #13533, #208516, #27651, #43929, #61224, #47132, #94813, #60151, #195496, #125244, #91622, #191204, #126308, #10325, #192268 ),
 ( #110044, #209579, #207465, #77467, #113247, #25514, #79603, #159787, #143586, #127380, #142508, #95886, #93749, #11389, #12457, #157673, #141458, #193352, #44996, #177111, #111105, #145722, #28727, #194418, #9270, #108977, #75341, #174996, #160863, #46060, #161941, #26581, #78532, #211721, #63357, #144650, #210665, #62291, #112182, #178186, #51379, #163003, #81738, #15649, #212788, #148870, #101173, #198659, #167262, #134781, #132655, #34047, #17770, #18847, #146771, #197607, #84932, #83859, #151021, #50308, #64425, #49251, #2588, #149949, #68658, #116426, #164070, #66513, #182417, #115372, #100120, #65456, #14584, #130569, #165119, #166182, #30876, #35102, #181364, #67582, #147819, #32988, #96955, #213838, #199733, #80680, #99065, #200790, #179253, #131606, #1518, #52441, #16711, #82796, #196559, #48201, #114313, #180312, #31932, #445, #117502, #133727, #183493, #98014, #120719, #152078, #40471, #105482, #104396, #87067, #106574, #172601, #36173, #153139, #74026, #70787, #139040, #24180, #90283, #201856, #23109, #184552, #3648, #140116, #56707, #206142, #88140, #55634, #187757, #86004, #19919, #205065, #53500, #168324, #4713, #154210, #69727, #170443, #118567, #7936, #156352, #38320, #22031, #5780, #169385, #188835, #136900, #202929, #171515, #102250, #135831, #186692, #71859, #121790, #54571, #119637, #137966, #72936, #185621, #37253, #103323, #20970, #203987, #122874, #39386, #89224, #155277, #6857, #128207, #93499, #193099, #95642, #109800, #207214, #144410, #41544, #174752, #108726, #91364, #27399, #194168, #77214, #45815, #13287, #11137, #127129, #110854, #111935, #26325, #175807, #78282, #12211, #158478, #177937, #142258, #141203, #160609, #145478, #190952, #62052, #57773, #9015, #75091, #157424, #123934, #159539, #124993, #210410, #44748, #92439, #176862, #59903, #189902, #29550, #25263, #60973, #143333, #58838, #42616, #79360, #126056, #209326, #208270, #28474, #161693, #10078, #94566, #76154, #107658, #173687, #192018, #43681, #112996, #80425, #116181, #181118, #32737, #164869, #16463, #30623, #167013, #17523, #47958, #198416, #46884, #165938, #131366, #82543, #63107, #15401, #182166, #199479, #83611, #115122, #196314, #50060, #114073, #146524, #96712, #147569, #180065, #64183, #130324, #1275, #14335, #100925, #99875, #51123, #31688, #213590, #81492, #98817, #18605, #66266, #97764, #84685, #162761, #129275, #212543, #163823, #65215, #197361, #49004, #179009, #148631, #197, #211473, #132414, #33797, #149692, #67333, #133477, #117246, #183246, #195248, #34850, #187509, #35926, #85751, #151833, #5526, #155024, #104144, #23932, #4462, #70532, #20724, #88969, #150772, #136650, #86818, #3406, #40210, #102003, #184301, #21777, #202675, #152884, #6608, #2334, #54323, #120464, #69475, #106320, #168072, #19672, #87886, #53252, #186436, #171261, #105221, #36992, #56455, #38074, #135582, #39138, #68410, #201604, #72689, #134537, #119383, #185369, #103075, #200543, #170191, #169130, #22855, #71607, #153960, #55384, #137718, #52189, #122615, #118315, #203738, #121539, #138784, #204804, #172344, #188578, #109546, #26072, #208020, #61787, #57523, #60708, #123681, #210143, #175550, #189643, #206956, #205890, #173424, #209071, #59646, #125804, #43422, #27139, #41294, #45554, #110605, #140942, #76953, #139859, #44488, #9825, #93245 ),
 ( #92184, #58585, #157169, #8761, #94311, #107402, #193906, #192830, #78027, #124740, #158234, #108472, #191767, #111670, #159279, #190699, #177677, #25006, #156095, #91108, #42360, #74842, #174495, #75901, #142005, #10878, #143078, #90036, #126872, #176606, #28218, #160352, #11954, #144151, #127953, #7680, #73764, #66001, #129001, #178746, #30359, #98547, #33537, #197099, #119922, #97499, #115916, #147309, #14069, #16196, #80156, #112736, #62839, #179804, #146261, #96446, #162497, #99609, #46614, #136115, #132151, #17264, #212274, #31423, #47690, #64960, #53791, #164611, #63909, #202130, #194978, #95381, #130065, #196058, #113802, #163556, #15139, #145208, #81227, #213335, #29287, #131112, #48740, #114853, #180853, #32475, #181902, #86285, #161430, #82277, #198157, #148372, #214371, #49790, #165675, #152356, #3931, #13013, #70001, #79090, #211214, #124217, #185897, #39669, #55920, #186974, #75376, #71071, #4994, #56989, #88432, #23397, #206428, #140410, #72145, #91653, #122078, #54856, #74313, #59118, #104684, #190179, #37532, #137188, #203210, #121007, #103609, #89510, #38606, #58052, #106863, #6075, #90578, #188040, #169665, #157706, #153425, #189122, #123162, #170733, #22319, #207496, #105780, #205355, #171805, #155564, #9303, #154496, #156638, #138255, #141490, #40757, #204267, #7146, #87357, #73218, #8230, #139324, #172890, #24465, #41834, #107945, #21250, #173971, #25545, #112212, #175028, #79636, #45030, #210696, #191237, #143619, #29836, #113282, #160896, #78565, #144685, #158762, #80714, #145755, #176088, #178221, #26615, #211755, #111144, #62326, #42900, #209614, #95920, #179288, #63393, #28761, #110076, #161974, #27686, #208548, #10357, #61256, #93785, #192301, #43960, #129547, #142542, #14618, #13564, #30912, #159821, #127414, #193386, #12492, #146804, #194451, #11424, #212822, #76434, #109009, #60182, #77500, #177144, #94845, #128485, #92716, #126341, #46096, #125275, #195529, #47168, #96987, #163038, #16742, #133755, #183523, #130602, #132686, #149978, #31964, #15683, #81770, #34078, #51409, #198693, #2617, #82827, #148903, #33021, #117529, #64458, #477, #165151, #213868, #196591, #147850, #164100, #100147, #181397, #50337, #35132, #101204, #99098, #84961, #66543, #65491, #199764, #48233, #49286, #167290, #114346, #131638, #197641, #115404, #180343, #166211, #116457, #18877, #151050, #182450, #98047, #17803, #1549, #83887, #67610, #46797, #129184, #193004, #11050, #65128, #45728, #63014, #194075, #161606, #15313, #77129, #14240, #143251, #163732, #195162, #209241, #160521, #159452, #127044, #162670, #13195, #111847, #196228, #29464, #12125, #95554, #177852, #60885, #179978, #30536, #79272, #78197, #31599, #97675, #175717, #144324, #213507, #210322, #64093, #81402, #147485, #44657, #80334, #109713, #110771, #131286, #47870, #43595, #145389, #112910, #178921, #176771, #28386, #130235, #94481, #93414, #61959, #211388, #128117, #96616, #27309, #146435, #212449, #113981, #100841, #18520, #33710, #53167, #165853, #17438, #184217, #70451, #98726, #199392, #84598, #134455, #83522, #36904, #2248, #151748, #48913, #164785, #115033, #148545, #117161, #3319, #119295, #82456, #68324, #201519, #185282, #150686, #118233, #20641, #34768, #132323, #69388, #181032, #99787, #149603, #16377, #166926, #102986, #200458, #169044, #152800 ),
 ( #52104, #35840, #1188, #101918, #67252, #32649, #111, #183164, #167984, #66178, #86730, #51038, #85662, #133387, #19589, #198329, #135496, #4379, #49969, #197273, #116088, #182078, #105140, #173338, #25986, #154941, #171180, #21692, #9740, #92094, #104060, #58501, #74755, #136566, #106236, #73678, #205804, #170106, #37987, #8672, #5446, #186352, #22771, #172261, #87804, #188494, #202587, #158148, #124657, #56370, #40126, #23849, #187425, #206870, #88887, #6525, #123596, #54239, #153877, #138702, #89956, #139777, #72602, #190613, #156007, #91022, #120377, #71525, #137636, #203655, #122533, #157084, #42272, #55305, #7594, #140857, #108384, #57435, #189561, #174409, #41207, #121454, #39055, #204720, #107314, #24918, #2163, #86648, #150603, #204638, #52026, #87717, #170023, #19501, #118152, #106154, #152716, #103980, #20565, #202506, #56289, #184136, #55222, #35760, #122449, #21609, #101835, #201437, #200378, #167903, #203571, #54156, #120295, #37904, #153790, #85577, #40045, #105058, #135416, #71441, #134374, #38972, #4298, #5359, #68240, #102902, #121368, #72519, #171096, #186268, #69304, #137553, #53078, #151667, #3238, #70369, #119213, #185196, #36821, #88800, #168961, #188408, #187343, #138615, #136484, #22687, #154859, #6441, #172180, #84515, #58421, #127783, #123517, #89875, #57354, #124574, #8589, #190535, #140774, #42191, #142908, #11784, #110437, #141847, #74671, #10717, #206789, #107236, #189481, #174326, #108306, #90937, #157003, #28051, #41124, #193738, #126700, #77858, #25902, #92012, #158070, #59478, #45384, #93074, #9658, #111500, #173257, #155927, #24838, #75734, #207852, #125635, #191596, #139696, #43258, #109376, #23770, #175383, #26969, #159116, #76786, #208908, #176439, #143981, #7512, #60542, #192661, #44315, #94144, #160183, #209972, #61613, #73594, #205719, #31260, #97334, #47522, #115750, #177506, #163392, #113635, #178575, #66906, #62666, #211040, #48580, #79989, #14966, #197999, #131990, #63741, #83179, #179640, #46443, #65841, #50694, #96273, #181741, #29118, #128825, #194807, #112564, #95205, #81063, #30183, #49625, #13907, #199048, #161254, #147149, #12841, #149262, #145037, #180690, #114696, #162323, #146093, #78915, #213174, #196940, #64803, #130950, #841, #212104, #148210, #129900, #133046, #32315, #195884, #98383, #164447, #16034, #82117, #214212, #33371, #99452, #165509, #17101, #75217, #140245, #167646, #106698, #166584, #74151, #39505, #205185, #182820, #18173, #200126, #24301, #89344, #155392, #73056, #139155, #150345, #141328, #206266, #19247, #172723, #84260, #57891, #105604, #56826, #34436, #138087, #90406, #107783, #124054, #23232, #101578, #156476, #85327, #51779, #1915, #55753, #151410, #183889, #35501, #190020, #134117, #9143, #8065, #173808, #5905, #121909, #204101, #6975, #207341, #188953, #71978, #116818, #67974, #100509, #117896, #187878, #171635, #122996, #40593, #41672, #25387, #91486, #157547, #109920, #61098, #12328, #127257, #193228, #145597, #47003, #125118, #94693, #95760, #158603, #208394, #60028, #128331, #63229, #78408, #146645, #44875, #110980, #143456, #211593, #58963, #176986, #209454, #126179, #162877, #10202, #92563, #144529, #175931, #28604, #79479, #13403, #159665, #179125, #160734, #142385, #161813, #191076, #192143, #129392, #42743, #76277, #43807, #27524 ),
 ( #210538, #194294, #112058, #113119, #26454, #77344, #195371, #178058, #30747, #62172, #93623, #45939, #29676, #96828, #14457, #11266, #108848, #80548, #174874, #199607, #198537, #181236, #134661, #52313, #130447, #32864, #168196, #164994, #18723, #200664, #118443, #81609, #117375, #64302, #31811, #19795, #150896, #85879, #182294, #149825, #67456, #180189, #114190, #84807, #147693, #48079, #98940, #33921, #97887, #50183, #212660, #102127, #184430, #132539, #116304, #99996, #49128, #68533, #16585, #82667, #51250, #196435, #163948, #321, #166063, #1395, #148751, #36047, #17649, #167138, #15523, #213711, #65334, #131481, #83733, #2457, #197485, #115246, #133602, #66391, #183372, #34977, #101048, #189773, #203869, #86946, #24064, #135707, #54451, #155157, #153013, #156233, #4589, #171393, #73903, #107532, #105356, #6738, #204938, #139996, #119509, #170317, #206017, #56589, #57653, #22984, #136773, #39262, #89103, #21905, #72817, #38199, #201733, #185495, #137848, #138919, #3525, #7810, #154086, #40347, #120594, #88015, #69599, #186571, #172477, #53374, #5654, #173563, #151955, #104272, #188711, #41424, #71734, #55513, #37120, #25135, #103199, #169261, #123812, #121668, #90167, #187635, #122749, #106453, #20847, #70663, #202802, #145344, #8887, #125935, #46753, #43555, #111801, #79227, #211345, #174626, #210278, #157297, #124864, #112864, #29423, #178879, #60844, #28346, #160480, #58715, #207085, #177807, #26202, #141076, #59778, #127006, #190830, #143214, #91237, #195115, #62970, #11010, #209204, #192964, #142133, #161562, #191893, #109676, #78154, #74966, #42489, #93374, #44617, #94441, #175678, #129139, #110732, #45685, #108598, #92320, #158361, #9954, #77087, #95514, #13150, #76030, #176732, #208147, #27267, #12087, #144285, #159410, #61918, #128078, #194034, #14198, #147437, #33662, #31556, #34722, #97631, #49924, #166878, #200411, #198283, #99736, #83475, #18469, #212403, #48868, #84548, #149556, #150637, #116045, #15270, #132275, #182033, #114984, #165808, #131241, #80291, #64045, #16327, #17392, #96575, #100793, #32605, #133340, #213461, #180984, #162622, #65085, #50991, #146389, #98680, #52057, #30491, #197228, #67203, #134407, #164736, #82410, #130190, #118184, #196183, #47825, #2198, #148499, #183114, #67, #66131, #1141, #199344, #113937, #68275, #117112, #179932, #163688, #81357, #106190, #186302, #122483, #170057, #86682, #21642, #37938, #3270, #172215, #171130, #87749, #152749, #23804, #89909, #101869, #4331, #139731, #136519, #204674, #155961, #7547, #53113, #88837, #35792, #69337, #205755, #188445, #57385, #153826, #121404, #39007, #151701, #85613, #56323, #119246, #19536, #70400, #5396, #135448, #71475, #184172, #73632, #167936, #104012, #137587, #203604, #20596, #40078, #202537, #54186, #22723, #201470, #185230, #55257, #187376, #105091, #120326, #36853, #154895, #138652, #102937, #168997, #6477, #72554, #43293, #144016, #193773, #8624, #142942, #127818, #45419, #159150, #44350, #161291, #175418, #58455, #210009, #107268, #25940, #126736, #124610, #111535, #190568, #208942, #177542, #78953, #76822, #192696, #176472, #29153, #90974, #141878, #95243, #28083, #12877, #60578, #108341, #10751, #110472, #207887, #94179, #9693, #173288, #157036, #109413, #160218, #189513, #145075, #125667, #11819, #92047, #59510 ),
 ( #158104, #74705, #211078, #77895, #174361, #206821, #140809, #191629, #75770, #42224, #27002, #123549, #93108, #41159, #61651, #24870, #31294, #213209, #81095, #98417, #84295, #132025, #97369, #166619, #162362, #128862, #96306, #163427, #47560, #15004, #179674, #178612, #63776, #64838, #150380, #113670, #130984, #16068, #196975, #48614, #149298, #50729, #194844, #164482, #99489, #13941, #212140, #129935, #198035, #66945, #82152, #62701, #114729, #180727, #147184, #879, #46477, #32352, #148244, #195923, #18211, #80024, #146127, #214246, #65877, #49665, #83216, #17139, #115788, #182856, #181777, #33410, #165546, #112601, #133085, #199083, #30222, #116855, #34474, #100546, #89659, #120077, #69088, #88587, #52866, #23552, #134153, #4086, #68012, #122234, #183927, #5147, #87513, #151448, #35539, #1951, #70157, #21403, #152502, #186053, #188193, #101616, #187128, #167683, #39829, #153578, #19284, #119001, #117933, #85366, #121159, #37688, #103765, #169816, #71224, #3020, #171961, #22476, #184979, #203358, #51815, #170883, #136268, #137339, #200161, #20352, #38757, #204422, #154644, #55010, #201225, #135210, #104838, #138403, #36605, #6226, #72296, #56077, #105937, #102691, #86437, #168749, #202288, #53940, #26765, #140566, #43053, #175179, #174121, #92867, #41983, #205508, #189270, #141636, #109166, #7295, #11580, #157860, #44109, #58207, #91802, #73373, #190324, #176238, #57139, #25694, #111296, #155712, #124366, #192455, #45182, #9453, #108092, #40909, #28914, #177300, #123306, #77652, #75525, #93937, #207645, #59265, #125421, #191387, #107015, #143774, #142694, #158913, #10509, #209769, #61409, #139478, #76583, #173039, #208704, #27840, #127572, #193540, #24622, #60331, #90729, #156792, #8378, #159978, #74461, #126492, #110230, #206578, #62471, #210845, #181538, #178373, #144839, #63542, #64605, #128633, #146951, #182599, #198839, #82972, #14770, #212966, #130745, #145895, #165296, #129698, #195680, #81914, #94999, #194599, #97133, #196739, #32107, #47317, #149045, #114492, #49423, #161045, #46243, #12641, #112360, #80861, #115543, #16891, #29982, #180488, #99248, #621, #48379, #15828, #132835, #98192, #96067, #33166, #78711, #211905, #164240, #162120, #66688, #116606, #148001, #113430, #50485, #13709, #79782, #179437, #31057, #163186, #214012, #65634, #131782, #197786, #36347, #121966, #85107, #102425, #202020, #168494, #20093, #120895, #22209, #100295, #69896, #70965, #133906, #183676, #35281, #103501, #38500, #53680, #34223, #86181, #152250, #118739, #186868, #166362, #3823, #184723, #101357, #138147, #199912, #67755, #119811, #151193, #136007, #54745, #203100, #134955, #154386, #185791, #117684, #137075, #17953, #167435, #104578, #84040, #51559, #19027, #2764, #150128, #37424, #68835, #170623, #200963, #55811, #1701, #169561, #52610, #5964, #21143, #87247, #153312, #4887, #88322, #72034, #204156, #207395, #124112, #91544, #159720, #155449, #158659, #7032, #93678, #59014, #73109, #90465, #89400, #56881, #92617, #157603, #9198, #141385, #125171, #139209, #143513, #208446, #24355, #174928, #23290, #142439, #107837, #191131, #39562, #206322, #10258, #175986, #60079, #75270, #172782, #26508, #156532, #123056, #205240, #190075, #8123, #40653, #106754, #192198, #189010, #77397, #76332, #27580, #74209, #41727, #57947, #42797 ) ),
 .UNSPECIFIED., .T., .F., .T. ) 
 B_SPLINE_SURFACE_WITH_KNOTS ( ( 4, 3, 4 ),
 ( 4, 1, 1, 1, 1, 1, 1, 1, 1, 1, 1, 1, 1, 1, 1, 1, 1, 1, 1, 1, 1, 1, 1, 1, 1, 1, 1, 1, 1, 1, 1, 1, 1, 1, 1, 1, 1, 1, 1, 1, 1, 1, 1, 1, 1, 1, 1, 1, 1, 1, 1, 1, 1, 1, 1, 1, 1, 1, 1, 1, 1, 1, 1, 1, 1, 1, 1, 1, 1, 1, 1, 1, 1, 1, 1, 1, 1, 1, 1, 1, 1, 1, 1, 1, 1, 1, 1, 1, 1, 1, 1, 1, 1, 1, 1, 1, 1, 1, 1, 1, 1, 1, 1, 1, 1, 1, 1, 1, 1, 1, 1, 1, 1, 1, 1, 1, 1, 1, 1, 1, 1, 1, 1, 1, 1, 1, 1, 1, 1, 1, 1, 1, 1, 1, 1, 1, 1, 1, 1, 1, 1, 1, 1, 1, 1, 1, 1, 1, 1, 1, 1, 1, 1, 1, 1, 1, 1, 1, 1, 1, 1, 1, 1, 1, 1, 1, 1, 1, 1, 1, 1, 1, 1, 1, 1, 1, 1, 1, 1, 1, 1, 1, 1, 1, 1, 1, 1, 1, 1, 1, 1, 1, 1, 1, 1, 1, 1, 1, 1, 1, 1, 1, 1, 1, 1, 1, 1, 1, 1, 1, 1, 1, 1, 1, 1, 1, 1, 1, 1, 1, 1, 1, 1, 1, 1, 1, 1, 1, 1, 1, 1, 1, 1, 1, 1, 1, 1, 1, 1, 1, 1, 1, 1, 1, 1, 1, 1, 1, 1, 1, 1, 1, 1, 1, 1, 1, 1, 1, 1, 1, 1, 1, 1, 1, 1, 1, 1, 1, 1, 1, 1, 1, 1, 1, 1, 1, 1, 1, 1, 1, 1, 1, 1, 1, 1, 1, 1, 1, 1, 1, 1, 1, 1, 1, 1, 1, 1, 1, 1, 1, 1, 1, 1, 1, 1, 1, 1, 1, 1, 1, 1, 1, 1, 1, 1, 1, 1, 1, 1, 1, 1, 1, 1, 1, 1, 1, 1, 1, 1, 1, 1, 1, 1, 1, 1, 1, 1, 1, 1, 1, 1, 1, 1, 1, 1, 1, 1, 1, 1, 1, 1, 1, 1, 1, 1, 1, 1, 1, 1, 1, 1, 1, 1, 1, 1, 1, 1, 1, 1, 1, 1, 1, 1, 1, 1, 1, 1, 1, 1, 1, 1, 1, 1, 1, 4 ),
 ( 0.000000000000000000, 0.5000000000000000000, 1.000000000000000000 ),
 ( 0.000000000000000000, 0.002599942752653872004, 0.005208763852970823248, 0.007813103504395044890, 0.01041666580238601383, 0.01302040446826325734, 0.01562503794709516405, 0.01822898659850798186, 0.02083325479626091381, 0.02343751936515397344, 0.02604147156932860516, 0.02864593660736421826, 0.03124971754428982826, 0.03385421962853985695, 0.03645805019290717514, 0.03906245553539786086, 0.04166655880408994678, 0.04427067902208449424, 0.04687506736766395427, 0.04947890482860387018, 0.05208340383233839299, 0.05468718329397467132, 0.05729165635893663372, 0.05989559287350183087, 0.06249988401580178210, 0.06510415622071820396, 0.06770810475871495704, 0.07031256650665723695, 0.07291634835701975292, 0.07552085129243907291, 0.07812468146351797538, 0.08072908640827750060, 0.08333318980393969455, 0.08593730989448074287, 0.08854169822802662737, 0.09114553558425014801, 0.09375003453682481669, 0.09635381396055957282, 0.09895828689139142542, 0.1015622234206122604, 0.1041665143989399522, 0.1067707866525781646, 0.1093747350801187734, 0.1119791968332524285, 0.1145829786367304204, 0.1171874814968899975, 0.1197913116783300008, 0.1223957164865987768, 0.1249998199429257079, 0.1276039399106482508, 0.1302083283009266290, 0.1328121656006459317, 0.1354166645410730119, 0.1380204439687620910, 0.1406249168095159707, 0.1432288533966223909, 0.1458331442541831724, 0.1484374165996726891, 0.1510413649597071029, 0.1536458267615184170, 0.1562496085608837959, 0.1588541113892728840, 0.1614579416238982879, 0.1640623463390579739, 0.1666664498991252963, 0.1692705697871219883, 0.1718749582774928841, 0.1744787955635339893, 0.1770832945353020271, 0.1796870740097127606, 0.1822915468038420750, 0.1848954834917516388, 0.1874997742717963711, 0.1901040467523684718, 0.1927079950878241021, 0.1953124569817516476, 0.1979162388197689970, 0.2005207416598733527, 0.2031245719904950509, 0.2057289766559125821, 0.2083330803627857220, 0.2109372002141371993, 0.2135415888479497148, 0.2161454261631269858, 0.2187499252097131475, 0.2213537047736018060, 0.2239581775645482220, 0.2265621143961681627, 0.2291664051419355919, 0.2317706778008114532, 0.2343746261546043874, 0.2369790881840763974, 0.2395828701034999064, 0.2421873729987945312, 0.2447912034682135918, 0.2473956081272447038, 0.2499997120239797754, 0.2526038318817556694, 0.2552082207023498306, 0.2578120580894675551, 0.2604165572543392093, 0.2630203369504529598, 0.2656248097816475973, 0.2682287467998764607, 0.2708330375545950908, 0.2734373104349877015, 0.2760412588500244513, 0.2786457210584605826, 0.2812495031020356140, 0.2838540060959860445, 0.2864578367469951536, 0.2890622414429859233, 0.2916663455726313803, 0.2942704654798921071, 0.2968748545306000852, 0.2994786920324540302, 0.3020831913590704687, 0.3046869712301484290, 0.3072914441450140810, 0.3098953813927431966, 0.3124996721996327054, 0.3151039453447485039, 0.3177078938639273376, 0.3203123562947402525, 0.3229161385052047861, 0.3255206416412691484, 0.3281244725166545528, 0.3307288772929431464, 0.3333329816985414751, 0.3359371016983396796, 0.3385414910224879836, 0.3411453286818670882, 0.3437498282136811634, 0.3463536083024566503, 0.3489580813444087548, 0.3515620188645239841, 0.3541663097667969717, 0.3567705832198370119, 0.3593745318860498972, 0.3619789945826469846, 0.3645827770027332826, 0.3671872803243637073, 0.3697911114669067967, 0.3723955163668249413, 0.3749996210914142147, 0.3776037412267966853, 0.3802081308677072724, 0.3828119687273952576, 0.3854164685078552144, 0.3880202488570567709, 0.3906247220695055478, 0.3932286599048890885, 0.3958329509457525486, 0.3984372247499146091, 0.4010411736060487398, 0.4036456366118335581, 0.4062494192842699414, 0.4088539228349143406, 0.4114577542873927851, 0.4140621593542673784, 0.4166662644408827831, 0.4192703847548917562, 0.4218747747558840855, 0.4244786128586610641, 0.4270831129312115948, 0.4296868935835649328, 0.4322913670099168826, 0.4348953052034483235, 0.4374995964261053638, 0.4401038706245853915, 0.4427078197135246862, 0.4453122830718987402, 0.4479160660394111426, 0.4505205698625146526, 0.4531244016677045128, 0.4557288069448597878, 0.4583329124365353446, 0.4609370329722101700, 0.4635414233766025904, 0.4661452617652466213, 0.4687497621733308639, 0.4713535431715604185, 0.4739580168552197104, 0.4765619554497781962, 0.4791662468974299260, 0.4817705215334236457, 0.4843744708980504132, 0.4869789346524148743, 0.4895827179577280641, 0.4921872220967347111, 0.4947910542974118808, 0.4973954598281701278, 0.4999995657679404681, 0.5026036865683194410, 0.5052080774194306345, 0.5078119161367193879, 0.5104164169237808135, 0.5130201983106112973, 0.5156246722949818784, 0.5182286113334474420, 0.5208329030492938605, 0.5234371781659985512, 0.5260411278491948783, 0.5286455920429519173, 0.5312493757287917173, 0.5338538802271461936, 0.5364577128660878991, 0.5390621186937718523, 0.5416662251246735504, 0.5442703462327953545, 0.5468747375739465566, 0.5494785766626585355, 0.5520830778721422805, 0.5546868596903002935, 0.5572913340187868325, 0.5598952735440421158, 0.5624995655712847764, 0.5651038412119004928, 0.5677077912565504647, 0.5703122559331050834, 0.5729160400421993149, 0.5755205449433484777, 0.5781243780633351648, 0.5807287842312690573, 0.5833328911963423513, 0.5859370126552478908, 0.5885414045297637786, 0.5911452440326808722, 0.5937497457080352925, 0.5963535280002507655, 0.5989580027162609843, 0.6015619427711926814, 0.6041662351530351360, 0.6067705113607667622, 0.6093744618097575172, 0.6119789270125192138, 0.6145827115875999169, 0.6171872169349945647, 0.6197910505788110092, 0.6223954571303226269, 0.6249995646726131948, 0.6276036865253464825, 0.6302080789765573954, 0.6328119189364656005, 0.6354164211211439373, 0.6380202039301521300, 0.6406246790770983024, 0.6432286197045988807, 0.6458329124842493441, 0.6484371893023079814, 0.6510411401985315427, 0.6536456059709156996, 0.6562493910547204656, 0.6588538968918166150, 0.6614577311022542538, 0.6640621380806766005, 0.6666662462432366709, 0.6692703685328477148, 0.6718747616040910975, 0.6744786020637821844, 0.6770831048012443398, 0.6796868881697873954, 0.6822913637910873463, 0.6848953050340567117, 0.6874995982547292828, 0.6901038757263339152, 0.6927078271126885234, 0.6953122934981186276, 0.6979160791333920422, 0.7005205855036529261, 0.7031244203235108570, 0.7057288277721832648, 0.7083329365980738368, 0.7109370593676189731, 0.7135414531022405971, 0.7161452941045143294, 0.7187497974382286436, 0.7213535814090563658, 0.7239580575481356917, 0.7265619994494829648, 0.7291662931543987369, 0.7317705713227778963, 0.7343745232421703406, 0.7369789902840787610, 0.7395827765135741805, 0.7421872834604720248, 0.7447911189325585601, 0.7473955268948287989, 0.7499996364271210858, 0.7526037597196653106, 0.7552081541610216053, 0.7578119957486867397, 0.7604164997221309896, 0.7630202843380037292, 0.7656247610382975743, 0.7682287036409420899, 0.7708329978733315935, 0.7734372767817252470, 0.7760412292770711984, 0.7786456970189011839, 0.7812494838853828449, 0.7838539914523996455, 0.7864578276195345330, 0.7890622361387605865, 0.7916663464205372369, 0.7942704702791556493, 0.7968748654706151457, 0.7994787076864910969, 0.8020832123431549388, 0.8046869976468442598, 0.8072914749517984268, 0.8098954182986718431, 0.8124997131017763774, 0.8151039927934364826, 0.8177079459076636025, 0.8203124143928716139, 0.8229162019391148553, 0.8255207101697450423, 0.8281245470747605752, 0.8307289561943111966, 0.8333330672686687368, 0.8359371917364484261, 0.8385415877213925340, 0.8411454306083117061, 0.8437499359916976749, 0.8463537220259882421, 0.8489581999790609679, 0.8515621441131088210, 0.8541664395301816759, 0.8567707200483754004, 0.8593746738244238959, 0.8619791430964799384, 0.8645829313652741988, 0.8671874403030259693, 0.8697912779887684298, 0.8723956877520262498, 0.8749997996620757501, 0.8776039247821166844, 0.8802083216039426894, 0.8828121652047509205, 0.8854166713583762061, 0.8880204581660676721, 0.8906249368107317377, 0.8932288817749149956, 0.8958331778492237829, 0.8984374592372342816, 0.9010414137180589034, 0.9036458838204490807, 0.9062496728545991198, 0.9088541825429954368, 0.9114580210523274273, 0.9140624315026897317, 0.9166665442915585826, 0.9192706701069754960, 0.9218750678090992245, 0.9244789121666602272, 0.9270834191340497910, 0.9296872067579531329, 0.9322916861377325004, 0.9348956319750387767, 0.9374999287497546296, 0.9401042110508202043, 0.9427081662796877870, 0.9453126372565492375, 0.9479164270979697493, 0.9505209375757615042, 0.9531247769568838013, 0.9557291881641908349, 0.9583333018366511080, 0.9609374282806871781, 0.9635418271385329803, 0.9661456726567504427, 0.9687501794391485399, 0.9713539669241311181, 0.9739584505366999378, 0.9765624007674321705, 0.9791666904763859369, 0.9817709514985233366, 0.9843749191276834898, 0.9869795472165283634, 0.9895832986789295793, 0.9921868791097946394, 0.9947912178632822844, 0.9974000636350187632, 1.000000000000000000 ),
 .UNSPECIFIED. ) 
 GEOMETRIC_REPRESENTATION_ITEM ( )  RATIONAL_B_SPLINE_SURFACE ( (
 ( 1.000000000000000222, 1.000000000000000222, 1.000000000000000444, 1.000000000000000000, 1.000000000000000444, 1.000000000000000222, 1.000000000000000444, 0.9999999999999997780, 1.000000000000000444, 1.000000000000000000, 1.000000000000000444, 1.000000000000000000, 1.000000000000000444, 1.000000000000000222, 1.000000000000000000, 1.000000000000000666, 0.9999999999999997780, 1.000000000000000444, 1.000000000000000444, 1.000000000000000444, 1.000000000000000222, 1.000000000000000222, 1.000000000000000444, 1.000000000000000444, 1.000000000000000000, 1.000000000000000222, 1.000000000000000222, 1.000000000000000444, 1.000000000000000222, 1.000000000000000444, 1.000000000000000000, 1.000000000000000222, 1.000000000000000444, 1.000000000000000000, 1.000000000000000444, 1.000000000000000222, 1.000000000000000444, 1.000000000000000444, 1.000000000000000222, 1.000000000000000000, 1.000000000000000444, 1.000000000000000222, 1.000000000000000000, 1.000000000000000222, 1.000000000000000444, 1.000000000000000444, 1.000000000000000444, 1.000000000000000444, 1.000000000000000222, 1.000000000000000444, 1.000000000000000000, 1.000000000000000444, 1.000000000000000222, 1.000000000000000222, 1.000000000000000444, 1.000000000000000000, 1.000000000000000222, 1.000000000000000444, 1.000000000000000222, 1.000000000000000000, 1.000000000000000444, 1.000000000000000222, 1.000000000000000222, 1.000000000000000000, 1.000000000000000444, 0.9999999999999997780, 1.000000000000000444, 1.000000000000000000, 1.000000000000000444, 1.000000000000000000, 1.000000000000000444, 0.9999999999999997780, 1.000000000000000222, 1.000000000000000444, 1.000000000000000444, 1.000000000000000000, 1.000000000000000444, 1.000000000000000222, 1.000000000000000000, 1.000000000000000666, 1.000000000000000000, 1.000000000000000444, 1.000000000000000222, 1.000000000000000444, 0.9999999999999997780, 1.000000000000000444, 1.000000000000000000, 1.000000000000000444, 1.000000000000000444, 1.000000000000000222, 1.000000000000000222, 1.000000000000000444, 1.000000000000000222, 1.000000000000000444, 1.000000000000000444, 1.000000000000000222, 1.000000000000000444, 1.000000000000000222, 1.000000000000000444, 1.000000000000000000, 1.000000000000000444, 1.000000000000000000, 1.000000000000000000, 1.000000000000000444, 1.000000000000000222, 1.000000000000000222, 1.000000000000000444, 1.000000000000000000, 1.000000000000000444, 1.000000000000000000, 1.000000000000000222, 1.000000000000000444, 0.9999999999999997780, 1.000000000000000444, 1.000000000000000222, 1.000000000000000444, 1.000000000000000000, 1.000000000000000444, 1.000000000000000000, 1.000000000000000222, 1.000000000000000222, 1.000000000000000444, 1.000000000000000222, 1.000000000000000000, 1.000000000000000444, 1.000000000000000222, 1.000000000000000222, 1.000000000000000222, 1.000000000000000444, 0.9999999999999997780, 1.000000000000000666, 0.9999999999999996669, 1.000000000000000444, 1.000000000000000444, 1.000000000000000222, 1.000000000000000444, 1.000000000000000444, 1.000000000000000222, 1.000000000000000000, 1.000000000000000444, 1.000000000000000000, 1.000000000000000444, 1.000000000000000222, 1.000000000000000444, 1.000000000000000000, 1.000000000000000444, 1.000000000000000222, 1.000000000000000222, 1.000000000000000444, 1.000000000000000222, 0.9999999999999997780, 1.000000000000000444, 1.000000000000000444, 1.000000000000000444, 1.000000000000000222, 1.000000000000000444, 1.000000000000000444, 1.000000000000000222, 1.000000000000000444, 1.000000000000000000, 1.000000000000000222, 1.000000000000000444, 1.000000000000000000, 1.000000000000000222, 1.000000000000000444, 1.000000000000000000, 1.000000000000000444, 0.9999999999999997780, 1.000000000000000222, 1.000000000000000444, 1.000000000000000000, 1.000000000000000222, 1.000000000000000222, 1.000000000000000444, 1.000000000000000000, 1.000000000000000666, 0.9999999999999996669, 1.000000000000000666, 1.000000000000000222, 1.000000000000000444, 1.000000000000000222, 1.000000000000000444, 1.000000000000000222, 1.000000000000000222, 1.000000000000000000, 1.000000000000000444, 0.9999999999999997780, 1.000000000000000444, 1.000000000000000222, 1.000000000000000444, 0.9999999999999997780, 1.000000000000000444, 1.000000000000000000, 1.000000000000000222, 1.000000000000000444, 1.000000000000000000, 1.000000000000000444, 1.000000000000000444, 1.000000000000000222, 1.000000000000000222, 1.000000000000000000, 1.000000000000000444, 1.000000000000000444, 1.000000000000000000, 1.000000000000000222, 1.000000000000000222, 1.000000000000000444, 1.000000000000000222, 1.000000000000000222, 1.000000000000000444, 1.000000000000000222, 1.000000000000000000, 1.000000000000000444, 1.000000000000000000, 1.000000000000000222, 1.000000000000000444, 1.000000000000000222, 1.000000000000000222, 1.000000000000000444, 1.000000000000000000, 1.000000000000000222, 1.000000000000000222, 1.000000000000000222, 1.000000000000000000, 1.000000000000000222, 1.000000000000000222, 1.000000000000000000, 1.000000000000000222, 1.000000000000000222, 1.000000000000000444, 1.000000000000000000, 1.000000000000000000, 1.000000000000000222, 1.000000000000000000, 1.000000000000000888, 1.000000000000000000, 1.000000000000000444, 1.000000000000000222, 1.000000000000000222, 1.000000000000000444, 1.000000000000000222, 1.000000000000000222, 1.000000000000000444, 1.000000000000000444, 1.000000000000000222, 1.000000000000000444, 1.000000000000000222, 1.000000000000000000, 1.000000000000000222, 1.000000000000000444, 1.000000000000000444, 1.000000000000000222, 1.000000000000000444, 1.000000000000000222, 1.000000000000000444, 1.000000000000000222, 1.000000000000000444, 1.000000000000000222, 1.000000000000000000, 1.000000000000000444, 1.000000000000000000, 1.000000000000000666, 1.000000000000000000, 1.000000000000000000, 1.000000000000000444, 1.000000000000000222, 1.000000000000000444, 0.9999999999999997780, 1.000000000000000666, 1.000000000000000222, 1.000000000000000444, 1.000000000000000222, 1.000000000000000444, 1.000000000000000222, 1.000000000000000444, 0.9999999999999997780, 1.000000000000000666, 1.000000000000000222, 1.000000000000000222, 1.000000000000000444, 1.000000000000000444, 0.9999999999999997780, 1.000000000000000444, 1.000000000000000222, 1.000000000000000222, 1.000000000000000000, 1.000000000000000000, 1.000000000000000444, 1.000000000000000444, 1.000000000000000222, 1.000000000000000000, 1.000000000000000444, 0.9999999999999997780, 1.000000000000000444, 1.000000000000000222, 1.000000000000000000, 1.000000000000000222, 1.000000000000000000, 1.000000000000000444, 1.000000000000000000, 1.000000000000000444, 1.000000000000000222, 1.000000000000000222, 1.000000000000000222, 1.000000000000000222, 1.000000000000000222, 1.000000000000000444, 1.000000000000000222, 1.000000000000000444, 1.000000000000000222, 1.000000000000000000, 1.000000000000000888, 0.9999999999999996669, 1.000000000000000444, 1.000000000000000444, 1.000000000000000222, 1.000000000000000444, 1.000000000000000000, 1.000000000000000444, 0.9999999999999997780, 1.000000000000000444, 1.000000000000000222, 1.000000000000000444, 0.9999999999999997780, 1.000000000000000222, 1.000000000000000222, 1.000000000000000444, 1.000000000000000000, 1.000000000000000444, 1.000000000000000444, 1.000000000000000222, 1.000000000000000000, 1.000000000000000444, 1.000000000000000000, 1.000000000000000222, 1.000000000000000222, 1.000000000000000444, 1.000000000000000000, 1.000000000000000666, 1.000000000000000000, 1.000000000000000444, 1.000000000000000222, 1.000000000000000444, 1.000000000000000222, 1.000000000000000444, 1.000000000000000222, 1.000000000000000222, 1.000000000000000222, 1.000000000000000444, 1.000000000000000444, 1.000000000000000222, 1.000000000000000000, 1.000000000000000444, 1.000000000000000444, 1.000000000000000000, 1.000000000000000444, 0.9999999999999997780, 1.000000000000000444, 1.000000000000000222, 1.000000000000000222, 1.000000000000000444, 1.000000000000000222, 1.000000000000000222, 1.000000000000000444, 1.000000000000000444, 1.000000000000000444, 1.000000000000000000, 1.000000000000000444, 1.000000000000000222, 1.000000000000000222, 1.000000000000000000, 1.000000000000000444, 0.9999999999999997780, 1.000000000000000444, 1.000000000000000000, 1.000000000000000444, 1.000000000000000000, 1.000000000000000444, 1.000000000000000222, 1.000000000000000000, 1.000000000000000444, 1.000000000000000222, 1.000000000000000444, 0.9999999999999997780, 1.000000000000000444, 1.000000000000000222, 1.000000000000000222),
 ( 0.3333333333333334259, 0.3333333333333334259, 0.3333333333333334814, 0.3333333333333333703, 0.3333333333333335369, 0.3333333333333334259, 0.3333333333333334814, 0.3333333333333333703, 0.3333333333333334259, 0.3333333333333333703, 0.3333333333333335369, 0.3333333333333333703, 0.3333333333333334259, 0.3333333333333334259, 0.3333333333333333703, 0.3333333333333335369, 0.3333333333333333703, 0.3333333333333334259, 0.3333333333333335369, 0.3333333333333334259, 0.3333333333333333703, 0.3333333333333334259, 0.3333333333333334814, 0.3333333333333335369, 0.3333333333333333148, 0.3333333333333334259, 0.3333333333333334259, 0.3333333333333334814, 0.3333333333333334259, 0.3333333333333334259, 0.3333333333333334259, 0.3333333333333333148, 0.3333333333333335924, 0.3333333333333333148, 0.3333333333333335369, 0.3333333333333333703, 0.3333333333333335369, 0.3333333333333334259, 0.3333333333333333703, 0.3333333333333333703, 0.3333333333333335924, 0.3333333333333333148, 0.3333333333333334259, 0.3333333333333334259, 0.3333333333333335369, 0.3333333333333334814, 0.3333333333333334259, 0.3333333333333334259, 0.3333333333333334259, 0.3333333333333334259, 0.3333333333333333703, 0.3333333333333335369, 0.3333333333333334259, 0.3333333333333334259, 0.3333333333333334814, 0.3333333333333333703, 0.3333333333333333703, 0.3333333333333334814, 0.3333333333333334259, 0.3333333333333333703, 0.3333333333333334814, 0.3333333333333333703, 0.3333333333333334814, 0.3333333333333332593, 0.3333333333333335924, 0.3333333333333333148, 0.3333333333333335924, 0.3333333333333333148, 0.3333333333333335924, 0.3333333333333334259, 0.3333333333333334814, 0.3333333333333333703, 0.3333333333333333703, 0.3333333333333334814, 0.3333333333333335369, 0.3333333333333333703, 0.3333333333333334814, 0.3333333333333334259, 0.3333333333333333703, 0.3333333333333335369, 0.3333333333333333148, 0.3333333333333335369, 0.3333333333333334259, 0.3333333333333334259, 0.3333333333333333703, 0.3333333333333334259, 0.3333333333333333703, 0.3333333333333335369, 0.3333333333333333703, 0.3333333333333334259, 0.3333333333333334259, 0.3333333333333334814, 0.3333333333333333703, 0.3333333333333335924, 0.3333333333333333703, 0.3333333333333334259, 0.3333333333333334814, 0.3333333333333334259, 0.3333333333333335369, 0.3333333333333333148, 0.3333333333333335369, 0.3333333333333333148, 0.3333333333333334259, 0.3333333333333333703, 0.3333333333333334259, 0.3333333333333334259, 0.3333333333333335924, 0.3333333333333333703, 0.3333333333333335924, 0.3333333333333333148, 0.3333333333333335369, 0.3333333333333335369, 0.3333333333333333148, 0.3333333333333334259, 0.3333333333333334259, 0.3333333333333334814, 0.3333333333333333703, 0.3333333333333335369, 0.3333333333333333703, 0.3333333333333333703, 0.3333333333333334814, 0.3333333333333334814, 0.3333333333333334259, 0.3333333333333333703, 0.3333333333333334814, 0.3333333333333334814, 0.3333333333333334259, 0.3333333333333334259, 0.3333333333333334259, 0.3333333333333333703, 0.3333333333333335369, 0.3333333333333333703, 0.3333333333333334259, 0.3333333333333334814, 0.3333333333333334259, 0.3333333333333334814, 0.3333333333333334259, 0.3333333333333333703, 0.3333333333333333703, 0.3333333333333334259, 0.3333333333333333148, 0.3333333333333334814, 0.3333333333333334814, 0.3333333333333334259, 0.3333333333333333703, 0.3333333333333334259, 0.3333333333333334259, 0.3333333333333333703, 0.3333333333333335369, 0.3333333333333334259, 0.3333333333333333148, 0.3333333333333333703, 0.3333333333333335369, 0.3333333333333335369, 0.3333333333333333148, 0.3333333333333335369, 0.3333333333333334259, 0.3333333333333334259, 0.3333333333333335369, 0.3333333333333333703, 0.3333333333333333703, 0.3333333333333334259, 0.3333333333333333703, 0.3333333333333334259, 0.3333333333333334259, 0.3333333333333333703, 0.3333333333333335369, 0.3333333333333333703, 0.3333333333333334259, 0.3333333333333335369, 0.3333333333333333703, 0.3333333333333333703, 0.3333333333333334814, 0.3333333333333334259, 0.3333333333333333703, 0.3333333333333335369, 0.3333333333333332593, 0.3333333333333335369, 0.3333333333333335369, 0.3333333333333333703, 0.3333333333333334814, 0.3333333333333334814, 0.3333333333333334259, 0.3333333333333333703, 0.3333333333333334259, 0.3333333333333334814, 0.3333333333333333148, 0.3333333333333335369, 0.3333333333333333703, 0.3333333333333334259, 0.3333333333333333703, 0.3333333333333334259, 0.3333333333333333148, 0.3333333333333334259, 0.3333333333333334814, 0.3333333333333333703, 0.3333333333333334814, 0.3333333333333334259, 0.3333333333333333703, 0.3333333333333334259, 0.3333333333333333703, 0.3333333333333334259, 0.3333333333333334814, 0.3333333333333332593, 0.3333333333333334259, 0.3333333333333333703, 0.3333333333333335369, 0.3333333333333334259, 0.3333333333333333703, 0.3333333333333334259, 0.3333333333333334259, 0.3333333333333333148, 0.3333333333333335369, 0.3333333333333333703, 0.3333333333333334259, 0.3333333333333335924, 0.3333333333333333703, 0.3333333333333334259, 0.3333333333333335369, 0.3333333333333333703, 0.3333333333333334259, 0.3333333333333334259, 0.3333333333333334259, 0.3333333333333333703, 0.3333333333333334259, 0.3333333333333334259, 0.3333333333333333703, 0.3333333333333333148, 0.3333333333333334814, 0.3333333333333334259, 0.3333333333333334259, 0.3333333333333333703, 0.3333333333333333703, 0.3333333333333334259, 0.3333333333333335369, 0.3333333333333333703, 0.3333333333333335369, 0.3333333333333333703, 0.3333333333333334259, 0.3333333333333335369, 0.3333333333333333148, 0.3333333333333334259, 0.3333333333333334814, 0.3333333333333335369, 0.3333333333333333148, 0.3333333333333335369, 0.3333333333333333703, 0.3333333333333334259, 0.3333333333333333703, 0.3333333333333335369, 0.3333333333333334259, 0.3333333333333334259, 0.3333333333333334259, 0.3333333333333333703, 0.3333333333333335924, 0.3333333333333334259, 0.3333333333333335369, 0.3333333333333333148, 0.3333333333333333703, 0.3333333333333334814, 0.3333333333333333703, 0.3333333333333335924, 0.3333333333333333148, 0.3333333333333333703, 0.3333333333333335369, 0.3333333333333333703, 0.3333333333333335924, 0.3333333333333332593, 0.3333333333333335924, 0.3333333333333334259, 0.3333333333333335369, 0.3333333333333334259, 0.3333333333333334814, 0.3333333333333333703, 0.3333333333333334814, 0.3333333333333333148, 0.3333333333333335369, 0.3333333333333333148, 0.3333333333333334814, 0.3333333333333334814, 0.3333333333333334814, 0.3333333333333333148, 0.3333333333333335369, 0.3333333333333333148, 0.3333333333333335369, 0.3333333333333333703, 0.3333333333333333703, 0.3333333333333335369, 0.3333333333333334259, 0.3333333333333334259, 0.3333333333333333703, 0.3333333333333335369, 0.3333333333333333148, 0.3333333333333335924, 0.3333333333333334259, 0.3333333333333334259, 0.3333333333333333703, 0.3333333333333333703, 0.3333333333333334259, 0.3333333333333334259, 0.3333333333333334259, 0.3333333333333334259, 0.3333333333333334259, 0.3333333333333334259, 0.3333333333333334259, 0.3333333333333333703, 0.3333333333333335369, 0.3333333333333333703, 0.3333333333333334814, 0.3333333333333333703, 0.3333333333333333148, 0.3333333333333337034, 0.3333333333333332038, 0.3333333333333334814, 0.3333333333333335369, 0.3333333333333334814, 0.3333333333333334259, 0.3333333333333334259, 0.3333333333333334814, 0.3333333333333333703, 0.3333333333333334814, 0.3333333333333334259, 0.3333333333333334814, 0.3333333333333333148, 0.3333333333333333703, 0.3333333333333335369, 0.3333333333333334259, 0.3333333333333333703, 0.3333333333333335369, 0.3333333333333334814, 0.3333333333333334259, 0.3333333333333333703, 0.3333333333333334259, 0.3333333333333333148, 0.3333333333333335369, 0.3333333333333333148, 0.3333333333333335369, 0.3333333333333333703, 0.3333333333333335369, 0.3333333333333334259, 0.3333333333333334814, 0.3333333333333334259, 0.3333333333333335369, 0.3333333333333334259, 0.3333333333333334259, 0.3333333333333333703, 0.3333333333333334259, 0.3333333333333333703, 0.3333333333333335369, 0.3333333333333334814, 0.3333333333333333703, 0.3333333333333333148, 0.3333333333333335369, 0.3333333333333333703, 0.3333333333333333703, 0.3333333333333334814, 0.3333333333333333148, 0.3333333333333334814, 0.3333333333333333703, 0.3333333333333334259, 0.3333333333333334814, 0.3333333333333334814, 0.3333333333333334259, 0.3333333333333334259, 0.3333333333333335369, 0.3333333333333334814, 0.3333333333333333148, 0.3333333333333335369, 0.3333333333333334259, 0.3333333333333333703, 0.3333333333333334259, 0.3333333333333334259, 0.3333333333333333148, 0.3333333333333334814, 0.3333333333333333703, 0.3333333333333334259, 0.3333333333333333148, 0.3333333333333334814, 0.3333333333333334259, 0.3333333333333333148, 0.3333333333333334814, 0.3333333333333334259, 0.3333333333333334814, 0.3333333333333332593, 0.3333333333333335924, 0.3333333333333334259, 0.3333333333333334259),
 ( 0.3333333333333334259, 0.3333333333333334259, 0.3333333333333334814, 0.3333333333333333703, 0.3333333333333335369, 0.3333333333333334259, 0.3333333333333334814, 0.3333333333333333703, 0.3333333333333334259, 0.3333333333333333703, 0.3333333333333335369, 0.3333333333333333703, 0.3333333333333334259, 0.3333333333333334259, 0.3333333333333333703, 0.3333333333333335369, 0.3333333333333333703, 0.3333333333333334259, 0.3333333333333335369, 0.3333333333333334259, 0.3333333333333333703, 0.3333333333333334259, 0.3333333333333334814, 0.3333333333333335369, 0.3333333333333333148, 0.3333333333333334259, 0.3333333333333334259, 0.3333333333333334814, 0.3333333333333334259, 0.3333333333333334259, 0.3333333333333334259, 0.3333333333333333148, 0.3333333333333335924, 0.3333333333333333148, 0.3333333333333335369, 0.3333333333333333703, 0.3333333333333335369, 0.3333333333333334259, 0.3333333333333333703, 0.3333333333333333703, 0.3333333333333335924, 0.3333333333333333148, 0.3333333333333334259, 0.3333333333333334259, 0.3333333333333335369, 0.3333333333333334814, 0.3333333333333334259, 0.3333333333333334259, 0.3333333333333334259, 0.3333333333333334259, 0.3333333333333333703, 0.3333333333333335369, 0.3333333333333334259, 0.3333333333333334259, 0.3333333333333334814, 0.3333333333333333703, 0.3333333333333333703, 0.3333333333333334814, 0.3333333333333334259, 0.3333333333333333703, 0.3333333333333334814, 0.3333333333333333703, 0.3333333333333334814, 0.3333333333333332593, 0.3333333333333335924, 0.3333333333333333148, 0.3333333333333335924, 0.3333333333333333148, 0.3333333333333335924, 0.3333333333333334259, 0.3333333333333334814, 0.3333333333333333703, 0.3333333333333333703, 0.3333333333333334814, 0.3333333333333335369, 0.3333333333333333703, 0.3333333333333334814, 0.3333333333333334259, 0.3333333333333333703, 0.3333333333333335369, 0.3333333333333333148, 0.3333333333333335369, 0.3333333333333334259, 0.3333333333333334259, 0.3333333333333333703, 0.3333333333333334259, 0.3333333333333333703, 0.3333333333333335369, 0.3333333333333333703, 0.3333333333333334259, 0.3333333333333334259, 0.3333333333333334814, 0.3333333333333333703, 0.3333333333333335924, 0.3333333333333333703, 0.3333333333333334259, 0.3333333333333334814, 0.3333333333333334259, 0.3333333333333335369, 0.3333333333333333148, 0.3333333333333335369, 0.3333333333333333148, 0.3333333333333334259, 0.3333333333333333703, 0.3333333333333334259, 0.3333333333333334259, 0.3333333333333335924, 0.3333333333333333703, 0.3333333333333335924, 0.3333333333333333148, 0.3333333333333335369, 0.3333333333333335369, 0.3333333333333333148, 0.3333333333333334259, 0.3333333333333334259, 0.3333333333333334814, 0.3333333333333333703, 0.3333333333333335369, 0.3333333333333333703, 0.3333333333333333703, 0.3333333333333334814, 0.3333333333333334814, 0.3333333333333334259, 0.3333333333333333703, 0.3333333333333334814, 0.3333333333333334814, 0.3333333333333334259, 0.3333333333333334259, 0.3333333333333334259, 0.3333333333333333703, 0.3333333333333335369, 0.3333333333333333703, 0.3333333333333334259, 0.3333333333333334814, 0.3333333333333334259, 0.3333333333333334814, 0.3333333333333334259, 0.3333333333333333703, 0.3333333333333333703, 0.3333333333333334259, 0.3333333333333333148, 0.3333333333333334814, 0.3333333333333334814, 0.3333333333333334259, 0.3333333333333333703, 0.3333333333333334259, 0.3333333333333334259, 0.3333333333333333703, 0.3333333333333335369, 0.3333333333333334259, 0.3333333333333333148, 0.3333333333333333703, 0.3333333333333335369, 0.3333333333333335369, 0.3333333333333333148, 0.3333333333333335369, 0.3333333333333334259, 0.3333333333333334259, 0.3333333333333335369, 0.3333333333333333703, 0.3333333333333333703, 0.3333333333333334259, 0.3333333333333333703, 0.3333333333333334259, 0.3333333333333334259, 0.3333333333333333703, 0.3333333333333335369, 0.3333333333333333703, 0.3333333333333334259, 0.3333333333333335369, 0.3333333333333333703, 0.3333333333333333703, 0.3333333333333334814, 0.3333333333333334259, 0.3333333333333333703, 0.3333333333333335369, 0.3333333333333332593, 0.3333333333333335369, 0.3333333333333335369, 0.3333333333333333703, 0.3333333333333334814, 0.3333333333333334814, 0.3333333333333334259, 0.3333333333333333703, 0.3333333333333334259, 0.3333333333333334814, 0.3333333333333333148, 0.3333333333333335369, 0.3333333333333333703, 0.3333333333333334259, 0.3333333333333333703, 0.3333333333333334259, 0.3333333333333333148, 0.3333333333333334259, 0.3333333333333334814, 0.3333333333333333703, 0.3333333333333334814, 0.3333333333333334259, 0.3333333333333333703, 0.3333333333333334259, 0.3333333333333333703, 0.3333333333333334259, 0.3333333333333334814, 0.3333333333333332593, 0.3333333333333334259, 0.3333333333333333703, 0.3333333333333335369, 0.3333333333333334259, 0.3333333333333333703, 0.3333333333333334259, 0.3333333333333334259, 0.3333333333333333148, 0.3333333333333335369, 0.3333333333333333703, 0.3333333333333334259, 0.3333333333333335924, 0.3333333333333333703, 0.3333333333333334259, 0.3333333333333335369, 0.3333333333333333703, 0.3333333333333334259, 0.3333333333333334259, 0.3333333333333334259, 0.3333333333333333703, 0.3333333333333334259, 0.3333333333333334259, 0.3333333333333333703, 0.3333333333333333148, 0.3333333333333334814, 0.3333333333333334259, 0.3333333333333334259, 0.3333333333333333703, 0.3333333333333333703, 0.3333333333333334259, 0.3333333333333335369, 0.3333333333333333703, 0.3333333333333335369, 0.3333333333333333703, 0.3333333333333334259, 0.3333333333333335369, 0.3333333333333333148, 0.3333333333333334259, 0.3333333333333334814, 0.3333333333333335369, 0.3333333333333333148, 0.3333333333333335369, 0.3333333333333333703, 0.3333333333333334259, 0.3333333333333333703, 0.3333333333333335369, 0.3333333333333334259, 0.3333333333333334259, 0.3333333333333334259, 0.3333333333333333703, 0.3333333333333335924, 0.3333333333333334259, 0.3333333333333335369, 0.3333333333333333148, 0.3333333333333333703, 0.3333333333333334814, 0.3333333333333333703, 0.3333333333333335924, 0.3333333333333333148, 0.3333333333333333703, 0.3333333333333335369, 0.3333333333333333703, 0.3333333333333335924, 0.3333333333333332593, 0.3333333333333335924, 0.3333333333333334259, 0.3333333333333335369, 0.3333333333333334259, 0.3333333333333334814, 0.3333333333333333703, 0.3333333333333334814, 0.3333333333333333148, 0.3333333333333335369, 0.3333333333333333148, 0.3333333333333334814, 0.3333333333333334814, 0.3333333333333334814, 0.3333333333333333148, 0.3333333333333335369, 0.3333333333333333148, 0.3333333333333335369, 0.3333333333333333703, 0.3333333333333333703, 0.3333333333333335369, 0.3333333333333334259, 0.3333333333333334259, 0.3333333333333333703, 0.3333333333333335369, 0.3333333333333333148, 0.3333333333333335924, 0.3333333333333334259, 0.3333333333333334259, 0.3333333333333333703, 0.3333333333333333703, 0.3333333333333334259, 0.3333333333333334259, 0.3333333333333334259, 0.3333333333333334259, 0.3333333333333334259, 0.3333333333333334259, 0.3333333333333334259, 0.3333333333333333703, 0.3333333333333335369, 0.3333333333333333703, 0.3333333333333334814, 0.3333333333333333703, 0.3333333333333333148, 0.3333333333333337034, 0.3333333333333332038, 0.3333333333333334814, 0.3333333333333335369, 0.3333333333333334814, 0.3333333333333334259, 0.3333333333333334259, 0.3333333333333334814, 0.3333333333333333703, 0.3333333333333334814, 0.3333333333333334259, 0.3333333333333334814, 0.3333333333333333148, 0.3333333333333333703, 0.3333333333333335369, 0.3333333333333334259, 0.3333333333333333703, 0.3333333333333335369, 0.3333333333333334814, 0.3333333333333334259, 0.3333333333333333703, 0.3333333333333334259, 0.3333333333333333148, 0.3333333333333335369, 0.3333333333333333148, 0.3333333333333335369, 0.3333333333333333703, 0.3333333333333335369, 0.3333333333333334259, 0.3333333333333334814, 0.3333333333333334259, 0.3333333333333335369, 0.3333333333333334259, 0.3333333333333334259, 0.3333333333333333703, 0.3333333333333334259, 0.3333333333333333703, 0.3333333333333335369, 0.3333333333333334814, 0.3333333333333333703, 0.3333333333333333148, 0.3333333333333335369, 0.3333333333333333703, 0.3333333333333333703, 0.3333333333333334814, 0.3333333333333333148, 0.3333333333333334814, 0.3333333333333333703, 0.3333333333333334259, 0.3333333333333334814, 0.3333333333333334814, 0.3333333333333334259, 0.3333333333333334259, 0.3333333333333335369, 0.3333333333333334814, 0.3333333333333333148, 0.3333333333333335369, 0.3333333333333334259, 0.3333333333333333703, 0.3333333333333334259, 0.3333333333333334259, 0.3333333333333333148, 0.3333333333333334814, 0.3333333333333333703, 0.3333333333333334259, 0.3333333333333333148, 0.3333333333333334814, 0.3333333333333334259, 0.3333333333333333148, 0.3333333333333334814, 0.3333333333333334259, 0.3333333333333334814, 0.3333333333333332593, 0.3333333333333335924, 0.3333333333333334259, 0.3333333333333334259),
 ( 1.000000000000000222, 1.000000000000000222, 1.000000000000000444, 1.000000000000000000, 1.000000000000000444, 1.000000000000000222, 1.000000000000000444, 0.9999999999999997780, 1.000000000000000444, 1.000000000000000000, 1.000000000000000444, 1.000000000000000000, 1.000000000000000444, 1.000000000000000222, 1.000000000000000000, 1.000000000000000666, 0.9999999999999997780, 1.000000000000000444, 1.000000000000000444, 1.000000000000000444, 1.000000000000000222, 1.000000000000000222, 1.000000000000000444, 1.000000000000000444, 1.000000000000000000, 1.000000000000000222, 1.000000000000000222, 1.000000000000000444, 1.000000000000000222, 1.000000000000000444, 1.000000000000000000, 1.000000000000000222, 1.000000000000000444, 1.000000000000000000, 1.000000000000000444, 1.000000000000000222, 1.000000000000000444, 1.000000000000000444, 1.000000000000000222, 1.000000000000000000, 1.000000000000000444, 1.000000000000000222, 1.000000000000000000, 1.000000000000000222, 1.000000000000000444, 1.000000000000000444, 1.000000000000000444, 1.000000000000000444, 1.000000000000000222, 1.000000000000000444, 1.000000000000000000, 1.000000000000000444, 1.000000000000000222, 1.000000000000000222, 1.000000000000000444, 1.000000000000000000, 1.000000000000000222, 1.000000000000000444, 1.000000000000000222, 1.000000000000000000, 1.000000000000000444, 1.000000000000000222, 1.000000000000000222, 1.000000000000000000, 1.000000000000000444, 0.9999999999999997780, 1.000000000000000444, 1.000000000000000000, 1.000000000000000444, 1.000000000000000000, 1.000000000000000444, 0.9999999999999997780, 1.000000000000000222, 1.000000000000000444, 1.000000000000000444, 1.000000000000000000, 1.000000000000000444, 1.000000000000000222, 1.000000000000000000, 1.000000000000000666, 1.000000000000000000, 1.000000000000000444, 1.000000000000000222, 1.000000000000000444, 0.9999999999999997780, 1.000000000000000444, 1.000000000000000000, 1.000000000000000444, 1.000000000000000444, 1.000000000000000222, 1.000000000000000222, 1.000000000000000444, 1.000000000000000222, 1.000000000000000444, 1.000000000000000444, 1.000000000000000222, 1.000000000000000444, 1.000000000000000222, 1.000000000000000444, 1.000000000000000000, 1.000000000000000444, 1.000000000000000000, 1.000000000000000000, 1.000000000000000444, 1.000000000000000222, 1.000000000000000222, 1.000000000000000444, 1.000000000000000000, 1.000000000000000444, 1.000000000000000000, 1.000000000000000222, 1.000000000000000444, 0.9999999999999997780, 1.000000000000000444, 1.000000000000000222, 1.000000000000000444, 1.000000000000000000, 1.000000000000000444, 1.000000000000000000, 1.000000000000000222, 1.000000000000000222, 1.000000000000000444, 1.000000000000000222, 1.000000000000000000, 1.000000000000000444, 1.000000000000000222, 1.000000000000000222, 1.000000000000000222, 1.000000000000000444, 0.9999999999999997780, 1.000000000000000666, 0.9999999999999996669, 1.000000000000000444, 1.000000000000000444, 1.000000000000000222, 1.000000000000000444, 1.000000000000000444, 1.000000000000000222, 1.000000000000000000, 1.000000000000000444, 1.000000000000000000, 1.000000000000000444, 1.000000000000000222, 1.000000000000000444, 1.000000000000000000, 1.000000000000000444, 1.000000000000000222, 1.000000000000000222, 1.000000000000000444, 1.000000000000000222, 0.9999999999999997780, 1.000000000000000444, 1.000000000000000444, 1.000000000000000444, 1.000000000000000222, 1.000000000000000444, 1.000000000000000444, 1.000000000000000222, 1.000000000000000444, 1.000000000000000000, 1.000000000000000222, 1.000000000000000444, 1.000000000000000000, 1.000000000000000222, 1.000000000000000444, 1.000000000000000000, 1.000000000000000444, 0.9999999999999997780, 1.000000000000000222, 1.000000000000000444, 1.000000000000000000, 1.000000000000000222, 1.000000000000000222, 1.000000000000000444, 1.000000000000000000, 1.000000000000000666, 0.9999999999999996669, 1.000000000000000666, 1.000000000000000222, 1.000000000000000444, 1.000000000000000222, 1.000000000000000444, 1.000000000000000222, 1.000000000000000222, 1.000000000000000000, 1.000000000000000444, 0.9999999999999997780, 1.000000000000000444, 1.000000000000000222, 1.000000000000000444, 0.9999999999999997780, 1.000000000000000444, 1.000000000000000000, 1.000000000000000222, 1.000000000000000444, 1.000000000000000000, 1.000000000000000444, 1.000000000000000444, 1.000000000000000222, 1.000000000000000222, 1.000000000000000000, 1.000000000000000444, 1.000000000000000444, 1.000000000000000000, 1.000000000000000222, 1.000000000000000222, 1.000000000000000444, 1.000000000000000222, 1.000000000000000222, 1.000000000000000444, 1.000000000000000222, 1.000000000000000000, 1.000000000000000444, 1.000000000000000000, 1.000000000000000222, 1.000000000000000444, 1.000000000000000222, 1.000000000000000222, 1.000000000000000444, 1.000000000000000000, 1.000000000000000222, 1.000000000000000222, 1.000000000000000222, 1.000000000000000000, 1.000000000000000222, 1.000000000000000222, 1.000000000000000000, 1.000000000000000222, 1.000000000000000222, 1.000000000000000444, 1.000000000000000000, 1.000000000000000000, 1.000000000000000222, 1.000000000000000000, 1.000000000000000888, 1.000000000000000000, 1.000000000000000444, 1.000000000000000222, 1.000000000000000222, 1.000000000000000444, 1.000000000000000222, 1.000000000000000222, 1.000000000000000444, 1.000000000000000444, 1.000000000000000222, 1.000000000000000444, 1.000000000000000222, 1.000000000000000000, 1.000000000000000222, 1.000000000000000444, 1.000000000000000444, 1.000000000000000222, 1.000000000000000444, 1.000000000000000222, 1.000000000000000444, 1.000000000000000222, 1.000000000000000444, 1.000000000000000222, 1.000000000000000000, 1.000000000000000444, 1.000000000000000000, 1.000000000000000666, 1.000000000000000000, 1.000000000000000000, 1.000000000000000444, 1.000000000000000222, 1.000000000000000444, 0.9999999999999997780, 1.000000000000000666, 1.000000000000000222, 1.000000000000000444, 1.000000000000000222, 1.000000000000000444, 1.000000000000000222, 1.000000000000000444, 0.9999999999999997780, 1.000000000000000666, 1.000000000000000222, 1.000000000000000222, 1.000000000000000444, 1.000000000000000444, 0.9999999999999997780, 1.000000000000000444, 1.000000000000000222, 1.000000000000000222, 1.000000000000000000, 1.000000000000000000, 1.000000000000000444, 1.000000000000000444, 1.000000000000000222, 1.000000000000000000, 1.000000000000000444, 0.9999999999999997780, 1.000000000000000444, 1.000000000000000222, 1.000000000000000000, 1.000000000000000222, 1.000000000000000000, 1.000000000000000444, 1.000000000000000000, 1.000000000000000444, 1.000000000000000222, 1.000000000000000222, 1.000000000000000222, 1.000000000000000222, 1.000000000000000222, 1.000000000000000444, 1.000000000000000222, 1.000000000000000444, 1.000000000000000222, 1.000000000000000000, 1.000000000000000888, 0.9999999999999996669, 1.000000000000000444, 1.000000000000000444, 1.000000000000000222, 1.000000000000000444, 1.000000000000000000, 1.000000000000000444, 0.9999999999999997780, 1.000000000000000444, 1.000000000000000222, 1.000000000000000444, 0.9999999999999997780, 1.000000000000000222, 1.000000000000000222, 1.000000000000000444, 1.000000000000000000, 1.000000000000000444, 1.000000000000000444, 1.000000000000000222, 1.000000000000000000, 1.000000000000000444, 1.000000000000000000, 1.000000000000000222, 1.000000000000000222, 1.000000000000000444, 1.000000000000000000, 1.000000000000000666, 1.000000000000000000, 1.000000000000000444, 1.000000000000000222, 1.000000000000000444, 1.000000000000000222, 1.000000000000000444, 1.000000000000000222, 1.000000000000000222, 1.000000000000000222, 1.000000000000000444, 1.000000000000000444, 1.000000000000000222, 1.000000000000000000, 1.000000000000000444, 1.000000000000000444, 1.000000000000000000, 1.000000000000000444, 0.9999999999999997780, 1.000000000000000444, 1.000000000000000222, 1.000000000000000222, 1.000000000000000444, 1.000000000000000222, 1.000000000000000222, 1.000000000000000444, 1.000000000000000444, 1.000000000000000444, 1.000000000000000000, 1.000000000000000444, 1.000000000000000222, 1.000000000000000222, 1.000000000000000000, 1.000000000000000444, 0.9999999999999997780, 1.000000000000000444, 1.000000000000000000, 1.000000000000000444, 1.000000000000000000, 1.000000000000000444, 1.000000000000000222, 1.000000000000000000, 1.000000000000000444, 1.000000000000000222, 1.000000000000000444, 0.9999999999999997780, 1.000000000000000444, 1.000000000000000222, 1.000000000000000222),
 ( 0.3333333333333334259, 0.3333333333333334259, 0.3333333333333334814, 0.3333333333333333703, 0.3333333333333335369, 0.3333333333333334259, 0.3333333333333334814, 0.3333333333333333703, 0.3333333333333334259, 0.3333333333333333703, 0.3333333333333335369, 0.3333333333333333703, 0.3333333333333334259, 0.3333333333333334259, 0.3333333333333333703, 0.3333333333333335369, 0.3333333333333333703, 0.3333333333333334259, 0.3333333333333335369, 0.3333333333333334259, 0.3333333333333333703, 0.3333333333333334259, 0.3333333333333334814, 0.3333333333333335369, 0.3333333333333333148, 0.3333333333333334259, 0.3333333333333334259, 0.3333333333333334814, 0.3333333333333334259, 0.3333333333333334259, 0.3333333333333334259, 0.3333333333333333148, 0.3333333333333335924, 0.3333333333333333148, 0.3333333333333335369, 0.3333333333333333703, 0.3333333333333335369, 0.3333333333333334259, 0.3333333333333333703, 0.3333333333333333703, 0.3333333333333335924, 0.3333333333333333148, 0.3333333333333334259, 0.3333333333333334259, 0.3333333333333335369, 0.3333333333333334814, 0.3333333333333334259, 0.3333333333333334259, 0.3333333333333334259, 0.3333333333333334259, 0.3333333333333333703, 0.3333333333333335369, 0.3333333333333334259, 0.3333333333333334259, 0.3333333333333334814, 0.3333333333333333703, 0.3333333333333333703, 0.3333333333333334814, 0.3333333333333334259, 0.3333333333333333703, 0.3333333333333334814, 0.3333333333333333703, 0.3333333333333334814, 0.3333333333333332593, 0.3333333333333335924, 0.3333333333333333148, 0.3333333333333335924, 0.3333333333333333148, 0.3333333333333335924, 0.3333333333333334259, 0.3333333333333334814, 0.3333333333333333703, 0.3333333333333333703, 0.3333333333333334814, 0.3333333333333335369, 0.3333333333333333703, 0.3333333333333334814, 0.3333333333333334259, 0.3333333333333333703, 0.3333333333333335369, 0.3333333333333333148, 0.3333333333333335369, 0.3333333333333334259, 0.3333333333333334259, 0.3333333333333333703, 0.3333333333333334259, 0.3333333333333333703, 0.3333333333333335369, 0.3333333333333333703, 0.3333333333333334259, 0.3333333333333334259, 0.3333333333333334814, 0.3333333333333333703, 0.3333333333333335924, 0.3333333333333333703, 0.3333333333333334259, 0.3333333333333334814, 0.3333333333333334259, 0.3333333333333335369, 0.3333333333333333148, 0.3333333333333335369, 0.3333333333333333148, 0.3333333333333334259, 0.3333333333333333703, 0.3333333333333334259, 0.3333333333333334259, 0.3333333333333335924, 0.3333333333333333703, 0.3333333333333335924, 0.3333333333333333148, 0.3333333333333335369, 0.3333333333333335369, 0.3333333333333333148, 0.3333333333333334259, 0.3333333333333334259, 0.3333333333333334814, 0.3333333333333333703, 0.3333333333333335369, 0.3333333333333333703, 0.3333333333333333703, 0.3333333333333334814, 0.3333333333333334814, 0.3333333333333334259, 0.3333333333333333703, 0.3333333333333334814, 0.3333333333333334814, 0.3333333333333334259, 0.3333333333333334259, 0.3333333333333334259, 0.3333333333333333703, 0.3333333333333335369, 0.3333333333333333703, 0.3333333333333334259, 0.3333333333333334814, 0.3333333333333334259, 0.3333333333333334814, 0.3333333333333334259, 0.3333333333333333703, 0.3333333333333333703, 0.3333333333333334259, 0.3333333333333333148, 0.3333333333333334814, 0.3333333333333334814, 0.3333333333333334259, 0.3333333333333333703, 0.3333333333333334259, 0.3333333333333334259, 0.3333333333333333703, 0.3333333333333335369, 0.3333333333333334259, 0.3333333333333333148, 0.3333333333333333703, 0.3333333333333335369, 0.3333333333333335369, 0.3333333333333333148, 0.3333333333333335369, 0.3333333333333334259, 0.3333333333333334259, 0.3333333333333335369, 0.3333333333333333703, 0.3333333333333333703, 0.3333333333333334259, 0.3333333333333333703, 0.3333333333333334259, 0.3333333333333334259, 0.3333333333333333703, 0.3333333333333335369, 0.3333333333333333703, 0.3333333333333334259, 0.3333333333333335369, 0.3333333333333333703, 0.3333333333333333703, 0.3333333333333334814, 0.3333333333333334259, 0.3333333333333333703, 0.3333333333333335369, 0.3333333333333332593, 0.3333333333333335369, 0.3333333333333335369, 0.3333333333333333703, 0.3333333333333334814, 0.3333333333333334814, 0.3333333333333334259, 0.3333333333333333703, 0.3333333333333334259, 0.3333333333333334814, 0.3333333333333333148, 0.3333333333333335369, 0.3333333333333333703, 0.3333333333333334259, 0.3333333333333333703, 0.3333333333333334259, 0.3333333333333333148, 0.3333333333333334259, 0.3333333333333334814, 0.3333333333333333703, 0.3333333333333334814, 0.3333333333333334259, 0.3333333333333333703, 0.3333333333333334259, 0.3333333333333333703, 0.3333333333333334259, 0.3333333333333334814, 0.3333333333333332593, 0.3333333333333334259, 0.3333333333333333703, 0.3333333333333335369, 0.3333333333333334259, 0.3333333333333333703, 0.3333333333333334259, 0.3333333333333334259, 0.3333333333333333148, 0.3333333333333335369, 0.3333333333333333703, 0.3333333333333334259, 0.3333333333333335924, 0.3333333333333333703, 0.3333333333333334259, 0.3333333333333335369, 0.3333333333333333703, 0.3333333333333334259, 0.3333333333333334259, 0.3333333333333334259, 0.3333333333333333703, 0.3333333333333334259, 0.3333333333333334259, 0.3333333333333333703, 0.3333333333333333148, 0.3333333333333334814, 0.3333333333333334259, 0.3333333333333334259, 0.3333333333333333703, 0.3333333333333333703, 0.3333333333333334259, 0.3333333333333335369, 0.3333333333333333703, 0.3333333333333335369, 0.3333333333333333703, 0.3333333333333334259, 0.3333333333333335369, 0.3333333333333333148, 0.3333333333333334259, 0.3333333333333334814, 0.3333333333333335369, 0.3333333333333333148, 0.3333333333333335369, 0.3333333333333333703, 0.3333333333333334259, 0.3333333333333333703, 0.3333333333333335369, 0.3333333333333334259, 0.3333333333333334259, 0.3333333333333334259, 0.3333333333333333703, 0.3333333333333335924, 0.3333333333333334259, 0.3333333333333335369, 0.3333333333333333148, 0.3333333333333333703, 0.3333333333333334814, 0.3333333333333333703, 0.3333333333333335924, 0.3333333333333333148, 0.3333333333333333703, 0.3333333333333335369, 0.3333333333333333703, 0.3333333333333335924, 0.3333333333333332593, 0.3333333333333335924, 0.3333333333333334259, 0.3333333333333335369, 0.3333333333333334259, 0.3333333333333334814, 0.3333333333333333703, 0.3333333333333334814, 0.3333333333333333148, 0.3333333333333335369, 0.3333333333333333148, 0.3333333333333334814, 0.3333333333333334814, 0.3333333333333334814, 0.3333333333333333148, 0.3333333333333335369, 0.3333333333333333148, 0.3333333333333335369, 0.3333333333333333703, 0.3333333333333333703, 0.3333333333333335369, 0.3333333333333334259, 0.3333333333333334259, 0.3333333333333333703, 0.3333333333333335369, 0.3333333333333333148, 0.3333333333333335924, 0.3333333333333334259, 0.3333333333333334259, 0.3333333333333333703, 0.3333333333333333703, 0.3333333333333334259, 0.3333333333333334259, 0.3333333333333334259, 0.3333333333333334259, 0.3333333333333334259, 0.3333333333333334259, 0.3333333333333334259, 0.3333333333333333703, 0.3333333333333335369, 0.3333333333333333703, 0.3333333333333334814, 0.3333333333333333703, 0.3333333333333333148, 0.3333333333333337034, 0.3333333333333332038, 0.3333333333333334814, 0.3333333333333335369, 0.3333333333333334814, 0.3333333333333334259, 0.3333333333333334259, 0.3333333333333334814, 0.3333333333333333703, 0.3333333333333334814, 0.3333333333333334259, 0.3333333333333334814, 0.3333333333333333148, 0.3333333333333333703, 0.3333333333333335369, 0.3333333333333334259, 0.3333333333333333703, 0.3333333333333335369, 0.3333333333333334814, 0.3333333333333334259, 0.3333333333333333703, 0.3333333333333334259, 0.3333333333333333148, 0.3333333333333335369, 0.3333333333333333148, 0.3333333333333335369, 0.3333333333333333703, 0.3333333333333335369, 0.3333333333333334259, 0.3333333333333334814, 0.3333333333333334259, 0.3333333333333335369, 0.3333333333333334259, 0.3333333333333334259, 0.3333333333333333703, 0.3333333333333334259, 0.3333333333333333703, 0.3333333333333335369, 0.3333333333333334814, 0.3333333333333333703, 0.3333333333333333148, 0.3333333333333335369, 0.3333333333333333703, 0.3333333333333333703, 0.3333333333333334814, 0.3333333333333333148, 0.3333333333333334814, 0.3333333333333333703, 0.3333333333333334259, 0.3333333333333334814, 0.3333333333333334814, 0.3333333333333334259, 0.3333333333333334259, 0.3333333333333335369, 0.3333333333333334814, 0.3333333333333333148, 0.3333333333333335369, 0.3333333333333334259, 0.3333333333333333703, 0.3333333333333334259, 0.3333333333333334259, 0.3333333333333333148, 0.3333333333333334814, 0.3333333333333333703, 0.3333333333333334259, 0.3333333333333333148, 0.3333333333333334814, 0.3333333333333334259, 0.3333333333333333148, 0.3333333333333334814, 0.3333333333333334259, 0.3333333333333334814, 0.3333333333333332593, 0.3333333333333335924, 0.3333333333333334259, 0.3333333333333334259),
 ( 0.3333333333333334259, 0.3333333333333334259, 0.3333333333333334814, 0.3333333333333333703, 0.3333333333333335369, 0.3333333333333334259, 0.3333333333333334814, 0.3333333333333333703, 0.3333333333333334259, 0.3333333333333333703, 0.3333333333333335369, 0.3333333333333333703, 0.3333333333333334259, 0.3333333333333334259, 0.3333333333333333703, 0.3333333333333335369, 0.3333333333333333703, 0.3333333333333334259, 0.3333333333333335369, 0.3333333333333334259, 0.3333333333333333703, 0.3333333333333334259, 0.3333333333333334814, 0.3333333333333335369, 0.3333333333333333148, 0.3333333333333334259, 0.3333333333333334259, 0.3333333333333334814, 0.3333333333333334259, 0.3333333333333334259, 0.3333333333333334259, 0.3333333333333333148, 0.3333333333333335924, 0.3333333333333333148, 0.3333333333333335369, 0.3333333333333333703, 0.3333333333333335369, 0.3333333333333334259, 0.3333333333333333703, 0.3333333333333333703, 0.3333333333333335924, 0.3333333333333333148, 0.3333333333333334259, 0.3333333333333334259, 0.3333333333333335369, 0.3333333333333334814, 0.3333333333333334259, 0.3333333333333334259, 0.3333333333333334259, 0.3333333333333334259, 0.3333333333333333703, 0.3333333333333335369, 0.3333333333333334259, 0.3333333333333334259, 0.3333333333333334814, 0.3333333333333333703, 0.3333333333333333703, 0.3333333333333334814, 0.3333333333333334259, 0.3333333333333333703, 0.3333333333333334814, 0.3333333333333333703, 0.3333333333333334814, 0.3333333333333332593, 0.3333333333333335924, 0.3333333333333333148, 0.3333333333333335924, 0.3333333333333333148, 0.3333333333333335924, 0.3333333333333334259, 0.3333333333333334814, 0.3333333333333333703, 0.3333333333333333703, 0.3333333333333334814, 0.3333333333333335369, 0.3333333333333333703, 0.3333333333333334814, 0.3333333333333334259, 0.3333333333333333703, 0.3333333333333335369, 0.3333333333333333148, 0.3333333333333335369, 0.3333333333333334259, 0.3333333333333334259, 0.3333333333333333703, 0.3333333333333334259, 0.3333333333333333703, 0.3333333333333335369, 0.3333333333333333703, 0.3333333333333334259, 0.3333333333333334259, 0.3333333333333334814, 0.3333333333333333703, 0.3333333333333335924, 0.3333333333333333703, 0.3333333333333334259, 0.3333333333333334814, 0.3333333333333334259, 0.3333333333333335369, 0.3333333333333333148, 0.3333333333333335369, 0.3333333333333333148, 0.3333333333333334259, 0.3333333333333333703, 0.3333333333333334259, 0.3333333333333334259, 0.3333333333333335924, 0.3333333333333333703, 0.3333333333333335924, 0.3333333333333333148, 0.3333333333333335369, 0.3333333333333335369, 0.3333333333333333148, 0.3333333333333334259, 0.3333333333333334259, 0.3333333333333334814, 0.3333333333333333703, 0.3333333333333335369, 0.3333333333333333703, 0.3333333333333333703, 0.3333333333333334814, 0.3333333333333334814, 0.3333333333333334259, 0.3333333333333333703, 0.3333333333333334814, 0.3333333333333334814, 0.3333333333333334259, 0.3333333333333334259, 0.3333333333333334259, 0.3333333333333333703, 0.3333333333333335369, 0.3333333333333333703, 0.3333333333333334259, 0.3333333333333334814, 0.3333333333333334259, 0.3333333333333334814, 0.3333333333333334259, 0.3333333333333333703, 0.3333333333333333703, 0.3333333333333334259, 0.3333333333333333148, 0.3333333333333334814, 0.3333333333333334814, 0.3333333333333334259, 0.3333333333333333703, 0.3333333333333334259, 0.3333333333333334259, 0.3333333333333333703, 0.3333333333333335369, 0.3333333333333334259, 0.3333333333333333148, 0.3333333333333333703, 0.3333333333333335369, 0.3333333333333335369, 0.3333333333333333148, 0.3333333333333335369, 0.3333333333333334259, 0.3333333333333334259, 0.3333333333333335369, 0.3333333333333333703, 0.3333333333333333703, 0.3333333333333334259, 0.3333333333333333703, 0.3333333333333334259, 0.3333333333333334259, 0.3333333333333333703, 0.3333333333333335369, 0.3333333333333333703, 0.3333333333333334259, 0.3333333333333335369, 0.3333333333333333703, 0.3333333333333333703, 0.3333333333333334814, 0.3333333333333334259, 0.3333333333333333703, 0.3333333333333335369, 0.3333333333333332593, 0.3333333333333335369, 0.3333333333333335369, 0.3333333333333333703, 0.3333333333333334814, 0.3333333333333334814, 0.3333333333333334259, 0.3333333333333333703, 0.3333333333333334259, 0.3333333333333334814, 0.3333333333333333148, 0.3333333333333335369, 0.3333333333333333703, 0.3333333333333334259, 0.3333333333333333703, 0.3333333333333334259, 0.3333333333333333148, 0.3333333333333334259, 0.3333333333333334814, 0.3333333333333333703, 0.3333333333333334814, 0.3333333333333334259, 0.3333333333333333703, 0.3333333333333334259, 0.3333333333333333703, 0.3333333333333334259, 0.3333333333333334814, 0.3333333333333332593, 0.3333333333333334259, 0.3333333333333333703, 0.3333333333333335369, 0.3333333333333334259, 0.3333333333333333703, 0.3333333333333334259, 0.3333333333333334259, 0.3333333333333333148, 0.3333333333333335369, 0.3333333333333333703, 0.3333333333333334259, 0.3333333333333335924, 0.3333333333333333703, 0.3333333333333334259, 0.3333333333333335369, 0.3333333333333333703, 0.3333333333333334259, 0.3333333333333334259, 0.3333333333333334259, 0.3333333333333333703, 0.3333333333333334259, 0.3333333333333334259, 0.3333333333333333703, 0.3333333333333333148, 0.3333333333333334814, 0.3333333333333334259, 0.3333333333333334259, 0.3333333333333333703, 0.3333333333333333703, 0.3333333333333334259, 0.3333333333333335369, 0.3333333333333333703, 0.3333333333333335369, 0.3333333333333333703, 0.3333333333333334259, 0.3333333333333335369, 0.3333333333333333148, 0.3333333333333334259, 0.3333333333333334814, 0.3333333333333335369, 0.3333333333333333148, 0.3333333333333335369, 0.3333333333333333703, 0.3333333333333334259, 0.3333333333333333703, 0.3333333333333335369, 0.3333333333333334259, 0.3333333333333334259, 0.3333333333333334259, 0.3333333333333333703, 0.3333333333333335924, 0.3333333333333334259, 0.3333333333333335369, 0.3333333333333333148, 0.3333333333333333703, 0.3333333333333334814, 0.3333333333333333703, 0.3333333333333335924, 0.3333333333333333148, 0.3333333333333333703, 0.3333333333333335369, 0.3333333333333333703, 0.3333333333333335924, 0.3333333333333332593, 0.3333333333333335924, 0.3333333333333334259, 0.3333333333333335369, 0.3333333333333334259, 0.3333333333333334814, 0.3333333333333333703, 0.3333333333333334814, 0.3333333333333333148, 0.3333333333333335369, 0.3333333333333333148, 0.3333333333333334814, 0.3333333333333334814, 0.3333333333333334814, 0.3333333333333333148, 0.3333333333333335369, 0.3333333333333333148, 0.3333333333333335369, 0.3333333333333333703, 0.3333333333333333703, 0.3333333333333335369, 0.3333333333333334259, 0.3333333333333334259, 0.3333333333333333703, 0.3333333333333335369, 0.3333333333333333148, 0.3333333333333335924, 0.3333333333333334259, 0.3333333333333334259, 0.3333333333333333703, 0.3333333333333333703, 0.3333333333333334259, 0.3333333333333334259, 0.3333333333333334259, 0.3333333333333334259, 0.3333333333333334259, 0.3333333333333334259, 0.3333333333333334259, 0.3333333333333333703, 0.3333333333333335369, 0.3333333333333333703, 0.3333333333333334814, 0.3333333333333333703, 0.3333333333333333148, 0.3333333333333337034, 0.3333333333333332038, 0.3333333333333334814, 0.3333333333333335369, 0.3333333333333334814, 0.3333333333333334259, 0.3333333333333334259, 0.3333333333333334814, 0.3333333333333333703, 0.3333333333333334814, 0.3333333333333334259, 0.3333333333333334814, 0.3333333333333333148, 0.3333333333333333703, 0.3333333333333335369, 0.3333333333333334259, 0.3333333333333333703, 0.3333333333333335369, 0.3333333333333334814, 0.3333333333333334259, 0.3333333333333333703, 0.3333333333333334259, 0.3333333333333333148, 0.3333333333333335369, 0.3333333333333333148, 0.3333333333333335369, 0.3333333333333333703, 0.3333333333333335369, 0.3333333333333334259, 0.3333333333333334814, 0.3333333333333334259, 0.3333333333333335369, 0.3333333333333334259, 0.3333333333333334259, 0.3333333333333333703, 0.3333333333333334259, 0.3333333333333333703, 0.3333333333333335369, 0.3333333333333334814, 0.3333333333333333703, 0.3333333333333333148, 0.3333333333333335369, 0.3333333333333333703, 0.3333333333333333703, 0.3333333333333334814, 0.3333333333333333148, 0.3333333333333334814, 0.3333333333333333703, 0.3333333333333334259, 0.3333333333333334814, 0.3333333333333334814, 0.3333333333333334259, 0.3333333333333334259, 0.3333333333333335369, 0.3333333333333334814, 0.3333333333333333148, 0.3333333333333335369, 0.3333333333333334259, 0.3333333333333333703, 0.3333333333333334259, 0.3333333333333334259, 0.3333333333333333148, 0.3333333333333334814, 0.3333333333333333703, 0.3333333333333334259, 0.3333333333333333148, 0.3333333333333334814, 0.3333333333333334259, 0.3333333333333333148, 0.3333333333333334814, 0.3333333333333334259, 0.3333333333333334814, 0.3333333333333332593, 0.3333333333333335924, 0.3333333333333334259, 0.3333333333333334259),
 ( 1.000000000000000222, 1.000000000000000222, 1.000000000000000444, 1.000000000000000000, 1.000000000000000444, 1.000000000000000222, 1.000000000000000444, 0.9999999999999997780, 1.000000000000000444, 1.000000000000000000, 1.000000000000000444, 1.000000000000000000, 1.000000000000000444, 1.000000000000000222, 1.000000000000000000, 1.000000000000000666, 0.9999999999999997780, 1.000000000000000444, 1.000000000000000444, 1.000000000000000444, 1.000000000000000222, 1.000000000000000222, 1.000000000000000444, 1.000000000000000444, 1.000000000000000000, 1.000000000000000222, 1.000000000000000222, 1.000000000000000444, 1.000000000000000222, 1.000000000000000444, 1.000000000000000000, 1.000000000000000222, 1.000000000000000444, 1.000000000000000000, 1.000000000000000444, 1.000000000000000222, 1.000000000000000444, 1.000000000000000444, 1.000000000000000222, 1.000000000000000000, 1.000000000000000444, 1.000000000000000222, 1.000000000000000000, 1.000000000000000222, 1.000000000000000444, 1.000000000000000444, 1.000000000000000444, 1.000000000000000444, 1.000000000000000222, 1.000000000000000444, 1.000000000000000000, 1.000000000000000444, 1.000000000000000222, 1.000000000000000222, 1.000000000000000444, 1.000000000000000000, 1.000000000000000222, 1.000000000000000444, 1.000000000000000222, 1.000000000000000000, 1.000000000000000444, 1.000000000000000222, 1.000000000000000222, 1.000000000000000000, 1.000000000000000444, 0.9999999999999997780, 1.000000000000000444, 1.000000000000000000, 1.000000000000000444, 1.000000000000000000, 1.000000000000000444, 0.9999999999999997780, 1.000000000000000222, 1.000000000000000444, 1.000000000000000444, 1.000000000000000000, 1.000000000000000444, 1.000000000000000222, 1.000000000000000000, 1.000000000000000666, 1.000000000000000000, 1.000000000000000444, 1.000000000000000222, 1.000000000000000444, 0.9999999999999997780, 1.000000000000000444, 1.000000000000000000, 1.000000000000000444, 1.000000000000000444, 1.000000000000000222, 1.000000000000000222, 1.000000000000000444, 1.000000000000000222, 1.000000000000000444, 1.000000000000000444, 1.000000000000000222, 1.000000000000000444, 1.000000000000000222, 1.000000000000000444, 1.000000000000000000, 1.000000000000000444, 1.000000000000000000, 1.000000000000000000, 1.000000000000000444, 1.000000000000000222, 1.000000000000000222, 1.000000000000000444, 1.000000000000000000, 1.000000000000000444, 1.000000000000000000, 1.000000000000000222, 1.000000000000000444, 0.9999999999999997780, 1.000000000000000444, 1.000000000000000222, 1.000000000000000444, 1.000000000000000000, 1.000000000000000444, 1.000000000000000000, 1.000000000000000222, 1.000000000000000222, 1.000000000000000444, 1.000000000000000222, 1.000000000000000000, 1.000000000000000444, 1.000000000000000222, 1.000000000000000222, 1.000000000000000222, 1.000000000000000444, 0.9999999999999997780, 1.000000000000000666, 0.9999999999999996669, 1.000000000000000444, 1.000000000000000444, 1.000000000000000222, 1.000000000000000444, 1.000000000000000444, 1.000000000000000222, 1.000000000000000000, 1.000000000000000444, 1.000000000000000000, 1.000000000000000444, 1.000000000000000222, 1.000000000000000444, 1.000000000000000000, 1.000000000000000444, 1.000000000000000222, 1.000000000000000222, 1.000000000000000444, 1.000000000000000222, 0.9999999999999997780, 1.000000000000000444, 1.000000000000000444, 1.000000000000000444, 1.000000000000000222, 1.000000000000000444, 1.000000000000000444, 1.000000000000000222, 1.000000000000000444, 1.000000000000000000, 1.000000000000000222, 1.000000000000000444, 1.000000000000000000, 1.000000000000000222, 1.000000000000000444, 1.000000000000000000, 1.000000000000000444, 0.9999999999999997780, 1.000000000000000222, 1.000000000000000444, 1.000000000000000000, 1.000000000000000222, 1.000000000000000222, 1.000000000000000444, 1.000000000000000000, 1.000000000000000666, 0.9999999999999996669, 1.000000000000000666, 1.000000000000000222, 1.000000000000000444, 1.000000000000000222, 1.000000000000000444, 1.000000000000000222, 1.000000000000000222, 1.000000000000000000, 1.000000000000000444, 0.9999999999999997780, 1.000000000000000444, 1.000000000000000222, 1.000000000000000444, 0.9999999999999997780, 1.000000000000000444, 1.000000000000000000, 1.000000000000000222, 1.000000000000000444, 1.000000000000000000, 1.000000000000000444, 1.000000000000000444, 1.000000000000000222, 1.000000000000000222, 1.000000000000000000, 1.000000000000000444, 1.000000000000000444, 1.000000000000000000, 1.000000000000000222, 1.000000000000000222, 1.000000000000000444, 1.000000000000000222, 1.000000000000000222, 1.000000000000000444, 1.000000000000000222, 1.000000000000000000, 1.000000000000000444, 1.000000000000000000, 1.000000000000000222, 1.000000000000000444, 1.000000000000000222, 1.000000000000000222, 1.000000000000000444, 1.000000000000000000, 1.000000000000000222, 1.000000000000000222, 1.000000000000000222, 1.000000000000000000, 1.000000000000000222, 1.000000000000000222, 1.000000000000000000, 1.000000000000000222, 1.000000000000000222, 1.000000000000000444, 1.000000000000000000, 1.000000000000000000, 1.000000000000000222, 1.000000000000000000, 1.000000000000000888, 1.000000000000000000, 1.000000000000000444, 1.000000000000000222, 1.000000000000000222, 1.000000000000000444, 1.000000000000000222, 1.000000000000000222, 1.000000000000000444, 1.000000000000000444, 1.000000000000000222, 1.000000000000000444, 1.000000000000000222, 1.000000000000000000, 1.000000000000000222, 1.000000000000000444, 1.000000000000000444, 1.000000000000000222, 1.000000000000000444, 1.000000000000000222, 1.000000000000000444, 1.000000000000000222, 1.000000000000000444, 1.000000000000000222, 1.000000000000000000, 1.000000000000000444, 1.000000000000000000, 1.000000000000000666, 1.000000000000000000, 1.000000000000000000, 1.000000000000000444, 1.000000000000000222, 1.000000000000000444, 0.9999999999999997780, 1.000000000000000666, 1.000000000000000222, 1.000000000000000444, 1.000000000000000222, 1.000000000000000444, 1.000000000000000222, 1.000000000000000444, 0.9999999999999997780, 1.000000000000000666, 1.000000000000000222, 1.000000000000000222, 1.000000000000000444, 1.000000000000000444, 0.9999999999999997780, 1.000000000000000444, 1.000000000000000222, 1.000000000000000222, 1.000000000000000000, 1.000000000000000000, 1.000000000000000444, 1.000000000000000444, 1.000000000000000222, 1.000000000000000000, 1.000000000000000444, 0.9999999999999997780, 1.000000000000000444, 1.000000000000000222, 1.000000000000000000, 1.000000000000000222, 1.000000000000000000, 1.000000000000000444, 1.000000000000000000, 1.000000000000000444, 1.000000000000000222, 1.000000000000000222, 1.000000000000000222, 1.000000000000000222, 1.000000000000000222, 1.000000000000000444, 1.000000000000000222, 1.000000000000000444, 1.000000000000000222, 1.000000000000000000, 1.000000000000000888, 0.9999999999999996669, 1.000000000000000444, 1.000000000000000444, 1.000000000000000222, 1.000000000000000444, 1.000000000000000000, 1.000000000000000444, 0.9999999999999997780, 1.000000000000000444, 1.000000000000000222, 1.000000000000000444, 0.9999999999999997780, 1.000000000000000222, 1.000000000000000222, 1.000000000000000444, 1.000000000000000000, 1.000000000000000444, 1.000000000000000444, 1.000000000000000222, 1.000000000000000000, 1.000000000000000444, 1.000000000000000000, 1.000000000000000222, 1.000000000000000222, 1.000000000000000444, 1.000000000000000000, 1.000000000000000666, 1.000000000000000000, 1.000000000000000444, 1.000000000000000222, 1.000000000000000444, 1.000000000000000222, 1.000000000000000444, 1.000000000000000222, 1.000000000000000222, 1.000000000000000222, 1.000000000000000444, 1.000000000000000444, 1.000000000000000222, 1.000000000000000000, 1.000000000000000444, 1.000000000000000444, 1.000000000000000000, 1.000000000000000444, 0.9999999999999997780, 1.000000000000000444, 1.000000000000000222, 1.000000000000000222, 1.000000000000000444, 1.000000000000000222, 1.000000000000000222, 1.000000000000000444, 1.000000000000000444, 1.000000000000000444, 1.000000000000000000, 1.000000000000000444, 1.000000000000000222, 1.000000000000000222, 1.000000000000000000, 1.000000000000000444, 0.9999999999999997780, 1.000000000000000444, 1.000000000000000000, 1.000000000000000444, 1.000000000000000000, 1.000000000000000444, 1.000000000000000222, 1.000000000000000000, 1.000000000000000444, 1.000000000000000222, 1.000000000000000444, 0.9999999999999997780, 1.000000000000000444, 1.000000000000000222, 1.000000000000000222) ) ) 
 REPRESENTATION_ITEM ( '' )  SURFACE ( )  );
#57012 = EDGE_CURVE ( 'NONE', #75921, #58680, #77718, .T. ) ;
#57011 = CARTESIAN_POINT ( 'NONE',  ( 5.624284779170636739, 1.176309258369928390, -1.581782371169083712 ) ) ;
#57013 = CARTESIAN_POINT ( 'NONE',  ( 0.6823417656249882723, 1.676041667008083769, -1.181850606188749264 ) ) ;
#57015 = CARTESIAN_POINT ( 'NONE',  ( 0.3693899063928334781, -1.702925086422102163, -1.073505336752482053 ) ) ;
#57014 = AXIS2_PLACEMENT_3D ( 'NONE', #4278, #70348, #136465 ) ;
#57016 = VERTEX_POINT ( 'NONE', #115880 ) ;
#57017 = CARTESIAN_POINT ( 'NONE',  ( 6.157425464982741126, 2.025529447029483343, -0.6166105444416707382 ) ) ;
#57019 = EDGE_CURVE ( 'NONE', #14247, #159583, #41832, .T. ) ;
#57018 = SPHERICAL_SURFACE ( 'NONE', #59617, 0.08000000000000000167 ) ;
#57020 = CARTESIAN_POINT ( 'NONE',  ( 1.979048004138800998, 1.930994533390210544, 0.7472069620131777112 ) ) ;
#57021 = ORIENTED_EDGE ( 'NONE', *, *, #159108, .T. ) ;
#57022 = CARTESIAN_POINT ( 'NONE',  ( 4.044074958626150185, 7.940114228364351767, 0.7998128361456271485 ) ) ;
#57023 = CARTESIAN_POINT ( 'NONE',  ( 5.631432701629774051, 7.663367133358481631, 1.599625672291269396 ) ) ;
#57025 = CARTESIAN_POINT ( 'NONE',  ( 5.952193131599331721, 6.902979060742733708, 1.199719254218462483 ) ) ;
#57024 = CARTESIAN_POINT ( 'NONE',  ( 3.363305035154311007, 2.039577031997115597, -0.4584567826917042010 ) ) ;
#57026 = CARTESIAN_POINT ( 'NONE',  ( 5.664274315459256748, 9.830346811336296398, -0.7998128361456481317 ) ) ;
#57029 = ORIENTED_EDGE ( 'NONE', *, *, #148486, .F. ) ;
#57028 = CARTESIAN_POINT ( 'NONE',  ( 1.523755425131537278, -1.797796875034236797, 0.2216367714752715545 ) ) ;
#57027 = CARTESIAN_POINT ( 'NONE',  ( 2.151128115021032627, -1.464471472660273665, -1.089769533225225073 ) ) ;
#57030 = CARTESIAN_POINT ( 'NONE',  ( 4.987059637548557411, -0.2676712469649074055, -2.190530366034774801 ) ) ;
#57031 = CARTESIAN_POINT ( 'NONE',  ( -1.326716514427061987E-15, 2.999999999999988454, -1.225000000000003864 ) ) ;
#57032 = CARTESIAN_POINT ( 'NONE',  ( 3.839080194659278966, 0.3211572903306300075, 2.183152695405643051 ) ) ;
#57033 = CARTESIAN_POINT ( 'NONE',  ( 6.825640269476072497, 10.05066518344239412, 1.199719254218460707 ) ) ;
#57034 = CARTESIAN_POINT ( 'NONE',  ( 11.92619526913699879, 12.69999999999998153, 1.328859060402684644 ) ) ;
#57035 = CARTESIAN_POINT ( 'NONE',  ( 3.369685512061989741, 0.4621021693036463374, -1.855490417808260961 ) ) ;
#57036 = CARTESIAN_POINT ( 'NONE',  ( 9.596473800374404561, 10.09030761005864285, 0.000000000000000000 ) ) ;
#57037 = CARTESIAN_POINT ( 'NONE',  ( 5.107906530550561541, 0.6527686194882609261, -1.964817160181750788 ) ) ;
#57038 = AXIS2_PLACEMENT_3D ( 'NONE', #126600, #110339, #160083 ) ;
#57039 = DIRECTION ( 'NONE',  ( 0.000000000000000000, 0.000000000000000000, 1.000000000000000000 ) ) ;
#57040 = CARTESIAN_POINT ( 'NONE',  ( 6.356982542327763497, 0.3766756592470664744, -2.158781491689326426 ) ) ;
#57041 = CARTESIAN_POINT ( 'NONE',  ( 5.713240515264599750, 7.403118591225121392, -1.316831503761767719 ) ) ;
#57042 = ORIENTED_EDGE ( 'NONE', *, *, #214118, .T. ) ;
#57043 = CARTESIAN_POINT ( 'NONE',  ( 0.3910849555524695265, 2.914282954768474099, 2.026372354441466683 ) ) ;
#57044 = CARTESIAN_POINT ( 'NONE',  ( 3.237364818613055473, 6.998952398349030268, -1.734723475976807094E-15 ) ) ;
#57045 = CARTESIAN_POINT ( 'NONE',  ( 3.285556943750000514, -2.151041666188709733, 1.896917185911906722 ) ) ;
#57046 = CARTESIAN_POINT ( 'NONE',  ( 3.469446951953614189E-15, 0.7598076211376182387, 6.938893903907228378E-15 ) ) ;
#57047 = ADVANCED_FACE ( 'NONE', ( #116945 ), #45372, .T. ) ;
#57049 = CARTESIAN_POINT ( 'NONE',  ( -7.944714827928056167, 10.29191993738131927, 1.443375672974090751 ) ) ;
#57048 = AXIS2_PLACEMENT_3D ( 'NONE', #157325, #8917, #124896 ) ;
#57050 = CARTESIAN_POINT ( 'NONE',  ( 5.357406976055401948, 6.279338222599979424, 1.199719254218452935 ) ) ;
#57051 = CARTESIAN_POINT ( 'NONE',  ( 6.174686067066745387, 1.394736081427111030, -1.530067588329916850 ) ) ;
#57052 = CARTESIAN_POINT ( 'NONE',  ( 4.582597182753257670, -1.869065293654921023, -0.4664472792492486697 ) ) ;
#57053 = CARTESIAN_POINT ( 'NONE',  ( 1.511342449054883241, -1.897691915346022329, 0.6820157586827847451 ) ) ;
#57054 = CARTESIAN_POINT ( 'NONE',  ( -7.784352752540590004, 12.23349531127272094, 0.7998128361456481317 ) ) ;
#57055 = CARTESIAN_POINT ( 'NONE',  ( 3.410758162289653672, 6.136912401716668519, -1.199719254218453823 ) ) ;
#57056 = CARTESIAN_POINT ( 'NONE',  ( 1.271705539736139423, 1.307743536042236920, 1.758333696453084016 ) ) ;
#57057 = CARTESIAN_POINT ( 'NONE',  ( 4.986841741376339066, -0.2268417095559888130, -1.811474396668552700 ) ) ;
#57058 = AXIS2_PLACEMENT_3D ( 'NONE', #101806, #103952, #55194 ) ;
#57059 = CARTESIAN_POINT ( 'NONE',  ( 5.885648082108190238, 7.959951743916638733, 1.443375672974065660 ) ) ;
#57060 = CARTESIAN_POINT ( 'NONE',  ( 9.236128959407556849, 11.79856975744075598, -1.599625672291262513 ) ) ;
#57061 = CARTESIAN_POINT ( 'NONE',  ( -6.089547271193396227, 7.133501900260939443, -1.199719254218453823 ) ) ;
#57062 = CARTESIAN_POINT ( 'NONE',  ( 5.352771719296971042, 5.139321848801576387, 0.7998128361456341429 ) ) ;
#57063 = CARTESIAN_POINT ( 'NONE',  ( 5.174371902270911150, 6.065797303184739420, 1.199719254218452047 ) ) ;
#57064 = ORIENTED_EDGE ( 'NONE', *, *, #130804, .T. ) ;
#57066 = CARTESIAN_POINT ( 'NONE',  ( 6.011982430150495382, -0.6741147929612385514, 1.897138445369117354 ) ) ;
#57065 = CARTESIAN_POINT ( 'NONE',  ( 2.542321706073047416, -1.529623444112483632, 1.024600984555257277 ) ) ;
#57067 = CARTESIAN_POINT ( 'NONE',  ( 1.757567914286566335, -2.287329856776819881, -0.2253975434684113155 ) ) ;
#57068 = CARTESIAN_POINT ( 'NONE',  ( 6.719590461409528537, 0.3385411321301828314, -1.932175811092277096 ) ) ;
#57069 = CARTESIAN_POINT ( 'NONE',  ( -6.392833124043511894, 7.417059051927569868, 1.199719254218450271 ) ) ;
#57070 = CARTESIAN_POINT ( 'NONE',  ( -4.528121930731268563, 7.284834279576167582, -1.112404534407253953 ) ) ;
#57071 = CARTESIAN_POINT ( 'NONE',  ( -2.785310492603665367, 5.336947110424484109, 1.199719254218462483 ) ) ;
#57072 = DIRECTION ( 'NONE',  ( 1.000000000000000000, 0.000000000000000000, 0.000000000000000000 ) ) ;
#57073 = CARTESIAN_POINT ( 'NONE',  ( -3.363304624641834106, 6.081549941127532222, -1.199719254218452047 ) ) ;
#57075 = CARTESIAN_POINT ( 'NONE',  ( 1.551402291579254022, 0.5461136009352780540, -1.789155053659279071 ) ) ;
#57074 = CARTESIAN_POINT ( 'NONE',  ( 2.595357119365874432, -0.6533576199754445035, 1.986123937679643348 ) ) ;
#57076 = CARTESIAN_POINT ( 'NONE',  ( 1.845077155533506374, -1.080901620906085325, 1.701686244941137183 ) ) ;
#57077 = CARTESIAN_POINT ( 'NONE',  ( 7.944714827928043732, 10.29191993738131927, 1.443375672974076540 ) ) ;
#57078 = ORIENTED_EDGE ( 'NONE', *, *, #176104, .T. ) ;
#57079 = CARTESIAN_POINT ( 'NONE',  ( 0.6823417656249917140, 4.155208333674755394, 1.181850606188765695 ) ) ;
#57080 = CARTESIAN_POINT ( 'NONE',  ( 2.436699184107835592, -1.290689972581187339, -1.167790367532922646 ) ) ;
#57081 = CARTESIAN_POINT ( 'NONE',  ( 3.960953433486789521, 7.772862772376584850, -0.7998128361456221525 ) ) ;
#57082 = CARTESIAN_POINT ( 'NONE',  ( 0.2892308902501606327, 3.295301175517658443, -2.053744536655083941 ) ) ;
#57083 = CARTESIAN_POINT ( 'NONE',  ( 2.437784706471317175, 0.8137022719644730895, -1.520871857739027444 ) ) ;
#57084 = CARTESIAN_POINT ( 'NONE',  ( 2.472451708263478931, -2.098117355222902436, -0.6331711661175795092 ) ) ;
#57085 = CARTESIAN_POINT ( 'NONE',  ( 4.740968412965463230, 0.3751893352213676591, 2.174603215771487630 ) ) ;
#57086 = CARTESIAN_POINT ( 'NONE',  ( -9.429315115559251836, 5.003428342543706719, -6.892195246777336415 ) ) ;
#57087 = CARTESIAN_POINT ( 'NONE',  ( 2.905323041198346612, -1.807408099546173208, 1.202558989554833646 ) ) ;
#57088 = CARTESIAN_POINT ( 'NONE',  ( 1.400715809426569702, 1.493624456287694358, -1.049586478250638999 ) ) ;
#57089 = PRESENTATION_STYLE_ASSIGNMENT (( #40858 ) ) ;
#57090 = CARTESIAN_POINT ( 'NONE',  ( 4.065693644434860587, 1.385821322041587145, 1.600864752689701076 ) ) ;
#57091 = FACE_OUTER_BOUND ( 'NONE', #62858, .T. ) ;
#57092 = ORIENTED_EDGE ( 'NONE', *, *, #127934, .F. ) ;
#57094 = CARTESIAN_POINT ( 'NONE',  ( 1.364683531249988757, 1.196875000341421469, 0.000000000000000000 ) ) ;
#57093 = CARTESIAN_POINT ( 'NONE',  ( 4.423529165095542837, -1.409716928370784661, -1.807567988613969723 ) ) ;
#57095 = DIRECTION ( 'NONE',  ( 1.276756478318932585E-15, -1.000000000000000000, 1.665334536937738262E-16 ) ) ;
#57096 = CARTESIAN_POINT ( 'NONE',  ( 3.216308754939877446, 4.775446185561722956, -1.599625672291262513 ) ) ;
#57097 = CARTESIAN_POINT ( 'NONE',  ( 0.6629299983115041206, 0.6194173074674096391, 2.027988828570789437 ) ) ;
#57098 = CARTESIAN_POINT ( 'NONE',  ( -6.399085315970155285, 6.567947078161039620, -0.7216878364870278340 ) ) ;
#57099 = CARTESIAN_POINT ( 'NONE',  ( 4.202664430556254160, 5.926194473780837413, 1.443375672974062551 ) ) ;
#57100 = CARTESIAN_POINT ( 'NONE',  ( -7.185458225118419584, 7.485382138834033583, 1.040834085586084257E-14 ) ) ;
#57101 = CARTESIAN_POINT ( 'NONE',  ( 5.085717018901939390, 5.105960408239938353, 0.000000000000000000 ) ) ;
#57102 = ORIENTED_EDGE ( 'NONE', *, *, #35615, .T. ) ;
#57103 = CARTESIAN_POINT ( 'NONE',  ( 5.027970288326706338, -1.728003250605243180, 1.038991650911202713 ) ) ;
#57105 = CARTESIAN_POINT ( 'NONE',  ( 2.905193444429104321, -1.717358790072313957, 1.142030567362181559 ) ) ;
#57104 = CARTESIAN_POINT ( 'NONE',  ( 6.647575389402066826, 6.649926130590872120, 1.040834085586084257E-14 ) ) ;
#57107 = CARTESIAN_POINT ( 'NONE',  ( -0.2409995289980246258, 2.020898751655671788, -2.415740196953279462 ) ) ;
#57106 = CARTESIAN_POINT ( 'NONE',  ( 7.991605200612358573, 8.288237253661408843, 0.7998128361456281477 ) ) ;
#57108 = CARTESIAN_POINT ( 'NONE',  ( 7.526711554241970248, 8.810193563817646734, -1.199719254218452047 ) ) ;
#57109 = CARTESIAN_POINT ( 'NONE',  ( 3.285556943749998737, -2.355208332855375453, -1.896917185911906500 ) ) ;
#57110 = FILL_AREA_STYLE ('',( #153548 ) ) ;
#57111 = CARTESIAN_POINT ( 'NONE',  ( 5.701184558104195332, -0.5354452791076976803, 2.124913622581547479 ) ) ;
#57112 = CARTESIAN_POINT ( 'NONE',  ( 3.551407868487792552, -1.352154898762620849, 1.496051317864899088 ) ) ;
#57113 = CARTESIAN_POINT ( 'NONE',  ( 2.788419073117563762, 1.577926727847511312, -0.9486480243563880643 ) ) ;
#57114 = CARTESIAN_POINT ( 'NONE',  ( 6.277588818327314080, 7.282607361925381717, 1.199719254218462483 ) ) ;
#57115 = CARTESIAN_POINT ( 'NONE',  ( 6.000976577881286467, 1.490888274384492895, -1.053294804101669868 ) ) ;
#57116 = EDGE_CURVE ( 'NONE', #123335, #186645, #211251, .T. ) ;
#57117 = CARTESIAN_POINT ( 'NONE',  ( -0.03393210605391345364, -2.232032725161440023, -0.5493522527948471179 ) ) ;
#57118 = CARTESIAN_POINT ( 'NONE',  ( -5.526920175865215334, 9.599823971818089774, 0.7998128361456481317 ) ) ;
#57119 = CARTESIAN_POINT ( 'NONE',  ( 0.2985908658455891929, -2.261944659375872302, -0.05357643010404227607 ) ) ;
#57120 = CARTESIAN_POINT ( 'NONE',  ( 1.805437418371407254, 1.751699828856004837, 1.168899091633753384 ) ) ;
#57121 = CARTESIAN_POINT ( 'NONE',  ( -6.622231685632140596, 6.690634819517756959, 0.000000000000000000 ) ) ;
#57122 = CARTESIAN_POINT ( 'NONE',  ( 8.586391356156291010, 8.911878091804165791, 0.7998128361456481317 ) ) ;
#57123 = CARTESIAN_POINT ( 'NONE',  ( 6.441532379824158383, 9.568852638886589546, -1.082531754730548412 ) ) ;
#57124 =( NAMED_UNIT ( * ) PLANE_ANGLE_UNIT ( ) SI_UNIT ( $, .RADIAN. ) );
#57125 = CARTESIAN_POINT ( 'NONE',  ( -6.901263884555985051, 8.010228272525461435, 1.199719254218450271 ) ) ;
#57126 = CARTESIAN_POINT ( 'NONE',  ( 6.602457619730756733, 9.686322408785807525, 1.082531754730558626 ) ) ;
#57127 = CARTESIAN_POINT ( 'NONE',  ( 4.001130546182508851, 7.826233022050814725, 0.1222016466962717873 ) ) ;
#57128 = CARTESIAN_POINT ( 'NONE',  ( -6.247609857798938293, 6.183299677053865295, -0.7998128361456291469 ) ) ;
#57129 = CARTESIAN_POINT ( 'NONE',  ( 4.324628213192062809, -0.9515899357304625772, -2.007430035002121471 ) ) ;
#57130 = CARTESIAN_POINT ( 'NONE',  ( 2.080269975650438585, -2.149535124392497831, -0.4257020960420563882 ) ) ;
#57131 = CARTESIAN_POINT ( 'NONE',  ( 0.4697016844467936103, 0.2121168557088908557, -2.196667960996725011 ) ) ;
#57132 = CARTESIAN_POINT ( 'NONE',  ( -5.632486471834530661, 5.535932070087196344, -0.7998128361456362523 ) ) ;
#57133 = CARTESIAN_POINT ( 'NONE',  ( 4.580490334204036174, 1.208584658811951762, -1.545285769342201965 ) ) ;
#57134 = CARTESIAN_POINT ( 'NONE',  ( 10.38962578677386084, 11.01565159419135043, 0.000000000000000000 ) ) ;
#57135 = CARTESIAN_POINT ( 'NONE',  ( 0.6823417656249882723, 2.426041667008084435, -1.181850606188749264 ) ) ;
#57136 = CARTESIAN_POINT ( 'NONE',  ( 6.609999999999998543, 2.109033691136730226, 2.032371550245914094 ) ) ;
#57137 = CARTESIAN_POINT ( 'NONE',  ( -6.724481002698130538, 7.907944593645035880, -1.082531754730544860 ) ) ;
#57138 = ADVANCED_FACE ( 'NONE', ( #198122 ), #168831, .T. ) ;
#57139 = CARTESIAN_POINT ( 'NONE',  ( 3.674183785563363447, 2.104178206457421485, -0.2630699042918820396 ) ) ;
#57140 = CARTESIAN_POINT ( 'NONE',  ( -4.553559489343377287, 6.405848385690952718, -1.599625672291271394 ) ) ;
#57141 = CARTESIAN_POINT ( 'NONE',  ( 5.348557406608104969, 0.6236849695623291057, 2.069784783864880851 ) ) ;
#57142 = CARTESIAN_POINT ( 'NONE',  ( 3.649809678215182096, 0.6660801477775115664, 1.716721118343276231 ) ) ;
#57143 = UNCERTAINTY_MEASURE_WITH_UNIT (LENGTH_MEASURE( 1.000000000000000082E-05 ), #178346, 'distance_accuracy_value', 'NONE');
#57144 = CARTESIAN_POINT ( 'NONE',  ( -5.796211742468360129, 6.069872997065163922, -0.5622600474686073602 ) ) ;
#57145 = CARTESIAN_POINT ( 'NONE',  ( -0.6823417656250212460, 1.363541667008083547, 1.181850606188755259 ) ) ;
#57146 = CARTESIAN_POINT ( 'NONE',  ( 6.421804192028983671, 0.9955936683583621605, -1.427223192643598537 ) ) ;
#57147 = CARTESIAN_POINT ( 'NONE',  ( 6.827182134110161726, 7.629137130509067610, 2.310944104600751281 ) ) ;
#57148 = CARTESIAN_POINT ( 'NONE',  ( 3.050221373394638835, 6.502416002361635528, 0.000000000000000000 ) ) ;
#57149 = CARTESIAN_POINT ( 'NONE',  ( 8.868539443929959631, 12.79154120890452440, 8.085006497731432873 ) ) ;
#57150 = ADVANCED_FACE ( 'NONE', ( #85448 ), #196633, .T. ) ;
#57151 = CARTESIAN_POINT ( 'NONE',  ( 4.329101982860062314, 0.1031891237209987822, 2.159356164053369387 ) ) ;
#57152 = AXIS2_PLACEMENT_3D ( 'NONE', #14948, #36550, #34418 ) ;
#57153 = CARTESIAN_POINT ( 'NONE',  ( -4.623494077460110319, 5.352830164246910272, 1.199719254218462483 ) ) ;
#57154 = CARTESIAN_POINT ( 'NONE',  ( 5.905624997962407363, 0.3905408587613137805, 1.977747231101577352 ) ) ;
#57155 = CARTESIAN_POINT ( 'NONE',  ( -6.995644074527074707, 11.10540915368285475, 0.000000000000000000 ) ) ;
#57156 = CARTESIAN_POINT ( 'NONE',  ( 3.801785103514757846, -0.6297183656660889639, 2.067937956787009757 ) ) ;
#57157 = CARTESIAN_POINT ( 'NONE',  ( 4.938727034960622930, 0.3341968672867478007, 1.942665651468850951 ) ) ;
#57158 = CARTESIAN_POINT ( 'NONE',  ( 3.708057520534962848, -1.311595775785476148, -1.134043610401070712 ) ) ;
#57159 = CIRCLE ( 'NONE', #91819, 2.350000000000007194 ) ;
#57160 = CARTESIAN_POINT ( 'NONE',  ( 0.2928600448571066495, 1.818678932476354149, -1.222557900829209121 ) ) ;
#57161 = CARTESIAN_POINT ( 'NONE',  ( 1.273011573350724568, -1.461848840328241694, 1.785463964174689000 ) ) ;
#57162 = CARTESIAN_POINT ( 'NONE',  ( 3.638010413220875705, 0.9297346566990055683, -1.839232330223056433 ) ) ;
#57163 = CARTESIAN_POINT ( 'NONE',  ( 5.478056170419292492, -1.895640208600479326, -0.4214399443674861079 ) ) ;
#57165 = ORIENTED_EDGE ( 'NONE', *, *, #33313, .F. ) ;
#57164 = CARTESIAN_POINT ( 'NONE',  ( -7.822691444960713447, 9.189190109618056823, -1.082531754730543083 ) ) ;
#57166 = CARTESIAN_POINT ( 'NONE',  ( -5.926849427829407269, 6.943687749669614995, -1.199719254218453823 ) ) ;
#57167 = SURFACE_SIDE_STYLE ('',( #21429 ) ) ;
#57169 = ORIENTED_EDGE ( 'NONE', *, *, #75599, .F. ) ;
#57168 = CARTESIAN_POINT ( 'NONE',  ( -4.842197138736131556, 5.678260079060780008, 1.199719254218452935 ) ) ;
#57170 = CARTESIAN_POINT ( 'NONE',  ( -7.659993601596713830, 9.959745173328078849, -1.443375672974058777 ) ) ;
#57171 = CARTESIAN_POINT ( 'NONE',  ( 2.766872162265196611, -1.522532973755141850, 1.597636210702752635 ) ) ;
#57172 = CARTESIAN_POINT ( 'NONE',  ( 3.285556943749998737, -3.142708332855375986, -1.896917185911906500 ) ) ;
#57173 = ORIENTED_EDGE ( 'NONE', *, *, #135275, .F. ) ;
#57174 = CARTESIAN_POINT ( 'NONE',  ( 0.8657744530725123289, -1.852701964455932604, 0.1747518070307155780 ) ) ;
#57175 = CARTESIAN_POINT ( 'NONE',  ( -0.1291982275798625457, 7.629137130509075604, -2.673995287120598086 ) ) ;
#57176 = CARTESIAN_POINT ( 'NONE',  ( 0.7499999999999920064, 5.014583334016150751, 1.299038105676669330 ) ) ;
#57177 =( NAMED_UNIT ( * ) PLANE_ANGLE_UNIT ( ) SI_UNIT ( $, .RADIAN. ) );
#57179 = CARTESIAN_POINT ( 'NONE',  ( -4.787437654953777155, 6.678706214094487947, -1.250000000000001110 ) ) ;
#57178 = CARTESIAN_POINT ( 'NONE',  ( -7.065207446497166366, 9.336104335703744539, 0.000000000000000000 ) ) ;
#57180 = CARTESIAN_POINT ( 'NONE',  ( 6.720655732516647163, 0.005566325962592238996, 1.826293863978686982 ) ) ;
#57181 = VERTEX_POINT ( 'NONE', #24707 ) ;
#57182 = CARTESIAN_POINT ( 'NONE',  ( 2.237249138949083171, -1.841491494976960075, 0.9254197329602343869 ) ) ;
#57183 = CARTESIAN_POINT ( 'NONE',  ( -0.6801582343750125492, 1.098958333674737720, -1.178068619123855409 ) ) ;
#57184 = CARTESIAN_POINT ( 'NONE',  ( -5.747767057189642870, 8.793146435774861658, -1.199719254218440723 ) ) ;
#57185 = CARTESIAN_POINT ( 'NONE',  ( 10.91804383151480096, -9.900000000000005684, -0.1905751639681742271 ) ) ;
#57186 =( NAMED_UNIT ( * ) PLANE_ANGLE_UNIT ( ) SI_UNIT ( $, .RADIAN. ) );
#57187 = B_SPLINE_CURVE_WITH_KNOTS ( 'NONE', 3,
 ( #33694, #51021, #182062, #133369, #201501, #16360, #68306, #82438, #15299, #117143, #148528, #49952, #99770, #165836, #134437, #34750, #84580, #200440, #52086, #101900, #140839, #36886, #5428, #205786, #86713, #203634, #206851, #185262 ),
 .UNSPECIFIED., .F., .F.,
 ( 4, 2, 2, 2, 2, 2, 2, 2, 2, 2, 2, 2, 2, 4 ),
 ( 0.002695587478349080121, 0.002974090769189313352, 0.003252594060029546583, 0.003531097350869780247, 0.003809600641710013478, 0.004366607223390480373, 0.004645110514230714471, 0.004923613805070947702, 0.005202117095911182668, 0.005480620386751415031, 0.006037626968431882360, 0.006594633550112348822, 0.006873136840952582052, 0.007151640131792815283 ),
 .UNSPECIFIED. ) ;
#57188 = CARTESIAN_POINT ( 'NONE',  ( 5.118366684358879759, 5.930181538962194132, 1.199719254218462483 ) ) ;
#57189 = CARTESIAN_POINT ( 'NONE',  ( 0.6903932018771785639, -2.045263458338997253, -0.2527981509174073715 ) ) ;
#57191 = CARTESIAN_POINT ( 'NONE',  ( 4.634224865634020141, 0.3196297827482602050, 1.813140464320086132 ) ) ;
#57190 = CARTESIAN_POINT ( 'NONE',  ( 0.000000000000000000, -3.517800438942085606, 0.000000000000000000 ) ) ;
#57192 = CARTESIAN_POINT ( 'NONE',  ( 5.472687561410540802, 9.536552588287639409, 0.7998128361456462443 ) ) ;
#57193 = CARTESIAN_POINT ( 'NONE',  ( -5.224688093219839402, 7.188831756880171397, -1.599625672291271394 ) ) ;
#57195 = ORIENTED_EDGE ( 'NONE', *, *, #195841, .F. ) ;
#57194 = CARTESIAN_POINT ( 'NONE',  ( 4.010620668045937975, 3.846206254399761715, 2.500000000000000444 ) ) ;
#57196 = AXIS2_PLACEMENT_3D ( 'NONE', #61810, #30385, #197127 ) ;
#57197 = CARTESIAN_POINT ( 'NONE',  ( 4.688207069967821106, -1.042061291317699423, 1.945354640606362873 ) ) ;
#57198 = CARTESIAN_POINT ( 'NONE',  ( 0.2456851981432126020, -1.670693100197045977, -1.371219901248825535 ) ) ;
#57199 = CARTESIAN_POINT ( 'NONE',  ( -6.561783159334145132, 6.757761228752363181, -0.7216878364870278340 ) ) ;
#57200 = CARTESIAN_POINT ( 'NONE',  ( 0.2461629937395051204, 0.9812432698282257393, -1.641294572782559413 ) ) ;
#57201 = CARTESIAN_POINT ( 'NONE',  ( 0.5500180045474002410, 0.9981291480291035745, 1.752136972055001518 ) ) ;
#57202 = CARTESIAN_POINT ( 'NONE',  ( 5.994113310573177422, 10.00723293906178846, 0.000000000000000000 ) ) ;
#57203 = CARTESIAN_POINT ( 'NONE',  ( 0.000000000000000000, -0.5000000000000004441, 0.000000000000000000 ) ) ;
#57204 = CARTESIAN_POINT ( 'NONE',  ( 6.533860241792342372, -1.853627334332415888, 0.4695604596292660138 ) ) ;
#57205 = SURFACE_STYLE_USAGE ( .BOTH. , #56136 ) ;
#57206 = CARTESIAN_POINT ( 'NONE',  ( 0.3736316133628528879, 1.073300769168658908, 1.531925686032776124 ) ) ;
#57207 = CARTESIAN_POINT ( 'NONE',  ( 1.868375392651611122, -1.978555653031977446, -0.3886301775877995524 ) ) ;
#57209 = CARTESIAN_POINT ( 'NONE',  ( -4.204198463910354455, 7.819496816371283465, 0.4055711146801060929 ) ) ;
#57208 = CARTESIAN_POINT ( 'NONE',  ( 1.364683531249986537, 1.155208333674754728, -0.7879004041258239610 ) ) ;
#57211 = CARTESIAN_POINT ( 'NONE',  ( 3.774133669461790852, 1.169908569812891264, 1.751025317131530423 ) ) ;
#57210 = CARTESIAN_POINT ( 'NONE',  ( -6.991200766141138168, 11.30815132714001159, 0.7998128361456481317 ) ) ;
#57212 = CARTESIAN_POINT ( 'NONE',  ( 6.988338112840064120, 10.24047933403371502, 1.199719254218460707 ) ) ;
#57214 = CARTESIAN_POINT ( 'NONE',  ( -8.178592977541617515, 10.56477777859713463, 1.599625672291295375 ) ) ;
#57213 = CARTESIAN_POINT ( 'NONE',  ( 6.059568310664962709, 6.034194215389424798, 0.7998128361456352531 ) ) ;
#57215 = PLANE ( 'NONE',  #44401 ) ;
#57216 = CARTESIAN_POINT ( 'NONE',  ( 3.814717077619066643, -0.6377016420256261808, -1.916516432535425363 ) ) ;
#57217 = CARTESIAN_POINT ( 'NONE',  ( -1.001543065824772872E-14, 4.321875000341417916, 1.575800808251672791 ) ) ;
#57218 = VECTOR ( 'NONE', #160975, 1000.000000000000000 ) ;
#57219 = CARTESIAN_POINT ( 'NONE',  ( 9.300530189294644146, 10.91333531134101165, -1.082531754730543083 ) ) ;
#57220 = CARTESIAN_POINT ( 'NONE',  ( 4.306063477043454490, -2.156128079323017754, 0.1542669963271598166 ) ) ;
#57221 = CARTESIAN_POINT ( 'NONE',  ( 7.550965208168244125, 7.774157262476569130, -0.7998128361456341429 ) ) ;
#57222 = CARTESIAN_POINT ( 'NONE',  ( -1.364683531250014514, -0.4072916663252447167, 0.7879004041258379498 ) ) ;
#57224 = FILL_AREA_STYLE ('',( #8456 ) ) ;
#57223 = CARTESIAN_POINT ( 'NONE',  ( 5.155843554946782703, 9.237177590738404831, -0.7998128361456481317 ) ) ;
#57225 = CARTESIAN_POINT ( 'NONE',  ( 9.097157884645296733, 10.67606762258344055, -1.082531754730543083 ) ) ;
#57227 = DIRECTION ( 'NONE',  ( 1.000000000000000000, -0.000000000000000000, -0.000000000000000000 ) ) ;
#57226 = CARTESIAN_POINT ( 'NONE',  ( 1.838563082212365085, -1.162459688571298111, 1.833603174184100792 ) ) ;
#57229 = CARTESIAN_POINT ( 'NONE',  ( 1.434833617064284805, -1.334073193498284793, -1.269287082821937362 ) ) ;
#57228 = CARTESIAN_POINT ( 'NONE',  ( -5.097502569058210753, 7.930541516334467467, -1.082531754730549967 ) ) ;
#57230 = CARTESIAN_POINT ( 'NONE',  ( -1.402160292154681736E-14, 2.446875000341416584, -1.575800808251660134 ) ) ;
#57231 = CARTESIAN_POINT ( 'NONE',  ( 3.491892070630482348, -2.189115664112693871, -0.1057334378413293807 ) ) ;
#57232 = CARTESIAN_POINT ( 'NONE',  ( -11.33772463945037146, 12.69999999999998153, 3.599999999999999201 ) ) ;
#57233 = CARTESIAN_POINT ( 'NONE',  ( 3.678848304420906601, -2.179822953419420006, -0.6058417560294343529 ) ) ;
#57234 = CARTESIAN_POINT ( 'NONE',  ( -8.030507057996002729, 8.263346410617135263, 1.040834085586084257E-14 ) ) ;
#57235 = B_SPLINE_CURVE_WITH_KNOTS ( 'NONE', 3,
 ( #57284, #204568, #107159, #88730, #172106, #74600, #23699 ),
 .UNSPECIFIED., .F., .F.,
 ( 4, 3, 4 ),
 ( 0.000000000000000000, 3.303441823992926441E-05, 4.225144977697881029E-05 ),
 .UNSPECIFIED. ) ;
#57236 = CARTESIAN_POINT ( 'NONE',  ( -1.364683531250012516, 5.051041667008085767, -0.7879004041258300672 ) ) ;
#57237 = CARTESIAN_POINT ( 'NONE',  ( 6.348661983278831578, 6.841051910588018536, 0.6299351563821649069 ) ) ;
#57238 = CARTESIAN_POINT ( 'NONE',  ( 1.499999999999993117, 14.10416666666666607, 0.8660254037844409281 ) ) ;
#57239 = CARTESIAN_POINT ( 'NONE',  ( 4.895902868310594513, 8.725987423088758632, 0.000000000000000000 ) ) ;
#57240 = CARTESIAN_POINT ( 'NONE',  ( 5.325387591137793919, -1.680293062798293713, 0.5557786991975487423 ) ) ;
#57241 = CARTESIAN_POINT ( 'NONE',  ( 9.121938423896107651, 9.536683004167278099, -0.7998128361456221525 ) ) ;
#57242 = CARTESIAN_POINT ( 'NONE',  ( 1.553890309278640025, 0.6119248022173563450, -2.015079113363055452 ) ) ;
#57244 = CARTESIAN_POINT ( 'NONE',  ( 1.499999999999987121, 1.004166666666687968, 0.8660254037844524744 ) ) ;
#57243 = CARTESIAN_POINT ( 'NONE',  ( -1.364683531250010295, 10.63020833367473195, 0.7879004041258445001 ) ) ;
#57245 = CARTESIAN_POINT ( 'NONE',  ( 1.064831551406957511, 1.493571888342230203, -1.284017422347245807 ) ) ;
#57246 = DIRECTION ( 'NONE',  ( 1.779758311459929505E-16, 0.000000000000000000, -1.000000000000000000 ) ) ;
#57247 = CARTESIAN_POINT ( 'NONE',  ( -1.201851678989727383E-14, 5.368750000682816825, -1.732050807568863648 ) ) ;
#57249 = ORIENTED_EDGE ( 'NONE', *, *, #144373, .T. ) ;
#57248 = CARTESIAN_POINT ( 'NONE',  ( 5.783446960131396253, 0.1242560548703756929, -1.807377920737750499 ) ) ;
#57250 = CARTESIAN_POINT ( 'NONE',  ( 8.283668668269706714, 8.766627655843892697, 1.040834085586084257E-14 ) ) ;
#57251 = CARTESIAN_POINT ( 'NONE',  ( 8.992082194361556091, 11.51384853155376220, 1.599625672291279388 ) ) ;
#57252 = CARTESIAN_POINT ( 'NONE',  ( 4.698043743269282757, -1.870269067358639958, -0.04562963166049315705 ) ) ;
#57253 = CARTESIAN_POINT ( 'NONE',  ( 4.566398809704347528, 4.221886787610169556, -0.7998128361456211532 ) ) ;
#57254 = ORIENTED_EDGE ( 'NONE', *, *, #64428, .F. ) ;
#57255 = CARTESIAN_POINT ( 'NONE',  ( 4.698136132249701724, 0.8899761679339033282, -1.869364561350304488 ) ) ;
#57256 = CARTESIAN_POINT ( 'NONE',  ( -3.755786496842897795E-14, 1.937500000000033085, -1.414508159514593411 ) ) ;
#57257 = CARTESIAN_POINT ( 'NONE',  ( -3.973948422136968084, 7.650373902552835226, -0.7216878364870458196 ) ) ;
#57258 = FILL_AREA_STYLE ('',( #24739 ) ) ;
#57259 = CARTESIAN_POINT ( 'NONE',  ( 9.240045382913317340, 10.73880668727576015, -1.199719254218446718 ) ) ;
#57260 = CARTESIAN_POINT ( 'NONE',  ( -8.967828540435322182, 12.54988483289483980, 1.199719254218462483 ) ) ;
#57261 = CARTESIAN_POINT ( 'NONE',  ( 6.749980374757213575, 8.968339418673846097, 1.599625672291268286 ) ) ;
#57262 = DIRECTION ( 'NONE',  ( 0.7592566023653005702, -0.6507913734559639396, 0.000000000000000000 ) ) ;
#57263 = CARTESIAN_POINT ( 'NONE',  ( -0.6823417656250003738, -0.03229166632524871350, -1.181850606188749264 ) ) ;
#57264 = CARTESIAN_POINT ( 'NONE',  ( -1.500000000000013101, 0.6708333333333583726, 0.8660254037844403729 ) ) ;
#57265 = CARTESIAN_POINT ( 'NONE',  ( 4.000408739481801312, 1.952204270133122810, 0.1946113827649766925 ) ) ;
#57266 = CARTESIAN_POINT ( 'NONE',  ( 1.985703663612121472, 1.880146017696176619, 0.7282698753105636413 ) ) ;
#57267 = CARTESIAN_POINT ( 'NONE',  ( -1.284279953904132077, 2.909610286488902187, -0.7749999999999936939 ) ) ;
#57268 = CARTESIAN_POINT ( 'NONE',  ( 7.719547554928809951, -5.360178282914182191, 7.836475020641952227 ) ) ;
#57269 = CARTESIAN_POINT ( 'NONE',  ( 11.84668730067608244, 10.19999999999999929, -1.320000000000001616 ) ) ;
#57270 = CARTESIAN_POINT ( 'NONE',  ( 1.879943753831798015, -1.004885234286160722, 1.577526331995420472 ) ) ;
#57271 = CARTESIAN_POINT ( 'NONE',  ( 1.364683531249988535, 5.405208333674750953, -0.7879004041258300672 ) ) ;
#57272 = CARTESIAN_POINT ( 'NONE',  ( 4.588143835816930860, 1.162566388618992308, 1.643413508355499708 ) ) ;
#57273 = CARTESIAN_POINT ( 'NONE',  ( -8.483651433849100698, 10.92067931095586886, 1.599625672291269396 ) ) ;
#57275 = CARTESIAN_POINT ( 'NONE',  ( 2.882529129721671080, -0.6171794022716176054, -2.025259201532733755 ) ) ;
#57274 = CARTESIAN_POINT ( 'NONE',  ( -5.910991785878183080, 5.998504626387068051, -0.7216878364870278340 ) ) ;
#57277 = EDGE_CURVE ( 'NONE', #94066, #46791, #204508, .T. ) ;
#57276 = CYLINDRICAL_SURFACE ( 'NONE', #52658, 0.08000000000000020983 ) ;
#57278 = CARTESIAN_POINT ( 'NONE',  ( 4.527825515032589898, 2.008996319933327612, -0.4998958796476050681 ) ) ;
#57279 = CARTESIAN_POINT ( 'NONE',  ( 7.340813827156391191, 7.528980651296110160, 0.7998128361456281477 ) ) ;
#57280 = CARTESIAN_POINT ( 'NONE',  ( 0.1520488688747126949, 0.8040222321012976403, 1.930173718738151578 ) ) ;
#57282 = ORIENTED_EDGE ( 'NONE', *, *, #104201, .F. ) ;
#57281 = CARTESIAN_POINT ( 'NONE',  ( 6.387720234973090605, 1.261301916940280154, 1.320039730931761524 ) ) ;
#57283 = CARTESIAN_POINT ( 'NONE',  ( 7.944187942603509356, 11.35563746875774882, 1.199719254218460707 ) ) ;
#57284 = CARTESIAN_POINT ( 'NONE',  ( 1.734723475976807094E-15, 14.57349900225068495, 11.91973154060107376 ) ) ;
#57285 = CARTESIAN_POINT ( 'NONE',  ( -10.82994025801865590, 5.589394046361075397, 6.507174183487985708 ) ) ;
#57286 = CARTESIAN_POINT ( 'NONE',  ( 8.392133896734671694, 8.893170422386358354, 0.7216878364870458196 ) ) ;
#57287 = CARTESIAN_POINT ( 'NONE',  ( 1.364683531249997417, 12.54687500034139980, 2.602085213965210642E-15 ) ) ;
#57288 = CARTESIAN_POINT ( 'NONE',  ( 6.041656841763191288, -1.799011877964010520, 0.6487133288125003228 ) ) ;
#57289 = CARTESIAN_POINT ( 'NONE',  ( -7.797910906154257304, 12.24931315715533486, 0.000000000000000000 ) ) ;
#57290 = CARTESIAN_POINT ( 'NONE',  ( 6.328958779480917229, 6.278206752349526631, 0.7998128361456341429 ) ) ;
#57291 = CARTESIAN_POINT ( 'NONE',  ( 2.358755538653318773, 5.695705861830088423, 1.040834085586084257E-14 ) ) ;
#57292 = CARTESIAN_POINT ( 'NONE',  ( -0.4019237886466933696, 12.33258545099817205, 1.500000000000005995 ) ) ;
#57293 = CARTESIAN_POINT ( 'NONE',  ( 2.822068529938852155, 6.444163718237301275, -0.7998128361456291469 ) ) ;
#57294 = ORIENTED_EDGE ( 'NONE', *, *, #25109, .F. ) ;
#57295 = CARTESIAN_POINT ( 'NONE',  ( -5.749539660647037032, 8.865490816466966351, 1.199719254218454489 ) ) ;
#57296 = CARTESIAN_POINT ( 'NONE',  ( 5.413685477598253470, -1.281375732037979942, -1.556898226837098331 ) ) ;
#57297 = DIRECTION ( 'NONE',  ( 0.6483454320283799088, 0.000000000000000000, -0.7613463080411786432 ) ) ;
#57298 = CIRCLE ( 'NONE', #84966, 0.1000000000000000472 ) ;
#57299 = CARTESIAN_POINT ( 'NONE',  ( -6.773846765307970585, -7.473374494058216300, 6.773846765307992790 ) ) ;
#57300 = CARTESIAN_POINT ( 'NONE',  ( -0.1405533004718494683, 4.096626656942652822, -2.275097870671268563 ) ) ;
#57301 = EDGE_CURVE ( 'NONE', #80420, #112800, #55093, .T. ) ;
#57302 = CARTESIAN_POINT ( 'NONE',  ( -6.100805936469506641, 6.219954468743612352, 0.7216878364870317197 ) ) ;
#57303 = CARTESIAN_POINT ( 'NONE',  ( 3.979481780810941949, 4.601482484822914998, 1.199719254218464037 ) ) ;
#57304 = CARTESIAN_POINT ( 'NONE',  ( 2.799605281554286229, -1.456005023894543893, -1.326338995474019011 ) ) ;
#57305 = CARTESIAN_POINT ( 'NONE',  ( 3.972279928656559100, -1.994873972748755442, -0.2930500606010341125 ) ) ;
#57306 = CARTESIAN_POINT ( 'NONE',  ( -5.831978632172702071, 9.955725504176825780, 0.7998128361456481317 ) ) ;
#57307 = CARTESIAN_POINT ( 'NONE',  ( 6.727182134110178069, 2.947419669445831669, 2.641212418657997496 ) ) ;
#57308 = CARTESIAN_POINT ( 'NONE',  ( 5.208995777154565410, -0.3238732214236837992, 2.167259527466679270 ) ) ;
#57309 = CARTESIAN_POINT ( 'NONE',  ( 3.135679483595578798, -1.292546426170533058, -1.428565414989799054 ) ) ;
#57310 = CARTESIAN_POINT ( 'NONE',  ( -9.508345801885592863, 9.987491611821676329, 0.7998128361456462443 ) ) ;
#57311 = SURFACE_STYLE_USAGE ( .BOTH. , #175343 ) ;
#57312 = CARTESIAN_POINT ( 'NONE',  ( -1.500000000000039524, 6.999999999999999112, -10.89724735885167739 ) ) ;
#57313 = CARTESIAN_POINT ( 'NONE',  ( 0.07556134207193675179, -0.004209888911949481380, -2.244269416743961187 ) ) ;
#57314 = CARTESIAN_POINT ( 'NONE',  ( -1.364683531250014514, 13.08854166700806410, -0.7879004041258335089 ) ) ;
#57315 = CARTESIAN_POINT ( 'NONE',  ( 4.299907273828439180, 8.168308919441841454, 1.040834085586084257E-14 ) ) ;
#57316 = CARTESIAN_POINT ( 'NONE',  ( -7.055228938193937260, -8.176568542494910830, 6.396834479292722975 ) ) ;
#57317 = CARTESIAN_POINT ( 'NONE',  ( 5.899206235721897507, 6.055031161196562373, 0.000000000000000000 ) ) ;
#57319 = CARTESIAN_POINT ( 'NONE',  ( 2.965492324039080252, -1.647071928310759326, -1.157207142784054010 ) ) ;
#57318 = CARTESIAN_POINT ( 'NONE',  ( 6.269096963164666469, 1.759884223096353173, -0.5412972069449849544 ) ) ;
#57320 = CARTESIAN_POINT ( 'NONE',  ( 5.624470717464387093, 0.4563550445067353079, -2.252502686463413006 ) ) ;
#57322 = CARTESIAN_POINT ( 'NONE',  ( 3.274093294390582276, -0.9130387472845059582, -1.621452132119176159 ) ) ;
#57321 = PRESENTATION_STYLE_ASSIGNMENT (( #120263 ) ) ;
#57323 = CARTESIAN_POINT ( 'NONE',  ( 6.502017186205484300, 9.743381262951846367, -1.199719254218452047 ) ) ;
#57324 = CARTESIAN_POINT ( 'NONE',  ( 11.97929049433705373, 11.37999999999999901, -0.7046979865771834106 ) ) ;
#57325 = LINE ( 'NONE', #24807, #209622 ) ;
#57326 = CARTESIAN_POINT ( 'NONE',  ( -6.612626235163205024, 8.737816579155630592, -1.599625672291263179 ) ) ;
#57327 = CARTESIAN_POINT ( 'NONE',  ( -4.340018570150309785, 7.117086527600392287, -1.082531754730551743 ) ) ;
#57328 = CARTESIAN_POINT ( 'NONE',  ( 5.917543283689063571, -1.162172991910553010, -1.737764066907695915 ) ) ;
#57329 = CARTESIAN_POINT ( 'NONE',  ( 6.005898861173831094, 6.109229547565340646, 1.040834085586084257E-14 ) ) ;
#57330 = ORIENTED_EDGE ( 'NONE', *, *, #62930, .T. ) ;
#57331 = CARTESIAN_POINT ( 'NONE',  ( 9.367496997597598352, 3.481540744127370690, 7.500000000000000000 ) ) ;
#57333 = CARTESIAN_POINT ( 'NONE',  ( 3.167801447087334576, 6.847518788243868393, -0.7998128361456291469 ) ) ;
#57332 = CARTESIAN_POINT ( 'NONE',  ( 4.728284716797250375, 8.273450856974118750, 0.7059987189090509707 ) ) ;
#57334 = CARTESIAN_POINT ( 'NONE',  ( 6.252575197229738535, 0.5485693247098271108, 1.635415954441843844 ) ) ;
#57335 = CARTESIAN_POINT ( 'NONE',  ( -4.225337428953291230, 8.081310767087481750, 0.7998128361456341429 ) ) ;
#57336 = CARTESIAN_POINT ( 'NONE',  ( 1.599856272741075447, -0.2119130288822292651, 1.721036989116639493 ) ) ;
#57337 = CARTESIAN_POINT ( 'NONE',  ( -7.788094311009213122, 14.55185938206740026, 9.081607124763383609 ) ) ;
#57338 = DIRECTION ( 'NONE',  ( 0.000000000000000000, 0.000000000000000000, 1.000000000000000000 ) ) ;
#57339 = CIRCLE ( 'NONE', #178422, 0.2000000000000005107 ) ;
#57340 = CARTESIAN_POINT ( 'NONE',  ( 0.08058608058606736568, -5.770897281092849163, -10.99970480893079738 ) ) ;
#57341 = CARTESIAN_POINT ( 'NONE',  ( 6.772352023501587936, -1.015705593385501482, -1.918810339808636023 ) ) ;
#57342 = CARTESIAN_POINT ( 'NONE',  ( 5.303274670167754223, 1.494737065598227943, 1.048009559513597866 ) ) ;
#57343 = CARTESIAN_POINT ( 'NONE',  ( 2.096468001391890823, 1.939661435718213811, 0.2929505381348077031 ) ) ;
#57344 = FACE_OUTER_BOUND ( 'NONE', #39448, .T. ) ;
#57345 = CARTESIAN_POINT ( 'NONE',  ( 6.100279051144945619, 9.204410428722734849, -1.199719254218440723 ) ) ;
#57346 = CARTESIAN_POINT ( 'NONE',  ( 3.686284471605893120, 1.179319764668992576, 1.762089746328721507 ) ) ;
#57347 = LINE ( 'NONE', #107228, #34321 ) ;
#57348 = LINE ( 'NONE', #76780, #198151 ) ;
#57349 =( GEOMETRIC_REPRESENTATION_CONTEXT ( 3 ) GLOBAL_UNCERTAINTY_ASSIGNED_CONTEXT ( ( #106179 ) ) GLOBAL_UNIT_ASSIGNED_CONTEXT ( ( #134317, #51975, #114900 ) ) REPRESENTATION_CONTEXT ( 'NONE', 'WORKASPACE' ) );
#57350 = CARTESIAN_POINT ( 'NONE',  ( -4.379705010876359772, 7.173806194452361673, -1.050513582990858064 ) ) ;
#57351 = CARTESIAN_POINT ( 'NONE',  ( 2.325130699016836555, -1.891071737562114219, -0.8429460452448679364 ) ) ;
#57353 = CARTESIAN_POINT ( 'NONE',  ( 1.364683531249986981, -1.053124999658580752, 0.000000000000000000 ) ) ;
#57352 = DIRECTION ( 'NONE',  ( -5.578564026256490882E-16, -1.000000000000000000, -9.066213480720158442E-32 ) ) ;
#57355 = VERTEX_POINT ( 'NONE', #56157 ) ;
#57354 = CARTESIAN_POINT ( 'NONE',  ( 3.950012332353939559, -1.532167235135332373, -1.608510083909537869 ) ) ;
#57356 = CARTESIAN_POINT ( 'NONE',  ( 1.477568294945711180, -2.288151160537778672, -0.2198310841375460678 ) ) ;
#57358 = CARTESIAN_POINT ( 'NONE',  ( 0.3737810522974581717, -1.925036204310347943, 0.3769080146646397456 ) ) ;
#57357 = CARTESIAN_POINT ( 'NONE',  ( 9.463228032658635769, 11.10314946193233965, -1.082531754730543083 ) ) ;
#57360 = CARTESIAN_POINT ( 'NONE',  ( 3.475000000000000533, -0.1750000000000015432, 0.000000000000000000 ) ) ;
#57359 = CARTESIAN_POINT ( 'NONE',  ( 5.239300017038202917, 5.077214539491492928, 0.000000000000000000 ) ) ;
#57361 = CYLINDRICAL_SURFACE ( 'NONE', #113249, 2.000000000000000000 ) ;
#57362 = CARTESIAN_POINT ( 'NONE',  ( -10.96785329849812562, -5.223431457505089526, 0.4373225248172959434 ) ) ;
#57364 = PLANE ( 'NONE',  #18266 ) ;
#57363 = VECTOR ( 'NONE', #121652, 1000.000000000000000 ) ;
#57365 = CARTESIAN_POINT ( 'NONE',  ( -0.2102771530458277249, 4.081134801423261571, -2.758393064927369576 ) ) ;
#57366 = CARTESIAN_POINT ( 'NONE',  ( 2.942113945249478668, 1.711507881387188013, 0.2129122850730424121 ) ) ;
#57367 = CARTESIAN_POINT ( 'NONE',  ( 1.850796360583713884, -1.845628094615419768, -0.8128149310912060610 ) ) ;
#57368 = CARTESIAN_POINT ( 'NONE',  ( 3.567884397833466892, 2.208229897964437249, -0.4915367949662046154 ) ) ;
#57369 = CARTESIAN_POINT ( 'NONE',  ( 5.285806214103678791, 1.413684203821091945, 1.561263235811745309 ) ) ;
#57370 = CARTESIAN_POINT ( 'NONE',  ( -7.160114521792834807, 8.486460042580672436, 1.082531754730549078 ) ) ;
#57371 = CARTESIAN_POINT ( 'NONE',  ( 3.532247091833766284, 1.725908789131404220, 0.3905704408769093416 ) ) ;
#57373 = CARTESIAN_POINT ( 'NONE',  ( 6.321853416579415352, 1.323700039822506280, -1.871417125626378075 ) ) ;
#57372 = CARTESIAN_POINT ( 'NONE',  ( 5.664274315459256748, 9.830346811336296398, -0.7998128361456481317 ) ) ;
#57374 = CARTESIAN_POINT ( 'NONE',  ( 5.507694354943953208, -0.8313836724207699369, -1.642813217252625524 ) ) ;
#57375 = CARTESIAN_POINT ( 'NONE',  ( -4.111146893441842920, 5.819424013814012753, 1.599625672291267398 ) ) ;
#57376 = CARTESIAN_POINT ( 'NONE',  ( 5.630878078874809844, -1.982435003639994031, 0.9343296635366815650 ) ) ;
#57377 = CARTESIAN_POINT ( 'NONE',  ( -3.110706179331648169, 5.716575411607132118, 1.199719254218462483 ) ) ;
#57378 = CARTESIAN_POINT ( 'NONE',  ( -9.512045263456270661, -8.176568542494905500, 0.4655551865852137206 ) ) ;
#57379 = CARTESIAN_POINT ( 'NONE',  ( 5.740704066448026666, -2.019076491677873619, -0.4572469816465085657 ) ) ;
#57380 = CARTESIAN_POINT ( 'NONE',  ( 0.02267320670834571672, 0.3494893071277604402, 1.985867805234131644 ) ) ;
#57381 = CARTESIAN_POINT ( 'NONE',  ( -1.500000000000015099, -0.7979166659838445863, 0.8660254037844403729 ) ) ;
#57382 = CARTESIAN_POINT ( 'NONE',  ( 4.529859951405730278, -1.186268397688082343, -1.517871513682719886 ) ) ;
#57383 = CARTESIAN_POINT ( 'NONE',  ( 1.364683531249997417, 9.734375000341396245, 2.602085213965210642E-15 ) ) ;
#57384 = DIRECTION ( 'NONE',  ( 0.9120491373041519356, 0.000000000000000000, -0.4100809324301145642 ) ) ;
#57385 = CARTESIAN_POINT ( 'NONE',  ( 1.248599636731639428, 1.089134306475655789, -1.936006665247846481 ) ) ;
#57387 = ORIENTED_EDGE ( 'NONE', *, *, #209784, .T. ) ;
#57386 = CARTESIAN_POINT ( 'NONE',  ( 4.523580528814945545, 5.306540700819438960, 1.199719254218452047 ) ) ;
#57389 = CARTESIAN_POINT ( 'NONE',  ( 0.000000000000000000, -9.900000000000005684, 10.91970695577495931 ) ) ;
#57388 = CARTESIAN_POINT ( 'NONE',  ( -5.167065940583949413, 5.200867483535597913, 0.000000000000000000 ) ) ;
#57390 = CARTESIAN_POINT ( 'NONE',  ( 4.729096653068339151, 4.411700938201493116, -0.7998128361456211532 ) ) ;
#57391 = DIRECTION ( 'NONE',  ( 2.949029909160572061E-17, 1.000000000000000000, -8.673600428462616880E-15 ) ) ;
#57392 = CARTESIAN_POINT ( 'NONE',  ( 11.75674451658838393, 7.888068978623318017, 2.183490823870577024 ) ) ;
#57393 = CARTESIAN_POINT ( 'NONE',  ( 10.35806617071623315, 11.18675807536486566, 0.000000000000000000 ) ) ;
#57394 = CARTESIAN_POINT ( 'NONE',  ( 1.504273306027693602, 1.959471947749168663, 0.09963418240711149898 ) ) ;
#57395 = CARTESIAN_POINT ( 'NONE',  ( -1.364683531250012516, 1.342708333674755616, 0.7879004041258379498 ) ) ;
#57396 = EDGE_CURVE ( 'NONE', #94342, #54853, #149845, .T. ) ;
#57397 = CARTESIAN_POINT ( 'NONE',  ( -0.7500000000000215383, 3.691666666666690411, 1.299038105676671107 ) ) ;
#57398 = CARTESIAN_POINT ( 'NONE',  ( 0.4146024514614836676, 0.7878568475925759040, 1.906473239439598677 ) ) ;
#57399 = CARTESIAN_POINT ( 'NONE',  ( -7.296259222448620463, 11.66405285949874759, 0.7998128361456481317 ) ) ;
#57400 = CARTESIAN_POINT ( 'NONE',  ( -4.406036734316882253, 8.084200590104265061, -0.7216878364870257245 ) ) ;
#57401 = CARTESIAN_POINT ( 'NONE',  ( 0.6028508490328026159, -0.7652319425662640340, -2.129318446015377120 ) ) ;
#57403 = ORIENTED_EDGE ( 'NONE', *, *, #213637, .F. ) ;
#57402 = CARTESIAN_POINT ( 'NONE',  ( -6.878064000834399394, 6.918829510595249310, -0.7998128361456291469 ) ) ;
#57404 = CARTESIAN_POINT ( 'NONE',  ( 0.7499999999999885647, -0.9854166659838472508, 1.299038105676657340 ) ) ;
#57405 = CARTESIAN_POINT ( 'NONE',  ( 1.915107840602244593, -0.2339084544023955492, 1.855816807740391150 ) ) ;
#57406 = CARTESIAN_POINT ( 'NONE',  ( 0.2637851986186890429, 1.619078963417280859, -0.6216347861247341067 ) ) ;
#57408 = CARTESIAN_POINT ( 'NONE',  ( 3.896163805485418852, -0.6886730243073329039, -2.080591098665984795 ) ) ;
#57407 = CARTESIAN_POINT ( 'NONE',  ( -0.6801582343750004478, 2.348958333674739052, -1.178068619123869398 ) ) ;
#57409 = CARTESIAN_POINT ( 'NONE',  ( 4.823409937486792032, -0.1187154998047341425, 2.304658580708033533 ) ) ;
#57410 = B_SPLINE_CURVE_WITH_KNOTS ( 'NONE', 3,
 ( #92220, #140981, #13050, #10914 ),
 .UNSPECIFIED., .F., .F.,
 ( 4, 4 ),
 ( 4.159586391574946371E-16, 0.0002852080176109775202 ),
 .UNSPECIFIED. ) ;
#57411 = CARTESIAN_POINT ( 'NONE',  ( 0.08096513915848214948, -0.1534363407719694927, -2.027498111301667905 ) ) ;
#57412 = CARTESIAN_POINT ( 'NONE',  ( 2.660020691486902233, -1.338829530657672073, 1.406886975181226296 ) ) ;
#57413 = CARTESIAN_POINT ( 'NONE',  ( -6.033015167956818026, 6.140865238812146742, -0.7216878364870267237 ) ) ;
#57414 = PRODUCT_DEFINITION_SHAPE ( 'NONE', 'NONE',  #90511 ) ;
#57415 = ADVANCED_FACE ( 'NONE', ( #189352 ), #180179, .T. ) ;
#57416 =( LENGTH_UNIT ( ) NAMED_UNIT ( * ) SI_UNIT ( .MILLI., .METRE. ) );
#57417 = CARTESIAN_POINT ( 'NONE',  ( 5.273731010124149243, 0.4114677744767555878, -2.080124947408354963 ) ) ;
#57418 = DIRECTION ( 'NONE',  ( 0.000000000000000000, -1.000000000000000000, 0.000000000000000000 ) ) ;
#57419 = CARTESIAN_POINT ( 'NONE',  ( 3.867814693791224112, -0.2004342644464084944, -2.006446243107910199 ) ) ;
#57420 = CARTESIAN_POINT ( 'NONE',  ( -4.650083499362882122, 6.448183387388563226, 1.443375672974064550 ) ) ;
#57421 = CARTESIAN_POINT ( 'NONE',  ( -7.795011973214244883, 8.058878488363559356, 0.7998128361456341429 ) ) ;
#57422 = CARTESIAN_POINT ( 'NONE',  ( 8.062294901620731480, 12.55776115186623620, 1.040834085586084257E-14 ) ) ;
#57423 = CARTESIAN_POINT ( 'NONE',  ( 0.5217476098421744979, -0.9739702522407606144, -1.544006022310390192 ) ) ;
#57424 = CARTESIAN_POINT ( 'NONE',  ( -6.608673532018475960, 6.674816973635147477, -0.7998128361456362523 ) ) ;
#57425 = CARTESIAN_POINT ( 'NONE',  ( -0.05083690440159556456, 15.48930801145573533, 11.99422659986762163 ) ) ;
#57426 = CARTESIAN_POINT ( 'NONE',  ( -10.81685113641997020, 3.157239479008171035, 6.648618798508739935 ) ) ;
#57427 = ORIENTED_EDGE ( 'NONE', *, *, #172633, .F. ) ;
#57428 = CARTESIAN_POINT ( 'NONE',  ( 5.840714686760185792, 0.3996242267790580116, 2.021590886677153254 ) ) ;
#57429 = B_SPLINE_CURVE_WITH_KNOTS ( 'NONE', 3,
 ( #54867, #135068, #198946, #116714, #18067, #104695, #70011 ),
 .UNSPECIFIED., .F., .F.,
 ( 4, 3, 4 ),
 ( 3.314949680324280829E-05, 0.0009000000012044579497, 0.001958074173707490418 ),
 .UNSPECIFIED. ) ;
#57430 = CARTESIAN_POINT ( 'NONE',  ( -6.333067150914850174, 8.481940657524365434, 1.443375672974064550 ) ) ;
#57431 = CARTESIAN_POINT ( 'NONE',  ( 7.363486825553451354, 8.723727730301414240, -1.082531754730548412 ) ) ;
#57432 = CARTESIAN_POINT ( 'NONE',  ( -4.603156847039612920, 5.329103395422994716, 1.199719254218462483 ) ) ;
#57433 = CARTESIAN_POINT ( 'NONE',  ( -8.839026081105473054, 12.39961529701003684, -1.199719254218446718 ) ) ;
#57434 = CARTESIAN_POINT ( 'NONE',  ( 4.020179312760450152, -2.014129041962478883, 0.1506293649766801690 ) ) ;
#57436 = ORIENTED_EDGE ( 'NONE', *, *, #692, .T. ) ;
#57435 = CARTESIAN_POINT ( 'NONE',  ( 5.303485788544977098, 1.959706058537356910, -1.045853978123905570 ) ) ;
#57438 = CARTESIAN_POINT ( 'NONE',  ( 7.076992996653421741, 10.23994701519558781, -1.082531754730537976 ) ) ;
#57437 = CARTESIAN_POINT ( 'NONE',  ( -7.587723245503481095, 8.881373870289390737, 1.199719254218452047 ) ) ;
#57439 = CARTESIAN_POINT ( 'NONE',  ( 6.494519276145969577, 7.535692896047149425, -1.199719254218446718 ) ) ;
#57440 = CARTESIAN_POINT ( 'NONE',  ( 4.698151523293167209, -2.060395484190484794, -0.05257267949314303745 ) ) ;
#57441 = CARTESIAN_POINT ( 'NONE',  ( 3.990861413484114273, -2.010826503599131065, 0.1511389102963680842 ) ) ;
#57442 = VERTEX_POINT ( 'NONE', #39917 ) ;
#57443 =( BOUNDED_SURFACE ( )  B_SPLINE_SURFACE ( 3, 2, ( 
 ( #113815, #145218, #127964 ),
 ( #179815, #144161, #196070 ),
 ( #210153, #193916, #78037 ),
 ( #60718, #212285, #80168 ) ),
 .UNSPECIFIED., .F., .F., .F. ) 
 B_SPLINE_SURFACE_WITH_KNOTS ( ( 4, 4 ),
 ( 3, 3 ),
 ( 0.0002170249176783703470, 0.0009435326495461454589 ),
 ( 0.000000000000000000, 1.000000000000000000 ),
 .UNSPECIFIED. ) 
 GEOMETRIC_REPRESENTATION_ITEM ( )  RATIONAL_B_SPLINE_SURFACE ( (
 ( 1.000000000000000000, 0.6273451206645686007, 1.000000000000000000),
 ( 1.000000000000000000, 0.6198154398457387249, 1.000000000000000000),
 ( 1.000000000000000000, 0.6183696555398903172, 1.000000000000000000),
 ( 1.000000000000000000, 0.6222646319068203535, 1.000000000000000000) ) ) 
 REPRESENTATION_ITEM ( '' )  SURFACE ( )  );
#57444 = FACE_OUTER_BOUND ( 'NONE', #120630, .T. ) ;
#57445 = CARTESIAN_POINT ( 'NONE',  ( 3.680148631105580215, 6.380924938676771241, -1.199719254218446718 ) ) ;
#57447 = ORIENTED_EDGE ( 'NONE', *, *, #109647, .F. ) ;
#57446 = CARTESIAN_POINT ( 'NONE',  ( -5.932574734431526942, 9.079031735882207244, 1.199719254218454489 ) ) ;
#57448 = CARTESIAN_POINT ( 'NONE',  ( 5.410124943364367667, 7.538760657221164507, -1.247639402986647550 ) ) ;
#57449 = CARTESIAN_POINT ( 'NONE',  ( 3.585314394424500062, 1.281165535658060017, -1.556669873624405120 ) ) ;
#57450 = CARTESIAN_POINT ( 'NONE',  ( 2.677489186553200007, -0.9463553590365643142, 1.579155189138586435 ) ) ;
#57451 = EDGE_CURVE ( 'NONE', #23490, #185214, #106026, .T. ) ;
#57452 = CARTESIAN_POINT ( 'NONE',  ( 5.717509255324264572, 7.006698007003683948, 2.500000000000000444 ) ) ;
#57453 = CARTESIAN_POINT ( 'NONE',  ( 0.9971819109757291688, -0.5654680449962052879, -2.237236815885994989 ) ) ;
#57454 = CARTESIAN_POINT ( 'NONE',  ( 5.598591087800349086, 5.496387455380669529, -0.7998128361456481317 ) ) ;
#57455 = CARTESIAN_POINT ( 'NONE',  ( 3.831458500214664387, -1.998831773244442056, 0.8233788064144487162 ) ) ;
#57456 = CARTESIAN_POINT ( 'NONE',  ( -6.196239896645333367, 7.187700286629718605, -1.199719254218446718 ) ) ;
#57457 = CARTESIAN_POINT ( 'NONE',  ( 3.339543098909302898, -1.371423271284638590, 1.844254897846734131 ) ) ;
#57458 = AXIS2_PLACEMENT_3D ( 'NONE', #39643, #175797, #204242 ) ;
#57459 = CARTESIAN_POINT ( 'NONE',  ( 0.000000000000000000, 18.91999999999999815, -12.00000000000000178 ) ) ;
#57460 = CARTESIAN_POINT ( 'NONE',  ( 2.588565208901713266, -0.3177388942022137397, -1.843305967786903032 ) ) ;
#57461 = CARTESIAN_POINT ( 'NONE',  ( 6.280149219824591178, -1.055055557545642175, 1.665224566959803143 ) ) ;
#57462 = AXIS2_PLACEMENT_3D ( 'NONE', #142368, #208377, #171618 ) ;
#57465 = EDGE_CURVE ( 'NONE', #36555, #34978, #200864, .T. ) ;
#57464 = CARTESIAN_POINT ( 'NONE',  ( -6.749980374757255319, 8.968339418673846097, 1.599625672291269396 ) ) ;
#57463 = CARTESIAN_POINT ( 'NONE',  ( 1.364683531249988535, 4.363541667008090208, 0.7879004041258500513 ) ) ;
#57467 = CARTESIAN_POINT ( 'NONE',  ( 0.7685542157043163680, 1.090964843879228097, 1.918292034055509632 ) ) ;
#57466 = CARTESIAN_POINT ( 'NONE',  ( -4.740547266272593596, 8.682388910626682943, -0.7998128361456281477 ) ) ;
#57468 = LINE ( 'NONE', #156035, #188871 ) ;
#57469 = CARTESIAN_POINT ( 'NONE',  ( 4.819033534653518025, 7.709623992816043270, -1.199719254218452047 ) ) ;
#57470 = CARTESIAN_POINT ( 'NONE',  ( -5.063080299699540987, 7.994345218703034384, 1.199719254218464037 ) ) ;
#57471 = CARTESIAN_POINT ( 'NONE',  ( -0.01387835396683118061, -7.030163990561719700, -9.597420367780069128 ) ) ;
#57472 = CARTESIAN_POINT ( 'NONE',  ( 6.473508845062264427, 1.886732274579514756, -0.5718055884485659934 ) ) ;
#57473 = EDGE_CURVE ( 'NONE', #51181, #197365, #117940, .T. ) ;
#57474 = CARTESIAN_POINT ( 'NONE',  ( 5.988978958577418688, -0.3324729122747641097, -2.283524998171110543 ) ) ;
#57475 = CARTESIAN_POINT ( 'NONE',  ( 6.619592957969418379, 0.3166511089685022928, -1.833750044983559535 ) ) ;
#57476 = CARTESIAN_POINT ( 'NONE',  ( 3.098538415137185531, 2.046439989356943823, 0.2571918767454490773 ) ) ;
#57477 = CARTESIAN_POINT ( 'NONE',  ( 5.504247177468168495, 9.365446107114122398, 0.7216878364870438212 ) ) ;
#57478 = CARTESIAN_POINT ( 'NONE',  ( 8.167861197590044142, 8.493869250135347215, 0.000000000000000000 ) ) ;
#57479 = CARTESIAN_POINT ( 'NONE',  ( 5.775410249297131315, 9.681803024247919609, 1.040834085586084257E-14 ) ) ;
#57480 = CARTESIAN_POINT ( 'NONE',  ( -1.364683531250012516, 3.051041667008083547, -0.7879004041258289570 ) ) ;
#57481 = CARTESIAN_POINT ( 'NONE',  ( -7.058728332971268671, 14.55191201140709012, 9.659722983215184300 ) ) ;
#57482 = CARTESIAN_POINT ( 'NONE',  ( 4.148431815657221300, 7.783661518334664464, 1.040834085586084257E-14 ) ) ;
#57483 = CARTESIAN_POINT ( 'NONE',  ( 5.248546085168739772, -2.154154806625402596, -0.2710006578958406576 ) ) ;
#57484 = CARTESIAN_POINT ( 'NONE',  ( 4.722110844128335039, 1.763445737372179689, 0.5296355584529164329 ) ) ;
#57486 = CARTESIAN_POINT ( 'NONE',  ( 6.620655732516649294, 0.5971256128398574337, 1.879834161342401666 ) ) ;
#57485 = DIRECTION ( 'NONE',  ( 0.000000000000000000, 1.000000000000000000, 0.000000000000000000 ) ) ;
#57487 = CARTESIAN_POINT ( 'NONE',  ( 6.515165533258342023, -2.126321577054360201, 0.5302794918828001025 ) ) ;
#57488 = CARTESIAN_POINT ( 'NONE',  ( 0.5439545674776785633, 1.865077268347898665, 0.1441030193207945287 ) ) ;
#57489 = CARTESIAN_POINT ( 'NONE',  ( 6.737213295527981316, -2.024711933681651477, 1.009942563148768846 ) ) ;
#57490 = CARTESIAN_POINT ( 'NONE',  ( -5.337630915675663168, 6.534101986612459001, 1.368282111488251074 ) ) ;
#57491 = DIRECTION ( 'NONE',  ( 0.7592566023653005702, 0.6507913734559640506, 0.000000000000000000 ) ) ;
#57492 = CARTESIAN_POINT ( 'NONE',  ( 6.430738266435902517, 6.882057634903050669, 0.7203813067775278745 ) ) ;
#57493 = PRODUCT_DEFINITION ( 'UNKNOWN', '', #10696, #187288 ) ;
#57494 = CARTESIAN_POINT ( 'NONE',  ( -3.797692425159308716, 7.444741906078900406, 0.000000000000000000 ) ) ;
#57495 = CARTESIAN_POINT ( 'NONE',  ( 0.2582720099171369466, 1.907150531373353664, 0.1405958444523764117 ) ) ;
#57496 = CARTESIAN_POINT ( 'NONE',  ( 1.428175943150990390, 1.704372189200783705, 0.4766478552604267449 ) ) ;
#57497 = AXIS2_PLACEMENT_3D ( 'NONE', #7704, #42386, #23957 ) ;
#57498 = CARTESIAN_POINT ( 'NONE',  ( 5.988937038716908745, -1.912324646158647168, -0.6291777902352905238 ) ) ;
#57500 = CARTESIAN_POINT ( 'NONE',  ( 3.673361179623610084, 1.389826993061950899, 1.318567953439080620 ) ) ;
#57499 = CARTESIAN_POINT ( 'NONE',  ( -2.453662613948990323, 5.806430783008362795, -0.7216878364870257245 ) ) ;
#57501 = CARTESIAN_POINT ( 'NONE',  ( 9.499766273075866962, -9.919999999999998153, -0.06663900456893058488 ) ) ;
#57502 = CARTESIAN_POINT ( 'NONE',  ( 4.598083368088573764, 0.8440023354334601491, -1.779705283501178181 ) ) ;
#57503 = CARTESIAN_POINT ( 'NONE',  ( 6.240491321897984278, 1.159586379754873331, -1.653562141909877603 ) ) ;
#57504 = CARTESIAN_POINT ( 'NONE',  ( -3.972702704004144714, 4.593573561881607148, 1.199719254218462483 ) ) ;
#57505 = CARTESIAN_POINT ( 'NONE',  ( 2.746779440450992649, -1.556306552617524597, 1.037596984913228937 ) ) ;
#57507 = VERTEX_POINT ( 'NONE', #170965 ) ;
#57506 = CARTESIAN_POINT ( 'NONE',  ( 5.830603237517035353, 1.664100180626144398, 0.4535787370015566533 ) ) ;
#57509 = CARTESIAN_POINT ( 'NONE',  ( 3.375617060122621194, 6.882044303544283537, 1.040834085586084257E-14 ) ) ;
#57508 = CARTESIAN_POINT ( 'NONE',  ( 2.754729969050898841, 0.7443088323898851000, 2.077706851784946185 ) ) ;
#57510 = PRESENTATION_LAYER_ASSIGNMENT (  '', '', ( #199581 ) ) ;
#57511 = CARTESIAN_POINT ( 'NONE',  ( -0.6823417656250003738, 3.030208333674754062, -1.181850606188749264 ) ) ;
#57512 = CARTESIAN_POINT ( 'NONE',  ( 6.426224708462171087, 1.007414738832881351, 1.683299376423300853 ) ) ;
#57513 = CARTESIAN_POINT ( 'NONE',  ( 6.726816770674637347, 10.99970333242910669, -0.7998128361456291469 ) ) ;
#57514 = CARTESIAN_POINT ( 'NONE',  ( -8.455481356417053007, 13.01647868246193518, 0.7998128361456341429 ) ) ;
#57515 = CARTESIAN_POINT ( 'NONE',  ( 0.3313999689851374608, -9.006862915010144022, -9.494725171580505219 ) ) ;
#57516 = CARTESIAN_POINT ( 'NONE',  ( -5.603597561149804562, 5.431951997629870910, 0.7998128361456341429 ) ) ;
#57517 = SPHERICAL_SURFACE ( 'NONE', #120336, 1.250000000000000000 ) ;
#57518 = ORIENTED_EDGE ( 'NONE', *, *, #158806, .F. ) ;
#57519 = CARTESIAN_POINT ( 'NONE',  ( 1.856005582152659317, -0.6995316168164237292, 1.948720873434762080 ) ) ;
#57520 = CARTESIAN_POINT ( 'NONE',  ( -0.7499999999999972244, 3.108333333333358706, -1.299038105676652011 ) ) ;
#57521 = CARTESIAN_POINT ( 'NONE',  ( 5.281064527722868718, 6.119995689553514140, 1.199719254218462483 ) ) ;
#57522 = CARTESIAN_POINT ( 'NONE',  ( 4.095444919779759552, 6.935713618788495793, 1.199719254218451159 ) ) ;
#57523 = CARTESIAN_POINT ( 'NONE',  ( 0.2584707923105635796, 2.014430608512500775, 0.1461574478831758339 ) ) ;
#57524 =( NAMED_UNIT ( * ) PLANE_ANGLE_UNIT ( ) SI_UNIT ( $, .RADIAN. ) );
#57525 = CARTESIAN_POINT ( 'NONE',  ( 0.6823417656249917140, 3.842708333674754506, 1.181850606188765695 ) ) ;
#57526 = ORIENTED_EDGE ( 'NONE', *, *, #74644, .T. ) ;
#57527 = AXIS2_PLACEMENT_3D ( 'NONE', #211867, #196702, #48342 ) ;
#57529 = CARTESIAN_POINT ( 'NONE',  ( 8.758204044747998296, 11.24099069033793974, 1.443375672974076540 ) ) ;
#57528 = CARTESIAN_POINT ( 'NONE',  ( -0.4019237886467001974, 11.80133545031536890, 1.500000000000001998 ) ) ;
#57530 = CARTESIAN_POINT ( 'NONE',  ( 5.220077296912079667, -1.701688162634030999, -1.080898591909580597 ) ) ;
#57531 = CARTESIAN_POINT ( 'NONE',  ( 5.049963001771692106, 0.9498492218114750196, 1.663612537209507858 ) ) ;
#57532 = CARTESIAN_POINT ( 'NONE',  ( 6.539320575229274013, 2.055156488754609878, 2.310649141506931681 ) ) ;
#57533 = CARTESIAN_POINT ( 'NONE',  ( 2.226364491882920404, 2.126620374013419301, 0.5291077681483095096 ) ) ;
#57534 = CARTESIAN_POINT ( 'NONE',  ( -0.7500000000000215383, 2.472916667349486897, 1.299038105676671107 ) ) ;
#57535 = CARTESIAN_POINT ( 'NONE',  ( 2.742330423940505302, 1.058908597569432120, -1.592262909973440888 ) ) ;
#57536 = CARTESIAN_POINT ( 'NONE',  ( -6.389970470742427189, 6.349387058821269747, -0.7998128361456291469 ) ) ;
#57538 = CARTESIAN_POINT ( 'NONE',  ( 0.08751785467620704084, -0.5350655163729299835, 1.944078888069140865 ) ) ;
#57537 = CARTESIAN_POINT ( 'NONE',  ( 1.500000000000007105, 10.64264068711930733, 1.214306433183764966E-14 ) ) ;
#57540 = EDGE_CURVE ( 'NONE', #106229, #169055, #155798, .T. ) ;
#57539 = CARTESIAN_POINT ( 'NONE',  ( -1.364683531250014514, 10.15104166700806587, -0.7879004041258335089 ) ) ;
#57542 = CARTESIAN_POINT ( 'NONE',  ( -4.959250327548641479, 9.007818825440551791, -0.7998128361456362523 ) ) ;
#57541 = CARTESIAN_POINT ( 'NONE',  ( 5.618738332679400038, -0.05485954975367920983, 2.191026952110195491 ) ) ;
#57544 = EDGE_LOOP ( 'NONE', ( #18403, #1270, #47196, #166621 ) ) ;
#57543 = CARTESIAN_POINT ( 'NONE',  ( 3.592533753846867128, -0.3360022577178176650, -1.691527450499834995 ) ) ;
#57545 = CARTESIAN_POINT ( 'NONE',  ( 5.888958097455844864, -2.014202512972632420, -0.6635655960139998921 ) ) ;
#57546 = CARTESIAN_POINT ( 'NONE',  ( 4.364835388595708743, 7.179726155748598515, 1.199719254218462483 ) ) ;
#57547 = CARTESIAN_POINT ( 'NONE',  ( 0.2034672893990868703, -1.513989045467616146, -1.247398002513319781 ) ) ;
#57548 = CARTESIAN_POINT ( 'NONE',  ( 0.000000000000000000, 3.956598013261175772, 0.000000000000000000 ) ) ;
#57549 = CARTESIAN_POINT ( 'NONE',  ( 4.656335691289526402, 7.519809842224722374, -1.199719254218452047 ) ) ;
#57550 = CARTESIAN_POINT ( 'NONE',  ( 0.1399997263885795762, 1.361443548867202757, -2.255028951473649901 ) ) ;
#57551 = ORIENTED_EDGE ( 'NONE', *, *, #84582, .T. ) ;
#57552 = CARTESIAN_POINT ( 'NONE',  ( 9.495347311156807635, -6.857257212219900921, -1.861063089699362494E-15 ) ) ;
#57553 = EDGE_LOOP ( 'NONE', ( #63025, #179576, #141493, #87386 ) ) ;
#57554 = CARTESIAN_POINT ( 'NONE',  ( 2.930093016812723050, -0.8946826049299866357, -1.575034454935933859 ) ) ;
#57555 = VERTEX_POINT ( 'NONE', #123387 ) ;
#57556 = CARTESIAN_POINT ( 'NONE',  ( 9.673906298550626559, 11.24497775551929557, 1.199719254218452047 ) ) ;
#57557 = CARTESIAN_POINT ( 'NONE',  ( 6.086684617892325733, 6.065829907154645539, -0.7998128361456481317 ) ) ;
#57558 = CARTESIAN_POINT ( 'NONE',  ( 3.492628052329676880, -1.746589362535276191, -0.4802254367691183856 ) ) ;
#57559 = CARTESIAN_POINT ( 'NONE',  ( 7.526184668917440312, 8.913541880892736913, -1.082531754730548412 ) ) ;
#57560 = DIRECTION ( 'NONE',  ( 0.6783731810844091381, 3.929830605827845711E-15, 0.7347175152297782397 ) ) ;
#57561 = CARTESIAN_POINT ( 'NONE',  ( 5.841717777309253457, 6.007722996832359996, 0.3783690319567531435 ) ) ;
#57563 = CARTESIAN_POINT ( 'NONE',  ( -1.364683531250000748, 14.60937500034140157, 0.000000000000000000 ) ) ;
#57562 = CARTESIAN_POINT ( 'NONE',  ( 4.756226040108163744, -1.860656195911802646, -0.04637829637440040592 ) ) ;
#57564 = CARTESIAN_POINT ( 'NONE',  ( 2.987788816292748173, -1.913300742920095221, 0.09679331860494060080 ) ) ;
#57565 = CARTESIAN_POINT ( 'NONE',  ( 1.026062881544724137, 1.091098483296793820, -1.463488004260153907 ) ) ;
#57566 = CARTESIAN_POINT ( 'NONE',  ( 4.726673625894836306, 8.212911231124076394, 0.6865719651209405416 ) ) ;
#57567 = CARTESIAN_POINT ( 'NONE',  ( -11.50450067106337571, 6.429220943216678030, -3.050492100467481205 ) ) ;
#57568 = CARTESIAN_POINT ( 'NONE',  ( 5.417061852544872380, 7.532864896096530316, 1.248242807326222392 ) ) ;
#57569 = CARTESIAN_POINT ( 'NONE',  ( 9.598595877357185557, 13.73909624707286703, 8.266025096903813818 ) ) ;
#57570 = CARTESIAN_POINT ( 'NONE',  ( -10.99947830037066865, -9.912501460265211506, 0.1071380031274376810 ) ) ;
#57571 = CARTESIAN_POINT ( 'NONE',  ( 0.000000000000000000, -9.919999999999998153, 0.000000000000000000 ) ) ;
#57572 = CARTESIAN_POINT ( 'NONE',  ( 5.639828713604826405, 9.523624565940227882, -0.7216878364870267237 ) ) ;
#57573 = CARTESIAN_POINT ( 'NONE',  ( 5.576995328841173105, 1.818227641914264225, 0.7572995901278417596 ) ) ;
#57574 = CARTESIAN_POINT ( 'NONE',  ( -4.253507506385335368, 5.985511395581417204, 1.599625672291267398 ) ) ;
#57575 = CARTESIAN_POINT ( 'NONE',  ( 1.078203232848734094, -2.040033308301641757, -0.4564361842656887713 ) ) ;
#57576 = CARTESIAN_POINT ( 'NONE',  ( 6.756866522006341746, -1.488468187722398417, 1.222521302487014072 ) ) ;
#57577 = CARTESIAN_POINT ( 'NONE',  ( -6.579784621333750749, 6.570836901177822931, 0.7998128361456341429 ) ) ;
#57578 = EDGE_CURVE ( 'NONE', #157346, #37534, #93783, .T. ) ;
#57579 = CARTESIAN_POINT ( 'NONE',  ( 1.992912282819898850, 1.589903476415389871, -0.8970392876451321884 ) ) ;
#57580 = CARTESIAN_POINT ( 'NONE',  ( 3.580891165198408110, -2.126768340858419926, -0.5889919780145411732 ) ) ;
#57581 = CARTESIAN_POINT ( 'NONE',  ( 11.86145017031048177, 12.59418046486144327, 1.099999999999996980 ) ) ;
#57582 = CARTESIAN_POINT ( 'NONE',  ( 0.9492982845318720386, -1.727743609841876360, 0.8201845251225792222 ) ) ;
#57583 = CARTESIAN_POINT ( 'NONE',  ( 2.014047288863869412, 1.964499257916036079, -0.1416769614510370867 ) ) ;
#57584 = CARTESIAN_POINT ( 'NONE',  ( 2.349080241353004528, 0.5156090978439072936, -1.872316843566106614 ) ) ;
#57585 = MECHANICAL_DESIGN_GEOMETRIC_PRESENTATION_REPRESENTATION (  '', ( #71310 ), #85233 ) ;
#57586 = EDGE_LOOP ( 'NONE', ( #189373, #45539, #134977, #167456 ) ) ;
#57587 = CARTESIAN_POINT ( 'NONE',  ( 3.094265954482837255, 2.800000000000017586, 2.490342512183689294 ) ) ;
#57589 = CARTESIAN_POINT ( 'NONE',  ( 6.983263157960402090, -0.0002233252893329463486, 1.845923184817334084 ) ) ;
#57588 = CARTESIAN_POINT ( 'NONE',  ( -4.736594563127865420, 6.619389305106191834, -1.599625672291271394 ) ) ;
#57590 = CARTESIAN_POINT ( 'NONE',  ( 4.817943484809818600, 6.714296380401858499, 1.599625672291269396 ) ) ;
#57591 = CARTESIAN_POINT ( 'NONE',  ( 1.250000000000037526, 8.500000000000000000, -11.02939254900286592 ) ) ;
#57592 = CARTESIAN_POINT ( 'NONE',  ( 10.57266086055835075, 11.22919251360659310, 0.000000000000000000 ) ) ;
#57593 = CARTESIAN_POINT ( 'NONE',  ( -5.529746549527323474, 7.544733289238903851, -1.599625672291271394 ) ) ;
#57594 = CARTESIAN_POINT ( 'NONE',  ( 2.525153347276567484, -2.043736813514348771, 0.7916865192442237298 ) ) ;
#57595 = CARTESIAN_POINT ( 'NONE',  ( 5.580062740476173566, 8.667767742934335828, 1.199719254218451159 ) ) ;
#57596 = LINE ( 'NONE', #172418, #68384 ) ;
#57597 = CARTESIAN_POINT ( 'NONE',  ( 2.965264444195826243, 0.2674972279559268973, -1.805858685475017378 ) ) ;
#57598 =( NAMED_UNIT ( * ) PLANE_ANGLE_UNIT ( ) SI_UNIT ( $, .RADIAN. ) );
#57599 = CARTESIAN_POINT ( 'NONE',  ( -2.103486388414573138, 5.605817886458954291, 1.040834085586084257E-14 ) ) ;
#57600 = CARTESIAN_POINT ( 'NONE',  ( -5.747140441703231240, 7.374164810257596514, -1.320148062302946013 ) ) ;
#57601 = CARTESIAN_POINT ( 'NONE',  ( -0.4577034257980932552, -0.8887487162305418575, -3.253519940713586855 ) ) ;
#57602 = CARTESIAN_POINT ( 'NONE',  ( 8.239604668803105270, 10.63595808506888396, -1.599625672291268286 ) ) ;
#57603 = CARTESIAN_POINT ( 'NONE',  ( 2.314956460678399885, 1.720770591318865339, 0.8663633404912238767 ) ) ;
#57604 = CARTESIAN_POINT ( 'NONE',  ( 0.5281409364047099375, 2.800000000000018030, 1.340854145587128787 ) ) ;
#57605 = CARTESIAN_POINT ( 'NONE',  ( -0.7500000000000006661, 15.20833333333333748, -1.299038105676657340 ) ) ;
#57606 = CARTESIAN_POINT ( 'NONE',  ( -8.213542131780492639, 8.476887330032372603, 1.040834085586084257E-14 ) ) ;
#57607 = CARTESIAN_POINT ( 'NONE',  ( 5.009901455449552010, 5.803638771901306725, -1.199719254218452047 ) ) ;
#57608 = ADVANCED_FACE ( 'NONE', ( #28994 ), #202284, .T. ) ;
#57609 = CARTESIAN_POINT ( 'NONE',  ( -4.624739795592943459, 6.488892076315448065, -1.443375672974066548 ) ) ;
#57610 = CONICAL_SURFACE ( 'NONE', #199358, 4.500000000000000000, 0.7853981633974491672 ) ;
#57611 =( GEOMETRIC_REPRESENTATION_CONTEXT ( 3 ) GLOBAL_UNCERTAINTY_ASSIGNED_CONTEXT ( ( #72303 ) ) GLOBAL_UNIT_ASSIGNED_CONTEXT ( ( #139680, #91994, #158054 ) ) REPRESENTATION_CONTEXT ( 'NONE', 'WORKASPACE' ) );
#57612 = CARTESIAN_POINT ( 'NONE',  ( 10.37606763316019531, 10.99983374830873650, 0.7998128361456462443 ) ) ;
#57613 = CARTESIAN_POINT ( 'NONE',  ( 1.737500000000001155, -2.333333333333333037, 3.009438278150922130 ) ) ;
#57614 = CARTESIAN_POINT ( 'NONE',  ( 5.243061650278370678, -0.2479348644398685908, -2.055265572831247667 ) ) ;
#57616 = CARTESIAN_POINT ( 'NONE',  ( -1.364683531250012516, 3.051041667008083547, -0.7879004041258289570 ) ) ;
#57615 = CARTESIAN_POINT ( 'NONE',  ( 0.2043192855987647494, 1.601443664334546213, 0.9084302959305108338 ) ) ;
#57617 = VERTEX_POINT ( 'NONE', #162200 ) ;
#57618 = CARTESIAN_POINT ( 'NONE',  ( 5.291695567192507887, 1.742433043099327561, -1.499359156687163575 ) ) ;
#57619 = CARTESIAN_POINT ( 'NONE',  ( 5.639828713604826405, 9.523624565940227882, -0.7216878364870267237 ) ) ;
#57621 =( NAMED_UNIT ( * ) SI_UNIT ( $, .STERADIAN. ) SOLID_ANGLE_UNIT ( ) );
#57620 = CARTESIAN_POINT ( 'NONE',  ( 4.231553341240963384, 7.950912974840849579, -0.7216878364870357165 ) ) ;
#57622 = CARTESIAN_POINT ( 'NONE',  ( 6.585440809757122871, -0.9837151097084917417, 2.068200907652519405 ) ) ;
#57623 = CARTESIAN_POINT ( 'NONE',  ( 6.773846765317306229, -7.246166700180828535, -6.773846765317331986 ) ) ;
#57624 = CARTESIAN_POINT ( 'NONE',  ( -7.045397100956844127, 8.248660034984974132, -1.199719254218452047 ) ) ;
#57625 = CARTESIAN_POINT ( 'NONE',  ( 4.435450497376713486, 0.8291751068889623433, -1.756158939159500276 ) ) ;
#57626 = ORIENTED_EDGE ( 'NONE', *, *, #48949, .T. ) ;
#57627 = CARTESIAN_POINT ( 'NONE',  ( 9.531018800282609504, 10.22186947652563305, 0.7216878364870458196 ) ) ;
#57628 = ORIENTED_EDGE ( 'NONE', *, *, #18034, .T. ) ;
#57629 = CARTESIAN_POINT ( 'NONE',  ( -0.1052096654315381741, -1.953846233167291002, -0.4849948655165080558 ) ) ;
#57630 = CARTESIAN_POINT ( 'NONE',  ( 0.09967489844521590370, -1.724374414367945141, -0.04833993824084405894 ) ) ;
#57631 = CARTESIAN_POINT ( 'NONE',  ( 6.051970301643104122, 1.040788372175960541, 1.727066800951609027 ) ) ;
#57633 = CARTESIAN_POINT ( 'NONE',  ( -11.86145016429273014, 10.90000000000000036, -1.100000000000002087 ) ) ;
#57632 = CARTESIAN_POINT ( 'NONE',  ( -8.585337585951595685, 11.03931315507545108, -1.599625672291263179 ) ) ;
#57634 = CARTESIAN_POINT ( 'NONE',  ( -3.285556943750000514, -1.626041666188708046, -1.896917185911906500 ) ) ;
#57636 = CARTESIAN_POINT ( 'NONE',  ( 1.094210320218844679, -0.4249228298987791086, -1.717946482988210510 ) ) ;
#57635 = CARTESIAN_POINT ( 'NONE',  ( 2.273483640244071680, 1.287084957891961423, 1.647379119656503965 ) ) ;
#57637 = CARTESIAN_POINT ( 'NONE',  ( 4.181342156266883769, 7.197418463578268089, 1.132749409379085748 ) ) ;
#57638 = CARTESIAN_POINT ( 'NONE',  ( 4.066585926679040064, -2.138228679320841152, -0.8265488639036464580 ) ) ;
#57639 = CARTESIAN_POINT ( 'NONE',  ( 2.589492015636893907, -1.735658606974595619, -0.1281804514613407997 ) ) ;
#57640 = CARTESIAN_POINT ( 'NONE',  ( 3.344057444064992168, 7.053150784717805877, 1.040834085586084257E-14 ) ) ;
#57641 = CARTESIAN_POINT ( 'NONE',  ( 5.899733120602060232, 6.912052057904395141, -1.199719254218452047 ) ) ;
#57642 = CARTESIAN_POINT ( 'NONE',  ( 1.756802591741468245, -1.724947740463366852, -0.1754148046573481556 ) ) ;
#57643 = CARTESIAN_POINT ( 'NONE',  ( 0.6801582343749987825, 2.338541667008108060, -1.178068619123883165 ) ) ;
#57644 = CARTESIAN_POINT ( 'NONE',  ( 2.084208510888691190, 1.074786400414856624, -1.519112143004421434 ) ) ;
#57645 = CARTESIAN_POINT ( 'NONE',  ( 2.277988012537075502, -2.106425727361205702, 0.5258826003073436839 ) ) ;
#57646 = CARTESIAN_POINT ( 'NONE',  ( 4.961394147597008697, 7.875711374583454827, -1.199719254218452047 ) ) ;
#57647 = CARTESIAN_POINT ( 'NONE',  ( 3.766814776335784209, -0.2024620155892907503, -2.006371719556559796 ) ) ;
#57649 = CIRCLE ( 'NONE', #113071, 0.08000000000000023759 ) ;
#57648 = CARTESIAN_POINT ( 'NONE',  ( 2.875000000000002220, 2.052068128417948056, -1.638482584539516883E-13 ) ) ;
#57650 = CARTESIAN_POINT ( 'NONE',  ( 1.499999999999987121, 2.827083334016148530, -0.8660254037844262731 ) ) ;
#57651 = CARTESIAN_POINT ( 'NONE',  ( 1.184454412485607344, -1.878822398200689525, -0.4247803175085519412 ) ) ;
#57652 = CARTESIAN_POINT ( 'NONE',  ( 1.364683531249996529, 14.71354166700806410, 0.7879004041258405033 ) ) ;
#57653 = CARTESIAN_POINT ( 'NONE',  ( 4.728890529236228879, 1.530954898644999451, -1.609847601234422276 ) ) ;
#57654 = ORIENTED_EDGE ( 'NONE', *, *, #148115, .F. ) ;
#57655 = PLANE ( 'NONE',  #29019 ) ;
#57656 = CARTESIAN_POINT ( 'NONE',  ( 1.499999999999989120, 0.2750000000000182854, 0.000000000000000000 ) ) ;
#57657 = CARTESIAN_POINT ( 'NONE',  ( 8.101160479365381306, 9.410107633136481908, -1.199719254218446718 ) ) ;
#57658 = ADVANCED_FACE ( 'NONE', ( #46322 ), #173247, .T. ) ;
#57659 = CARTESIAN_POINT ( 'NONE',  ( 1.364683531249988757, -0.3656249996585800299, 0.000000000000000000 ) ) ;
#57660 = CARTESIAN_POINT ( 'NONE',  ( 5.976846119194893170, -1.571437351877506439, 1.570356403719268101 ) ) ;
#57662 = CARTESIAN_POINT ( 'NONE',  ( 4.773855682050706761, -1.924389145058275963, 0.3807478752155256663 ) ) ;
#57661 = VECTOR ( 'NONE', #158972, 1000.000000000000000 ) ;
#57663 = CARTESIAN_POINT ( 'NONE',  ( 8.432808358020004391, 12.78210081775797669, 0.7216878364870438212 ) ) ;
#57664 = CARTESIAN_POINT ( 'NONE',  ( 5.501357770389488699, 1.845074063491736860, 1.309031944507930589 ) ) ;
#57665 = CARTESIAN_POINT ( 'NONE',  ( -5.722950238744243023, 7.770137593325314285, 1.443375672974058777 ) ) ;
#57666 = CARTESIAN_POINT ( 'NONE',  ( 2.805193546069509214, -1.716336894061726737, 1.143758443631032407 ) ) ;
#57667 = CARTESIAN_POINT ( 'NONE',  ( -4.693093728624763372, 8.627026450037540428, 0.7998128361456481317 ) ) ;
#57668 = B_SPLINE_CURVE_WITH_KNOTS ( 'NONE', 3,
 ( #194126, #31646, #130284, #213551, #197323, #32695, #163781, #147530, #80384, #13246 ),
 .UNSPECIFIED., .F., .F.,
 ( 4, 2, 2, 2, 4 ),
 ( 0.000000000000000000, 0.0002299353307164137407, 0.0004598706614328274813, 0.0006898059921492411678, 0.0009197413228656549627 ),
 .UNSPECIFIED. ) ;
#57669 = CARTESIAN_POINT ( 'NONE',  ( -1.500000000000013101, 2.160416667349489561, -0.8660254037844313801 ) ) ;
#57670 = CARTESIAN_POINT ( 'NONE',  ( 1.364683531249988535, 4.467708333674754506, -0.7879004041258300672 ) ) ;
#57671 = CARTESIAN_POINT ( 'NONE',  ( 5.096879011283717453, 1.555924861325823416, -1.037969726935553005 ) ) ;
#57672 = CARTESIAN_POINT ( 'NONE',  ( 3.322662972295143291, 0.7760272377477626105, -1.550874960589002871 ) ) ;
#57673 = CARTESIAN_POINT ( 'NONE',  ( 2.788295088316892656, 1.491546084125561888, -0.8966509355741271170 ) ) ;
#57674 = CARTESIAN_POINT ( 'NONE',  ( 0.6973257247198815234, 1.878305535369644064, 1.313909787900492843 ) ) ;
#57675 = CARTESIAN_POINT ( 'NONE',  ( 0.5873203293235219613, -0.2722241568871349160, -2.189838084831654541 ) ) ;
#57676 = CARTESIAN_POINT ( 'NONE',  ( 4.810148555269133652, 1.440736570533694527, -1.515338330687252988 ) ) ;
#57677 = CARTESIAN_POINT ( 'NONE',  ( 5.138593782488270811, -1.664572445771801634, 0.9999684565626990596 ) ) ;
#57678 = CIRCLE ( 'NONE', #178749, 1.868950538045371035 ) ;
#57679 = EDGE_CURVE ( 'NONE', #93554, #103541, #109252, .T. ) ;
#57681 = EDGE_LOOP ( 'NONE', ( #145116, #116094, #143253, #159848 ) ) ;
#57680 = FACE_OUTER_BOUND ( 'NONE', #190607, .T. ) ;
#57682 = CARTESIAN_POINT ( 'NONE',  ( 0.2467204944939948574, 1.994070950632735428, -0.2986300710981006357 ) ) ;
#57683 = CARTESIAN_POINT ( 'NONE',  ( -0.1753031400193918732, -0.9122597987226389593, -1.912455998546586544 ) ) ;
#57684 = CARTESIAN_POINT ( 'NONE',  ( 1.685698123273788651, -1.399999999999998579, -1.979500400907064916 ) ) ;
#57685 = CARTESIAN_POINT ( 'NONE',  ( -7.991641480251377772, 11.41099992934688956, 1.199719254218453823 ) ) ;
#57686 = CARTESIAN_POINT ( 'NONE',  ( 5.784525094524856748, 9.900363043587685041, 1.040834085586084257E-14 ) ) ;
#57687 = CARTESIAN_POINT ( 'NONE',  ( 3.914527900857078357, 1.289819402409349669, -1.292354223553587644 ) ) ;
#57688 = CARTESIAN_POINT ( 'NONE',  ( 2.063769564651289912, 0.3772465526380370804, -2.174136642525636098 ) ) ;
#57689 = VERTEX_POINT ( 'NONE', #178451 ) ;
#57690 = CARTESIAN_POINT ( 'NONE',  ( -7.095713291905736853, 9.371694488680407886, 1.599625672291269396 ) ) ;
#57691 = CARTESIAN_POINT ( 'NONE',  ( -5.015590482412729756, 4.816220082428420923, 0.000000000000000000 ) ) ;
#57692 = CARTESIAN_POINT ( 'NONE',  ( 1.642778471875001811, -2.180208332855374742, 2.845375778867859751 ) ) ;
#57693 = CARTESIAN_POINT ( 'NONE',  ( -8.342344591110322227, 8.627156865917170236, -0.7998128361456291469 ) ) ;
#57694 = CARTESIAN_POINT ( 'NONE',  ( 1.424088383587719386, -2.004042310577313302, 0.2513328237187910652 ) ) ;
#57695 = CARTESIAN_POINT ( 'NONE',  ( -5.808742468812186033, 5.741564066561132940, 0.000000000000000000 ) ) ;
#57696 = CARTESIAN_POINT ( 'NONE',  ( 3.485049009367678252, 0.04119252264746588871, 1.860649646085434039 ) ) ;
#57697 = CARTESIAN_POINT ( 'NONE',  ( 3.297657676621871925, 4.870353260857385180, 1.599625672291267398 ) ) ;
#57698 = CARTESIAN_POINT ( 'NONE',  ( -0.4170821662629279336, 3.033599471985628959, -0.4170821662629279336 ) ) ;
#57699 = VERTEX_POINT ( 'NONE', #113509 ) ;
#57700 = CARTESIAN_POINT ( 'NONE',  ( -3.879604511804807032, 7.677955697080923514, 0.7998128361456341429 ) ) ;
#57701 = CARTESIAN_POINT ( 'NONE',  ( -7.784352752540590004, 12.23349531127272094, 0.7998128361456481317 ) ) ;
#57702 = CARTESIAN_POINT ( 'NONE',  ( 5.356004772612798170, 1.823420152956479523, -0.09349780940721279243 ) ) ;
#57704 = CARTESIAN_POINT ( 'NONE',  ( -3.985535776513723150, 7.835598525918981316, 0.2247789072947203870 ) ) ;
#57703 = CARTESIAN_POINT ( 'NONE',  ( -3.980200614063634568, 6.801261928786307642, 1.199719254218452935 ) ) ;
#57705 = CARTESIAN_POINT ( 'NONE',  ( 6.596403382356258227, 6.772441155557838321, -0.1798620802159808241 ) ) ;
#57706 = CARTESIAN_POINT ( 'NONE',  ( 0.3152591496230552348, -1.397726865852641387, 1.025726801146044531 ) ) ;
#57707 = CARTESIAN_POINT ( 'NONE',  ( 6.597600327481837112, -1.840612352326329804, 0.05063316525460298534 ) ) ;
#57708 = CARTESIAN_POINT ( 'NONE',  ( 4.301628547034565209, 1.852045629758605649, 1.376555262909467947 ) ) ;
#57709 = CARTESIAN_POINT ( 'NONE',  ( 4.179656494762836516, 8.098292687190454586, -0.7998128361456362523 ) ) ;
#57710 = CARTESIAN_POINT ( 'NONE',  ( 0.5794586325245559832, 1.923780613697351427, -0.7393501692522960189 ) ) ;
#57711 = CARTESIAN_POINT ( 'NONE',  ( 7.142447996300871793, 7.227277505306155092, 0.7998128361456341429 ) ) ;
#57712 = CARTESIAN_POINT ( 'NONE',  ( 6.046309306592402955, 2.127046199546629435, -0.8712367593181246095 ) ) ;
#57713 = CARTESIAN_POINT ( 'NONE',  ( -2.587713642112661638, -3.232243495192087757, 2.046355377693061861 ) ) ;
#57714 = CARTESIAN_POINT ( 'NONE',  ( -4.938913097128142304, 8.984092056616635347, -0.7998128361456362523 ) ) ;
#57715 = CARTESIAN_POINT ( 'NONE',  ( 5.664887262500884368, -1.691755685069219695, -0.7986314380193232365 ) ) ;
#57716 = EDGE_LOOP ( 'NONE', ( #98343, #125560, #42423, #32241 ) ) ;
#57719 = EDGE_CURVE ( 'NONE', #58569, #30509, #88084, .T. ) ;
#57718 = CARTESIAN_POINT ( 'NONE',  ( -3.298376509874564988, 7.070132704820777825, 0.000000000000000000 ) ) ;
#57717 = CARTESIAN_POINT ( 'NONE',  ( 2.443496805918866865, -1.782974011999260977, 0.6919810379762069141 ) ) ;
#57720 = CARTESIAN_POINT ( 'NONE',  ( 5.127635347277352373, -2.096377701570474539, 0.6897739467496829535 ) ) ;
#57721 = CARTESIAN_POINT ( 'NONE',  ( 4.259064461820570635, -0.003692207519963904699, -2.117513409117043999 ) ) ;
#57722 = CARTESIAN_POINT ( 'NONE',  ( -1.225000000000044276, 1.083333334016145066, 0.7072540797572517413 ) ) ;
#57723 = CARTESIAN_POINT ( 'NONE',  ( -10.12738493804958750, 3.691521601903835936, 6.358798186737252500 ) ) ;
#57724 = CARTESIAN_POINT ( 'NONE',  ( 6.685579144870162693, 6.972466221869550118, -0.7216878364870458196 ) ) ;
#57725 = CARTESIAN_POINT ( 'NONE',  ( -5.817857313595549584, 6.920493299683823096, 1.082531754730549078 ) ) ;
#57726 = EDGE_CURVE ( 'NONE', #73290, #4315, #180904, .T. ) ;
#57727 = CARTESIAN_POINT ( 'NONE',  ( 1.835461723582560767, 0.2275736305563350881, 2.296322244814374081 ) ) ;
#57728 = CARTESIAN_POINT ( 'NONE',  ( 3.262109210011232108, -1.959739898415867154, 0.09363895518171151677 ) ) ;
#57729 = DIRECTION ( 'NONE',  ( 0.000000000000000000, 0.000000000000000000, 1.000000000000000000 ) ) ;
#57730 = CARTESIAN_POINT ( 'NONE',  ( 6.227400143195995774, 0.1575970216860186346, -2.056636196940288652 ) ) ;
#57731 = CARTESIAN_POINT ( 'NONE',  ( 3.334942599281629949, 5.874221551595115720, -1.082531754730543083 ) ) ;
#57732 = CARTESIAN_POINT ( 'NONE',  ( 3.553118775233146120, 6.302999783484076524, -1.199719254218453823 ) ) ;
#57733 = ORIENTED_EDGE ( 'NONE', *, *, #59313, .F. ) ;
#57734 = CARTESIAN_POINT ( 'NONE',  ( 5.770720322323381168, -0.3006437417610394736, -1.993894057904864514 ) ) ;
#57735 = CARTESIAN_POINT ( 'NONE',  ( -8.134002093194872884, 11.57708731111429401, 1.199719254218453823 ) ) ;
#57736 = CARTESIAN_POINT ( 'NONE',  ( -10.50660484223216606, 5.359830900411396648, 5.105327592218940502 ) ) ;
#57738 =( GEOMETRIC_REPRESENTATION_CONTEXT ( 3 ) GLOBAL_UNCERTAINTY_ASSIGNED_CONTEXT ( ( #101339 ) ) GLOBAL_UNIT_ASSIGNED_CONTEXT ( ( #45689, #65088, #185235 ) ) REPRESENTATION_CONTEXT ( 'NONE', 'WORKASPACE' ) );
#57737 = CARTESIAN_POINT ( 'NONE',  ( 1.551893958816989993, 1.642325835523240629, 1.420010234424383455 ) ) ;
#57739 = DIRECTION ( 'NONE',  ( 0.000000000000000000, 1.000000000000000000, 0.000000000000000000 ) ) ;
#57740 = CARTESIAN_POINT ( 'NONE',  ( -1.402160292154681736E-14, 0.2437500006828163535, 1.732050807568877637 ) ) ;
#57741 = CARTESIAN_POINT ( 'NONE',  ( -11.86145016429273014, 10.19999999999999929, -1.100000000000000311 ) ) ;
#57742 = CARTESIAN_POINT ( 'NONE',  ( 5.323208952783781811, 7.729862296028469970, 1.309151360253474339 ) ) ;
#57743 = CARTESIAN_POINT ( 'NONE',  ( 0.7376602057446514094, -1.455437688833590926, -1.459210590049898171 ) ) ;
#57745 = CARTESIAN_POINT ( 'NONE',  ( 6.727182134110209155, 1.290711256955964448, 1.927001067762003972 ) ) ;
#57744 = DIRECTION ( 'NONE',  ( 0.000000000000000000, 0.000000000000000000, -1.000000000000000000 ) ) ;
#57746 = CARTESIAN_POINT ( 'NONE',  ( -0.6823417656250246877, 0.3010416670080895418, 1.181850606188755259 ) ) ;
#57747 = FACE_OUTER_BOUND ( 'NONE', #35768, .T. ) ;
#57748 = ORIENTED_EDGE ( 'NONE', *, *, #89709, .T. ) ;
#57749 = CARTESIAN_POINT ( 'NONE',  ( 3.404848115249804685, -0.3755933644018424888, -1.874856250562627391 ) ) ;
#57750 = CARTESIAN_POINT ( 'NONE',  ( 5.576936095668227900, -0.04655786065462656775, -1.769397458738901197 ) ) ;
#57751 = CARTESIAN_POINT ( 'NONE',  ( 7.035755370848908896, 7.173079118937375931, 0.7998128361456352531 ) ) ;
#57752 = CARTESIAN_POINT ( 'NONE',  ( -3.391510981712833939, 7.108513245306943062, 0.7998128361456341429 ) ) ;
#57754 = CARTESIAN_POINT ( 'NONE',  ( 6.603150280507321668, -0.1401627607961895561, 1.883980500587930429 ) ) ;
#57753 = CARTESIAN_POINT ( 'NONE',  ( -0.1263493754108893363, 6.487495393664095111, -3.100011470320000573 ) ) ;
#57755 = CARTESIAN_POINT ( 'NONE',  ( -0.7500000000000249800, -0.5583333333333134751, 1.299038105676659116 ) ) ;
#57756 = CARTESIAN_POINT ( 'NONE',  ( 0.6607010325807397555, -0.6960017893198193750, -1.950014918625786020 ) ) ;
#57757 = CARTESIAN_POINT ( 'NONE',  ( -1.402160292154681736E-14, -1.115624999658584082, 1.575800808251672791 ) ) ;
#57758 = CARTESIAN_POINT ( 'NONE',  ( 5.858239598252557911, 0.7595784280203803362, 1.709674162104061645 ) ) ;
#57759 = CARTESIAN_POINT ( 'NONE',  ( 2.648829494986388422, -1.517897411861212076, 1.014145048410304284 ) ) ;
#57761 = CARTESIAN_POINT ( 'NONE',  ( 6.124909263556299166, 6.992440323537196356, 0.9511531368890328020 ) ) ;
#57760 = CARTESIAN_POINT ( 'NONE',  ( 5.988949835885216011, -0.3198878037087344306, -2.183464699167809275 ) ) ;
#57762 = CARTESIAN_POINT ( 'NONE',  ( -0.6823417656250003738, 0.7177083336747519526, -1.181850606188749264 ) ) ;
#57763 = CARTESIAN_POINT ( 'NONE',  ( 2.822777196768213592, -1.424206252425799679, 1.492280444834346520 ) ) ;
#57764 = CARTESIAN_POINT ( 'NONE',  ( -6.201965203247477909, 9.323044272842313518, 1.199719254218452047 ) ) ;
#57765 = CARTESIAN_POINT ( 'NONE',  ( 9.901532256681887745, 10.44620914241737530, 0.000000000000000000 ) ) ;
#57766 = CARTESIAN_POINT ( 'NONE',  ( 5.678167406024951624, 5.518950149984223508, 0.7998128361456341429 ) ) ;
#57767 = CARTESIAN_POINT ( 'NONE',  ( 0.6148119136215323133, 1.491057340773978446, -1.565211586912764963 ) ) ;
#57768 = VECTOR ( 'NONE', #9639, 1000.000000000000000 ) ;
#57769 = CARTESIAN_POINT ( 'NONE',  ( 5.723117673755029777, -1.870111591731966616, -0.8886290660751752224 ) ) ;
#57770 = CARTESIAN_POINT ( 'NONE',  ( 0.6823417656249882723, 0.4885416670080827695, -1.181850606188749264 ) ) ;
#57771 = CARTESIAN_POINT ( 'NONE',  ( 3.655696586050953378, 0.5291108212043382775, -2.095698868369605616 ) ) ;
#57772 = CARTESIAN_POINT ( 'NONE',  ( -4.736138090107036902, 8.221507128720061175, -0.6901939221467829899 ) ) ;
#57774 = CARTESIAN_POINT ( 'NONE',  ( 2.224987305166142626, -1.792472147789250236, -0.7979012372742313453 ) ) ;
#57773 = CARTESIAN_POINT ( 'NONE',  ( 3.141275609595588492, 0.05172059693002092201, 2.019191109193402056 ) ) ;
#57777 = CARTESIAN_POINT ( 'NONE',  ( 7.158341918335438869, 7.453746447587225710, -0.7216878364870257245 ) ) ;
#57776 = CARTESIAN_POINT ( 'NONE',  ( -3.475000000000000533, -0.3791666666666649865, -2.006292185433948827 ) ) ;
#57775 = CARTESIAN_POINT ( 'NONE',  ( -1.225000000000014078, 1.479166666666654972, -0.7072540797573017013 ) ) ;
#57778 = CARTESIAN_POINT ( 'NONE',  ( -6.740338644649361832, 7.892758502626242567, -1.199719254218452047 ) ) ;
#57779 = CARTESIAN_POINT ( 'NONE',  ( 2.940638933469359895, -1.523795050681177710, 1.320827213682006285 ) ) ;
#57781 = SURFACE_STYLE_USAGE ( .BOTH. , #185629 ) ;
#57780 = CARTESIAN_POINT ( 'NONE',  ( -3.879604511804807032, 7.677955697080923514, 0.7998128361456341429 ) ) ;
#57782 = CARTESIAN_POINT ( 'NONE',  ( -1.500000000000011324, 5.410416667349489117, -0.8660254037844313801 ) ) ;
#57783 = CARTESIAN_POINT ( 'NONE',  ( 6.275647926998928483, 0.3200337115364470519, -1.885262484646981873 ) ) ;
#57784 = CARTESIAN_POINT ( 'NONE',  ( -11.94980361058168938, 12.70000000000000107, 1.099999999999996980 ) ) ;
#57785 = CARTESIAN_POINT ( 'NONE',  ( 5.219525951136835928, 7.112532914458205013, -1.443375672974051449 ) ) ;
#57787 = CARTESIAN_POINT ( 'NONE',  ( 3.726185550002871771, 2.006962945745351945, 0.1948219989877792990 ) ) ;
#57786 = CARTESIAN_POINT ( 'NONE',  ( -8.812436658758329600, 9.383523644747281622, 1.040834085586084257E-14 ) ) ;
#57788 = CARTESIAN_POINT ( 'NONE',  ( 1.499999999999987121, 3.545833333333356041, -0.8660254037844262731 ) ) ;
#57789 = CARTESIAN_POINT ( 'NONE',  ( -8.012344526598182026E-15, 13.35937500034140157, -1.575800808251669460 ) ) ;
#57790 = CARTESIAN_POINT ( 'NONE',  ( 5.877914075457827181, 1.031193140389017548, 1.382412309478407542 ) ) ;
#57791 = CARTESIAN_POINT ( 'NONE',  ( 5.851225812749518695, 8.984124660586543243, -1.199719254218452047 ) ) ;
#57792 = CARTESIAN_POINT ( 'NONE',  ( 8.812436659202669276, 10.34389285956704363, -1.082531754730543083 ) ) ;
#57793 = CARTESIAN_POINT ( 'NONE',  ( 10.99962150373186809, -9.919999999999998153, -0.09125116240079202135 ) ) ;
#57794 = CARTESIAN_POINT ( 'NONE',  ( 4.868341698904518289, -1.223052743625025141, 1.415352931214426846 ) ) ;
#57795 = CARTESIAN_POINT ( 'NONE',  ( -5.608757509018976961, 5.622941248444247364, -0.3933255993917709747 ) ) ;
#57796 = CIRCLE ( 'NONE', #130546, 0.07999999999999982125 ) ;
#57797 = CARTESIAN_POINT ( 'NONE',  ( 2.659107809384615884, 1.665393510391148801, -1.229642267604726058 ) ) ;
#57798 = CARTESIAN_POINT ( 'NONE',  ( 1.500000000000001332, 12.40625000068279427, 0.000000000000000000 ) ) ;
#57799 = ORIENTED_EDGE ( 'NONE', *, *, #212293, .F. ) ;
#57800 = CARTESIAN_POINT ( 'NONE',  ( 4.228163802615382494, 6.026220084508304708, -1.599625672291269396 ) ) ;
#57801 = SURFACE_SIDE_STYLE ('',( #24208 ) ) ;
#57802 = CARTESIAN_POINT ( 'NONE',  ( 0.3163054335677130680, -0.6107064426322272865, -1.705642966030767260 ) ) ;
#57803 = B_SPLINE_CURVE_WITH_KNOTS ( 'NONE', 3,
 ( #38616, #85218, #83075, #732 ),
 .UNSPECIFIED., .F., .F.,
 ( 4, 4 ),
 ( 0.000000000000000000, 0.002006572499523629795 ),
 .UNSPECIFIED. ) ;
#57804 = CARTESIAN_POINT ( 'NONE',  ( 4.055297343818933697, 5.824542549245813383, 1.443375672974058777 ) ) ;
#57805 = CARTESIAN_POINT ( 'NONE',  ( -0.3107038660269380026, -6.804704122739850369, -10.86205067566995375 ) ) ;
#57806 = EDGE_LOOP ( 'NONE', ( #185531, #34363 ) ) ;
#57807 = CARTESIAN_POINT ( 'NONE',  ( 9.101601193475611140, 9.512956235343358102, -0.7998128361456221525 ) ) ;
#57808 = CARTESIAN_POINT ( 'NONE',  ( 5.571877068885287443, -0.8567909204831600789, 1.713377365699362054 ) ) ;
#57809 = CARTESIAN_POINT ( 'NONE',  ( -11.52483635780546578, 13.87999991357544438, 3.345866325258015639 ) ) ;
#57811 = VERTEX_POINT ( 'NONE', #85193 ) ;
#57810 = CARTESIAN_POINT ( 'NONE',  ( 3.551873057100274789, 7.087676300018221021, 0.7216878364870298324 ) ) ;
#57812 = CARTESIAN_POINT ( 'NONE',  ( -7.293923454472094114, 9.532663335016016148, 1.443375672974090751 ) ) ;
#57813 = VECTOR ( 'NONE', #17365, 1000.000000000000000 ) ;
#57814 = CARTESIAN_POINT ( 'NONE',  ( 3.028364643526501698, 1.202066397148596977, -1.796461956351296019 ) ) ;
#57815 = CARTESIAN_POINT ( 'NONE',  ( -7.783789588021474692, 8.253711738879413673, 0.7216878364870317197 ) ) ;
#57816 = CARTESIAN_POINT ( 'NONE',  ( 4.065465959251388206, 5.836405933916976707, -1.599625672291269396 ) ) ;
#57817 = CARTESIAN_POINT ( 'NONE',  ( -0.05226516427493665962, -1.936187138999283297, 0.8653993394739032397 ) ) ;
#57818 = CARTESIAN_POINT ( 'NONE',  ( 5.315394819225006451, -0.2661953434012730435, 1.805952802178517613 ) ) ;
#57819 = CARTESIAN_POINT ( 'NONE',  ( 9.243398672612485711, 11.59071330704323799, 7.171203578799023148 ) ) ;
#57820 = CARTESIAN_POINT ( 'NONE',  ( 1.159376733683295191, 0.3886980088604417016, -1.932498344103703136 ) ) ;
#57821 = CARTESIAN_POINT ( 'NONE',  ( 3.498220628606643956, -0.9384276995785534314, 1.666209768436441419 ) ) ;
#57822 = ORIENTED_EDGE ( 'NONE', *, *, #81935, .T. ) ;
#57823 = CARTESIAN_POINT ( 'NONE',  ( -4.797639995575725180, 14.48151998940196883, -11.00824919010792158 ) ) ;
#57824 = CARTESIAN_POINT ( 'NONE',  ( 4.949637397294944563, 1.457986120030363431, 1.324331637980098675 ) ) ;
#57825 = EDGE_LOOP ( 'NONE', ( #126390, #67432, #126270, #25136, #66645, #213616 ) ) ;
#57826 = CARTESIAN_POINT ( 'NONE',  ( 6.128462272945822242, 0.1949450651400796986, 1.932269955005933904 ) ) ;
#57827 = ORIENTED_EDGE ( 'NONE', *, *, #179751, .F. ) ;
#57828 = CARTESIAN_POINT ( 'NONE',  ( -5.448397627845328550, 7.449826213943242514, 1.599625672291263179 ) ) ;
#57829 = CARTESIAN_POINT ( 'NONE',  ( -4.634908411025374875, 6.500755460986618495, 1.599625672291263179 ) ) ;
#57830 = B_SPLINE_CURVE_WITH_KNOTS ( 'NONE', 3,
 ( #19710, #6649, #186477, #168111, #90073, #187546 ),
 .UNSPECIFIED., .F., .F.,
 ( 4, 2, 4 ),
 ( 0.0006305064395556248327, 0.0009448735008584364763, 0.001259240562161248120 ),
 .UNSPECIFIED. ) ;
#57831 = CARTESIAN_POINT ( 'NONE',  ( 7.471952054462754234, 8.850270497362297206, 1.082531754730549078 ) ) ;
#57833 = VERTEX_POINT ( 'NONE', #131861 ) ;
#57832 = CARTESIAN_POINT ( 'NONE',  ( 4.143145976665215002, 0.09703654569752531711, 1.909951782607082427 ) ) ;
#57834 = CARTESIAN_POINT ( 'NONE',  ( 0.6400319944965120467, -1.562016764346199960, -1.559085968200937478 ) ) ;
#57835 = CARTESIAN_POINT ( 'NONE',  ( 7.681496476274699781, -5.295524846228401472, 7.873959529867727625 ) ) ;
#57836 = CARTESIAN_POINT ( 'NONE',  ( 6.445953599032193004, -1.316566896158730238, -1.522954124987923930 ) ) ;
#57837 = CARTESIAN_POINT ( 'NONE',  ( -3.147653791585956817, 8.919999999999845386, 2.419999999999999485 ) ) ;
#57838 = CARTESIAN_POINT ( 'NONE',  ( -1.420000000000001039, 7.176846818246207960, -4.202462424328208712 ) ) ;
#57839 = CARTESIAN_POINT ( 'NONE',  ( 1.662640112210824306, -0.7432673875312335587, -1.932532381715674097 ) ) ;
#57840 = CARTESIAN_POINT ( 'NONE',  ( -5.065942953000576843, 9.062017211809330064, -0.7998128361456231517 ) ) ;
#57841 = CARTESIAN_POINT ( 'NONE',  ( -5.122256578951685846, 7.813849795838854639, -1.152996464563345924 ) ) ;
#57842 = CARTESIAN_POINT ( 'NONE',  ( -6.391719147208884344, 6.567463349398176220, -2.438448605600926467 ) ) ;
#57843 = CARTESIAN_POINT ( 'NONE',  ( 6.148786358997489820, 7.132337826040578754, -1.199719254218446718 ) ) ;
#57844 = SURFACE_STYLE_FILL_AREA ( #206218 ) ;
#57845 = EDGE_CURVE ( 'NONE', #197886, #206340, #14105, .T. ) ;
#57846 = CARTESIAN_POINT ( 'NONE',  ( 4.746763178560254204, 6.631252689777363152, 1.443375672974065660 ) ) ;
#57847 = CARTESIAN_POINT ( 'NONE',  ( 0.1589091098076318986, -6.723650695528626819, 9.611540586923185359 ) ) ;
#57848 = CARTESIAN_POINT ( 'NONE',  ( 1.777638883463141806, 0.9165151389911742053, 1.199999999999999734 ) ) ;
#57849 = CARTESIAN_POINT ( 'NONE',  ( -0.6823417656250003738, 11.21354166700806765, 1.181850606188754593 ) ) ;
#57851 = CARTESIAN_POINT ( 'NONE',  ( -7.456058132872594335, 7.663432341298296535, 0.000000000000000000 ) ) ;
#57850 = CARTESIAN_POINT ( 'NONE',  ( 6.825078400183592464, 1.263193418084729958, 2.069194724180785538 ) ) ;
#57852 = EDGE_CURVE ( 'NONE', #84082, #14287, #59116, .T. ) ;
#57853 = CARTESIAN_POINT ( 'NONE',  ( 5.238767818816652877, 1.731821575490007703, -0.09270464131736801117 ) ) ;
#57854 = CARTESIAN_POINT ( 'NONE',  ( -6.064574784014443942, 5.969758757638621738, -0.7998128361456291469 ) ) ;
#57855 = CARTESIAN_POINT ( 'NONE',  ( 1.903268718874175480, -1.751121435885591548, 1.104011288380807532 ) ) ;
#57856 = CARTESIAN_POINT ( 'NONE',  ( 3.198929712650464996, 1.915108447241938627, 0.9030302060772307238 ) ) ;
#57857 = CARTESIAN_POINT ( 'NONE',  ( 6.100279051144945619, 9.204410428722734849, -1.199719254218440723 ) ) ;
#57858 = CARTESIAN_POINT ( 'NONE',  ( 0.3713344243775348885, 3.000000000000001776, 0.3713344243775348885 ) ) ;
#57859 = CARTESIAN_POINT ( 'NONE',  ( 1.498812192398508270, 0.3789717401675870567, 1.932455098789982895 ) ) ;
#57860 = CARTESIAN_POINT ( 'NONE',  ( 5.714115171586898079, 6.274818061858235652, 1.066218439657661721 ) ) ;
#57862 = DIRECTION ( 'NONE',  ( -0.9782075119097244364, 0.1245777785627091433, -0.1661037047502772757 ) ) ;
#57861 = CARTESIAN_POINT ( 'NONE',  ( -3.474999999999998312, -1.020833333333332815, 2.006292185433951047 ) ) ;
#57863 = CARTESIAN_POINT ( 'NONE',  ( 3.644716121489647076, -1.874467426877159504, 1.319156965210349197 ) ) ;
#57864 = CARTESIAN_POINT ( 'NONE',  ( 2.174178736149934732, -1.123764393468742906, 1.438770255985911684 ) ) ;
#57865 = CARTESIAN_POINT ( 'NONE',  ( 5.987861119090863049, 7.014868056141362551, 1.199719254218452047 ) ) ;
#57866 = CARTESIAN_POINT ( 'NONE',  ( 6.954969613686092345, 7.216478758829655504, -0.7216878364870257245 ) ) ;
#57867 = CARTESIAN_POINT ( 'NONE',  ( -8.342344591110322227, 8.627156865917170236, -0.7998128361456291469 ) ) ;
#57868 = CARTESIAN_POINT ( 'NONE',  ( 2.408449855729302591, -2.008082631278225616, -0.1440398445633188362 ) ) ;
#57869 = CARTESIAN_POINT ( 'NONE',  ( 3.379693149055284174, -1.891888713350448947, 0.5187481205842571219 ) ) ;
#57870 = CARTESIAN_POINT ( 'NONE',  ( -8.076906825439122528, 10.44614393447756129, -1.599625672291263179 ) ) ;
#57871 = TRIMMED_CURVE ( 'NONE', #135053, ( PARAMETER_VALUE ( 2.526112944919405301 ), #24326 ), ( PARAMETER_VALUE ( 3.141592653589793116 ), #55779 ), .T., .PARAMETER. ) ;
#57872 = CARTESIAN_POINT ( 'NONE',  ( -6.925517538482230506, 6.974191971184389160, 0.7998128361456341429 ) ) ;
#57873 = CARTESIAN_POINT ( 'NONE',  ( 0.07516593201273635838, 0.2333279341363985182, -2.077802470623245856 ) ) ;
#57875 = CARTESIAN_POINT ( 'NONE',  ( 4.680378828550276538, -1.717002404052007325, -0.4286406472287905278 ) ) ;
#57874 = CARTESIAN_POINT ( 'NONE',  ( 6.632766914392992597, -1.868179159523954302, 0.9385789683672930428 ) ) ;
#57876 = CARTESIAN_POINT ( 'NONE',  ( -1.225000000000045386, 2.250000000000001776, -4.683753385137379155E-14 ) ) ;
#57877 = CARTESIAN_POINT ( 'NONE',  ( 1.271705539736139423, 1.307743536042236920, 1.758333696453084016 ) ) ;
#57878 = CARTESIAN_POINT ( 'NONE',  ( 5.964775352603689740, 0.1210227373375266924, -1.736196924002187947 ) ) ;
#57879 = CARTESIAN_POINT ( 'NONE',  ( 6.968000882419564945, 10.21675256520979858, 1.199719254218460707 ) ) ;
#57880 = CARTESIAN_POINT ( 'NONE',  ( 4.260029445439537987, 7.236136616047151193, 2.419999999999999485 ) ) ;
#57881 = CARTESIAN_POINT ( 'NONE',  ( 0.1757712021154093640, -0.9832847084251387093, -2.074436467499872094 ) ) ;
#57882 = CARTESIAN_POINT ( 'NONE',  ( 0.1333692844072559280, 0.001398348041498076455, -2.053671342968105051 ) ) ;
#57883 = CARTESIAN_POINT ( 'NONE',  ( 5.114428339645875177, 0.5428861372157275378, -1.646692512460482982 ) ) ;
#57884 = CARTESIAN_POINT ( 'NONE',  ( 5.793482113768906316, -1.965262051535413335, 0.9231745368859373135 ) ) ;
#57885 = DIRECTION ( 'NONE',  ( 1.000000000000000000, 0.000000000000000000, 0.000000000000000000 ) ) ;
#57886 = CARTESIAN_POINT ( 'NONE',  ( 0.4447203898077173312, -1.529029696559053741, 1.464872618488068490 ) ) ;
#57887 = CARTESIAN_POINT ( 'NONE',  ( 3.062500000000001776, -1.451031289061242013, -1.451031289060994656 ) ) ;
#57888 = CARTESIAN_POINT ( 'NONE',  ( 6.827182134110196365, 7.629137130509086262, 2.689055895399253160 ) ) ;
#57889 = CARTESIAN_POINT ( 'NONE',  ( 4.383760159432283032, 1.257691660000469058, 1.459273733648867699 ) ) ;
#57890 = CARTESIAN_POINT ( 'NONE',  ( -0.7500000000000006661, 10.98958333401613174, -1.299038105676657340 ) ) ;
#57891 = CARTESIAN_POINT ( 'NONE',  ( 1.383751715516433833, 0.1588885597470449385, -2.215665637441687430 ) ) ;
#57892 = ORIENTED_EDGE ( 'NONE', *, *, #181856, .F. ) ;
#57893 = CARTESIAN_POINT ( 'NONE',  ( -0.7500000000000215383, 3.941666666666690411, 1.299038105676671107 ) ) ;
#57894 = CARTESIAN_POINT ( 'NONE',  ( 5.118366684358879759, 5.930181538962194132, 1.199719254218462483 ) ) ;
#57895 = CARTESIAN_POINT ( 'NONE',  ( 6.657217119509961201, 7.725507046638470321, -1.199719254218446718 ) ) ;
#57896 = CARTESIAN_POINT ( 'NONE',  ( 2.895431823567701457, -0.1657752626464791268, -2.215182847160178881 ) ) ;
#57897 = CARTESIAN_POINT ( 'NONE',  ( -7.510853912290736289, 11.70648729774046792, 0.7216878364870458196 ) ) ;
#57898 = CARTESIAN_POINT ( 'NONE',  ( 7.022760382198770301, 8.255937203062467589, -1.082531754730543083 ) ) ;
#57899 = CARTESIAN_POINT ( 'NONE',  ( -8.581948047326017459, 11.99572790764693409, 1.082531754730558626 ) ) ;
#57900 = CARTESIAN_POINT ( 'NONE',  ( 5.506019780925567986, 8.477421273504887722, -1.082531754730548412 ) ) ;
#57901 = VECTOR ( 'NONE', #56979, 1000.000000000000000 ) ;
#57902 = CARTESIAN_POINT ( 'NONE',  ( 1.090470458312575053, -0.4872005951904456733, 1.956561897242928172 ) ) ;
#57904 = CARTESIAN_POINT ( 'NONE',  ( 0.4794367124230074495, -0.1050040150484717050, 2.060039547518006664 ) ) ;
#57903 = CARTESIAN_POINT ( 'NONE',  ( 9.426996880203592610, 9.892584536526015881, -0.7998128361456281477 ) ) ;
#57905 = CYLINDRICAL_SURFACE ( 'NONE', #9272, 2.000000000000000000 ) ;
#57906 = CARTESIAN_POINT ( 'NONE',  ( 7.824464048418096951, 8.301165276008827476, -0.7216878364870317197 ) ) ;
#57907 = B_SPLINE_CURVE_WITH_KNOTS ( 'NONE', 3,
 ( #42459, #95485, #94410, #109646, #210247, #43524 ),
 .UNSPECIFIED., .F., .F.,
 ( 4, 2, 4 ),
 ( 0.000000000000000000, 0.0003845013059668464604, 0.0007690026119336929207 ),
 .UNSPECIFIED. ) ;
#57908 = CARTESIAN_POINT ( 'NONE',  ( -0.6823417656250212460, 2.551041667008084435, 1.181850606188767472 ) ) ;
#57909 = CARTESIAN_POINT ( 'NONE',  ( 1.071160155259534674, 1.707552549077664183, -0.4648152392626672680 ) ) ;
#57910 = CARTESIAN_POINT ( 'NONE',  ( 0.6861729220449981348, 1.650083401500940239, 1.158686392676591570 ) ) ;
#57911 = CARTESIAN_POINT ( 'NONE',  ( 0.2043192855987647494, 1.601443664334546213, 0.9084302959305108338 ) ) ;
#57912 = CARTESIAN_POINT ( 'NONE',  ( 3.843561273245421628, 0.7716866907857397040, -2.158722107141448188 ) ) ;
#57913 = CARTESIAN_POINT ( 'NONE',  ( 1.364683531249988757, -0.6156249996585803075, 0.000000000000000000 ) ) ;
#57914 = CARTESIAN_POINT ( 'NONE',  ( 1.991909005812149358, -0.4902695928585449892, -1.774584731258487036 ) ) ;
#57915 = ADVANCED_FACE ( 'NONE', ( #165378 ), #115094, .T. ) ;
#57916 = CARTESIAN_POINT ( 'NONE',  ( 9.694243528971124846, 11.26870452434320491, 1.199719254218450271 ) ) ;
#57917 = CARTESIAN_POINT ( 'NONE',  ( 11.88221712267702834, 7.173824839832926514, 1.903813004346444515 ) ) ;
#57918 = CARTESIAN_POINT ( 'NONE',  ( 3.030095697178539549, 1.015519584536026976, -1.516846343748608605 ) ) ;
#57919 = CARTESIAN_POINT ( 'NONE',  ( 4.166638809851969327, 1.319227567334404494, 1.525044649537968589 ) ) ;
#57920 = CARTESIAN_POINT ( 'NONE',  ( -8.469039510030723861, 13.03229652834454733, 1.040834085586084257E-14 ) ) ;
#57922 = DIRECTION ( 'NONE',  ( -0.000000000000000000, -1.000000000000000000, -0.000000000000000000 ) ) ;
#57921 = CARTESIAN_POINT ( 'NONE',  ( 3.151526295007577527, -1.848778841746369972, -1.303968314058404854 ) ) ;
#57923 = CARTESIAN_POINT ( 'NONE',  ( 5.086996280900090817, -0.2547426189827053378, -2.090417274992136587 ) ) ;
#57924 = CARTESIAN_POINT ( 'NONE',  ( 9.887462820343554171, 14.58581677083729566, 7.687850877847926867 ) ) ;
#57925 = CARTESIAN_POINT ( 'NONE',  ( 2.857943571468853250, -0.6518772230660694333, 1.965110387975615991 ) ) ;
#57926 = CARTESIAN_POINT ( 'NONE',  ( 3.246287715468270108, 5.874753870433235825, 1.199719254218450271 ) ) ;
#57927 = CARTESIAN_POINT ( 'NONE',  ( 1.360316468749989793, 0.5677083336747246189, -0.7853790794158941324 ) ) ;
#57928 = CARTESIAN_POINT ( 'NONE',  ( 5.057343377742961721, -1.818460011135439869, 1.090507627184752693 ) ) ;
#57929 = CONTEXT_DEPENDENT_SHAPE_REPRESENTATION ( #74081, #180407 ) ;
#57931 = CARTESIAN_POINT ( 'NONE',  ( 0.7153026426200872478, -0.2839029868492106701, 1.905349893463634814 ) ) ;
#57930 = CARTESIAN_POINT ( 'NONE',  ( -8.631737353394710155, 13.22211067893587533, 1.040834085586084257E-14 ) ) ;
#57932 = CARTESIAN_POINT ( 'NONE',  ( -4.305596300791617814, 7.180890229968955651, 1.199719254218452935 ) ) ;
#57933 = CARTESIAN_POINT ( 'NONE',  ( 7.574201371528760163, 11.98831870009225931, 1.040834085586084257E-14 ) ) ;
#57934 = CARTESIAN_POINT ( 'NONE',  ( 6.007671464186837618, 6.181573927739029806, 0.7216878364870328300 ) ) ;
#57935 = CARTESIAN_POINT ( 'NONE',  ( 4.301718403444327876, 7.219878030919558043, 0.9872997725082887088 ) ) ;
#57936 = CARTESIAN_POINT ( 'NONE',  ( 3.475000000000000533, -0.4812499990440831654, 0.000000000000000000 ) ) ;
#57937 = CARTESIAN_POINT ( 'NONE',  ( -4.416205349749324327, 6.175325546172740765, 1.599625672291267398 ) ) ;
#57938 = CARTESIAN_POINT ( 'NONE',  ( 0.4752230700786713169, -1.603524673181003779, 1.537559121520514660 ) ) ;
#57939 = CARTESIAN_POINT ( 'NONE',  ( 2.555815334374893943, 0.5629295958425766244, -2.029244372067032565 ) ) ;
#57940 = CARTESIAN_POINT ( 'NONE',  ( -4.248501033035892327, 6.049946853332221153, -1.599625672291271394 ) ) ;
#57941 = CARTESIAN_POINT ( 'NONE',  ( 8.938903350111612411, 9.323142084752035430, -0.7998128361456221525 ) ) ;
#57942 = CARTESIAN_POINT ( 'NONE',  ( 6.367989434593707365, -1.846973275860162467, 0.2267098040239327594 ) ) ;
#57943 = CARTESIAN_POINT ( 'NONE',  ( 8.111855979677986994, 8.358253485912799263, 1.040834085586084257E-14 ) ) ;
#57944 = EDGE_CURVE ( 'NONE', #154674, #123959, #111142, .T. ) ;
#57945 = CARTESIAN_POINT ( 'NONE',  ( -6.292392690518209264, 8.434487120394948079, -1.443375672974066548 ) ) ;
#57946 = CARTESIAN_POINT ( 'NONE',  ( -8.893785580884703279, 10.43879993486270585, 1.082531754730558626 ) ) ;
#57947 = CARTESIAN_POINT ( 'NONE',  ( -0.2046613956954954905, -0.1581703332043625232, -2.086340352340488646 ) ) ;
#57948 = DIRECTION ( 'NONE',  ( -8.638326563840814399E-31, 0.000000000000000000, -1.000000000000000000 ) ) ;
#57950 = CARTESIAN_POINT ( 'NONE',  ( 3.578520225191741844, 1.246510459297203610, -1.514941731618473009 ) ) ;
#57949 = CARTESIAN_POINT ( 'NONE',  ( -1.151774525698488676E-14, -0.6874999999999952260, 1.414508159514557439 ) ) ;
#57951 = CARTESIAN_POINT ( 'NONE',  ( 1.833122199354455972, 0.2117775504973731793, 2.151289291301178075 ) ) ;
#57953 = CARTESIAN_POINT ( 'NONE',  ( -5.565591498217608013, 6.214750235347503704, -0.9194985501971261188 ) ) ;
#57952 = CARTESIAN_POINT ( 'NONE',  ( -6.134138155540168391, 6.121192367743780949, 0.000000000000000000 ) ) ;
#57954 = CARTESIAN_POINT ( 'NONE',  ( -0.6823417656250212460, 1.551041667008083769, 1.181850606188755259 ) ) ;
#57955 = CARTESIAN_POINT ( 'NONE',  ( 3.064111502348449978, -1.608305157344312564, -0.6653965878143754953 ) ) ;
#57956 = CARTESIAN_POINT ( 'NONE',  ( 7.470179451449751262, 7.817556902887268677, 1.040834085586084257E-14 ) ) ;
#57957 = CARTESIAN_POINT ( 'NONE',  ( -11.82196040793749425, 4.889518425415825931, 4.884593937341564107 ) ) ;
#57958 = AXIS2_PLACEMENT_3D ( 'NONE', #40432, #191976, #108683 ) ;
#57959 = ORIENTED_EDGE ( 'NONE', *, *, #183332, .F. ) ;
#57960 = CARTESIAN_POINT ( 'NONE',  ( 2.143907462275076892, -0.09611812122205246056, -2.013924455302518624 ) ) ;
#57961 = CARTESIAN_POINT ( 'NONE',  ( 6.825078400183572036, 7.629137130509069387, 2.744348168701661095 ) ) ;
#57962 = FACE_OUTER_BOUND ( 'NONE', #81494, .T. ) ;
#57963 = CARTESIAN_POINT ( 'NONE',  ( 2.026188796938654946, 1.136581424768828397, -1.610674104117129302 ) ) ;
#57966 = ORIENTED_EDGE ( 'NONE', *, *, #103791, .T. ) ;
#57965 = EDGE_CURVE ( 'NONE', #170226, #159704, #10002, .T. ) ;
#57964 = CARTESIAN_POINT ( 'NONE',  ( -5.478903473698268023, 5.564677938835638216, -0.7216878364870338292 ) ) ;
#57967 = STYLED_ITEM ( 'NONE', ( #176501 ), #146923 ) ;
#57968 = CARTESIAN_POINT ( 'NONE',  ( -6.468648687051513413, 7.679749902049126220, 1.082531754730549078 ) ) ;
#57969 = CARTESIAN_POINT ( 'NONE',  ( 5.200434439293556643, 8.224868058221247225, -1.199719254218452047 ) ) ;
#57970 = CARTESIAN_POINT ( 'NONE',  ( -7.144220599758281054, 7.299621885998258897, 0.7998128361456341429 ) ) ;
#57971 = CARTESIAN_POINT ( 'NONE',  ( 2.631515421131935817, -0.1955963300145530936, 2.010161875231412765 ) ) ;
#57972 = LINE ( 'NONE', #88349, #118308 ) ;
#57973 = ADVANCED_FACE ( 'NONE', ( #199996 ), #32157, .T. ) ;
#57974 = CARTESIAN_POINT ( 'NONE',  ( 5.385860071389879877, 1.544758419828775153, 1.714431625121175751 ) ) ;
#57975 = CARTESIAN_POINT ( 'NONE',  ( 6.883263157960391787, -0.001104538646235289417, 1.946037152736757925 ) ) ;
#57976 = CARTESIAN_POINT ( 'NONE',  ( 2.500770564479499303, 0.4249116886347775179, 1.915039037836663738 ) ) ;
#57977 = CARTESIAN_POINT ( 'NONE',  ( 9.759171643738394408, 10.28012176064996197, 0.000000000000000000 ) ) ;
#57978 = CARTESIAN_POINT ( 'NONE',  ( 0.9146856577476671912, -1.281363086869342194, -1.556907195799726917 ) ) ;
#57979 = ORIENTED_EDGE ( 'NONE', *, *, #39637, .F. ) ;
#57980 = CARTESIAN_POINT ( 'NONE',  ( 2.061849949441786123, 1.306762352624482038, 1.665877332585569803 ) ) ;
#57982 = CARTESIAN_POINT ( 'NONE',  ( -6.775324078527193983, 8.927630729746953264, -1.599625672291263179 ) ) ;
#57981 = CARTESIAN_POINT ( 'NONE',  ( -4.485049888022365927, 4.126979712314507331, 0.7998128361456341429 ) ) ;
#57983 = CARTESIAN_POINT ( 'NONE',  ( 2.114959233223293822, -1.785989328681826027, 0.4467204754193611627 ) ) ;
#57984 = VERTEX_POINT ( 'NONE', #204669 ) ;
#57985 = CARTESIAN_POINT ( 'NONE',  ( -8.462260433223891098, 13.02438760540324481, -0.7998128361456281477 ) ) ;
#57986 = CARTESIAN_POINT ( 'NONE',  ( 9.904948225507595794, 11.51217390914785099, 6.696207100445890070 ) ) ;
#57987 = CARTESIAN_POINT ( 'NONE',  ( 2.865608904542978674, -1.736054085904148669, -1.217558864107195715 ) ) ;
#57988 = CARTESIAN_POINT ( 'NONE',  ( 0.4273693582952375891, 0.9489586001507933632, -1.577591209259328275 ) ) ;
#57989 = CARTESIAN_POINT ( 'NONE',  ( -1.500000000000011324, 5.660416667349481123, -0.8660254037844313801 ) ) ;
#57990 = CARTESIAN_POINT ( 'NONE',  ( 8.288111976655649471, 8.563885482386732306, -0.7998128361456291469 ) ) ;
#57991 = CARTESIAN_POINT ( 'NONE',  ( 7.147083253059300922, 8.367293879104554577, 1.199719254218452935 ) ) ;
#57992 = CARTESIAN_POINT ( 'NONE',  ( 4.270816029187285423, -1.921422972303673093, -0.7454010919232464394 ) ) ;
#57994 = CARTESIAN_POINT ( 'NONE',  ( 1.364538772237647413, 0.1349417713633893900, -1.836341338755695940 ) ) ;
#57993 = CARTESIAN_POINT ( 'NONE',  ( -6.204827856548512877, 10.39071626594860476, -0.7998128361456291469 ) ) ;
#57995 = CARTESIAN_POINT ( 'NONE',  ( -1.001543065824772872E-14, 4.821875000341419693, 1.575800808251672791 ) ) ;
#57996 = CARTESIAN_POINT ( 'NONE',  ( 9.428250952287722697, 13.54490846161957585, -7.423481931054030092 ) ) ;
#57997 = DIRECTION ( 'NONE',  ( 1.000000000000000000, -0.000000000000000000, 1.224646799147353207E-16 ) ) ;
#57998 = CARTESIAN_POINT ( 'NONE',  ( 1.260703874955213744, 0.8971468365699288849, 2.016480257658866737 ) ) ;
#57999 = CARTESIAN_POINT ( 'NONE',  ( 3.497619258099498030, 1.781045823846095111, 1.394991416339389501 ) ) ;
#58000 = CARTESIAN_POINT ( 'NONE',  ( -7.212574532790087645, 11.35849468832304154, -0.7216878364870267237 ) ) ;
#58001 = CARTESIAN_POINT ( 'NONE',  ( 3.691515636560299463, 1.703854809669336001, -0.6157217382992925536 ) ) ;
#58002 = CARTESIAN_POINT ( 'NONE',  ( 3.028439059693835311, 0.4704065786719989761, 1.856910451861475631 ) ) ;
#58003 = CARTESIAN_POINT ( 'NONE',  ( 3.947765587739564097, 1.497496809916948779, 1.429883829622953462 ) ) ;
#58004 = CARTESIAN_POINT ( 'NONE',  ( 1.364683531249990311, 2.696875000341415696, 1.214306433183764966E-14 ) ) ;
#58005 = CARTESIAN_POINT ( 'NONE',  ( 2.518385046665332361, 1.288922565979855994, -1.491834565112426070 ) ) ;
#58006 = CARTESIAN_POINT ( 'NONE',  ( 0.8680396935916842027, 0.9469273490957976769, 1.677514697326354387 ) ) ;
#58007 = CARTESIAN_POINT ( 'NONE',  ( 3.467518583331068438, 1.825290416974333807, -0.4087457676540603990 ) ) ;
#58008 = CARTESIAN_POINT ( 'NONE',  ( 2.227567673948157800, 0.002208658356158287820, 2.307868969919598889 ) ) ;
#58009 = CARTESIAN_POINT ( 'NONE',  ( 3.578407426278474190, 1.182412371022481645, -1.437126236693661241 ) ) ;
#58010 = CARTESIAN_POINT ( 'NONE',  ( -1.201851678989727383E-14, 4.946875000341420581, -1.575800808251660134 ) ) ;
#58011 = CARTESIAN_POINT ( 'NONE',  ( -5.271422797614987665, 5.044414773505913274, -0.7998128361456221525 ) ) ;
#58012 = CARTESIAN_POINT ( 'NONE',  ( 7.474622759835693131, 7.614814729430110951, -0.7998128361456281477 ) ) ;
#58013 = CARTESIAN_POINT ( 'NONE',  ( 11.04984958223792368, 9.990824862318733679, 1.056557932048283188 ) ) ;
#58014 =( BOUNDED_CURVE ( )  B_SPLINE_CURVE ( 2, ( #201396, #167861, #105007, #136443, #185153, #103936, #151624 ),
 .UNSPECIFIED., .F., .T. ) 
 B_SPLINE_CURVE_WITH_KNOTS ( ( 3, 2, 2, 3 ),
 ( 0.3962798098108560874, 0.3988095238095238360, 0.4047619047619047672, 0.4072916187605725158 ),
 .UNSPECIFIED. ) 
 CURVE ( )  GEOMETRIC_REPRESENTATION_ITEM ( )  RATIONAL_B_SPLINE_CURVE ( ( 0.9345202395942615592, 0.9430618748659230777, 1.000000000000000000, 0.8660254037844387076, 1.000000000000000000, 0.9430618748659225226, 0.9345202395942613371 ) ) 
 REPRESENTATION_ITEM ( '' )  );
#58015 = CARTESIAN_POINT ( 'NONE',  ( 0.2937649352797070401, 1.562083697590540998, 1.412785709394439815 ) ) ;
#58016 = CARTESIAN_POINT ( 'NONE',  ( 3.348500752450937590, 5.890039396959305229, 1.082531754730558626 ) ) ;
#58018 = CARTESIAN_POINT ( 'NONE',  ( 5.048745089568936528, 4.904218937602238704, 0.2966393288263181605 ) ) ;
#58017 = CARTESIAN_POINT ( 'NONE',  ( -0.6823417656249969321, 3.530208333674754506, -1.181850606188749264 ) ) ;
#58019 = CARTESIAN_POINT ( 'NONE',  ( 6.784453917077649443, -2.118420112955111456, -0.4290502581522498415 ) ) ;
#58020 = CARTESIAN_POINT ( 'NONE',  ( 1.600013431492643745, 1.466117565985028515, 1.532352819790145482 ) ) ;
#58021 = CARTESIAN_POINT ( 'NONE',  ( 0.2639333133152200750, 0.6296502125625064172, -1.919233096100453118 ) ) ;
#58022 = CARTESIAN_POINT ( 'NONE',  ( -1.201851678989727383E-14, 1.321875000341419248, 1.575800808251672791 ) ) ;
#58023 = CARTESIAN_POINT ( 'NONE',  ( -4.528060117284246289, 6.305822774963486310, 1.443375672974064550 ) ) ;
#58024 = CARTESIAN_POINT ( 'NONE',  ( 5.834086172582112262, 5.700855377634248100, 1.040834085586084257E-14 ) ) ;
#58025 = CARTESIAN_POINT ( 'NONE',  ( 1.388190569347878212, -0.9732202972718406730, 1.930209198840258100 ) ) ;
#58028 = CARTESIAN_POINT ( 'NONE',  ( 3.172244755917638770, 5.684407401003788607, -1.082531754730543083 ) ) ;
#58027 = CARTESIAN_POINT ( 'NONE',  ( 6.925078400183553029, 0.5781763343528348864, 2.007479843201316783 ) ) ;
#58026 = CARTESIAN_POINT ( 'NONE',  ( 4.899292406491845497, 6.809203455697518947, -1.599625672291273171 ) ) ;
#58029 = CARTESIAN_POINT ( 'NONE',  ( -5.002032328799064231, 4.800402236545811441, -0.7998128361456362523 ) ) ;
#58030 = CARTESIAN_POINT ( 'NONE',  ( 5.331267653506235327, -1.592659417495114083, -1.236803018183525449 ) ) ;
#58032 = CARTESIAN_POINT ( 'NONE',  ( -4.597623488365601752, 8.377994813152914944, 0.7216878364870267237 ) ) ;
#58031 = CARTESIAN_POINT ( 'NONE',  ( -8.324343129110692630, 12.65555805069709550, 0.7216878364870338292 ) ) ;
#58033 = DIRECTION ( 'NONE',  ( 1.224646799147343346E-16, 0.000000000000000000, 1.000000000000000000 ) ) ;
#58035 = CARTESIAN_POINT ( 'NONE',  ( 1.364683531250000748, 10.75520833367473195, -0.7879004041258355073 ) ) ;
#58034 = CARTESIAN_POINT ( 'NONE',  ( 0.4798239446817476606, 2.109833986122396254, -0.8175194613929820386 ) ) ;
#58036 = CARTESIAN_POINT ( 'NONE',  ( -10.89183506715999883, 4.909321371462038286, 5.036854565707436393 ) ) ;
#58038 = CARTESIAN_POINT ( 'NONE',  ( 0.01699859406821546334, -1.751214827781864436, 0.7768474416505846136 ) ) ;
#58037 = CARTESIAN_POINT ( 'NONE',  ( -5.138177029454855216, 7.017625839162543677, 1.443375672974064550 ) ) ;
#58039 = CARTESIAN_POINT ( 'NONE',  ( -0.6823417656250212460, 0.8635416670080899859, 1.181850606188755259 ) ) ;
#58040 = CARTESIAN_POINT ( 'NONE',  ( -6.663994888585885512, -7.154544010627095219, 6.770610912236877610 ) ) ;
#58041 = CARTESIAN_POINT ( 'NONE',  ( 1.438722679664439452, 7.870294296420976110, 3.684004759497596204 ) ) ;
#58042 = CARTESIAN_POINT ( 'NONE',  ( 3.422183312176851455, 1.093272757541150719, -1.334144266598129791 ) ) ;
#58043 = CARTESIAN_POINT ( 'NONE',  ( 3.627688620108284745, 6.389997935838436227, 1.199719254218452047 ) ) ;
#58044 = CARTESIAN_POINT ( 'NONE',  ( 6.866278450678116485, 6.975356045404744521, 0.000000000000000000 ) ) ;
#58045 = CARTESIAN_POINT ( 'NONE',  ( 1.405125766016354305, -0.4367768486257683769, 1.714848201936822525 ) ) ;
#58046 = CARTESIAN_POINT ( 'NONE',  ( 1.576815760046655912, -1.422047136828644476, 1.425140908648862448 ) ) ;
#58047 = FACE_OUTER_BOUND ( 'NONE', #193438, .T. ) ;
#58048 = CARTESIAN_POINT ( 'NONE',  ( 4.243358471946375943, -1.921622210924242458, 1.084848892642875429 ) ) ;
#58049 = CONICAL_SURFACE ( 'NONE', #92711, 10.99999999999999112, 0.7853981633974425058 ) ;
#58050 = EDGE_LOOP ( 'NONE', ( #77209, #145686, #206456, #3934 ) ) ;
#58051 = CARTESIAN_POINT ( 'NONE',  ( 7.822691444960700125, 10.14955932391940330, -1.443375672974058777 ) ) ;
#58053 = CARTESIAN_POINT ( 'NONE',  ( 2.987907820627898392, -2.013986125068282007, 0.1017690403029153784 ) ) ;
#58052 = CARTESIAN_POINT ( 'NONE',  ( 4.389387035479824561, -0.001039498178659337352, -2.120667954306009406 ) ) ;
#58055 = ORIENTED_EDGE ( 'NONE', *, *, #104082, .F. ) ;
#58054 = CARTESIAN_POINT ( 'NONE',  ( 3.181707836761258790, 1.766318828868058910, -0.4016052188219875752 ) ) ;
#58056 = CARTESIAN_POINT ( 'NONE',  ( 5.468734858265785093, 7.473552982767158070, 1.599625672291269396 ) ) ;
#58057 = ORIENTED_EDGE ( 'NONE', *, *, #100659, .F. ) ;
#58058 = CARTESIAN_POINT ( 'NONE',  ( 1.727212824277712944, -1.762453432929488528, 0.6273722324065673650 ) ) ;
#58059 = AXIS2_PLACEMENT_3D ( 'NONE', #142986, #48659, #195973 ) ;
#58060 = CARTESIAN_POINT ( 'NONE',  ( 6.340460056601358474, 1.806591233369018834, 0.2625940548972791611 ) ) ;
#58062 = CARTESIAN_POINT ( 'NONE',  ( 2.360426208626884570, -1.834515764125169257, -0.5519355525325749801 ) ) ;
#58061 = DIRECTION ( 'NONE',  ( 0.000000000000000000, 0.000000000000000000, -1.000000000000000000 ) ) ;
#58064 = CIRCLE ( 'NONE', #33934, 0.08000000000000050127 ) ;
#58063 = AXIS2_PLACEMENT_3D ( 'NONE', #38660, #105830, #156689 ) ;
#58065 = CARTESIAN_POINT ( 'NONE',  ( 1.270904146967303028, 3.246556430829583118, 0.7750000000000135669 ) ) ;
#58066 = CARTESIAN_POINT ( 'NONE',  ( 1.734723475976807094E-15, 0.2401923788623739342, 3.469446951953614189E-15 ) ) ;
#58067 = CARTESIAN_POINT ( 'NONE',  ( 1.364683531249988757, 1.696875000341414808, 0.000000000000000000 ) ) ;
#58068 =( LENGTH_UNIT ( ) NAMED_UNIT ( * ) SI_UNIT ( .MILLI., .METRE. ) );
#58069 = CARTESIAN_POINT ( 'NONE',  ( 5.560252395380198998, 9.501061871336672127, 0.7216878364870317197 ) ) ;
#58070 = CARTESIAN_POINT ( 'NONE',  ( -3.336715202739028552, 6.906935146588564223, 0.7216878364870338292 ) ) ;
#58071 = CARTESIAN_POINT ( 'NONE',  ( -7.774674742793745708, 8.035151719539642912, 0.7998128361456341429 ) ) ;
#58072 = CARTESIAN_POINT ( 'NONE',  ( 4.588201236890728119, 1.223260742344203900, 1.732012071221388450 ) ) ;
#58073 = EDGE_CURVE ( 'NONE', #174805, #85120, #109407, .T. ) ;
#58075 = CARTESIAN_POINT ( 'NONE',  ( -10.78552488895401318, 8.017604977416297629, -4.042330561003328881 ) ) ;
#58074 = CARTESIAN_POINT ( 'NONE',  ( -0.1296875068448159474, 0.7431874094961619104, -1.910093690679348200 ) ) ;
#58076 = CARTESIAN_POINT ( 'NONE',  ( 3.901606001822624403, -0.5752225463674947026, 1.885544661340606165 ) ) ;
#58077 = CARTESIAN_POINT ( 'NONE',  ( 0.2639318008525155523, 0.6274397771241714272, -1.913028341257965170 ) ) ;
#58078 = EDGE_LOOP ( 'NONE', ( #41981, #125831, #152772, #27462 ) ) ;
#58079 = CARTESIAN_POINT ( 'NONE',  ( 0.3865160979802947927, -0.7177084582802439883, -1.991989965223327275 ) ) ;
#58080 = SURFACE_SIDE_STYLE ('',( #43986 ) ) ;
#58081 = CARTESIAN_POINT ( 'NONE',  ( 1.311079954825690619, -1.633285661836245906, 1.272233187909928454 ) ) ;
#58082 = CARTESIAN_POINT ( 'NONE',  ( 7.018280793729500644, 8.217024343219755167, -1.199719254218452047 ) ) ;
#58083 = ORIENTED_EDGE ( 'NONE', *, *, #38859, .T. ) ;
#58084 = CARTESIAN_POINT ( 'NONE',  ( 5.611095471209277541, 7.639640364534566075, 1.599625672291268286 ) ) ;
#58085 = CARTESIAN_POINT ( 'NONE',  ( 7.550965208168244125, 7.774157262476569130, -0.7998128361456341429 ) ) ;
#58087 = CARTESIAN_POINT ( 'NONE',  ( 5.854423403002611437, 5.724582146458163656, 1.040834085586084257E-14 ) ) ;
#58086 = CARTESIAN_POINT ( 'NONE',  ( 3.943374907373353278, 0.7044166278388838132, -1.968527102906494575 ) ) ;
#58088 = CARTESIAN_POINT ( 'NONE',  ( 6.933015448541703485, 9.181880338089085214, 1.599625672291268286 ) ) ;
#58091 = ORIENTED_EDGE ( 'NONE', *, *, #186328, .F. ) ;
#58090 = CARTESIAN_POINT ( 'NONE',  ( 0.7678511737040129015, 1.809490520450097284, -0.08760732307166485544 ) ) ;
#58089 = CARTESIAN_POINT ( 'NONE',  ( 2.379681254797087586, 1.121034037677430595, 1.440765146680768272 ) ) ;
#58092 = CARTESIAN_POINT ( 'NONE',  ( 5.883472226557854512, 2.040502603023553796, -0.8411249186189363458 ) ) ;
#58093 = CARTESIAN_POINT ( 'NONE',  ( -0.3793797362570683895, -6.699757570937928008, -10.99387514841215641 ) ) ;
#58094 = CARTESIAN_POINT ( 'NONE',  ( 3.803933094734159415, -0.6430795383850876901, 2.110982628114480786 ) ) ;
#58095 = CARTESIAN_POINT ( 'NONE',  ( 7.741869408603235136, 8.990934717247309749, 1.199719254218462483 ) ) ;
#58096 = DIRECTION ( 'NONE',  ( 0.000000000000000000, 0.000000000000000000, -1.000000000000000000 ) ) ;
#58097 = CARTESIAN_POINT ( 'NONE',  ( 2.666550042863625958, 0.6461651886627232111, 1.799920402468312197 ) ) ;
#58098 = AXIS2_PLACEMENT_3D ( 'NONE', #15967, #151346, #147084 ) ;
#58099 =( BOUNDED_CURVE ( )  B_SPLINE_CURVE ( 2, ( #23700, #108233, #174258, #203498, #186197 ),
 .UNSPECIFIED., .F., .T. ) 
 B_SPLINE_CURVE_WITH_KNOTS ( ( 3, 2, 3 ),
 ( 0.1113702160535958441, 0.1125000000000000028, 0.1138193015819520398 ),
 .UNSPECIFIED. ) 
 CURVE ( )  GEOMETRIC_REPRESENTATION_ITEM ( )  RATIONAL_B_SPLINE_CURVE ( ( 0.9470460506485149921, 0.9636730364727230658, 1.000000000000000000, 0.9575793047851419715, 0.9420221409164282189 ) ) 
 REPRESENTATION_ITEM ( '' )  );
#58100 = CARTESIAN_POINT ( 'NONE',  ( 8.075853055234393452, 12.57357899774884658, 0.7998128361456462443 ) ) ;
#58101 = CARTESIAN_POINT ( 'NONE',  ( 5.301260566756325510, -1.777534899005998481, 1.061244097098137829 ) ) ;
#58103 = CARTESIAN_POINT ( 'NONE',  ( 2.501032641837992454, 1.736685530831501456, -1.287010829427559289 ) ) ;
#58102 = CARTESIAN_POINT ( 'NONE',  ( 1.523896559881090074, 8.692074762372739016, -2.522933744808672163 ) ) ;
#58104 = CARTESIAN_POINT ( 'NONE',  ( 5.847271748948593029, 0.6375361197438635941, -2.096799129279611762 ) ) ;
#58105 = ORIENTED_EDGE ( 'NONE', *, *, #157474, .F. ) ;
#58107 = EDGE_CURVE ( 'NONE', #93276, #24495, #194095, .T. ) ;
#58106 = CIRCLE ( 'NONE', #106558, 10.92874649719719571 ) ;
#58108 = CARTESIAN_POINT ( 'NONE',  ( -9.532262708098283355, -8.048696291100942091, 0.1899713450103325540 ) ) ;
#58109 = CARTESIAN_POINT ( 'NONE',  ( -0.1132184859782652403, 3.829867255648767621, 11.66962136008045192 ) ) ;
#58110 = CARTESIAN_POINT ( 'NONE',  ( 3.711900195091365262, 7.552577004240394132, -0.7998128361456362523 ) ) ;
#58111 = CARTESIAN_POINT ( 'NONE',  ( -3.285556943750000070, -1.946874999522042682, 0.000000000000000000 ) ) ;
#58112 = EDGE_CURVE ( 'NONE', #49891, #143955, #25910, .T. ) ;
#58113 = CARTESIAN_POINT ( 'NONE',  ( -8.080296364064746939, 9.489729181906076505, 1.082531754730558626 ) ) ;
#58114 = CARTESIAN_POINT ( 'NONE',  ( 4.603875680292229156, 7.528882839386387360, 1.199719254218452047 ) ) ;
#58115 = CARTESIAN_POINT ( 'NONE',  ( 6.086797785588474063, 1.993605056338519699, 0.5577928598018768724 ) ) ;
#58116 = CARTESIAN_POINT ( 'NONE',  ( 4.512281715141372551, -0.8252044610495885557, -1.740951444232276657 ) ) ;
#58117 = CARTESIAN_POINT ( 'NONE',  ( 6.450787963126683344, -1.935726721829626351, -0.8580517621625349811 ) ) ;
#58118 = FILL_AREA_STYLE ('',( #74374 ) ) ;
#58119 = CARTESIAN_POINT ( 'NONE',  ( 3.573456005653643519, 6.326726552307992080, -1.199719254218453823 ) ) ;
#58120 = CARTESIAN_POINT ( 'NONE',  ( -5.426287360647527258, 6.306760859481674864, -1.047964138152550406 ) ) ;
#58121 = CARTESIAN_POINT ( 'NONE',  ( 0.2874129202556953144, 1.626693421326959710, 1.468627725614686463 ) ) ;
#58122 = CARTESIAN_POINT ( 'NONE',  ( 5.039593146249601752, -1.293522693445445793, -1.288650932716684627 ) ) ;
#58123 = CARTESIAN_POINT ( 'NONE',  ( 6.712695452541852070, 7.004101914153185504, 0.000000000000000000 ) ) ;
#58124 = CARTESIAN_POINT ( 'NONE',  ( 4.989037339704528229, 4.922891105851139315, 1.040834085586084257E-14 ) ) ;
#58125 = EDGE_CURVE ( 'NONE', #186548, #74610, #31461, .T. ) ;
#58126 = CARTESIAN_POINT ( 'NONE',  ( -5.143339171537843590, 7.093924681584509173, 1.599625672291263179 ) ) ;
#58127 = CARTESIAN_POINT ( 'NONE',  ( 3.691562964670865199, 7.528850235416478576, -0.7998128361456362523 ) ) ;
#58128 = ORIENTED_EDGE ( 'NONE', *, *, #89674, .T. ) ;
#58130 = CARTESIAN_POINT ( 'NONE',  ( 6.381113974719265336, -1.842344568942927419, -0.8120077521172417434 ) ) ;
#58129 = CARTESIAN_POINT ( 'NONE',  ( 2.190726087351921425, 1.424366561657765207, 1.166803476217087576 ) ) ;
#58131 = CARTESIAN_POINT ( 'NONE',  ( 0.7030180566853957425, -1.627119059678893587, -1.623510667393740725 ) ) ;
#58132 = CARTESIAN_POINT ( 'NONE',  ( 6.315287901512626867, -1.680818388338392699, -1.011408691396285420 ) ) ;
#58133 = CARTESIAN_POINT ( 'NONE',  ( -4.530395885260773525, 8.437212299446219532, 0.7998128361456481317 ) ) ;
#58134 = CARTESIAN_POINT ( 'NONE',  ( 9.513083153069256781, -8.198316282515564879, 9.269928574751062911E-15 ) ) ;
#58135 = CARTESIAN_POINT ( 'NONE',  ( -4.457933580795036654, 4.095344020549286590, -0.7998128361456221525 ) ) ;
#58136 = CARTESIAN_POINT ( 'NONE',  ( 0.5903903138861701372, 1.065687334306382184, -1.774900233272216798 ) ) ;
#58137 = CARTESIAN_POINT ( 'NONE',  ( -4.767627293860968507, 5.591261926706423857, -1.199719254218453823 ) ) ;
#58139 = CARTESIAN_POINT ( 'NONE',  ( 1.410794581852807150, 1.648159533202856686, 0.8848386531258023435 ) ) ;
#58138 = CARTESIAN_POINT ( 'NONE',  ( 2.331682703721962291, 0.9828498176551370147, -1.845303212725694975 ) ) ;
#58140 = CARTESIAN_POINT ( 'NONE',  ( 1.546249734355091388, 1.863884247081739609, -0.7690006294575402190 ) ) ;
#58141 = CARTESIAN_POINT ( 'NONE',  ( 7.605760987586388744, 11.81721221891873697, 1.040834085586084257E-14 ) ) ;
#58142 = ORIENTED_EDGE ( 'NONE', *, *, #80217, .F. ) ;
#58143 = CARTESIAN_POINT ( 'NONE',  ( 1.364683531249990311, 4.676041667008083103, 0.7879004041258499402 ) ) ;
#58144 = CARTESIAN_POINT ( 'NONE',  ( 2.454330514505886018, -1.515118085899306521, -0.8562798468515414596 ) ) ;
#58145 = AXIS2_PLACEMENT_3D ( 'NONE', #136340, #168820, #185052 ) ;
#58146 = CARTESIAN_POINT ( 'NONE',  ( 4.313465427442102929, 8.184126765324453601, 0.7998128361456462443 ) ) ;
#58148 = CARTESIAN_POINT ( 'NONE',  ( 1.561525566895185957, 8.688907412369037075, 2.501944002935413192 ) ) ;
#58147 = DIRECTION ( 'NONE',  ( -7.387867266669436732E-31, 1.000000000000000000, 8.546850786086424434E-32 ) ) ;
#58149 = CARTESIAN_POINT ( 'NONE',  ( 2.842114037233371082, 1.711851238368550909, 0.2109339381748502329 ) ) ;
#58150 = CARTESIAN_POINT ( 'NONE',  ( 3.228257827484398490, 2.138632370135685523, 0.4780590757816546854 ) ) ;
#58151 = CARTESIAN_POINT ( 'NONE',  ( 4.987059637548557411, -0.2676712469649074055, -2.190530366034774801 ) ) ;
#58152 = CARTESIAN_POINT ( 'NONE',  ( -10.40894566972866286, 4.029202461753065734, -7.241727701387177696 ) ) ;
#58153 = CARTESIAN_POINT ( 'NONE',  ( 2.290094988384860919, -1.415387839477784571, -1.646397135256922661 ) ) ;
#58154 = CARTESIAN_POINT ( 'NONE',  ( 1.224926655537651676, -0.04696546880481740349, 1.825250005322680780 ) ) ;
#58155 = CARTESIAN_POINT ( 'NONE',  ( 3.714152660773429648, 1.129254856714853261, -1.790882643308453703 ) ) ;
#58156 = CARTESIAN_POINT ( 'NONE',  ( 6.539320575229292665, 7.052829955583200139, 2.594893642179775028 ) ) ;
#58157 = VERTEX_POINT ( 'NONE', #61645 ) ;
#58158 = CIRCLE ( 'NONE', #85832, 6.249999999999995559 ) ;
#58160 = CARTESIAN_POINT ( 'NONE',  ( -1.201851678989727383E-14, 1.134375000341418582, 1.575800808251672791 ) ) ;
#58159 = CARTESIAN_POINT ( 'NONE',  ( 4.054423531099146771, -1.698574802010197837, 1.539571537138052948 ) ) ;
#58161 = CARTESIAN_POINT ( 'NONE',  ( 6.856061878569608298E-15, 0.1875000000000181521, -1.225000000000034950 ) ) ;
#58162 = CARTESIAN_POINT ( 'NONE',  ( 5.190073875932979419, 4.949507698210251938, 0.7998128361456341429 ) ) ;
#58163 = CARTESIAN_POINT ( 'NONE',  ( 6.568989397875739655, -1.719265429537725431, 1.406094356362475706 ) ) ;
#58164 = CARTESIAN_POINT ( 'NONE',  ( -5.992340707560165569, 8.014150130285418783, 1.443375672974064550 ) ) ;
#58165 = CARTESIAN_POINT ( 'NONE',  ( 3.334942599281629949, 5.874221551595115720, -1.082531754730543083 ) ) ;
#58166 = CARTESIAN_POINT ( 'NONE',  ( -5.056828107772848746, 8.843457192469559303, -0.7216878364870207285 ) ) ;
#58167 = CARTESIAN_POINT ( 'NONE',  ( 3.092668437693027794, 6.622213920701574885, -0.7216878364870338292 ) ) ;
#58168 = ORIENTED_EDGE ( 'NONE', *, *, #27925, .F. ) ;
#58169 = CARTESIAN_POINT ( 'NONE',  ( 4.658827374183164949, 1.163267680695536876, 1.646840100852072997 ) ) ;
#58171 = CARTESIAN_POINT ( 'NONE',  ( 3.274340622259350742, -1.012630945124261661, -1.796778529651460898 ) ) ;
#58170 = CARTESIAN_POINT ( 'NONE',  ( 4.690231075323689325, 7.559354456931247412, 1.199719254218462483 ) ) ;
#58172 = CARTESIAN_POINT ( 'NONE',  ( 6.668631453075247073, 8.873432343378178544, -1.599625672291281386 ) ) ;
#58173 = CARTESIAN_POINT ( 'NONE',  ( 3.241808126998965811, 6.796210224891872542, 0.7216878364870257245 ) ) ;
#58174 = CARTESIAN_POINT ( 'NONE',  ( 1.642778471875000035, -4.076041666188710444, -2.845375778867859751 ) ) ;
#58175 = CARTESIAN_POINT ( 'NONE',  ( 6.298795234281088895, 1.819837665574381091, 1.220625243075368127 ) ) ;
#58176 = CARTESIAN_POINT ( 'NONE',  ( 3.322888845334175389, 0.9041102021897020613, -1.802417075407992897 ) ) ;
#58177 = CARTESIAN_POINT ( 'NONE',  ( 3.667381569930192597, 1.025862638139760419, 1.528780434079744843 ) ) ;
#58178 = EDGE_CURVE ( 'NONE', #93128, #169987, #94173, .T. ) ;
#58179 = CARTESIAN_POINT ( 'NONE',  ( 7.494959990256193194, 7.638541498254023843, -0.7998128361456281477 ) ) ;
#58180 = SURFACE_STYLE_USAGE ( .BOTH. , #90704 ) ;
#58181 = CARTESIAN_POINT ( 'NONE',  ( 6.686557121163758666, -1.791048715316777562, -0.3524728914669760793 ) ) ;
#58182 = CARTESIAN_POINT ( 'NONE',  ( -0.06910031042392690559, -1.782763753708914267, -1.450585907311294775 ) ) ;
#58183 = CARTESIAN_POINT ( 'NONE',  ( -5.852315862593199469, 9.979452273000736895, 0.7998128361456481317 ) ) ;
#58184 = CARTESIAN_POINT ( 'NONE',  ( 6.631690487938540102, -1.471565961622269381, -1.718669407966398666 ) ) ;
#58185 = CARTESIAN_POINT ( 'NONE',  ( 2.016375119164611984, -0.9936656701176631579, -1.856918979450744578 ) ) ;
#58186 = CARTESIAN_POINT ( 'NONE',  ( -5.773793314573309132, 7.829454515125894964, 1.599625672291263179 ) ) ;
#58187 = CARTESIAN_POINT ( 'NONE',  ( 6.591235234537977661, 10.84152487360300299, 0.7998128361456462443 ) ) ;
#58188 = CARTESIAN_POINT ( 'NONE',  ( 6.983858524370782028, 8.280828045588322084, 1.082531754730549967 ) ) ;
#58189 = CARTESIAN_POINT ( 'NONE',  ( -6.470265622219711688, 8.571729197388226140, -1.599625672291263179 ) ) ;
#58190 = CARTESIAN_POINT ( 'NONE',  ( -4.121315508874269007, 5.831287398485175189, -1.443375672974053892 ) ) ;
#58191 = CARTESIAN_POINT ( 'NONE',  ( 7.415946836550714849, 9.675023947441092176, 1.443375672974076540 ) ) ;
#58192 = CARTESIAN_POINT ( 'NONE',  ( 4.159596813995052322, 7.384974941181836172, -0.7733407813514819873 ) ) ;
#58193 = CARTESIAN_POINT ( 'NONE',  ( -6.112028321662274166, 6.025121218227761588, 0.7998128361456341429 ) ) ;
#58195 = CARTESIAN_POINT ( 'NONE',  ( 3.832468605949594043, -1.144296635937601669, -1.903904886208422909 ) ) ;
#58194 = CARTESIAN_POINT ( 'NONE',  ( 2.391022662813433453, -2.030629854096975606, -0.6112283555373964061 ) ) ;
#58196 = CARTESIAN_POINT ( 'NONE',  ( 1.588088344156918907, -2.181139600106785092, -0.2122876309011075546 ) ) ;
#58197 = CARTESIAN_POINT ( 'NONE',  ( 0.4170028235400899397, 1.518763190251697370, -1.601383572969114599 ) ) ;
#58198 = CARTESIAN_POINT ( 'NONE',  ( -6.147696309153835692, 6.137010213626392208, 0.7998128361456281477 ) ) ;
#58199 = CARTESIAN_POINT ( 'NONE',  ( 4.141029529442549872, -0.1900441490861082827, -1.952618137025011746 ) ) ;
#58200 = CARTESIAN_POINT ( 'NONE',  ( 9.673906298550626559, 11.24497775551929557, 1.199719254218452047 ) ) ;
#58201 = CARTESIAN_POINT ( 'NONE',  ( -5.219248474292968787, 6.450796296714536915, 1.173595342525960206 ) ) ;
#58202 = CARTESIAN_POINT ( 'NONE',  ( -1.402160292154681736E-14, -0.05312499965857903073, -1.575800808251665908 ) ) ;
#58203 = CARTESIAN_POINT ( 'NONE',  ( 6.610000000000037623, 2.481806704560181043, 2.105257736569548399 ) ) ;
#58205 = ORIENTED_EDGE ( 'NONE', *, *, #64968, .F. ) ;
#58204 = CARTESIAN_POINT ( 'NONE',  ( -5.422898255786193111, 8.310169817517122581, -1.082531754730544860 ) ) ;
#58207 = CARTESIAN_POINT ( 'NONE',  ( 3.762070191281779774, 0.7111978290502696254, -1.997938288694045550 ) ) ;
#58206 = CIRCLE ( 'NONE', #99797, 0.08000000000000027922 ) ;
#58208 = CARTESIAN_POINT ( 'NONE',  ( -3.284818356260900796, 7.054314858938165678, 0.7998128361456352531 ) ) ;
#58209 = CARTESIAN_POINT ( 'NONE',  ( 5.823154874416164084, -0.05760400987671504547, 2.161107263091876618 ) ) ;
#58210 = CARTESIAN_POINT ( 'NONE',  ( 3.983814121021773680, -1.821778379405362136, -0.2661574599523569007 ) ) ;
#58211 = CARTESIAN_POINT ( 'NONE',  ( -5.845765802024414981, 6.039811503853035113, 0.4322504083978280232 ) ) ;
#58212 = CARTESIAN_POINT ( 'NONE',  ( -0.6823417656250003738, 0.7802083336747520637, -1.181850606188749264 ) ) ;
#58213 = B_SPLINE_CURVE_WITH_KNOTS ( 'NONE', 3,
 ( #194715, #78825, #128741, #743, #96183, #114607 ),
 .UNSPECIFIED., .F., .F.,
 ( 4, 2, 4 ),
 ( 0.000000000000000000, 0.0003767011250903910184, 0.0007534022501807818200 ),
 .UNSPECIFIED. ) ;
#58214 = CARTESIAN_POINT ( 'NONE',  ( 0.5029371931441508625, -1.732330776274123796, 0.1679752909130062255 ) ) ;
#58215 = CARTESIAN_POINT ( 'NONE',  ( 6.827182134110203471, 1.269052739965634391, 2.024653661457261222 ) ) ;
#58216 = CARTESIAN_POINT ( 'NONE',  ( 3.768803514918948938, 4.459654191235965293, -1.082531754730543083 ) ) ;
#58217 = CARTESIAN_POINT ( 'NONE',  ( 1.499999999999996891, 11.89583333333333570, -0.8660254037844378194 ) ) ;
#58218 = CARTESIAN_POINT ( 'NONE',  ( 4.083022661009271914, -0.2092679848491978134, -2.151539631373246220 ) ) ;
#58219 = CARTESIAN_POINT ( 'NONE',  ( 5.782577320554741718, -1.967585831723076772, 0.4389650999883643046 ) ) ;
#58220 = CARTESIAN_POINT ( 'NONE',  ( -7.280365300414089802, 10.47721470291632784, 1.082531754730549967 ) ) ;
#58221 = AXIS2_PLACEMENT_3D ( 'NONE', #160311, #45513, #206914 ) ;
#58222 = CARTESIAN_POINT ( 'NONE',  ( 3.678741886385179072, -2.082744454470350615, -0.5786317199799119182 ) ) ;
#58223 = CARTESIAN_POINT ( 'NONE',  ( 3.848864690211077466, -1.613568265775822130, 1.132301161112803545 ) ) ;
#58224 = DIRECTION ( 'NONE',  ( 0.000000000000000000, -1.000000000000000000, -9.023263958591317418E-17 ) ) ;
#58225 = CARTESIAN_POINT ( 'NONE',  ( 1.114821240386947965, -1.040235440384199794, -2.059874970276051265 ) ) ;
#58226 = CARTESIAN_POINT ( 'NONE',  ( 3.304032624679804631, -2.058584765098357749, 0.09746896435120806779 ) ) ;
#58227 = CARTESIAN_POINT ( 'NONE',  ( 6.040568865451770186, -1.638250791085652303, 1.042688759833640066 ) ) ;
#58230 = ORIENTED_EDGE ( 'NONE', *, *, #9224, .T. ) ;
#58229 = EDGE_CURVE ( 'NONE', #90728, #140333, #197488, .T. ) ;
#58228 = CARTESIAN_POINT ( 'NONE',  ( -8.473482818416675499, 9.948446711983361723, -1.082531754730543083 ) ) ;
#58231 = CARTESIAN_POINT ( 'NONE',  ( -4.782994330570982555, 8.802186828966616972, 0.000000000000000000 ) ) ;
#58232 = CARTESIAN_POINT ( 'NONE',  ( 11.88172094500853859, 9.720000056015921430, 1.685553348215818925 ) ) ;
#58234 = ORIENTED_EDGE ( 'NONE', *, *, #87487, .F. ) ;
#58233 = CARTESIAN_POINT ( 'NONE',  ( 1.355252715606880543E-15, 4.021557182957056220, -11.93179687198411543 ) ) ;
#58235 = CARTESIAN_POINT ( 'NONE',  ( -8.148087131688699358, 8.608449196499371681, -0.7216878364870267237 ) ) ;
#58236 = CARTESIAN_POINT ( 'NONE',  ( 1.975870009618452050, 2.111717515986545113, -0.6407313945460398896 ) ) ;
#58237 = CARTESIAN_POINT ( 'NONE',  ( -1.642778471875000035, -3.755208332855374476, -2.845375778867859751 ) ) ;
#58238 = EDGE_LOOP ( 'NONE', ( #12559, #94278, #112828, #132962 ) ) ;
#58239 = CARTESIAN_POINT ( 'NONE',  ( 6.614115624646348834, 1.956711779489667125, -0.1410536379464824575 ) ) ;
#58240 = CARTESIAN_POINT ( 'NONE',  ( -0.02880301295729841352, 5.718910385480866054, -2.867850616339829628 ) ) ;
#58241 = CARTESIAN_POINT ( 'NONE',  ( -1.499999999999997780, 5.431250000682820378, 1.214306433183764966E-14 ) ) ;
#58242 = FACE_OUTER_BOUND ( 'NONE', #6638, .T. ) ;
#58243 = DIRECTION ( 'NONE',  ( 0.6507913734559627184, -0.7592566023653016805, 0.000000000000000000 ) ) ;
#58244 = CARTESIAN_POINT ( 'NONE',  ( 5.103375755629981469, -1.831930319445294719, 0.1838923505294575433 ) ) ;
#58245 = EDGE_LOOP ( 'NONE', ( #51854, #77240, #15271, #162854 ) ) ;
#58246 = CARTESIAN_POINT ( 'NONE',  ( 2.623961231070126132, -1.185536401616044566, -1.685555923420704039 ) ) ;
#58247 = CARTESIAN_POINT ( 'NONE',  ( -1.360316468750021768, 0.6406250003414132310, -3.469446951953614189E-14 ) ) ;
#58248 = EDGE_CURVE ( 'NONE', #92214, #183003, #112595, .T. ) ;
#58249 = CARTESIAN_POINT ( 'NONE',  ( -5.181187258716735577, 9.196468901811520880, 0.7998128361456481317 ) ) ;
#58250 = B_SPLINE_CURVE_WITH_KNOTS ( 'NONE', 3,
 ( #185451, #137801, #55465, #86900, #57604, #168151, #38155, #135662, #119463, #24016, #39215, #121620 ),
 .UNSPECIFIED., .F., .F.,
 ( 4, 2, 2, 2, 2, 4 ),
 ( 0.000000000000000000, 0.0005575204076271189505, 0.001115040815254237901, 0.001672561222881356960, 0.001951321426694916164, 0.002230081630508475368 ),
 .UNSPECIFIED. ) ;
#58251 = CARTESIAN_POINT ( 'NONE',  ( -6.966220764712169000, 6.002124920821316323, -2.420000000000000373 ) ) ;
#58252 =( NAMED_UNIT ( * ) SI_UNIT ( $, .STERADIAN. ) SOLID_ANGLE_UNIT ( ) );
#58253 = CARTESIAN_POINT ( 'NONE',  ( 4.578903193113299963, 6.365139696764064325, 1.599625672291267398 ) ) ;
#58254 = CARTESIAN_POINT ( 'NONE',  ( 0.9189065912094130928, 1.903898908998642447, 0.7894373168981814182 ) ) ;
#58256 = CARTESIAN_POINT ( 'NONE',  ( 4.599059095968327071, -0.4863373063577690059, 1.775805238918099382 ) ) ;
#58255 = DIRECTION ( 'NONE',  ( -0.000000000000000000, 1.000000000000000000, -0.000000000000000000 ) ) ;
#58257 = CARTESIAN_POINT ( 'NONE',  ( 6.109920781252839994, 10.27999134477033216, 1.040834085586084257E-14 ) ) ;
#58258 = CARTESIAN_POINT ( 'NONE',  ( -9.434499674138207226, 14.57978396016029699, -7.415633383874704165 ) ) ;
#58259 = CARTESIAN_POINT ( 'NONE',  ( -4.956387674247580755, 7.940146832334256111, 1.199719254218452935 ) ) ;
#58261 = ORIENTED_EDGE ( 'NONE', *, *, #59473, .T. ) ;
#58260 = CARTESIAN_POINT ( 'NONE',  ( -0.4019237886466871523, 10.44866454968463110, -1.499999999999998668 ) ) ;
#58262 = CARTESIAN_POINT ( 'NONE',  ( 3.914836437932368796, 1.561248537261412883, -1.560010120355350471 ) ) ;
#58263 = CARTESIAN_POINT ( 'NONE',  ( 6.925078400183534377, -0.01048729610059369148, 2.244148362790527429 ) ) ;
#58264 = CARTESIAN_POINT ( 'NONE',  ( -5.341549334104202629, 7.254893527920112994, 1.443375672974064550 ) ) ;
#58265 = CARTESIAN_POINT ( 'NONE',  ( 6.486573133654839118, -1.106559166176981579, 1.434805384617921842 ) ) ;
#58266 = CARTESIAN_POINT ( 'NONE',  ( 6.069544675611900253, 1.326465198304109583, 1.382431045765440514 ) ) ;
#58267 = VECTOR ( 'NONE', #22094, 1000.000000000000000 ) ;
#58268 = CARTESIAN_POINT ( 'NONE',  ( -10.50000000000000000, 13.39999999999998259, 3.599999999999999201 ) ) ;
#58269 = CARTESIAN_POINT ( 'NONE',  ( 1.704906730629534684, -1.665072001576539007, -1.584524786048894240 ) ) ;
#58270 = CARTESIAN_POINT ( 'NONE',  ( 8.276983181174589532, 15.22877027432517494, -8.690223756940865130 ) ) ;
#58271 = CARTESIAN_POINT ( 'NONE',  ( 5.250612361737760025, 1.884661702551674534, 0.3228764834103393100 ) ) ;
#58272 = DIRECTION ( 'NONE',  ( 0.000000000000000000, -1.000000000000000000, 0.000000000000000000 ) ) ;
#58273 = EDGE_CURVE ( 'NONE', #7968, #117790, #34980, .T. ) ;
#58274 = CARTESIAN_POINT ( 'NONE',  ( 0.7603692911175019553, -1.357789551990191246, 1.287012767582619510 ) ) ;
#58275 = CARTESIAN_POINT ( 'NONE',  ( 2.659388954101277847, 1.913261587491304150, -0.6371546050257800298 ) ) ;
#58277 = CARTESIAN_POINT ( 'NONE',  ( 4.231157339275457119, 0.1028475037690677746, 2.103686673710772670 ) ) ;
#58276 = CARTESIAN_POINT ( 'NONE',  ( -9.515124878692420296, 9.995400534762978850, 1.040834085586084257E-14 ) ) ;
#58278 = CARTESIAN_POINT ( 'NONE',  ( 8.796542737168120851, 9.157054702984622097, -0.7998128361456211532 ) ) ;
#58280 = CARTESIAN_POINT ( 'NONE',  ( -8.341290820905609138, 10.75459192918846618, 1.599625672291269396 ) ) ;
#58279 = CARTESIAN_POINT ( 'NONE',  ( -1.402160292154681736E-14, 0.2125000000000202283, 1.732050807568877637 ) ) ;
#58281 = CARTESIAN_POINT ( 'NONE',  ( 0.08058608058606961388, -9.999999999999994671, -10.99970480893079738 ) ) ;
#58282 = CARTESIAN_POINT ( 'NONE',  ( 4.306902303582704761, -0.4466378413249347257, -1.969604032634456825 ) ) ;
#58283 = CARTESIAN_POINT ( 'NONE',  ( 1.364683531249988535, 4.905208333674756283, -0.7879004041258300672 ) ) ;
#58284 = CARTESIAN_POINT ( 'NONE',  ( 8.541273586929342798, 11.94827437051752206, -1.082531754730543083 ) ) ;
#58285 = CARTESIAN_POINT ( 'NONE',  ( 4.393933622532245842, -0.8317529007547798114, 1.995363109761492337 ) ) ;
#58286 = CARTESIAN_POINT ( 'NONE',  ( 6.688968683495743583, 8.897159112202094988, -1.599625672291283607 ) ) ;
#58287 = CARTESIAN_POINT ( 'NONE',  ( 1.499999999999989120, 4.754166666666689522, 0.8660254037844524744 ) ) ;
#58288 = CARTESIAN_POINT ( 'NONE',  ( 5.169401708560450004, 9.252995436621013425, 0.000000000000000000 ) ) ;
#58289 =( BOUNDED_SURFACE ( )  B_SPLINE_SURFACE ( 3, 2, ( 
 ( #199706, #31913, #81714 ),
 ( #2558, #51353, #419 ),
 ( #165096, #84906, #150993 ),
 ( #68632, #200764, #131583 ),
 ( #181339, #13128, #61896 ),
 ( #177786, #96556, #213444 ),
 ( #129118, #14179, #126984 ),
 ( #130173, #195095, #111780 ) ),
 .UNSPECIFIED., .F., .F., .F. ) 
 B_SPLINE_SURFACE_WITH_KNOTS ( ( 4, 2, 2, 4 ),
 ( 3, 3 ),
 ( 0.000000000000000000, 0.003001918495469456383, 0.004502877743204184574, 0.006003836990938912765 ),
 ( 0.000000000000000000, 1.000000000000000000 ),
 .UNSPECIFIED. ) 
 GEOMETRIC_REPRESENTATION_ITEM ( )  RATIONAL_B_SPLINE_SURFACE ( (
 ( 1.000000000000000000, 0.7835651598521267136, 1.000000000000000000),
 ( 1.000000000000000000, 0.7913519369917237922, 1.000000000000000000),
 ( 1.000000000000000000, 0.8009496234828819006, 1.000000000000000000),
 ( 1.000000000000000000, 0.8230981486291126803, 1.000000000000000000),
 ( 1.000000000000000000, 0.8318333311017226395, 1.000000000000000000),
 ( 1.000000000000000000, 0.8529518727575166048, 1.000000000000000000),
 ( 1.000000000000000000, 0.8654984584225899891, 1.000000000000000000),
 ( 1.000000000000000000, 0.8789000212895413666, 1.000000000000000000) ) ) 
 REPRESENTATION_ITEM ( '' )  SURFACE ( )  );
#58290 = CARTESIAN_POINT ( 'NONE',  ( 8.717529583462649612, 10.23316793787035195, 1.082531754730558626 ) ) ;
#58292 = CARTESIAN_POINT ( 'NONE',  ( 3.740297717422798041, 7.429476292658457659, 2.448395595369510680 ) ) ;
#58291 = CARTESIAN_POINT ( 'NONE',  ( 2.383468162319524630, -0.001743713053406481962, 2.171350059665664300 ) ) ;
#58294 = CARTESIAN_POINT ( 'NONE',  ( 0.3800845246329161431, -0.2246070939678334044, -1.827447590993152682 ) ) ;
#58293 = CARTESIAN_POINT ( 'NONE',  ( -6.561783159334145132, 6.757761228752363181, -0.7216878364870278340 ) ) ;
#58295 = CARTESIAN_POINT ( 'NONE',  ( -0.6823417656250212460, 2.301041667008084435, 1.181850606188767472 ) ) ;
#58296 = CARTESIAN_POINT ( 'NONE',  ( 3.193114300108112147, 1.729001323093733111, 1.346577201094656395 ) ) ;
#58297 = CARTESIAN_POINT ( 'NONE',  ( 6.983263157960355016, 2.444413620957446742, 2.336241774956763884 ) ) ;
#58298 = CARTESIAN_POINT ( 'NONE',  ( 3.309705378935084763, -0.4432241279512488807, 2.218521802316391511 ) ) ;
#58299 = CARTESIAN_POINT ( 'NONE',  ( -6.531277313481209212, 8.642909503859968368, 1.599625672291283607 ) ) ;
#58301 = PRESENTATION_LAYER_ASSIGNMENT (  '', '', ( #168987 ) ) ;
#58300 = CARTESIAN_POINT ( 'NONE',  ( 0.6823417656249899377, 5.238541667008086655, -1.181850606188754593 ) ) ;
#58302 = CARTESIAN_POINT ( 'NONE',  ( 6.206332990038123221, 6.936436922908462144, -0.8583981852504622978 ) ) ;
#58303 = CARTESIAN_POINT ( 'NONE',  ( -1.500000000000015099, 11.72916666666666252, -0.8660254037844309360 ) ) ;
#58304 = CARTESIAN_POINT ( 'NONE',  ( 6.549997609177859559, 6.814287763561861944, 0.000000000000000000 ) ) ;
#58305 = CARTESIAN_POINT ( 'NONE',  ( 4.797990518455403475, -1.769373726167685623, -0.04385371103611360177 ) ) ;
#58306 = CARTESIAN_POINT ( 'NONE',  ( 6.760712154708803823, 11.03924794713562818, 1.040834085586084257E-14 ) ) ;
#58307 = CARTESIAN_POINT ( 'NONE',  ( 0.2707219772894990384, -1.375384669632748524, 1.594866825539154043 ) ) ;
#58309 = CARTESIAN_POINT ( 'NONE',  ( 1.499999999999989120, 1.775000000000019673, 0.000000000000000000 ) ) ;
#58308 = CARTESIAN_POINT ( 'NONE',  ( -0.6823417656250003738, 11.15104166700806765, 1.181850606188754593 ) ) ;
#58310 = CARTESIAN_POINT ( 'NONE',  ( 1.135132829348266092, -0.04487231981731241992, -1.969206670302141804 ) ) ;
#58311 = AXIS2_PLACEMENT_3D ( 'NONE', #184807, #36436, #86261 ) ;
#58312 = CARTESIAN_POINT ( 'NONE',  ( -4.390861645979385663, 6.216034235099629157, -1.599625672291271394 ) ) ;
#58313 = CARTESIAN_POINT ( 'NONE',  ( 0.2737812321212430566, -1.924752420120953822, 0.3788971555385572954 ) ) ;
#58314 = ORIENTED_EDGE ( 'NONE', *, *, #140577, .F. ) ;
#58315 = CARTESIAN_POINT ( 'NONE',  ( 6.317736394288131052, 9.354147645769410602, 1.082531754730558626 ) ) ;
#58316 = CARTESIAN_POINT ( 'NONE',  ( 4.522238337509359773, 1.150754656758418593, -1.474723989322044737 ) ) ;
#58317 = ORIENTED_EDGE ( 'NONE', *, *, #128138, .F. ) ;
#58318 = CARTESIAN_POINT ( 'NONE',  ( 4.223533608758993196, 0.2584441732129874603, -2.054024224480345939 ) ) ;
#58319 = CARTESIAN_POINT ( 'NONE',  ( -2.153317591523261390E-14, 2.187499999999986233, -1.414508159514625385 ) ) ;
#58320 = CARTESIAN_POINT ( 'NONE',  ( -7.078765599666485997, 7.431183752465250869, 0.000000000000000000 ) ) ;
#58321 = CARTESIAN_POINT ( 'NONE',  ( -2.494447209962484813, 3.467171072964057466, 11.73545145049398464 ) ) ;
#58322 = CARTESIAN_POINT ( 'NONE',  ( 8.239604668803105270, 10.63595808506888396, -1.599625672291268286 ) ) ;
#58323 = CARTESIAN_POINT ( 'NONE',  ( -10.66756793585402363, 11.33991743478486391, 0.7998128361456462443 ) ) ;
#58324 = CARTESIAN_POINT ( 'NONE',  ( 6.535912570239620578, 9.782925877658371405, 1.199719254218452047 ) ) ;
#58325 = PLANE ( 'NONE',  #52425 ) ;
#58326 = CARTESIAN_POINT ( 'NONE',  ( 1.364683531249986537, -0.8864583329919110133, 0.7879004041258500513 ) ) ;
#58327 = CARTESIAN_POINT ( 'NONE',  ( -0.7500000000000006661, 0.3583333333333563187, -1.299038105676652011 ) ) ;
#58328 = CARTESIAN_POINT ( 'NONE',  ( 4.281663391851794565, -1.878042059144067633, 0.5673916069991248312 ) ) ;
#58329 = CARTESIAN_POINT ( 'NONE',  ( 2.477888549845189470, 1.799646572043178683, 0.9090068759892779848 ) ) ;
#58330 = CARTESIAN_POINT ( 'NONE',  ( -3.975497760493641675, 7.849573349659754840, -7.471960471057975262E-11 ) ) ;
#58331 = CARTESIAN_POINT ( 'NONE',  ( 7.828177403543859825, -5.742104877864243839, 7.727873494160014900 ) ) ;
#58332 = DIRECTION ( 'NONE',  ( 0.000000000000000000, 0.000000000000000000, -1.000000000000000000 ) ) ;
#58333 = CARTESIAN_POINT ( 'NONE',  ( 0.4736314445139556684, 1.071599637473351629, 1.532994764490814177 ) ) ;
#58334 = CARTESIAN_POINT ( 'NONE',  ( -0.6823417656249969321, 5.717708333674756283, -1.181850606188749264 ) ) ;
#58335 = CARTESIAN_POINT ( 'NONE',  ( 2.549090200060105893, 0.2507624435445845457, 1.997490752340509879 ) ) ;
#58337 = CARTESIAN_POINT ( 'NONE',  ( 3.357133807288110727, 0.04956003552011908203, -2.116800119666595315 ) ) ;
#58336 = CARTESIAN_POINT ( 'NONE',  ( -4.609409038966229666, 8.321468278861834378, -0.7216878364870267237 ) ) ;
#58338 = DIRECTION ( 'NONE',  ( 0.000000000000000000, 1.000000000000000000, 0.000000000000000000 ) ) ;
#58339 = CARTESIAN_POINT ( 'NONE',  ( 5.248515149483167441, -2.054309126314420642, -0.2569322651706855143 ) ) ;
#58340 = CARTESIAN_POINT ( 'NONE',  ( 7.666209513884374438, 7.908608952478760834, 0.7998128361456281477 ) ) ;
#58342 = DIRECTION ( 'NONE',  ( 0.000000000000000000, 0.000000000000000000, 1.000000000000000000 ) ) ;
#58341 = CARTESIAN_POINT ( 'NONE',  ( 0.6090670738765286973, -0.3027767823605455599, 2.068569423397928819 ) ) ;
#58344 = ORIENTED_EDGE ( 'NONE', *, *, #10029, .F. ) ;
#58343 = CARTESIAN_POINT ( 'NONE',  ( 5.895480738319402114, 1.384055093596334274, 1.190509915477963698 ) ) ;
#58345 = CARTESIAN_POINT ( 'NONE',  ( 9.264299036839600987, 9.702770385934682551, -0.7998128361456281477 ) ) ;
#58346 = CARTESIAN_POINT ( 'NONE',  ( 10.95308175811721085, 9.799999999999998934, -1.800000000000001155 ) ) ;
#58347 = CARTESIAN_POINT ( 'NONE',  ( -11.96212011828584210, 13.82812445049947669, 0.9569185076417884295 ) ) ;
#58348 = CARTESIAN_POINT ( 'NONE',  ( -11.75337143377970328, 4.618255228540592228, 5.022398747751031678 ) ) ;
#58349 = CARTESIAN_POINT ( 'NONE',  ( -1.364683531250014514, 11.65104166700806587, -0.7879004041258335089 ) ) ;
#58350 = CARTESIAN_POINT ( 'NONE',  ( 5.707647354773449422, 1.450964518888698596, 1.245719642194928811 ) ) ;
#58351 = CARTESIAN_POINT ( 'NONE',  ( -9.982881178363895103, 10.54111621771303753, 1.040834085586084257E-14 ) ) ;
#58352 = CIRCLE ( 'NONE', #207080, 11.09999999999999964 ) ;
#58353 = CARTESIAN_POINT ( 'NONE',  ( 4.971035877704902184, 8.951292290631053916, 1.040834085586084257E-14 ) ) ;
#58354 = CARTESIAN_POINT ( 'NONE',  ( -0.6801582343750386395, 2.380208333674735499, -1.178068619123869398 ) ) ;
#58355 = CARTESIAN_POINT ( 'NONE',  ( 4.500943809612556024, 4.353448654077163305, 1.214306433183764966E-14 ) ) ;
#58356 = CARTESIAN_POINT ( 'NONE',  ( -2.081668171172168513E-14, 6.468705557303652931, 4.925226524755076163 ) ) ;
#58357 = CARTESIAN_POINT ( 'NONE',  ( 3.649115900372475796, 7.409052317076538330, 1.040834085586084257E-14 ) ) ;
#58358 = ORIENTED_EDGE ( 'NONE', *, *, #6353, .T. ) ;
#58359 = EDGE_CURVE ( 'NONE', #201490, #108500, #114547, .T. ) ;
#58360 = PRODUCT_RELATED_PRODUCT_CATEGORY ( 'part', '', ( #199001 ) ) ;
#58361 = CARTESIAN_POINT ( 'NONE',  ( -6.017840079619296567, 8.114175741012878973, -1.599625672291271394 ) ) ;
#58362 = CARTESIAN_POINT ( 'NONE',  ( 5.466422796518627614, -1.967893101392578448, -0.4390109167287381542 ) ) ;
#58363 = CARTESIAN_POINT ( 'NONE',  ( 0.07406709734308211668, -9.431556885384749123, -9.500634193481465317 ) ) ;
#58364 = CARTESIAN_POINT ( 'NONE',  ( 10.39230484541330313, 4.000000000000003553, 5.999999999999906741 ) ) ;
#58365 = AXIS2_PLACEMENT_3D ( 'NONE', #131294, #80344, #51047 ) ;
#58366 = CARTESIAN_POINT ( 'NONE',  ( -6.492041734278776843, 6.763935894940780180, 0.1675349064616058481 ) ) ;
#58367 = CARTESIAN_POINT ( 'NONE',  ( -4.934804725694220906, 7.740727365743146571, -1.082531754730549967 ) ) ;
#58368 = CARTESIAN_POINT ( 'NONE',  ( 9.164948653157988900, 11.71552606681625619, -1.443375672974057666 ) ) ;
#58369 = CARTESIAN_POINT ( 'NONE',  ( 2.043745906638486431, 1.354474275242853798, 1.429983431767953617 ) ) ;
#58370 = CARTESIAN_POINT ( 'NONE',  ( 2.970327539257538341, -1.987051465770898417, -0.3419137282784574516 ) ) ;
#58371 = CARTESIAN_POINT ( 'NONE',  ( -6.723954117373590833, 9.932031339322813679, -1.199719254218440723 ) ) ;
#58372 = CARTESIAN_POINT ( 'NONE',  ( 6.727182134110196721, 7.629137130509074716, 2.889055895399252005 ) ) ;
#58373 = CARTESIAN_POINT ( 'NONE',  ( 3.609492757825348175, -2.159078094573213757, 0.3743817768235499499 ) ) ;
#58374 = CARTESIAN_POINT ( 'NONE',  ( 2.327063250521405724, -0.002089543651138252821, 1.926566264030280307 ) ) ;
#58375 = CARTESIAN_POINT ( 'NONE',  ( -9.494787648271923786, 9.971673765939062406, 1.040834085586084257E-14 ) ) ;
#58376 = CARTESIAN_POINT ( 'NONE',  ( 0.2331563151865730654, 0.7315591717663977311, -2.029986209603263259 ) ) ;
#58377 = CARTESIAN_POINT ( 'NONE',  ( -9.367496996292747014, 15.51845925588232333, -7.500000001629758550 ) ) ;
#58378 = CARTESIAN_POINT ( 'NONE',  ( 6.096362627639171805, 10.26417349888772179, -0.7998128361456291469 ) ) ;
#58379 = ADVANCED_FACE ( 'NONE', ( #16064 ), #160213, .T. ) ;
#58380 = CARTESIAN_POINT ( 'NONE',  ( 6.471319392424407901, 6.444294134116939077, 0.7998128361456341429 ) ) ;
#58381 = CARTESIAN_POINT ( 'NONE',  ( -6.779954559072826292, -7.792646766725027874, 6.731761806397297931 ) ) ;
#58382 = CARTESIAN_POINT ( 'NONE',  ( 5.560252395380206991, 7.580323442733986283, 1.443375672974065660 ) ) ;
#58383 = ORIENTED_EDGE ( 'NONE', *, *, #61843, .T. ) ;
#58385 = CARTESIAN_POINT ( 'NONE',  ( 2.895184040856535468, -0.1504547458161388240, -2.007539188286605825 ) ) ;
#58384 = CARTESIAN_POINT ( 'NONE',  ( 5.618664544990171095, -0.03892770779775727580, 1.841008343696965310 ) ) ;
#58386 = CARTESIAN_POINT ( 'NONE',  ( 4.235939456923387247, -2.142719978266393710, -0.8318502446633867509 ) ) ;
#58388 = CARTESIAN_POINT ( 'NONE',  ( 2.764321045800025800, -0.7073474514263197177, -1.721481455096545377 ) ) ;
#58387 = CARTESIAN_POINT ( 'NONE',  ( -0.02880301295722555166, 0.6711181056864559125, -2.353869138803561079 ) ) ;
#58389 = CARTESIAN_POINT ( 'NONE',  ( 1.642778471875001811, -0.3427083328553758301, 2.845375778867859751 ) ) ;
#58390 = DIRECTION ( 'NONE',  ( 0.000000000000000000, 7.254698431490414842E-17, -1.000000000000000000 ) ) ;
#58391 = SURFACE_STYLE_USAGE ( .BOTH. , #155897 ) ;
#58392 = CARTESIAN_POINT ( 'NONE',  ( -6.347188469492005325, 10.55680364771601809, -0.7998128361456291469 ) ) ;
#58393 = CARTESIAN_POINT ( 'NONE',  ( -4.665414256878304577, 5.575976400180357118, -1.082531754730549967 ) ) ;
#58394 = CARTESIAN_POINT ( 'NONE',  ( 6.058164993413670096, -1.477959563288837375, 1.479067623735799586 ) ) ;
#58395 = CARTESIAN_POINT ( 'NONE',  ( 7.646435448427411963, 8.023188899361205273, -0.7216878364870257245 ) ) ;
#58396 = ORIENTED_EDGE ( 'NONE', *, *, #55551, .F. ) ;
#58397 = AXIS2_PLACEMENT_3D ( 'NONE', #98738, #133399, #14255 ) ;
#58398 = CARTESIAN_POINT ( 'NONE',  ( -2.788906526875773208E-15, 12.21875000068279782, -1.499999999999998446 ) ) ;
#58400 = CARTESIAN_POINT ( 'NONE',  ( 4.867540842506059562, 5.637551390133895168, -1.199719254218452047 ) ) ;
#58399 = CARTESIAN_POINT ( 'NONE',  ( 1.458777222063855294, 0.5999999999999998668, -1.713029193092652225 ) ) ;
#58401 = CARTESIAN_POINT ( 'NONE',  ( 6.375633740537438143, 1.648238817998586958, -0.5085109915310691564 ) ) ;
#58402 = CARTESIAN_POINT ( 'NONE',  ( -3.899941742225307539, 7.701682465904834629, 0.7998128361456341429 ) ) ;
#58403 = CARTESIAN_POINT ( 'NONE',  ( 1.265804362365889668, 1.602598504008081237, -0.6630416328189077113 ) ) ;
#58404 = CARTESIAN_POINT ( 'NONE',  ( 0.1945363205450193478, 1.000000000000000888, -11.93115981699675743 ) ) ;
#58405 = DIRECTION ( 'NONE',  ( 0.000000000000000000, -1.000000000000000000, 0.000000000000000000 ) ) ;
#58406 = CARTESIAN_POINT ( 'NONE',  ( -5.874320061489284761, 6.022657918099090679, -0.3309714775648956997 ) ) ;
#58407 = CARTESIAN_POINT ( 'NONE',  ( 6.139545750997863927, 2.009069680886385267, -0.8233997750264672177 ) ) ;
#58408 = CARTESIAN_POINT ( 'NONE',  ( 4.600122369450095228, -1.825375079466069694, -0.04201004182294298950 ) ) ;
#58409 = CARTESIAN_POINT ( 'NONE',  ( 2.008577182894935476, 0.6104510041588115943, 1.864461945915835583 ) ) ;
#58410 = CARTESIAN_POINT ( 'NONE',  ( 9.574107565776355244, 3.767509419443892504, 7.159700408882949674 ) ) ;
#58411 = CARTESIAN_POINT ( 'NONE',  ( -9.748756651491515157, 4.000000000000000888, 7.301653494243616649 ) ) ;
#58412 = CARTESIAN_POINT ( 'NONE',  ( 9.250740883225924804, 9.686952540052077509, 1.040834085586084257E-14 ) ) ;
#58413 = CARTESIAN_POINT ( 'NONE',  ( 3.176547234745368264, 0.9552152173708803318, 1.893241096743401464 ) ) ;
#58414 = CARTESIAN_POINT ( 'NONE',  ( -4.148431816101615155, 3.942184661647709198, 0.7216878364870317197 ) ) ;
#58415 = PRESENTATION_LAYER_ASSIGNMENT (  '', '', ( #106870 ) ) ;
#58416 = FILL_AREA_STYLE_COLOUR ( '', #156596 ) ;
#58417 = CARTESIAN_POINT ( 'NONE',  ( -4.916882227542496153, 6.680427897100001289, -1.249109758411016236 ) ) ;
#58418 = CARTESIAN_POINT ( 'NONE',  ( 2.307561340129569150, -1.660171796135110567, -1.236610361758017973 ) ) ;
#58420 = CARTESIAN_POINT ( 'NONE',  ( -1.364683531250014514, -0.9489583329919112353, -0.7879004041258359514 ) ) ;
#58419 =( NAMED_UNIT ( * ) SI_UNIT ( $, .STERADIAN. ) SOLID_ANGLE_UNIT ( ) );
#58422 = ORIENTED_EDGE ( 'NONE', *, *, #158609, .T. ) ;
#58421 = CARTESIAN_POINT ( 'NONE',  ( 4.020361658589631126, -2.215315801286695585, 0.1640026922601171833 ) ) ;
#58423 = CARTESIAN_POINT ( 'NONE',  ( 2.198211363809216667, 2.055062875077425577, 1.030007645627160517 ) ) ;
#58425 = CARTESIAN_POINT ( 'NONE',  ( 6.455934469078565385, -0.7002696157344409089, 1.940163012464599879 ) ) ;
#58424 = CARTESIAN_POINT ( 'NONE',  ( 8.093854517678360949, 12.38665467069271386, 1.040834085586084257E-14 ) ) ;
#58427 = CARTESIAN_POINT ( 'NONE',  ( 3.285556943749998737, -3.405208332855374831, -1.896917185911906500 ) ) ;
#58426 = CARTESIAN_POINT ( 'NONE',  ( 4.095444919779759552, 6.935713618788495793, 1.199719254218451159 ) ) ;
#58428 = CARTESIAN_POINT ( 'NONE',  ( 11.86145016429273191, 10.90000000000000036, 1.099999999999996758 ) ) ;
#58429 = CARTESIAN_POINT ( 'NONE',  ( 6.603072989126265391, -0.3962418105841297722, 1.804722624154910360 ) ) ;
#58430 = PRESENTATION_STYLE_ASSIGNMENT (( #140783 ) ) ;
#58431 = CARTESIAN_POINT ( 'NONE',  ( -0.2104748580754409182, 6.947232144882289795, -2.698723162346649662 ) ) ;
#58432 = CARTESIAN_POINT ( 'NONE',  ( 2.783889825318270450, -0.8885198777363271239, 1.478144978849999847 ) ) ;
#58433 = CARTESIAN_POINT ( 'NONE',  ( 2.852750215419812108, -1.865046845876184189, -0.7672916333427428626 ) ) ;
#58434 = CARTESIAN_POINT ( 'NONE',  ( 2.971610153692927803, -2.265147269936502727, -0.3905154627303064618 ) ) ;
#58435 = CARTESIAN_POINT ( 'NONE',  ( 3.251526197659323270, -1.847530484110882387, -1.305540666510462078 ) ) ;
#58436 = CARTESIAN_POINT ( 'NONE',  ( 5.250649905694958264, 0.6104557620976447385, 2.015647016877469166 ) ) ;
#58437 = CARTESIAN_POINT ( 'NONE',  ( -5.289089323106922258, 9.184704953684462936, 0.7216878364870267237 ) ) ;
#58438 = CARTESIAN_POINT ( 'NONE',  ( 3.461912321176093599, 0.7928900474763724837, 1.582224000876080172 ) ) ;
#58440 = CARTESIAN_POINT ( 'NONE',  ( 6.110887424941569002, -0.2848874328069994633, 2.274520343394012212 ) ) ;
#58439 = CARTESIAN_POINT ( 'NONE',  ( 5.207740400980577888, 5.248321020665011716, 0.000000000000000000 ) ) ;
#58441 = CARTESIAN_POINT ( 'NONE',  ( 5.982333729491328356, -0.2747192703472668418, -1.820405398140816589 ) ) ;
#58442 = CARTESIAN_POINT ( 'NONE',  ( -5.122283107864663343, 4.870418468797203637, 0.000000000000000000 ) ) ;
#58443 = AXIS2_PLACEMENT_3D ( 'NONE', #109735, #212475, #61987 ) ;
#58444 = CARTESIAN_POINT ( 'NONE',  ( 1.499999999999989120, 4.004166666666685970, 0.8660254037844524744 ) ) ;
#58445 = CARTESIAN_POINT ( 'NONE',  ( 5.296902861200166512, 1.790115547914197247, 1.263834295783084150 ) ) ;
#58446 = CARTESIAN_POINT ( 'NONE',  ( -2.948008335967658322, 5.526761261015804116, 1.199719254218462483 ) ) ;
#58447 = CARTESIAN_POINT ( 'NONE',  ( -3.069676183974461292, 15.51994954726069409, 11.60951955297166016 ) ) ;
#58448 = CARTESIAN_POINT ( 'NONE',  ( 5.494608840674215955, 2.039112051642687717, 0.3575134270455831986 ) ) ;
#58449 = CARTESIAN_POINT ( 'NONE',  ( -11.88168329227126563, 9.720000000000000639, -1.685799833707129380 ) ) ;
#58450 = B_SPLINE_CURVE_WITH_KNOTS ( 'NONE', 3,
 ( #4776, #130887, #98324, #118635, #196881, #114640, #164389, #18915 ),
 .UNSPECIFIED., .F., .F.,
 ( 4, 2, 2, 4 ),
 ( 0.0003136881264510912523, 0.0009048594355810784130, 0.001200445090146071885, 0.001496030744711065140 ),
 .UNSPECIFIED. ) ;
#58451 = CARTESIAN_POINT ( 'NONE',  ( -1.201851678989727383E-14, 4.446875000341417916, -1.575800808251660134 ) ) ;
#58452 = CARTESIAN_POINT ( 'NONE',  ( 4.213445252184796708, -0.3281303603181011108, 1.898201707710310826 ) ) ;
#58453 = CARTESIAN_POINT ( 'NONE',  ( -8.012344526598182026E-15, 10.54687500034139624, -1.575800808251669460 ) ) ;
#58454 = CARTESIAN_POINT ( 'NONE',  ( -3.795919822146293754, 4.491289883001181593, -1.082531754730549967 ) ) ;
#58455 = CARTESIAN_POINT ( 'NONE',  ( 0.4049022847291971483, -2.205595429402911201, -0.2640273158710532142 ) ) ;
#58457 = ORIENTED_EDGE ( 'NONE', *, *, #97488, .T. ) ;
#58456 = CARTESIAN_POINT ( 'NONE',  ( -1.115562610750309283E-14, 11.06250000000000178, 1.500000000000001554 ) ) ;
#58459 = DIRECTION ( 'NONE',  ( 1.224646799147353207E-16, 0.000000000000000000, -1.000000000000000000 ) ) ;
#58458 = CARTESIAN_POINT ( 'NONE',  ( -3.363831509966360489, 6.938570838353784076, -0.7216878364870458196 ) ) ;
#58460 = CARTESIAN_POINT ( 'NONE',  ( 10.05353459973327368, 11.68787744023238417, -1.199719254218440723 ) ) ;
#58461 = CARTESIAN_POINT ( 'NONE',  ( -0.6311622855796912290, 3.299999999999990496, -0.4000000000000270561 ) ) ;
#58462 = AXIS2_PLACEMENT_3D ( 'NONE', #156931, #205647, #204569 ) ;
#58463 = CARTESIAN_POINT ( 'NONE',  ( 9.422972378981830488, 13.09454993570456161, 7.356553532920802496 ) ) ;
#58464 = DIRECTION ( 'NONE',  ( 0.000000000000000000, 0.000000000000000000, 1.000000000000000000 ) ) ;
#58465 = CARTESIAN_POINT ( 'NONE',  ( 1.064813361795993618, 1.487921858168140377, -1.278797858372302088 ) ) ;
#58466 = CARTESIAN_POINT ( 'NONE',  ( -1.364683531250000748, 1.321875000341421469, 0.000000000000000000 ) ) ;
#58467 = CARTESIAN_POINT ( 'NONE',  ( 10.91804383151480096, 0.000000000000000000, -0.1905751639681742271 ) ) ;
#58468 = CARTESIAN_POINT ( 'NONE',  ( 5.670351692713981429, -0.8806477319739226539, -1.753155087565357428 ) ) ;
#58469 = CARTESIAN_POINT ( 'NONE',  ( -7.700141177557535244, 11.07091624287075859, -1.199719254218446718 ) ) ;
#58470 = CARTESIAN_POINT ( 'NONE',  ( -4.541618270453545492, 8.242379048930368768, 0.7216878364870458196 ) ) ;
#58471 = CARTESIAN_POINT ( 'NONE',  ( 6.596550757224428629, -0.5713381284546023009, -2.084776384472402100 ) ) ;
#58473 = ORIENTED_EDGE ( 'NONE', *, *, #28769, .F. ) ;
#58472 = CARTESIAN_POINT ( 'NONE',  ( -0.2977236940312470992, -5.250949308401958504, -10.97067990664317350 ) ) ;
#58474 = CARTESIAN_POINT ( 'NONE',  ( -1.500000000000015099, -1.297916665983847029, 0.8660254037844403729 ) ) ;
#58475 = CARTESIAN_POINT ( 'NONE',  ( 0.5791066246769066561, 1.747692025923882841, -0.6672336632058751826 ) ) ;
#58476 = CARTESIAN_POINT ( 'NONE',  ( 5.729790939124476346, -1.568816369837353619, -0.7386035493782086014 ) ) ;
#58478 = CARTESIAN_POINT ( 'NONE',  ( 3.439196427729715566, -1.660734982795486481, -1.430121640581414111 ) ) ;
#58477 = CARTESIAN_POINT ( 'NONE',  ( 1.360316468749983576, 0.9947916670081107249, 0.7853790794158601596 ) ) ;
#58479 = CARTESIAN_POINT ( 'NONE',  ( 3.927071981709300719, 2.190135382617847792, 0.7269923479944776501 ) ) ;
#58480 = CARTESIAN_POINT ( 'NONE',  ( 6.696563014664697278, -0.5452183415704283664, -1.987298092995327226 ) ) ;
#58481 = CARTESIAN_POINT ( 'NONE',  ( 2.238135065718354078, 0.4255327557451081266, 1.894600943326588238 ) ) ;
#58482 = CARTESIAN_POINT ( 'NONE',  ( -4.406036734316890247, 7.123831375802920363, -1.082531754730548412 ) ) ;
#58483 = CARTESIAN_POINT ( 'NONE',  ( 1.408489644590610990, 7.311701683603665458, -4.382268911471478567 ) ) ;
#58484 = CARTESIAN_POINT ( 'NONE',  ( 4.869442314738527067, -1.792836814666173062, -1.132239877606910472 ) ) ;
#58485 = CARTESIAN_POINT ( 'NONE',  ( 1.360316468749978025, 0.5364583336746844289, -0.7853790794159001276 ) ) ;
#58486 = CARTESIAN_POINT ( 'NONE',  ( 3.322888845334175389, 0.9041102021897020613, -1.802417075407992897 ) ) ;
#58487 = CARTESIAN_POINT ( 'NONE',  ( -4.487385655998893164, 6.258369236797239665, 1.443375672974064550 ) ) ;
#58488 = CARTESIAN_POINT ( 'NONE',  ( -6.474900878978163021, 9.711745571186627402, -1.199719254218452047 ) ) ;
#58489 = CARTESIAN_POINT ( 'NONE',  ( 10.23370702021670020, 10.83374636654133383, 0.7998128361456462443 ) ) ;
#58490 = CARTESIAN_POINT ( 'NONE',  ( 0.9085097582094739943, 1.384192474337717194, -1.190531929384466281 ) ) ;
#58491 = CARTESIAN_POINT ( 'NONE',  ( -5.478376588373717659, 8.549133898814758936, -1.199719254218452047 ) ) ;
#58492 = CARTESIAN_POINT ( 'NONE',  ( -0.08053691275167716712, 15.51887838114830132, 11.99972973886013961 ) ) ;
#58493 = CARTESIAN_POINT ( 'NONE',  ( -5.983791420057156252, 7.107340751733106643, 1.079986564815892613 ) ) ;
#58494 = VERTEX_POINT ( 'NONE', #147179 ) ;
#58495 = CARTESIAN_POINT ( 'NONE',  ( 6.069226122992825267, 0.1539936439061925788, -2.055202734049704105 ) ) ;
#58496 = CARTESIAN_POINT ( 'NONE',  ( -6.577113915960836721, 8.766661883411348555, -1.443375672974066548 ) ) ;
#58497 = EDGE_CURVE ( 'NONE', #198335, #12234, #126923, .T. ) ;
#58498 = CARTESIAN_POINT ( 'NONE',  ( -3.242371291962510504, 6.934516940598226320, 1.040834085586084257E-14 ) ) ;
#58499 = CARTESIAN_POINT ( 'NONE',  ( -5.164730172163054966, 4.990216387137135889, -0.7998128361456362523 ) ) ;
#58500 = CARTESIAN_POINT ( 'NONE',  ( 5.039715841750210146, -1.917062458738912012, 0.6357382205050918778 ) ) ;
#58502 = ORIENTED_EDGE ( 'NONE', *, *, #183135, .T. ) ;
#58501 = CARTESIAN_POINT ( 'NONE',  ( 6.112022827852052309, -0.7509524718064889415, 2.090657394127520163 ) ) ;
#58504 = CARTESIAN_POINT ( 'NONE',  ( 9.083599731475988648, 10.66024977721925104, 1.082531754730549967 ) ) ;
#58503 = CARTESIAN_POINT ( 'NONE',  ( -3.156015896931072540, 6.904045323053366268, 0.000000000000000000 ) ) ;
#58505 = CARTESIAN_POINT ( 'NONE',  ( 6.819914962873951936, 7.915321197229798322, -1.199719254218446718 ) ) ;
#58506 = CARTESIAN_POINT ( 'NONE',  ( 3.801680928091007772, -0.6000553829732765410, 1.971583879547859963 ) ) ;
#58507 = CARTESIAN_POINT ( 'NONE',  ( 3.815077410725796980, 1.076317812134291119, -1.704938119663282903 ) ) ;
#58508 = ORIENTED_EDGE ( 'NONE', *, *, #95890, .T. ) ;
#58509 = CARTESIAN_POINT ( 'NONE',  ( 1.913843478179629631, 3.256154753185150241, -0.4414708703500153653 ) ) ;
#58510 = CARTESIAN_POINT ( 'NONE',  ( 3.842846474469570062, 6.570739089268092137, -1.199719254218452047 ) ) ;
#58512 = ORIENTED_EDGE ( 'NONE', *, *, #97813, .F. ) ;
#58511 = CARTESIAN_POINT ( 'NONE',  ( -6.933015448541747006, 9.181880338089085214, 1.599625672291269396 ) ) ;
#58513 = CARTESIAN_POINT ( 'NONE',  ( 4.730098472736550264, 8.327237590489470875, -0.7222317683119976461 ) ) ;
#58514 = CARTESIAN_POINT ( 'NONE',  ( 3.848982377512807140, -0.9961485462514390044, 1.752762419822328832 ) ) ;
#58515 = CARTESIAN_POINT ( 'NONE',  ( 2.202840038917678545, -0.4038221959529255112, 1.796142596185656526 ) ) ;
#58516 = CARTESIAN_POINT ( 'NONE',  ( 0.7510979139944070626, 0.6750874020578813139, 2.206752807669599470 ) ) ;
#58517 = CARTESIAN_POINT ( 'NONE',  ( 4.598150373690133463, 5.393538853173795111, -1.199719254218452047 ) ) ;
#58518 = CARTESIAN_POINT ( 'NONE',  ( 4.270900206319126369, -2.015198044118733822, -0.7823990653590962019 ) ) ;
#58519 = CARTESIAN_POINT ( 'NONE',  ( -4.550733115681270036, 8.460939068270139529, 0.7998128361456481317 ) ) ;
#58520 = ORIENTED_EDGE ( 'NONE', *, *, #207763, .T. ) ;
#58521 = CARTESIAN_POINT ( 'NONE',  ( 0.3282377607280981269, 2.426335450315351139, -1.225000000000014300 ) ) ;
#58522 = CARTESIAN_POINT ( 'NONE',  ( 2.395189659270926086, 1.444574673180216706, 1.188490415850687265 ) ) ;
#58523 = EDGE_CURVE ( 'NONE', #147848, #108613, #210004, .T. ) ;
#58524 = CARTESIAN_POINT ( 'NONE',  ( 5.471542181860619358, 1.900225975651721244, -0.5249898485142224791 ) ) ;
#58526 = CARTESIAN_POINT ( 'NONE',  ( 8.392133896734655707, 11.77427806529038357, 1.082531754730546636 ) ) ;
#58525 = CARTESIAN_POINT ( 'NONE',  ( -1.001543065824772872E-14, 5.321875000341422357, 1.575800808251672791 ) ) ;
#58528 = CARTESIAN_POINT ( 'NONE',  ( 0.3466626200071438180, 2.201290530325435757, 0.1579762268871589825 ) ) ;
#58527 = CARTESIAN_POINT ( 'NONE',  ( -6.762819695118240659, 6.784377820593065600, 0.7998128361456341429 ) ) ;
#58529 = LINE ( 'NONE', #27083, #81575 ) ;
#58530 = CARTESIAN_POINT ( 'NONE',  ( 4.493637847925535667, 7.329995691633395261, -1.199719254218452047 ) ) ;
#58531 = CARTESIAN_POINT ( 'NONE',  ( -5.575427483717760424, 7.527751369135936343, 1.599625672291269396 ) ) ;
#58532 = CARTESIAN_POINT ( 'NONE',  ( 6.539320575229256249, 7.052319431262985105, 2.701414634427783845 ) ) ;
#58533 = CARTESIAN_POINT ( 'NONE',  ( 6.455938704688762186, 1.966190342143339764, -0.1448359745850023028 ) ) ;
#58534 = CARTESIAN_POINT ( 'NONE',  ( 5.321043329010971767, 2.130378997510178785, 0.8875623774946446165 ) ) ;
#58535 = CARTESIAN_POINT ( 'NONE',  ( 5.740631066870683696, -1.815735608131360479, -0.4073663091734185948 ) ) ;
#58536 = CARTESIAN_POINT ( 'NONE',  ( 2.799736005369108049, -1.525370932871713547, -1.388464765246626875 ) ) ;
#58537 = CARTESIAN_POINT ( 'NONE',  ( 7.022760382198770301, 8.255937203062467589, -1.082531754730543083 ) ) ;
#58538 = CARTESIAN_POINT ( 'NONE',  ( 5.969332771766739931, 10.18624834369502885, -0.7998128361456481317 ) ) ;
#58539 = CARTESIAN_POINT ( 'NONE',  ( 7.904040366642699489, 8.323727970612377902, 0.7216878364870458196 ) ) ;
#58540 = CARTESIAN_POINT ( 'NONE',  ( -1.201851678989727383E-14, 2.759375000341417916, -1.575800808251660134 ) ) ;
#58541 = FACE_OUTER_BOUND ( 'NONE', #135395, .T. ) ;
#58542 = CARTESIAN_POINT ( 'NONE',  ( 4.948362878863507675, 8.716914425408678113, -0.7216878364870267237 ) ) ;
#58543 = CARTESIAN_POINT ( 'NONE',  ( 5.441899255841128102, 1.454089660041712140, 1.612519925251713060 ) ) ;
#58544 = LINE ( 'NONE', #141966, #161983 ) ;
#58546 = CARTESIAN_POINT ( 'NONE',  ( 3.526749072549471453, -1.699942963128863838, 0.7078653300200200560 ) ) ;
#58545 = CARTESIAN_POINT ( 'NONE',  ( -2.304522924643024773, 5.632434478818063361, 0.7216878364870317197 ) ) ;
#58548 = CYLINDRICAL_SURFACE ( 'NONE', #189579, 1.500000000000000222 ) ;
#58547 = DIRECTION ( 'NONE',  ( -3.330669073875478989E-16, 3.540251991789410786E-16, 1.000000000000000000 ) ) ;
#58549 = CARTESIAN_POINT ( 'NONE',  ( 1.997444822565041855, 3.480956003828838075, 0.4000000000000185074 ) ) ;
#58550 = CARTESIAN_POINT ( 'NONE',  ( 0.000000000000000000, 0.000000000000000000, 0.000000000000000000 ) ) ;
#58551 = CARTESIAN_POINT ( 'NONE',  ( 0.5446534387809185418, 2.256470935699141034, 0.1650129453365980214 ) ) ;
#58552 = CARTESIAN_POINT ( 'NONE',  ( -4.009952404978103679, 7.802135278885950598, 0.4104602055842437314 ) ) ;
#58553 = CARTESIAN_POINT ( 'NONE',  ( 3.469446951953614189E-15, 0.7598076211376182387, 6.938893903907228378E-15 ) ) ;
#58554 = CARTESIAN_POINT ( 'NONE',  ( 6.548892101489681927, 6.803534504848940401, 0.4251794856353352525 ) ) ;
#58555 = AXIS2_PLACEMENT_3D ( 'NONE', #93464, #180029, #18569 ) ;
#58556 = CARTESIAN_POINT ( 'NONE',  ( -5.939880696118548187, 6.102484698325975288, 0.000000000000000000 ) ) ;
#58557 = CARTESIAN_POINT ( 'NONE',  ( -0.1049974700286886165, -0.1398519552151776535, -1.881156918050665094 ) ) ;
#58558 = CARTESIAN_POINT ( 'NONE',  ( 0.3734444151584931926, 1.013553851667288841, 1.450680648178425125 ) ) ;
#58559 = CARTESIAN_POINT ( 'NONE',  ( 4.934244218189309805, -1.078892596291732398, -1.699401429059212765 ) ) ;
#58560 = CARTESIAN_POINT ( 'NONE',  ( 6.328958779480917229, 6.278206752349526631, 0.7998128361456341429 ) ) ;
#58561 = CARTESIAN_POINT ( 'NONE',  ( 3.856552995061765632, 0.7561154531541111057, 1.965730562608114740 ) ) ;
#58563 = CARTESIAN_POINT ( 'NONE',  ( 3.005391328865916645, -1.845313015785840172, 0.5138285116655214591 ) ) ;
#58562 = CARTESIAN_POINT ( 'NONE',  ( -3.348500752450953577, 4.929670182657964084, 1.443375672974062551 ) ) ;
#58564 = CARTESIAN_POINT ( 'NONE',  ( 3.358669367883368118, 4.941533567329135401, -1.599625672291262513 ) ) ;
#58565 = CARTESIAN_POINT ( 'NONE',  ( 3.894935592111925526, 0.2864876570476772022, 1.948460325470881660 ) ) ;
#58566 = CARTESIAN_POINT ( 'NONE',  ( 5.449475261934634496, -1.824267568868439771, 0.8672911397697125047 ) ) ;
#58567 = CARTESIAN_POINT ( 'NONE',  ( 2.324885834233282544, -0.002380789299309681549, 1.870836310375329381 ) ) ;
#58569 = VERTEX_POINT ( 'NONE', #30217 ) ;
#58568 = CARTESIAN_POINT ( 'NONE',  ( 5.162619097868246243, -1.245661315326980212, 1.193383824415847450 ) ) ;
#58571 = CARTESIAN_POINT ( 'NONE',  ( 3.823036129373602154, 6.443664003369091731, -1.082531754730548412 ) ) ;
#58570 = CARTESIAN_POINT ( 'NONE',  ( 2.350463684150871035, 2.206416367115513477, 0.05273732197710182673 ) ) ;
#58572 = CARTESIAN_POINT ( 'NONE',  ( -0.6823417656250212460, 3.863541667008085767, 1.181850606188767472 ) ) ;
#58573 = CARTESIAN_POINT ( 'NONE',  ( 6.057081135787192316, 1.604708697955498087, -1.128374156723031430 ) ) ;
#58575 = AXIS2_PLACEMENT_3D ( 'NONE', #115018, #177837, #129170 ) ;
#58574 = CARTESIAN_POINT ( 'NONE',  ( 8.925345196497941558, 9.307324238869423283, 1.040834085586084257E-14 ) ) ;
#58576 = CARTESIAN_POINT ( 'NONE',  ( -9.398826802771548472, 11.98838390803207865, -1.599625672291263179 ) ) ;
#58577 = FACE_BOUND ( 'NONE', #109527, .T. ) ;
#58578 = CARTESIAN_POINT ( 'NONE',  ( -5.766295404513793521, 5.621766148221195358, 0.7998128361456341429 ) ) ;
#58579 = CARTESIAN_POINT ( 'NONE',  ( 7.214015694909405418, -7.024005795613374126, 7.869907041763756439 ) ) ;
#58580 = ORIENTED_EDGE ( 'NONE', *, *, #35599, .F. ) ;
#58581 = CARTESIAN_POINT ( 'NONE',  ( 2.014207461368537455, 2.064961549741591185, -0.1501100615294431728 ) ) ;
#58582 = CARTESIAN_POINT ( 'NONE',  ( -1.201851678989727383E-14, 3.712500000000020339, 1.732050807568877637 ) ) ;
#58583 = CARTESIAN_POINT ( 'NONE',  ( 6.745345117998789775, 7.828323044875442172, 1.199719254218462483 ) ) ;
#58584 = CARTESIAN_POINT ( 'NONE',  ( 4.146814880933355596, 5.931313009212638931, 1.599625672291261402 ) ) ;
#58585 = CARTESIAN_POINT ( 'NONE',  ( 6.633471380297788045, -0.1541069161683609745, 2.086224335282916620 ) ) ;
#58586 = FACE_OUTER_BOUND ( 'NONE', #172887, .T. ) ;
#58587 = CARTESIAN_POINT ( 'NONE',  ( -1.364683531250012516, 3.488541667008085767, -0.7879004041258300672 ) ) ;
#58589 = CARTESIAN_POINT ( 'NONE',  ( 10.23604278863759909, 11.04439746293979496, 0.000000000000000000 ) ) ;
#58588 = CARTESIAN_POINT ( 'NONE',  ( 0.000000000000000000, -6.836568542494925182, 0.000000000000000000 ) ) ;
#58590 = CARTESIAN_POINT ( 'NONE',  ( 4.991564454312596766, 1.928456700051227379, 0.5879293935868237231 ) ) ;
#58591 = CARTESIAN_POINT ( 'NONE',  ( 4.768704397049558175, -0.2406929234074564883, -1.900496090682921579 ) ) ;
#58592 = CARTESIAN_POINT ( 'NONE',  ( 6.539320575229236709, 3.694699318329996540, 2.517509839998680832 ) ) ;
#58593 = CARTESIAN_POINT ( 'NONE',  ( 2.156058135970494227, 0.9403143569667195001, 1.979733194660021622 ) ) ;
#58594 = CARTESIAN_POINT ( 'NONE',  ( 0.3636750363432239008, -6.893137084989843899, 10.99449589488468604 ) ) ;
#58595 = CARTESIAN_POINT ( 'NONE',  ( -0.7500000000000215383, 1.722916667349486008, 1.299038105676659116 ) ) ;
#58596 = CARTESIAN_POINT ( 'NONE',  ( 0.1529896150729666005, 0.3463191217260193633, 1.982936507005612414 ) ) ;
#58597 = CARTESIAN_POINT ( 'NONE',  ( 2.373185085050379506, -1.665764800640230803, -0.9392108107411781814 ) ) ;
#58598 = CARTESIAN_POINT ( 'NONE',  ( -4.693093728624763372, 8.627026450037540428, 0.7998128361456481317 ) ) ;
#58600 = CARTESIAN_POINT ( 'NONE',  ( 6.573823534745116604, -0.9041686956474543901, 1.912245183953432237 ) ) ;
#58599 = CARTESIAN_POINT ( 'NONE',  ( -3.551873057100300990, 5.166937871415542283, 1.443375672974064550 ) ) ;
#58601 = CARTESIAN_POINT ( 'NONE',  ( -0.6823417656250039265, 9.380208333674728394, -1.181850606188755259 ) ) ;
#58602 = MECHANICAL_DESIGN_GEOMETRIC_PRESENTATION_REPRESENTATION (  '', ( #34312 ), #155378 ) ;
#58604 = CARTESIAN_POINT ( 'NONE',  ( -6.363572996767778100, 8.517530811019446091, -1.599625672291271394 ) ) ;
#58603 = CARTESIAN_POINT ( 'NONE',  ( 3.667594231577479658, 1.163246697351211223, 1.737046641446901463 ) ) ;
#58606 = ORIENTED_EDGE ( 'NONE', *, *, #92773, .F. ) ;
#58605 = CARTESIAN_POINT ( 'NONE',  ( 2.326796526899118422, -0.003300274434325441240, 1.724958192180660044 ) ) ;
#58607 = DIRECTION ( 'NONE',  ( 1.000000000000000000, 0.000000000000000000, 1.224646799147353207E-16 ) ) ;
#58608 = CARTESIAN_POINT ( 'NONE',  ( 4.788000803920411386, 8.737751371215816576, 1.040834085586084257E-14 ) ) ;
#58609 =( NAMED_UNIT ( * ) SI_UNIT ( $, .STERADIAN. ) SOLID_ANGLE_UNIT ( ) );
#58610 = CARTESIAN_POINT ( 'NONE',  ( -11.80247861663003484, 9.799999999999998934, -1.695431928471868188 ) ) ;
#58611 = CARTESIAN_POINT ( 'NONE',  ( 4.171104814498611368, 8.018039383557042044, 0.7998128361456321445 ) ) ;
#58612 = CARTESIAN_POINT ( 'NONE',  ( -11.91826849282518452, 13.39999999999999858, -1.400000000000001465 ) ) ;
#58613 = ORIENTED_EDGE ( 'NONE', *, *, #105847, .F. ) ;
#58614 = CARTESIAN_POINT ( 'NONE',  ( 2.473076435208894530, -1.576862618776267100, -0.8914009245391883995 ) ) ;
#58615 = ORIENTED_EDGE ( 'NONE', *, *, #186000, .F. ) ;
#58616 = CARTESIAN_POINT ( 'NONE',  ( 3.460355519985863548, 5.060167411448709629, 1.599625672291267398 ) ) ;
#58617 = CARTESIAN_POINT ( 'NONE',  ( 6.059568310664962709, 6.034194215389424798, 0.7998128361456352531 ) ) ;
#58618 = CARTESIAN_POINT ( 'NONE',  ( 3.756361958294622383, 1.803085962505234008, 0.1738922897399265421 ) ) ;
#58619 = CARTESIAN_POINT ( 'NONE',  ( 6.539320575229274901, 7.053161517996441532, 2.494893549996656912 ) ) ;
#58620 = TOROIDAL_SURFACE ( 'NONE', #179681, 11.92000000000000171, 0.08000000000000000167 ) ;
#58621 = DIRECTION ( 'NONE',  ( 0.7592566023653005702, 0.6507913734559639396, 0.000000000000000000 ) ) ;
#58622 = CARTESIAN_POINT ( 'NONE',  ( 5.861148881710747993, 5.995921596292371092, 0.2991943293650864422 ) ) ;
#58624 = EDGE_CURVE ( 'NONE', #149119, #87461, #108869, .T. ) ;
#58623 = VECTOR ( 'NONE', #81752, 1000.000000000000114 ) ;
#58626 = CARTESIAN_POINT ( 'NONE',  ( -1.402160292154681736E-14, 14.17187500034139624, 1.575800808251682339 ) ) ;
#58625 = CARTESIAN_POINT ( 'NONE',  ( 3.859670702416746924, -0.5421201558965526024, 1.780318336934373802 ) ) ;
#58627 = CARTESIAN_POINT ( 'NONE',  ( 1.581495747622517323, -0.6437907056052544208, 1.804334155150161267 ) ) ;
#58628 = CARTESIAN_POINT ( 'NONE',  ( 0.6744773098602949712, -1.717252091951677384, -0.6198786263262797691 ) ) ;
#58629 = CARTESIAN_POINT ( 'NONE',  ( 4.790043373817672645, 8.140258622390808441, 0.8134525054356611662 ) ) ;
#58630 = CARTESIAN_POINT ( 'NONE',  ( -5.112833325684916552, 7.058334528089424076, -1.443375672974066770 ) ) ;
#58631 = CARTESIAN_POINT ( 'NONE',  ( 4.978641999450219124, 7.938775605734648799, 1.052364473307040305 ) ) ;
#58632 = CARTESIAN_POINT ( 'NONE',  ( 5.309888000197702240, 7.741188690324601218, 1.308016840036421602 ) ) ;
#58633 = CARTESIAN_POINT ( 'NONE',  ( -1.734723475976807094E-15, -8.327195405469542067, -10.91970695577494332 ) ) ;
#58634 = CARTESIAN_POINT ( 'NONE',  ( 6.925078400183593885, 7.051837472187183486, 2.742497896504832333 ) ) ;
#58635 = CARTESIAN_POINT ( 'NONE',  ( 6.751597309925441159, 9.860318714012938912, -1.082531754730537088 ) ) ;
#58636 = CARTESIAN_POINT ( 'NONE',  ( 5.858249334120006147, -1.969629310164786373, -0.003746551262697600092 ) ) ;
#58637 = CARTESIAN_POINT ( 'NONE',  ( -2.578021764892882040, 6.159442492350315490, 0.7998128361456341429 ) ) ;
#58638 = CARTESIAN_POINT ( 'NONE',  ( -11.86687215968023601, 9.990577876942106528, -1.056395335932043045 ) ) ;
#58639 = CARTESIAN_POINT ( 'NONE',  ( 1.834041477103361739, 2.068079971995392619, 0.3053845110000241170 ) ) ;
#58640 = CARTESIAN_POINT ( 'NONE',  ( 6.264670948233396430, -1.361836867979081545, 1.362739274238314868 ) ) ;
#58641 = CARTESIAN_POINT ( 'NONE',  ( -6.230135280679522936, 7.227244901336242755, 1.199719254218450271 ) ) ;
#58642 = CARTESIAN_POINT ( 'NONE',  ( 1.447985623159939284, 1.823312892812560593, 0.09356915273009414058 ) ) ;
#58643 = CARTESIAN_POINT ( 'NONE',  ( 3.686314334879085663, -1.088174899301070253, 1.919869060924610293 ) ) ;
#58644 = CARTESIAN_POINT ( 'NONE',  ( -1.115562610750309283E-14, 9.843750000682801371, 1.500000000000001554 ) ) ;
#58645 = CARTESIAN_POINT ( 'NONE',  ( 1.353610510645312237, -1.387278792934818705, -1.316581319992945920 ) ) ;
#58646 = ORIENTED_EDGE ( 'NONE', *, *, #153640, .F. ) ;
#58647 = CARTESIAN_POINT ( 'NONE',  ( 1.029674291210751269, 1.899031994249468225, -0.5220998716058099509 ) ) ;
#58648 = CARTESIAN_POINT ( 'NONE',  ( 2.401813893259804100, -0.7453968187615340746, -1.793506507769267788 ) ) ;
#58649 = ORIENTED_EDGE ( 'NONE', *, *, #10768, .T. ) ;
#58650 = CARTESIAN_POINT ( 'NONE',  ( -1.443289932012703552E-16, 1.999999999999999556, 2.600000000000008082 ) ) ;
#58652 = CARTESIAN_POINT ( 'NONE',  ( 6.367989434593707365, -1.846973275860162467, 0.2267098040239327594 ) ) ;
#58651 = CARTESIAN_POINT ( 'NONE',  ( -6.168033539574333979, 6.160736982450306876, 0.7998128361456281477 ) ) ;
#58653 = CARTESIAN_POINT ( 'NONE',  ( 3.250922972226694352, 7.014770244231638863, 0.7998128361456281477 ) ) ;
#58654 = DIRECTION ( 'NONE',  ( -0.4243160830846619547, -0.9055141421511264666, 5.421010862427548676E-14 ) ) ;
#58655 = CARTESIAN_POINT ( 'NONE',  ( 4.035228272797701798, 3.987058170690799042, -0.7945584926636685141 ) ) ;
#58656 = CARTESIAN_POINT ( 'NONE',  ( -5.641074431737709283, 8.738948049406083385, -1.199719254218452047 ) ) ;
#58657 = CARTESIAN_POINT ( 'NONE',  ( 3.070069520051089906, -1.303570237086741024, 1.761582097007891923 ) ) ;
#58658 = CARTESIAN_POINT ( 'NONE',  ( 10.89423718502886906, -6.453216945989374231, -0.03415196713897916680 ) ) ;
#58659 = FACE_OUTER_BOUND ( 'NONE', #212607, .T. ) ;
#58660 = CARTESIAN_POINT ( 'NONE',  ( 3.158640206316553289, -1.382037546686708973, 1.193037399656725395 ) ) ;
#58661 = DIRECTION ( 'NONE',  ( 1.000000000000000000, 0.000000000000000000, -1.465138070926357285E-17 ) ) ;
#58662 = CARTESIAN_POINT ( 'NONE',  ( -9.110716038703348119, 12.61262389758715408, 1.082531754730560403 ) ) ;
#58663 = STYLED_ITEM ( 'NONE', ( #168463 ), #174158 ) ;
#58664 = CARTESIAN_POINT ( 'NONE',  ( -4.671432059311929841, 8.392430178223424520, -0.5935467769075646327 ) ) ;
#58665 = CARTESIAN_POINT ( 'NONE',  ( 6.925078400183546812, 2.074047572655359328, 2.163550030515603684 ) ) ;
#58666 = CARTESIAN_POINT ( 'NONE',  ( 7.540305987494599016, 11.94877408538573427, -0.7998128361456291469 ) ) ;
#58668 = EDGE_CURVE ( 'NONE', #40348, #123271, #193955, .T. ) ;
#58667 = CARTESIAN_POINT ( 'NONE',  ( 0.6098321186917586845, -1.917330571200571265, 0.1878080533235688687 ) ) ;
#58669 = CARTESIAN_POINT ( 'NONE',  ( 5.436364959771895045, -1.092926877770916017, 1.628904810760459121 ) ) ;
#58670 = CARTESIAN_POINT ( 'NONE',  ( 1.499999999999997113, 15.14583333333333570, -0.8660254037844378194 ) ) ;
#58671 = CARTESIAN_POINT ( 'NONE',  ( -7.552055258011950656, 8.769484874890757453, 1.199719254218462483 ) ) ;
#58672 = CARTESIAN_POINT ( 'NONE',  ( 5.497994985541524215, 6.373081223675282736, -1.199719254218445830 ) ) ;
#58673 = CARTESIAN_POINT ( 'NONE',  ( 5.144143540903125533, 0.6357783856077160456, 2.097287126430439130 ) ) ;
#58674 = DIRECTION ( 'NONE',  ( 0.9629573728775006058, 0.2631879969435746425, 0.05869562407617064104 ) ) ;
#58676 = EDGE_CURVE ( 'NONE', #190223, #11451, #95777, .T. ) ;
#58675 = CARTESIAN_POINT ( 'NONE',  ( -4.134873662487946966, 3.926366815765101936, 1.214306433183764966E-14 ) ) ;
#58677 = CARTESIAN_POINT ( 'NONE',  ( 5.524307029080702591, 1.015476208609331188, 1.803995072556117574 ) ) ;
#58679 = CARTESIAN_POINT ( 'NONE',  ( -1.364683531250012516, 2.801041667008090652, -0.7879004041258289570 ) ) ;
#58678 = FACE_OUTER_BOUND ( 'NONE', #86612, .T. ) ;
#58680 = VERTEX_POINT ( 'NONE', #118100 ) ;
#58681 = CARTESIAN_POINT ( 'NONE',  ( 4.799617249347348569, 1.585997580420713593, -1.664126067976256840 ) ) ;
#58682 = CARTESIAN_POINT ( 'NONE',  ( 7.470179451449751262, 7.817556902887268677, 1.040834085586084257E-14 ) ) ;
#58683 = CARTESIAN_POINT ( 'NONE',  ( 4.068855497876973537, 7.761098824249525130, -0.7216878364870338292 ) ) ;
#58684 = CARTESIAN_POINT ( 'NONE',  ( 0.07670252363861564115, -2.225146658028719582, -0.5502862128906602646 ) ) ;
#58685 = CARTESIAN_POINT ( 'NONE',  ( -7.499070966595134280, -5.223177556212268868, -8.016215341155858098 ) ) ;
#58686 = CARTESIAN_POINT ( 'NONE',  ( -7.923814432544069142, 8.209148024248356990, 0.000000000000000000 ) ) ;
#58687 = CARTESIAN_POINT ( 'NONE',  ( 5.437426780092255996, 0.7852709207246920675, -1.776270868113111856 ) ) ;
#58688 = VERTEX_POINT ( 'NONE', #71384 ) ;
#58689 = CARTESIAN_POINT ( 'NONE',  ( 9.585251414737269826, 11.24551007435741568, -1.082531754730537088 ) ) ;
#58690 = ORIENTED_EDGE ( 'NONE', *, *, #203936, .T. ) ;
#58691 = CARTESIAN_POINT ( 'NONE',  ( 0.0002439367322616680669, -0.9454701154091667004, 1.777349279628215095 ) ) ;
#58692 = CARTESIAN_POINT ( 'NONE',  ( 6.510786919798099426, 1.273903079158642981, -1.162983891536113479 ) ) ;
#58693 = CARTESIAN_POINT ( 'NONE',  ( 5.577361344084559747, 1.530155114678043660, 1.313547687611632764 ) ) ;
#58695 = DIRECTION ( 'NONE',  ( 0.000000000000000000, 0.000000000000000000, 1.000000000000000000 ) ) ;
#58694 = CARTESIAN_POINT ( 'NONE',  ( -7.655550293210764856, 12.08322577538792331, 0.000000000000000000 ) ) ;
#58696 = CARTESIAN_POINT ( 'NONE',  ( 1.001543065824772753E-15, -2.209374999522042859, 3.793834371823811669 ) ) ;
#58698 = CARTESIAN_POINT ( 'NONE',  ( 6.555894367415777246, 1.764769525206461687, -0.1329060007094622631 ) ) ;
#58697 = CARTESIAN_POINT ( 'NONE',  ( 2.009825619773229377, -0.9864030779522957593, -1.843301731911746399 ) ) ;
#58699 = CARTESIAN_POINT ( 'NONE',  ( 5.555314621531947772, -1.277044735018734833, 1.560499014526220307 ) ) ;
#58701 = CARTESIAN_POINT ( 'NONE',  ( 3.064699953192471682, -2.118106589925540906, -0.8768602481810504612 ) ) ;
#58700 = CARTESIAN_POINT ( 'NONE',  ( 4.278479993564246797, 7.149254538203735798, 1.199719254218452047 ) ) ;
#58702 = B_SPLINE_CURVE_WITH_KNOTS ( 'NONE', 3,
 ( #94139, #143975, #26961, #7506, #188403, #155923, #8585 ),
 .UNSPECIFIED., .F., .F.,
 ( 4, 3, 4 ),
 ( 0.0001932309589017161869, 0.0009000000022123051842, 0.002089081127711812057 ),
 .UNSPECIFIED. ) ;
#58703 = CARTESIAN_POINT ( 'NONE',  ( 2.413636602577839518, 1.137377966863511780, -1.317326450295707607 ) ) ;
#58704 = CARTESIAN_POINT ( 'NONE',  ( 1.416652131158681049, 8.000043606524066320, 10.86080395187256897 ) ) ;
#58705 = CARTESIAN_POINT ( 'NONE',  ( 1.862203476926355794, -0.5897614712949137417, 1.630587920151181924 ) ) ;
#58706 = CARTESIAN_POINT ( 'NONE',  ( 1.360316468750005559, 1.567708333674729282, -0.7853790794158981292 ) ) ;
#58707 = CARTESIAN_POINT ( 'NONE',  ( 1.820531350174507512, -1.319122485308525716, 1.313071031887176998 ) ) ;
#58708 =( BOUNDED_SURFACE ( )  B_SPLINE_SURFACE ( 1, 2, ( 
 ( #25427, #157592, #141371, #9187, #90454, #59004, #57936, #60069, #78452, #92604, #106742, #75258, #41716, #8111, #109964, #76321, #207383, #27568, #107826, #125160, #42785, #190064, #24344, #44916, #174917, #156520, #158647, #159708, #143501, #128371, #10245, #142426, #160779, #208435, #11307, #77385, #126225, #74199, #192186, #175974, #209498, #61138, #193270, #111024, #177029, #62214, #140293, #28646, #206312, #94733, #12372, #144570, #210583, #194338, #178104, #79524, #114233, #182334, #161858, #115287, #45980, #149867, #112101, #13447, #83774, #197525, #181278, #145642, #131522, #49169, #95802, #133646, #211637, #48121, #81650, #63273, #129435, #166102, #47048, #147737, #195418, #113164, #132574, #165035, #179168, #148789, #1435, #97930, #100038, #96871, #82711, #33962, #65375, #67500, #32904, #130492, #180231, #17688, #98982, #16628, #146689, #29720, #30792, #162921, #15563, #14501, #198577, #80593, #212705, #64346, #196479, #31854, #163988, #213753, #359, #66431, #50224, #116343, #168236, #199645, #53412, #186611, #21944, #6775, #19835, #134700, #39302, #169301, #38237, #104310, #85921, #51292, #184468, #201772, #170359, #151993, #88054, #3566, #20885 ),
 ( #154126, #69640, #105397, #5696, #183414, #72850, #200705, #71773, #54489, #137889, #121709, #171435, #203908, #23025, #2501, #117416, #103241, #55555, #187672, #153052, #86982, #35017, #119549, #135748, #52356, #118484, #89140, #101088, #155194, #167175, #36085, #18764, #84848, #37163, #150938, #68573, #4628, #102169, #185535, #70700, #136813, #202840, #120633, #110768, #59817, #123849, #93411, #174664, #143248, #44654, #207127, #142168, #208184, #209238, #90205, #58753, #188747, #191928, #108636, #175714, #156269, #125971, #189812, #41462, #7851, #107571, #122788, #206057, #57692, #73938, #124905, #140032, #173605, #25177, #94478, #91279, #176768, #157338, #160518, #27306, #28383, #12122, #8926, #138957, #75007, #40386, #141116, #190868, #42532, #26238, #92355, #158393, #9991, #204978, #76068, #56623, #43592, #106490, #159449, #172516, #24101, #109710, #11047, #77126, #60882, #127041, #193001, #47867, #79269, #164782, #49966, #129181, #131283, #13192, #197270, #32646, #179975, #130232, #146432, #61956, #213504, #95550, #147482, #29461, #181029, #82452, #145386, #46794, #211385, #80331, #162667, #161603, #15310, #65125, #212446, #144321, #30533, #210319, #48910 ) ),
 .UNSPECIFIED., .F., .F., .T. ) 
 B_SPLINE_SURFACE_WITH_KNOTS ( ( 2, 2 ),
 ( 3, 2, 2, 2, 2, 2, 2, 2, 2, 2, 2, 2, 2, 2, 2, 2, 2, 2, 2, 2, 2, 2, 2, 2, 2, 2, 2, 2, 2, 2, 2, 2, 2, 2, 2, 2, 2, 2, 2, 2, 2, 2, 2, 2, 2, 2, 2, 2, 2, 2, 2, 2, 2, 2, 2, 2, 2, 2, 2, 2, 2, 2, 2, 2, 2, 2, 2, 2, 2, 3 ),
 ( 0.000000000000000000, 1.000000000000000000 ),
 ( 0.000000000000000000, 0.01388888888888888812, 0.02777777777777777624, 0.04166666666666666435, 0.05555555555555555247, 0.06944444444444444753, 0.08333333333333332871, 0.09722222222222222376, 0.1111111111111111049, 0.1250000000000000000, 0.1388888888888888951, 0.1527777777777777901, 0.1666666666666666574, 0.1805555555555555525, 0.1944444444444444475, 0.2083333333333333426, 0.2222222222222222099, 0.2361111111111111049, 0.2500000000000000000, 0.2638888888888888951, 0.2777777777777777901, 0.2916666666666666852, 0.3055555555555555802, 0.3194444444444444198, 0.3333333333333333148, 0.3472222222222222099, 0.3611111111111111049, 0.3750000000000000000, 0.3888888888888888951, 0.4027777777777777901, 0.4166666666666666852, 0.4305555555555555802, 0.4444444444444444198, 0.4583333333333333148, 0.4722222222222222099, 0.4861111111111111049, 0.5000000000000000000, 0.5138888888888888395, 0.5277777777777777901, 0.5416666666666666297, 0.5555555555555555802, 0.5694444444444444198, 0.5833333333333333703, 0.5972222222222222099, 0.6111111111111111605, 0.6250000000000000000, 0.6388888888888888395, 0.6527777777777777901, 0.6666666666666666297, 0.6805555555555555802, 0.6944444444444444198, 0.7083333333333333703, 0.7222222222222222099, 0.7361111111111111605, 0.7500000000000000000, 0.7638888888888888395, 0.7777777777777777901, 0.7916666666666666297, 0.8055555555555555802, 0.8194444444444444198, 0.8333333333333333703, 0.8472222222222222099, 0.8611111111111111605, 0.8750000000000000000, 0.8888888888888888395, 0.9027777777777777901, 0.9166666666666666297, 0.9305555555555555802, 0.9444444444444444198, 0.9523586263115634276 ),
 .UNSPECIFIED. ) 
 GEOMETRIC_REPRESENTATION_ITEM ( )  RATIONAL_B_SPLINE_SURFACE ( (
 ( 1.000000000000000000, 0.8660254037844387076, 1.000000000000000000, 0.8660254037844387076, 1.000000000000000000, 0.8660254037844387076, 1.000000000000000000, 0.8660254037844387076, 1.000000000000000000, 0.8660254037844387076, 1.000000000000000000, 0.8660254037844387076, 1.000000000000000000, 0.8660254037844387076, 1.000000000000000000, 0.8660254037844387076, 1.000000000000000000, 0.8660254037844387076, 1.000000000000000000, 0.8660254037844387076, 1.000000000000000000, 0.8660254037844387076, 1.000000000000000000, 0.8660254037844387076, 1.000000000000000000, 0.8660254037844387076, 1.000000000000000000, 0.8660254037844387076, 1.000000000000000000, 0.8660254037844387076, 1.000000000000000000, 0.8660254037844387076, 1.000000000000000000, 0.8660254037844387076, 1.000000000000000000, 0.8660254037844387076, 1.000000000000000000, 0.8660254037844387076, 1.000000000000000000, 0.8660254037844387076, 1.000000000000000000, 0.8660254037844387076, 1.000000000000000000, 0.8660254037844387076, 1.000000000000000000, 0.8660254037844387076, 1.000000000000000000, 0.8660254037844387076, 1.000000000000000000, 0.8660254037844387076, 1.000000000000000000, 0.8660254037844387076, 1.000000000000000000, 0.8660254037844387076, 1.000000000000000000, 0.8660254037844387076, 1.000000000000000000, 0.8660254037844387076, 1.000000000000000000, 0.8660254037844387076, 1.000000000000000000, 0.8660254037844387076, 1.000000000000000000, 0.8660254037844387076, 1.000000000000000000, 0.8660254037844387076, 1.000000000000000000, 0.8660254037844387076, 1.000000000000000000, 0.8660254037844387076, 1.000000000000000000, 0.8660254037844387076, 1.000000000000000000, 0.8660254037844387076, 1.000000000000000000, 0.8660254037844387076, 1.000000000000000000, 0.8660254037844387076, 1.000000000000000000, 0.8660254037844387076, 1.000000000000000000, 0.8660254037844387076, 1.000000000000000000, 0.8660254037844387076, 1.000000000000000000, 0.8660254037844387076, 1.000000000000000000, 0.8660254037844387076, 1.000000000000000000, 0.8660254037844387076, 1.000000000000000000, 0.8660254037844387076, 1.000000000000000000, 0.8660254037844387076, 1.000000000000000000, 0.8660254037844387076, 1.000000000000000000, 0.8660254037844387076, 1.000000000000000000, 0.8660254037844387076, 1.000000000000000000, 0.8660254037844387076, 1.000000000000000000, 0.8660254037844387076, 1.000000000000000000, 0.8660254037844387076, 1.000000000000000000, 0.8660254037844387076, 1.000000000000000000, 0.8660254037844387076, 1.000000000000000000, 0.8660254037844387076, 1.000000000000000000, 0.8660254037844387076, 1.000000000000000000, 0.8660254037844387076, 1.000000000000000000, 0.8660254037844387076, 1.000000000000000000, 0.8660254037844387076, 1.000000000000000000, 0.8660254037844387076, 1.000000000000000000, 0.8660254037844387076, 1.000000000000000000, 0.8660254037844387076, 1.000000000000000000, 0.8660254037844387076, 1.000000000000000000, 0.8660254037844387076, 1.000000000000000000, 0.8660254037844387076, 1.000000000000000000, 0.8660254037844387076, 1.000000000000000000, 0.8660254037844387076, 1.000000000000000000, 0.9236584489582877477, 0.9343189502471116459),
 ( 1.000000000000000000, 0.8660254037844387076, 1.000000000000000000, 0.8660254037844387076, 1.000000000000000000, 0.8660254037844387076, 1.000000000000000000, 0.8660254037844387076, 1.000000000000000000, 0.8660254037844387076, 1.000000000000000000, 0.8660254037844387076, 1.000000000000000000, 0.8660254037844387076, 1.000000000000000000, 0.8660254037844387076, 1.000000000000000000, 0.8660254037844387076, 1.000000000000000000, 0.8660254037844387076, 1.000000000000000000, 0.8660254037844387076, 1.000000000000000000, 0.8660254037844387076, 1.000000000000000000, 0.8660254037844387076, 1.000000000000000000, 0.8660254037844387076, 1.000000000000000000, 0.8660254037844387076, 1.000000000000000000, 0.8660254037844387076, 1.000000000000000000, 0.8660254037844387076, 1.000000000000000000, 0.8660254037844387076, 1.000000000000000000, 0.8660254037844387076, 1.000000000000000000, 0.8660254037844387076, 1.000000000000000000, 0.8660254037844387076, 1.000000000000000000, 0.8660254037844387076, 1.000000000000000000, 0.8660254037844387076, 1.000000000000000000, 0.8660254037844387076, 1.000000000000000000, 0.8660254037844387076, 1.000000000000000000, 0.8660254037844387076, 1.000000000000000000, 0.8660254037844387076, 1.000000000000000000, 0.8660254037844387076, 1.000000000000000000, 0.8660254037844387076, 1.000000000000000000, 0.8660254037844387076, 1.000000000000000000, 0.8660254037844387076, 1.000000000000000000, 0.8660254037844387076, 1.000000000000000000, 0.8660254037844387076, 1.000000000000000000, 0.8660254037844387076, 1.000000000000000000, 0.8660254037844387076, 1.000000000000000000, 0.8660254037844387076, 1.000000000000000000, 0.8660254037844387076, 1.000000000000000000, 0.8660254037844387076, 1.000000000000000000, 0.8660254037844387076, 1.000000000000000000, 0.8660254037844387076, 1.000000000000000000, 0.8660254037844387076, 1.000000000000000000, 0.8660254037844387076, 1.000000000000000000, 0.8660254037844387076, 1.000000000000000000, 0.8660254037844387076, 1.000000000000000000, 0.8660254037844387076, 1.000000000000000000, 0.8660254037844387076, 1.000000000000000000, 0.8660254037844387076, 1.000000000000000000, 0.8660254037844387076, 1.000000000000000000, 0.8660254037844387076, 1.000000000000000000, 0.8660254037844387076, 1.000000000000000000, 0.8660254037844387076, 1.000000000000000000, 0.8660254037844387076, 1.000000000000000000, 0.8660254037844387076, 1.000000000000000000, 0.8660254037844387076, 1.000000000000000000, 0.8660254037844387076, 1.000000000000000000, 0.8660254037844387076, 1.000000000000000000, 0.8660254037844387076, 1.000000000000000000, 0.8660254037844387076, 1.000000000000000000, 0.8660254037844387076, 1.000000000000000000, 0.8660254037844387076, 1.000000000000000000, 0.8660254037844387076, 1.000000000000000000, 0.8660254037844387076, 1.000000000000000000, 0.8660254037844387076, 1.000000000000000000, 0.8660254037844387076, 1.000000000000000000, 0.8660254037844387076, 1.000000000000000000, 0.8660254037844387076, 1.000000000000000000, 0.8660254037844387076, 1.000000000000000000, 0.8660254037844387076, 1.000000000000000000, 0.9236584489582877477, 0.9343189502471116459) ) ) 
 REPRESENTATION_ITEM ( '' )  SURFACE ( )  );
#58709 = CARTESIAN_POINT ( 'NONE',  ( 2.770184829093131462, -2.147865496273542174, 0.3164581508635355145 ) ) ;
#58710 = CARTESIAN_POINT ( 'NONE',  ( 3.274625289317079524, -0.3981104328964027994, -1.976669913042613747 ) ) ;
#58711 = CARTESIAN_POINT ( 'NONE',  ( 3.843750000000002220, 1.895863743164162063, 0.7852924748297951396 ) ) ;
#58712 = CARTESIAN_POINT ( 'NONE',  ( 1.499999999999987121, 2.327083334016154303, -0.8660254037844262731 ) ) ;
#58713 = CARTESIAN_POINT ( 'NONE',  ( 0.9207747878037384481, 1.778742719161881203, 0.7400954639872597829 ) ) ;
#58714 = CARTESIAN_POINT ( 'NONE',  ( -1.364683531250000748, 14.35937500034140157, 0.000000000000000000 ) ) ;
#58715 = CARTESIAN_POINT ( 'NONE',  ( 3.656649667753679278, 2.210956852819144114, 0.2149545701610345305 ) ) ;
#58716 = VERTEX_POINT ( 'NONE', #137496 ) ;
#58717 = CARTESIAN_POINT ( 'NONE',  ( 0.7499999999999885647, 0.4833333333333564297, 1.299038105676657340 ) ) ;
#58718 = CARTESIAN_POINT ( 'NONE',  ( 6.968000882419564945, 10.21675256520979858, 1.199719254218460707 ) ) ;
#58719 = CARTESIAN_POINT ( 'NONE',  ( 0.6823417656249882723, -0.4072916663252490466, 1.181850606188755259 ) ) ;
#58720 = CARTESIAN_POINT ( 'NONE',  ( 0.04794026018281431767, -2.028123841075918588, 0.9064578031776747702 ) ) ;
#58721 = CARTESIAN_POINT ( 'NONE',  ( 4.633228507203630997, 0.002057781214020309134, -1.962046631861932067 ) ) ;
#58723 = CARTESIAN_POINT ( 'NONE',  ( -6.073689629242165822, 7.148687991279732756, -1.082531754730544860 ) ) ;
#58722 = CARTESIAN_POINT ( 'NONE',  ( 8.758204044747998296, 11.24099069033793974, 1.443375672974076540 ) ) ;
#58724 = AXIS2_PLACEMENT_3D ( 'NONE', #102819, #88713, #20478 ) ;
#58725 =( NAMED_UNIT ( * ) SI_UNIT ( $, .STERADIAN. ) SOLID_ANGLE_UNIT ( ) );
#58726 = CARTESIAN_POINT ( 'NONE',  ( 5.220128827380259295, -1.204132088723122385, -1.915181361845545105 ) ) ;
#58727 = CARTESIAN_POINT ( 'NONE',  ( -4.990809943606269172, 8.836712344267034780, -0.7216878364870338292 ) ) ;
#58728 = CARTESIAN_POINT ( 'NONE',  ( 2.453648911872767346, 1.593012163857405961, 1.310297011819524293 ) ) ;
#58729 = CARTESIAN_POINT ( 'NONE',  ( -4.880045225915050189, 7.780804299287790826, 1.199719254218464037 ) ) ;
#58730 = EDGE_LOOP ( 'NONE', ( #55048, #17160, #111855, #113806 ) ) ;
#58731 = CARTESIAN_POINT ( 'NONE',  ( -0.7500000000000215383, 2.222916667349486453, 1.299038105676671107 ) ) ;
#58732 = CARTESIAN_POINT ( 'NONE',  ( -0.6823417656249969321, 3.780208333674754506, -1.181850606188749264 ) ) ;
#58733 = CARTESIAN_POINT ( 'NONE',  ( 3.303821147848403861, -1.868562489643767144, 0.08839296284299941187 ) ) ;
#58734 = CARTESIAN_POINT ( 'NONE',  ( 3.076526641549358398, -0.6997103666757237272, 1.586905598789583482 ) ) ;
#58735 = CARTESIAN_POINT ( 'NONE',  ( 0.5040057298127769148, -2.280580521882575429, 0.2324455964911649464 ) ) ;
#58736 = CARTESIAN_POINT ( 'NONE',  ( 0.6576010401811819284, -1.865379905010958517, -1.178792301215730642 ) ) ;
#58737 = CARTESIAN_POINT ( 'NONE',  ( 4.107036007299074143, -0.3554739980045698022, 2.060130632118581051 ) ) ;
#58738 = CARTESIAN_POINT ( 'NONE',  ( 5.753840666697315420, 0.7890659797671593090, 1.774590222461839506 ) ) ;
#58740 = ORIENTED_EDGE ( 'NONE', *, *, #183211, .T. ) ;
#58739 = DIRECTION ( 'NONE',  ( -0.000000000000000000, 1.000000000000000000, -0.000000000000000000 ) ) ;
#58741 = CARTESIAN_POINT ( 'NONE',  ( 0.2499999969303341174, 7.552774431159578439E-08, 2.052068128417954274 ) ) ;
#58742 = CARTESIAN_POINT ( 'NONE',  ( 0.5103889644224939293, -1.913802852362625151, 0.6352017490645140985 ) ) ;
#58743 = CARTESIAN_POINT ( 'NONE',  ( -1.852123800559039468, 2.268197483979258082E-16, 0.4894596299587841703 ) ) ;
#58744 = DIRECTION ( 'NONE',  ( 0.000000000000000000, -1.000000000000000000, 0.000000000000000000 ) ) ;
#58745 = CARTESIAN_POINT ( 'NONE',  ( -8.341290820905609138, 10.75459192918846618, 1.599625672291269396 ) ) ;
#58746 = CARTESIAN_POINT ( 'NONE',  ( 6.500244582748090139, 9.671036882259738121, 1.199719254218460707 ) ) ;
#58747 = DIRECTION ( 'NONE',  ( 0.000000000000000000, 0.000000000000000000, -1.000000000000000000 ) ) ;
#58748 = CARTESIAN_POINT ( 'NONE',  ( 4.547361323050268744, -1.413013347330991598, -1.156083184146582177 ) ) ;
#58749 = CARTESIAN_POINT ( 'NONE',  ( 2.081372155488591780, -0.1082299263688718260, -2.204229314041641352 ) ) ;
#58750 = ORIENTED_EDGE ( 'NONE', *, *, #73552, .F. ) ;
#58751 = CARTESIAN_POINT ( 'NONE',  ( -5.921879234118920365, 10.13088588310589699, 0.000000000000000000 ) ) ;
#58752 = EDGE_CURVE ( 'NONE', #60255, #112565, #203512, .T. ) ;
#58753 = CARTESIAN_POINT ( 'NONE',  ( 3.285556943750000514, -1.801041666188707424, 1.896917185911906500 ) ) ;
#58754 = CARTESIAN_POINT ( 'NONE',  ( -6.984421689334302741, 11.30024240419870374, 0.000000000000000000 ) ) ;
#58755 = CARTESIAN_POINT ( 'NONE',  ( 1.441672106306312484, -1.900340447277752087, 0.6846001189487918026 ) ) ;
#58756 = CARTESIAN_POINT ( 'NONE',  ( 0.3554123170485448124, 15.00000000000058265, -12.67999999502907471 ) ) ;
#58757 = CARTESIAN_POINT ( 'NONE',  ( -3.786470039966538970, 7.639575156594750283, 0.000000000000000000 ) ) ;
#58758 = CARTESIAN_POINT ( 'NONE',  ( 3.238934005158759621, -0.1320712000743811398, -1.856290971584534377 ) ) ;
#58759 = CARTESIAN_POINT ( 'NONE',  ( 4.552840656090682891, 4.206068941727564514, 1.214306433183764966E-14 ) ) ;
#58760 = CARTESIAN_POINT ( 'NONE',  ( 6.387299765813869712, 6.624473612970537495, 0.000000000000000000 ) ) ;
#58761 = ORIENTED_EDGE ( 'NONE', *, *, #205304, .T. ) ;
#58762 = CARTESIAN_POINT ( 'NONE',  ( -6.064574784014443942, 5.969758757638621738, -0.7998128361456291469 ) ) ;
#58763 = CARTESIAN_POINT ( 'NONE',  ( -8.833300774503376473, 10.26427131079744193, 1.199719254218462483 ) ) ;
#58764 = CARTESIAN_POINT ( 'NONE',  ( 3.703562413045482060, -0.5285312144065814621, 1.747510042522756990 ) ) ;
#58766 = CARTESIAN_POINT ( 'NONE',  ( 1.173530994449854870, -3.042800438942089514, 3.270848514539542506 ) ) ;
#58765 = CARTESIAN_POINT ( 'NONE',  ( -6.400331034103001748, 9.624747418832267698, 1.199719254218452935 ) ) ;
#58767 = CARTESIAN_POINT ( 'NONE',  ( 6.590809034589254267, 6.776089313701147532, -0.2235409772415736240 ) ) ;
#58768 = CARTESIAN_POINT ( 'NONE',  ( 0.9129801003131752246, 0.4962884120854795245, 1.661303041287894411 ) ) ;
#58769 = CARTESIAN_POINT ( 'NONE',  ( 6.351489326974223637, 1.835832825663574752, -0.1405570519043483624 ) ) ;
#58770 = CARTESIAN_POINT ( 'NONE',  ( 4.811288673970230967, 2.006026520401600788, 1.140621419682581239 ) ) ;
#58771 = CARTESIAN_POINT ( 'NONE',  ( 4.878955176071345434, 6.785476686873604280, -1.599625672291269396 ) ) ;
#58772 = CARTESIAN_POINT ( 'NONE',  ( 6.714160596891073141, -1.012370167489636819, -1.909856561116265450 ) ) ;
#58773 = CARTESIAN_POINT ( 'NONE',  ( 5.635385404774530649, 9.726366738878972740, 0.7998128361456462443 ) ) ;
#58774 = AXIS2_PLACEMENT_3D ( 'NONE', #197951, #210997, #163344 ) ;
#58775 = ADVANCED_FACE ( 'NONE', ( #191538 ), #205661, .F. ) ;
#58776 = CARTESIAN_POINT ( 'NONE',  ( 5.536544918007444416, 2.217299919257350371, -0.6050018498083614693 ) ) ;
#58777 = CARTESIAN_POINT ( 'NONE',  ( 0.4019237886466778820, 11.35491455036742536, 1.500000000000001554 ) ) ;
#58778 = CARTESIAN_POINT ( 'NONE',  ( -6.994027139803241866, 9.253060644560830994, -1.599625672291271394 ) ) ;
#58779 = CARTESIAN_POINT ( 'NONE',  ( 5.524238439434661530, 1.113281918156138639, -1.503147240406087271 ) ) ;
#58781 = CARTESIAN_POINT ( 'NONE',  ( -5.581116510680924847, 6.540332679663050541, -1.199719254218453823 ) ) ;
#58780 = CARTESIAN_POINT ( 'NONE',  ( 2.689602200614676697, 1.814610489020528350, -0.6038049036062518304 ) ) ;
#58782 = CARTESIAN_POINT ( 'NONE',  ( 3.932405576212230525, 1.181341412803040614, -1.863887651898883613 ) ) ;
#58783 = CARTESIAN_POINT ( 'NONE',  ( 4.241493788847498614, 0.4602237217972443561, -2.066584722733503909 ) ) ;
#58784 = CARTESIAN_POINT ( 'NONE',  ( -1.225000000000040057, 0.5833333340161187541, 0.7072540797572817173 ) ) ;
#58785 = CARTESIAN_POINT ( 'NONE',  ( 6.983263157960366563, 2.432509251381759441, 2.428019605373044509 ) ) ;
#58786 = CARTESIAN_POINT ( 'NONE',  ( 4.516274566683592617, 8.283087737857252719, -0.7216878364870357165 ) ) ;
#58787 = CARTESIAN_POINT ( 'NONE',  ( -5.926322542504877333, 7.047036066744706950, -1.082531754730549967 ) ) ;
#58788 = ADVANCED_FACE ( 'NONE', ( #91952 ), #204581, .F. ) ;
#58789 = CARTESIAN_POINT ( 'NONE',  ( 2.433052891977859566, 2.238319448195260186, 0.5606502339033142546 ) ) ;
#58790 = CARTESIAN_POINT ( 'NONE',  ( 2.998438581075290710, 1.946722116546204306, 0.2428724957088539971 ) ) ;
#58791 = CARTESIAN_POINT ( 'NONE',  ( 11.41381675112453387, 10.89999999999998259, 3.704697986577180302 ) ) ;
#58792 = CARTESIAN_POINT ( 'NONE',  ( 6.965701137139799215, -0.4614044149895025204, 2.017943399502773349 ) ) ;
#58793 = CARTESIAN_POINT ( 'NONE',  ( 4.365362273920250225, 5.155639410070820716, 1.082531754730560403 ) ) ;
#58794 = CARTESIAN_POINT ( 'NONE',  ( 3.366167277942881064, 7.149221934233827014, -0.7998128361456362523 ) ) ;
#58795 = VERTEX_POINT ( 'NONE', #113325 ) ;
#58796 = CARTESIAN_POINT ( 'NONE',  ( 4.856657812281613751, -1.900414607462055816, -0.6748505307947461063 ) ) ;
#58797 = CARTESIAN_POINT ( 'NONE',  ( -9.053093885623068715, 11.58502883802551153, -1.599625672291263179 ) ) ;
#58798 = DIRECTION ( 'NONE',  ( -0.6507913734559606089, 0.7592566023653033458, 0.000000000000000000 ) ) ;
#58799 = CARTESIAN_POINT ( 'NONE',  ( 2.969872605471104876, 6.605953636086679737, -0.06813560672779371552 ) ) ;
#58800 = CARTESIAN_POINT ( 'NONE',  ( 4.324687812634897988, 4.147816657603229373, 0.7216878364870317197 ) ) ;
#58801 = CARTESIAN_POINT ( 'NONE',  ( 2.413135165516873126, -1.680682958684741823, 1.374403011902309402 ) ) ;
#58802 = CARTESIAN_POINT ( 'NONE',  ( 6.933263157960367629, 7.629137130509066722, 2.653810918356712900 ) ) ;
#58803 = B_SPLINE_CURVE_WITH_KNOTS ( 'NONE', 3,
 ( #104058, #151746, #170104, #24916, #109457, #128911, #95294, #161343, #91020, #94226, #158146, #76868, #25984, #108382, #125714, #107312, #28130, #11866, #9738, #8670, #93156, #157082 ),
 .UNSPECIFIED., .F., .F.,
 ( 4, 2, 2, 2, 2, 2, 2, 2, 2, 2, 4 ),
 ( 0.5001299408125404744, 0.5533639344558343165, 0.5799809312774814041, 0.6065979280991283806, 0.6598319217424222227, 0.6864489185640691993, 0.7130659153857161758, 0.7662999090290101289, 0.8195339026723040821, 0.8727678963155980352, 0.9260018899588919883 ),
 .UNSPECIFIED. ) ;
#58804 = CARTESIAN_POINT ( 'NONE',  ( -1.538741480077424601E-10, 14.53091781611522748, -12.00000000000003375 ) ) ;
#58805 = CARTESIAN_POINT ( 'NONE',  ( 4.515632184204340760, 7.124593881049110955, 1.261186505319204398 ) ) ;
#58806 = CARTESIAN_POINT ( 'NONE',  ( 5.678247172832384670, 7.430942480705488684, 1.324022058552588366 ) ) ;
#58807 = CARTESIAN_POINT ( 'NONE',  ( 1.300152579660202923, -2.060967562519558705, -0.002860995899278336550 ) ) ;
#58809 = CARTESIAN_POINT ( 'NONE',  ( 6.727182134110237577, 2.455520393281558356, 2.294684051055717600 ) ) ;
#58808 = CARTESIAN_POINT ( 'NONE',  ( -0.02244404828160087226, 4.081832076214893412, -2.743766916979750281 ) ) ;
#58810 = CARTESIAN_POINT ( 'NONE',  ( -1.201851678989727383E-14, 1.071875000341418138, 1.575800808251672791 ) ) ;
#58811 = DIRECTION ( 'NONE',  ( 0.000000000000000000, 0.000000000000000000, -1.000000000000000000 ) ) ;
#58812 = VERTEX_POINT ( 'NONE', #30953 ) ;
#58813 = CARTESIAN_POINT ( 'NONE',  ( 3.018110381800835018, -1.909997030407738938, 0.09613604992317337228 ) ) ;
#58814 = STYLED_ITEM ( 'NONE', ( #169287 ), #181761 ) ;
#58815 = CARTESIAN_POINT ( 'NONE',  ( 4.750734298983296355, -1.420434005603900429, 1.055588576545069657 ) ) ;
#58816 = CARTESIAN_POINT ( 'NONE',  ( 2.191926089937683564, 1.177725938178806997, 1.506473034612793915 ) ) ;
#58817 = CARTESIAN_POINT ( 'NONE',  ( -4.928552533767591726, 5.708731696605642725, 1.199719254218462483 ) ) ;
#58819 = CARTESIAN_POINT ( 'NONE',  ( 0.2158530320381162604, 0.9822752966809102926, -1.644539037099991718 ) ) ;
#58818 = CARTESIAN_POINT ( 'NONE',  ( -11.41381675112453387, 19.00000000000000000, -3.704697986577182522 ) ) ;
#58820 = CARTESIAN_POINT ( 'NONE',  ( 1.499999999999989120, 0.2750000000000182854, 0.000000000000000000 ) ) ;
#58821 = CARTESIAN_POINT ( 'NONE',  ( 0.7661813929631040576, -2.060537521029872643, 0.2012509062776293156 ) ) ;
#58822 = CARTESIAN_POINT ( 'NONE',  ( -1.499999999999997780, 5.650000000000023448, 1.214306433183764966E-14 ) ) ;
#58823 = CARTESIAN_POINT ( 'NONE',  ( 6.157094445334826638, -1.605393284960114242, -0.9600186418455139981 ) ) ;
#58824 = CARTESIAN_POINT ( 'NONE',  ( 2.191784710619415044, -0.7813054520266484726, 1.650194661559079456 ) ) ;
#58826 = CARTESIAN_POINT ( 'NONE',  ( 4.594471896879979589, 8.374412622790375238, -0.01639726577711345112 ) ) ;
#58825 = CARTESIAN_POINT ( 'NONE',  ( 5.848300530743933301, 2.204158087718602221, 0.1119919437090263481 ) ) ;
#58827 = CARTESIAN_POINT ( 'NONE',  ( 1.364683531249986537, 0.9052083336747533959, -0.7879004041258239610 ) ) ;
#58828 = CARTESIAN_POINT ( 'NONE',  ( 3.121586329596927722, 0.3053734461533639255, -2.039847365138738766 ) ) ;
#58829 = CARTESIAN_POINT ( 'NONE',  ( -6.364663046611467756, 9.512858423433634414, 1.199719254218452047 ) ) ;
#58830 = CARTESIAN_POINT ( 'NONE',  ( 7.553864141108259211, 11.96459193126834464, 1.040834085586084257E-14 ) ) ;
#58831 = CARTESIAN_POINT ( 'NONE',  ( 5.515469562660962666, 5.329135999392899947, 0.7998128361456341429 ) ) ;
#58832 = CARTESIAN_POINT ( 'NONE',  ( 0.8608787451157869919, -1.566265403972837866, 1.489986575276234460 ) ) ;
#58833 = CARTESIAN_POINT ( 'NONE',  ( 5.643937085038755797, 9.806620042512378177, -0.7998128361456481317 ) ) ;
#58834 = CARTESIAN_POINT ( 'NONE',  ( 5.547352688424546763, 1.827615396715172258, -0.9727077141251788683 ) ) ;
#58835 = CARTESIAN_POINT ( 'NONE',  ( 0.6823417656249882723, -0.01145833299191073573, -1.181850606188749264 ) ) ;
#58836 = CARTESIAN_POINT ( 'NONE',  ( 2.477987356985793088, 1.327747062846416526, 1.705691702009938915 ) ) ;
#58837 = CARTESIAN_POINT ( 'NONE',  ( -4.675522092136524144, 8.294237829558845476, 0.5223692772225538850 ) ) ;
#58839 = CARTESIAN_POINT ( 'NONE',  ( 2.453501617077270769, 1.514643136537169310, 1.246875331876770243 ) ) ;
#58838 = CARTESIAN_POINT ( 'NONE',  ( 2.842449411481930532, 1.120122121419616423, -1.680381219987029606 ) ) ;
#58840 = CARTESIAN_POINT ( 'NONE',  ( 6.620655732516649294, 2.950034989283246478, 2.626075342966327497 ) ) ;
#58842 = CARTESIAN_POINT ( 'NONE',  ( 5.829642864196151741, 9.745074408296771296, 0.7216878364870438212 ) ) ;
#58841 = CARTESIAN_POINT ( 'NONE',  ( 1.001543065824772753E-15, -0.6125000000000012657, 4.012584370867899430 ) ) ;
#58843 = CARTESIAN_POINT ( 'NONE',  ( -6.794571259104023930, 7.956029886156682274, 1.199719254218452047 ) ) ;
#58844 = CARTESIAN_POINT ( 'NONE',  ( 1.042204282965590201, 0.8216761606248854655, 1.841732292558920570 ) ) ;
#58845 = B_SPLINE_CURVE_WITH_KNOTS ( 'NONE', 3,
 ( #19987, #167331, #169453, #151093, #138038, #88211, #69792, #67650 ),
 .UNSPECIFIED., .F., .F.,
 ( 4, 2, 2, 4 ),
 ( 1.064029803361153984E-15, 0.0004636157603174426438, 0.0006954236404756319748, 0.0009272315206338212516 ),
 .UNSPECIFIED. ) ;
#58847 = CARTESIAN_POINT ( 'NONE',  ( 6.392125918040960642, -0.5824770489515176397, -2.112646119873210271 ) ) ;
#58846 = CARTESIAN_POINT ( 'NONE',  ( -6.227272627378437342, 6.159572908229946187, -0.7998128361456291469 ) ) ;
#58848 = CARTESIAN_POINT ( 'NONE',  ( -10.91962425643199808, -9.919999999999998153, 0.09058751758333691284 ) ) ;
#58849 = CARTESIAN_POINT ( 'NONE',  ( 5.994389040191066442, -1.017321598621454548, 1.619163160827830517 ) ) ;
#58850 = CARTESIAN_POINT ( 'NONE',  ( -2.252626078164912560, 5.779814191167667481, 0.7998128361456341429 ) ) ;
#58851 = CARTESIAN_POINT ( 'NONE',  ( 6.304178240230120522, 6.457222156464352381, -0.7216878364870257245 ) ) ;
#58853 = CARTESIAN_POINT ( 'NONE',  ( 2.741814726283864800, 2.006445297011373974, -0.2004551355171620974 ) ) ;
#58852 = CARTESIAN_POINT ( 'NONE',  ( -8.473482818416664841, 11.86918514058604757, -1.082531754730543083 ) ) ;
#58854 = CARTESIAN_POINT ( 'NONE',  ( -1.500000000000013101, 3.379166666666691299, -0.8660254037844313801 ) ) ;
#58855 = CARTESIAN_POINT ( 'NONE',  ( -1.364683531250010295, 14.19270833367473195, 0.7879004041258445001 ) ) ;
#58856 = CARTESIAN_POINT ( 'NONE',  ( 6.545920775329808983, 0.6544052999908689383, -1.596017746584824426 ) ) ;
#58857 = CARTESIAN_POINT ( 'NONE',  ( 5.027041095616958444, 9.086908054853605421, 0.000000000000000000 ) ) ;
#58858 = CARTESIAN_POINT ( 'NONE',  ( 9.246297574839974942, 11.81043314211192019, 1.443375672974076540 ) ) ;
#58859 = CARTESIAN_POINT ( 'NONE',  ( 6.830415307812257808, -7.473374494058229622, 6.717278222822394618 ) ) ;
#58860 = CARTESIAN_POINT ( 'NONE',  ( 4.340975799156801429, -1.628549031532234403, 0.9200136957008757665 ) ) ;
#58861 = CARTESIAN_POINT ( 'NONE',  ( 1.604436975501881468, 2.067711310959176707, 0.1055696395834623824 ) ) ;
#58862 = B_SPLINE_CURVE_WITH_KNOTS ( 'NONE', 3,
 ( #57362, #174334, #25912, #172189, #107244, #121377, #21616, #59486 ),
 .UNSPECIFIED., .F., .F.,
 ( 4, 2, 2, 4 ),
 ( 7.521151966117911075E-18, 0.0002224730689913869807, 0.0004449461379827664804, 0.0008898922759655229862 ),
 .UNSPECIFIED. ) ;
#58863 = CARTESIAN_POINT ( 'NONE',  ( 0.000000000000000000, 3.500000000000003109, 0.000000000000000000 ) ) ;
#58864 = ORIENTED_EDGE ( 'NONE', *, *, #118985, .T. ) ;
#58865 = CARTESIAN_POINT ( 'NONE',  ( 4.041212305325117882, 6.872442235258051646, -1.199719254218448494 ) ) ;
#58866 = FILL_AREA_STYLE ('',( #43709 ) ) ;
#58867 = CARTESIAN_POINT ( 'NONE',  ( 0.5447927104418804900, 0.1337802856970966847, 1.806726864048732173 ) ) ;
#58868 = ADVANCED_FACE ( 'NONE', ( #7458 ), #56231, .F. ) ;
#58869 = CARTESIAN_POINT ( 'NONE',  ( 6.360183458142179447, 6.592837920686898556, -0.7216878364870458196 ) ) ;
#58870 = CARTESIAN_POINT ( 'NONE',  ( 11.63272104808981666, 8.261185799347773084, 2.974823062023182363 ) ) ;
#58871 = ORIENTED_EDGE ( 'NONE', *, *, #83547, .F. ) ;
#58872 = CARTESIAN_POINT ( 'NONE',  ( 8.473482818416664841, 10.90881592628469932, -1.443375672974063439 ) ) ;
#58873 = VECTOR ( 'NONE', #147470, 1000.000000000000000 ) ;
#58875 = CARTESIAN_POINT ( 'NONE',  ( 8.450809820019639318, 8.753699632978056755, -0.7998128361456291469 ) ) ;
#58874 = CARTESIAN_POINT ( 'NONE',  ( 1.029656018189710309, 1.891699080040713410, -0.5197978237033785698 ) ) ;
#58876 = CARTESIAN_POINT ( 'NONE',  ( 4.587445725801254426, -0.5070264450876013074, 1.847228357985892577 ) ) ;
#58877 = CARTESIAN_POINT ( 'NONE',  ( -11.48784849554592924, 13.83049527181932348, 3.469614872287846374 ) ) ;
#58878 = CARTESIAN_POINT ( 'NONE',  ( -1.967994056399313907, -3.170678274948564468, 2.724402440660230962 ) ) ;
#58879 = CARTESIAN_POINT ( 'NONE',  ( 10.72180055030867329, 11.40318881831530540, 0.7998128361456341429 ) ) ;
#58880 = B_SPLINE_CURVE_WITH_KNOTS ( 'NONE', 3,
 ( #169041, #17435, #151745, #70448, #120374, #83519, #52101 ),
 .UNSPECIFIED., .F., .F.,
 ( 4, 3, 4 ),
 ( -0.0002318125648490880985, 0.000000000000000000, 0.0004044109710639508877 ),
 .UNSPECIFIED. ) ;
#58881 = CARTESIAN_POINT ( 'NONE',  ( 6.825078400183573812, 0.002648415797040087893, 1.855566311045192540 ) ) ;
#58883 = ORIENTED_EDGE ( 'NONE', *, *, #76553, .F. ) ;
#58882 = CARTESIAN_POINT ( 'NONE',  ( 3.714570900464269076, 7.277490450609545469, 0.7216878364870298324 ) ) ;
#58884 = CARTESIAN_POINT ( 'NONE',  ( -8.365017589951714072, 8.861534731139549592, 1.040834085586084257E-14 ) ) ;
#58885 = CARTESIAN_POINT ( 'NONE',  ( 2.571340117545738657, 0.1069729528509130723, -2.159185227005658181 ) ) ;
#58886 = CARTESIAN_POINT ( 'NONE',  ( -4.339491684825780737, 7.220434844675483355, -1.199719254218455378 ) ) ;
#58887 = EDGE_CURVE ( 'NONE', #8679, #47758, #69750, .T. ) ;
#58888 = CARTESIAN_POINT ( 'NONE',  ( 4.577813143269636065, 5.369812084349879555, -1.199719254218450271 ) ) ;
#58889 = CARTESIAN_POINT ( 'NONE',  ( -0.1225938595818750754, -1.897163925677572305, -0.9476133185889324961 ) ) ;
#58890 = CARTESIAN_POINT ( 'NONE',  ( 4.453998568579462969, 1.825179399820752169, -0.04523609120457571658 ) ) ;
#58892 = CARTESIAN_POINT ( 'NONE',  ( 9.941052257571969974, 9.384232882455165736, -7.145601325162150630 ) ) ;
#58891 =( BOUNDED_SURFACE ( )  B_SPLINE_SURFACE ( 1, 2, ( 
 ( #166559, #211019, #179614, #33347, #100484, #14943, #147125, #49603, #32292, #99429, #112537, #62643, #163368, #34412, #83157, #18148, #149237, #148186, #133024, #17080, #213151, #165483, #31235, #812, #66880, #199023, #63719, #46420, #84235, #129877, #128802, #195860, #194784, #178549, #30159, #96247, #13885, #50670, #79964, #98358, #214188, #65815, #164423, #47500, #146068, #212081, #113609, #97308, #16007, #81039, #182793, #64781, #82093, #130922, #115727, #116796, #196915, #131962, #48555, #114674, #197974, #181718, #101556, #137279, #85302, #167625, #121099, #153518, #19224, #151388, #72233, #188134, #21342, #2958, #69030, #70093, #170825, #6164, #35479, #169755, #154587, #138341, #118940, #150323, #88525, #86377, #204358, #152445, #4024, #183864, #203299, #67949, #39765, #105870, #56014, #122168, #135146, #53880, #87451, #104777, #171896, #23493, #168687, #1889, #54946, #134094, #187066, #200102, #51752, #136208, #117875, #202227, #22416, #103703, #201162, #52802, #184920, #36544, #38698, #5087, #102631, #120013, #71162, #185989, #37623, #20291, #109101, #159911, #92804, #156728, #59202, #140503, #125359, #10445, #73309, #108032, #90665, #57081, #176176, #111232, #190263, #174058, #61347, #124304, #9391, #139412, #44046, #75463, #175115, #155650, #25630, #208639, #77588, #76518, #91742, #206514, #11518, #127507, #42989, #141575, #74403, #172980, #60271, #58146, #8318, #191323, #40848, #143711, #189209, #7233, #123245, #26702, #110166, #41922, #157795, #205445, #126428, #207582, #158848, #142629, #192391, #27776, #93874, #209703, #106955, #193477, #45121, #177234, #89599, #24559, #48315, #195618, #130686, #115482, #16823, #94935, #64542, #162057, #148980, #160984, #181474, #99178, #13646, #555, #97070, #163123, #14705, #113368, #33104, #198769, #196676, #80799, #114426, #146889, #82907, #178311, #194534, #81852, #212909, #180427, #78647, #129631, #66619, #179374, #112295, #131718, #116538, #79718, #165230, #145835, #132766, #29920, #32044, #98131, #96003, #164182, #15767, #30995, #213950, #147934, #211839, #63477, #50419, #28847, #65571, #47254, #46181, #197722, #49362, #12575, #128570, #144774, #210783, #62406, #151129, #182528, #120824, #118675, #170553, #184659, #36279, #1630, #169492, #100227, #71965, #138075, #104509, #186800, #35212, #86114, #201954, #137007, #5893, #204088, #200895, #22136, #21074, #88249, #87176, #154319, #55741, #168428, #51489, #2696, #52542, #18957, #152184, #83969, #34158, #153242, #69828, #203034, #102356, #20024, #17885, #166295, #117611, #70896, #150058, #3754, #67689, #133835, #68769, #4815, #199846, #135936, #53611, #54675, #119744, #38429, #183603, #101287, #134888, #167369, #85041, #185723, #37356, #103431, #43797, #142374, #57879, #10191, #156463, #208384, #76265, #60015, #188941, #171624, #77333, #40580, #121897, #106686, #11255, #105590, #187865, #155379, #143446, #126168, #209443, #91474, #58949, #191065, #75206, #172711, #139143, #205171, #23218, #90393, #157535, #89331, #93612, #24287, #207329, #140232, #174863, #175921, #8049, #9130, #192132, #74139, #206254, #108837, #73044, #26442, #56813, #122983, #141316, #109910, #125107, #124041, #42729, #190008, #92552, #158592, #6963, #41658, #107771, #173797, #27513, #39493, #25373, #159657, #32854, #95750, #195360, #110969, #15513, #46992, #146634, #127247, #79469, #180175, #49117, #196424, #211583, #178049, #197473, #98929, #14447, #113109, #45928, #144518, #31801, #112048, #194284, #30736, #12317, #115237, #160724, #193217, #28594, #80538, #81598, #13392, #29666, #44864, #97877, #179114, #161802, #212650, #145586, #63219, #129381, #96818, #176976, #62162, #162867, #148741, #64291, #82657, #130437, #48069, #114181, #147683, #181226, #94681, #163937, #213700, #164983, #78398, #65323, #131471, #16574, #61088, #210526, #128320, #68522, #84797, #153002, #170306, #168186, #134649, #19785, #200654, #202791, #149813, #166052, #53364, #52303, #118432, #50173, #101037, #120583, #150885, #83722, #103188, #88005, #133592, #4579, #199596, #186560, #1386, #184420, #36037, #67447, #102117, #85867, #2448, #21895, #151943, #86936 ),
 ( #309, #3516, #51239, #183362, #18713, #117364, #69587, #116293, #38189, #201723, #135697, #169249, #119498, #185484, #182284, #104260, #34966, #20837, #33909, #37110, #66380, #132529, #167128, #70653, #198526, #136763, #54441, #99985, #17637, #45393, #55502, #154076, #106440, #194817, #29128, #46453, #95215, #94154, #78926, #177515, #90153, #111509, #188699, #161265, #12851, #145049, #6726, #203857, #112575, #72804, #5643, #138906, #178586, #137836, #71724, #187623, #30194, #211050, #121656, #123800, #160193, #11794, #110447, #204924, #171381, #22972, #39251, #122736, #189758, #105344, #128835, #56577, #28061, #172463, #209984, #62676, #40334, #44325, #89090, #24050, #156221, #143992, #155144, #61625, #7797, #73890, #127792, #77869, #139983, #206005, #57640, #176449, #193746, #97347, #47533, #16046, #116831, #166597, #195897, #115762, #100523, #18186, #64815, #96283, #34449, #32326, #84272, #98394, #164458, #129912, #83191, #13919, #200139, #51792, #150359, #1929, #163403, #214223, #181752, #50707, #134130, #117910, #114708, #67988, #149274, #183902, #854, #79999, #66920, #82129, #147160, #33384, #81074, #213187, #196951, #130961, #212115, #14978, #148222, #162334, #48591, #146104, #99464, #180703, #198011, #182833, #63752, #113646, #132001, #65852, #179651, #31272, #49639, #165522, #17114, #133061, #199061, #103738, #169789, #120051, #188168, #205482, #203330, #21378, #54984, #87486, #23527, #184953, #201200, #88562, #153553, #5123, #85342, #136244, #155686, #186025, #118975, #138378, #123283, #168725, #39801, #20327, #7269, #36580, #71198, #137315, #102668, #121137, #187099, #37662, #57114, #38733, #122206, #104814, #52839, #105909, #19260, #89634, #154621, #170859, #151423, #22450, #6200, #72269, #204396, #86413, #56050, #171935, #73346, #152480, #139447, #4060, #35513, #101591, #2996, #53914, #70131, #69064, #167659, #135184, #202264, #59234, #161015, #9427, #109137, #24595, #143745, #175150, #60304, #40885, #207617, #93909, #177269, #110199, #125392, #91773, #111265, #12610, #142663, #26737, #174093, #58179, #159949, #25665, #108066, #158882, #140537, #28885, #74437, #106989, #156765, #208673, #209740, #141609, #157830, #124339, #77623, #62440, #75496, #193512, #191358, #94968, #190296, #43024, #92838, #41954, #76554, #126463, #10479, #210815, #192426, #61383, #44081, #206550, #45153, #173014, #78684, #11552, #176209, #90703, #27810, #127540, #144809, #189246, #8352, #147971, #198808, #131751, #195654, #98165, #179408, #164212, #49395, #112333, #146922, #129668, #96040, #591, #150098, #14740, #212940, #100265, #163156, #48349, #178345, #82942, #114461, #213982, #194569, #64577, #33137, #116573, #115514, #130718, #31029, #50455, #166331, #81886, #180460, #113402, #211875, #99217, #97104, #47288, #15799, #79752, #182567, #13681, #46216, #162092, #65602, #149016, #80832, #196709, #29954, #165267, #32077, #197757, #181508, #16862, #66658, #132804, #34191, #145868, #17922, #84007, #1669, #128603, #63514, #87214, #20060, #169530, #154354, #55778, #133875, #103468, #200932, #187902, #199882, #5932, #138116, #52580, #39532, #135975, #201990, #53648, #152221, #72004, #23256, #21110, #119780, #153279, #185761, #121935, #2733, #18998, #120864, #37393, #4856, #117651, #168462, #105632, #3790, #86150, #118708, #70934, #183644, #171660, #54714, #137044, #22176, #69866, #203070, #35249, #89369, #68805, #170590, #101324, #186837, #155417, #67724, #36317, #104545, #51525, #38469, #88292, #204126, #167406, #85078, #151163, #134925, #184696, #102395, #93646, #44899, #159689, #158630, #143482, #27550, #157573, #109945, #41696, #11289, #175954, #77368, #74179, #56852, #177011, #140272, #7001, #206291, #111006, #205210, #73078, #40620, #28628, #209479, #94715, #191100, #10228, #76302, #174899, #57916, #24325, #90433, #123025, #190044, #42768, #188976, #193252, #124081, #92588, #25409, #60051, #61120, #107807, #108875, #127281, #173832, #91513, #208417, #172750, #126206, #156501, #8091, #192168, #142409, #9165, #75241, #139179, #106723, #43829, #141352, #207367, #58986, #125143, #26478, #45962, #180213, #165018, #16613 ) ),
 .UNSPECIFIED., .F., .F., .T. ) 
 B_SPLINE_SURFACE_WITH_KNOTS ( ( 2, 2 ),
 ( 3, 2, 2, 2, 2, 2, 2, 2, 2, 2, 2, 2, 2, 2, 2, 2, 2, 2, 2, 2, 2, 2, 2, 2, 2, 2, 2, 2, 2, 2, 2, 2, 2, 2, 2, 2, 2, 2, 2, 2, 2, 2, 2, 2, 2, 2, 2, 2, 2, 2, 2, 2, 2, 2, 2, 2, 2, 2, 2, 2, 2, 2, 2, 2, 2, 2, 2, 2, 2, 2, 2, 2, 2, 2, 2, 2, 2, 2, 2, 2, 2, 2, 2, 2, 2, 2, 2, 2, 2, 2, 2, 2, 2, 2, 2, 2, 2, 2, 2, 2, 2, 2, 2, 2, 2, 2, 2, 2, 2, 2, 2, 2, 2, 2, 2, 2, 2, 2, 2, 2, 2, 2, 2, 2, 2, 2, 2, 2, 2, 2, 2, 2, 2, 2, 2, 2, 2, 2, 2, 2, 2, 2, 2, 2, 2, 2, 2, 2, 2, 2, 2, 2, 2, 2, 2, 2, 2, 2, 2, 2, 2, 2, 2, 2, 2, 2, 2, 2, 2, 2, 2, 2, 2, 2, 2, 2, 2, 2, 2, 2, 2, 2, 2, 2, 2, 2, 2, 2, 2, 2, 2, 2, 2, 2, 2, 2, 2, 2, 2, 2, 2, 2, 2, 2, 2, 2, 2, 2, 2, 2, 2, 2, 2, 2, 2, 2, 2, 2, 2, 2, 2, 2, 2, 2, 2, 2, 2, 2, 2, 2, 2, 2, 2, 2, 2, 2, 2, 2, 2, 2, 3 ),
 ( 0.000000000000000000, 1.000000000000000000 ),
 ( 0.000000000000000000, 0.004166666666666666609, 0.008333333333333333218, 0.01250000000000000069, 0.01666666666666666644, 0.02083333333333333218, 0.02500000000000000139, 0.02916666666666666713, 0.03333333333333333287, 0.03749999999999999861, 0.04166666666666666435, 0.04583333333333333010, 0.05000000000000000278, 0.05416666666666666852, 0.05833333333333333426, 0.06250000000000000000, 0.06666666666666666574, 0.07083333333333333148, 0.07499999999999999722, 0.07916666666666666297, 0.08333333333333332871, 0.08749999999999999445, 0.09166666666666666019, 0.09583333333333333981, 0.1000000000000000056, 0.1041666666666666713, 0.1083333333333333370, 0.1125000000000000028, 0.1166666666666666685, 0.1208333333333333343, 0.1250000000000000000, 0.1291666666666666796, 0.1333333333333333315, 0.1375000000000000111, 0.1416666666666666630, 0.1458333333333333426, 0.1499999999999999944, 0.1541666666666666741, 0.1583333333333333259, 0.1625000000000000056, 0.1666666666666666574, 0.1708333333333333370, 0.1749999999999999889, 0.1791666666666666685, 0.1833333333333333204, 0.1875000000000000000, 0.1916666666666666796, 0.1958333333333333315, 0.2000000000000000111, 0.2041666666666666630, 0.2083333333333333426, 0.2124999999999999944, 0.2166666666666666741, 0.2208333333333333259, 0.2250000000000000056, 0.2291666666666666574, 0.2333333333333333370, 0.2374999999999999889, 0.2416666666666666685, 0.2458333333333333204, 0.2500000000000000000, 0.2541666666666666519, 0.2583333333333333592, 0.2625000000000000111, 0.2666666666666666630, 0.2708333333333333148, 0.2750000000000000222, 0.2791666666666666741, 0.2833333333333333259, 0.2874999999999999778, 0.2916666666666666852, 0.2958333333333333370, 0.2999999999999999889, 0.3041666666666666408, 0.3083333333333333481, 0.3125000000000000000, 0.3166666666666666519, 0.3208333333333333592, 0.3250000000000000111, 0.3291666666666666630, 0.3333333333333333148, 0.3375000000000000222, 0.3416666666666666741, 0.3458333333333333259, 0.3499999999999999778, 0.3541666666666666852, 0.3583333333333333370, 0.3624999999999999889, 0.3666666666666666408, 0.3708333333333333481, 0.3750000000000000000, 0.3791666666666666519, 0.3833333333333333592, 0.3875000000000000111, 0.3916666666666666630, 0.3958333333333333148, 0.4000000000000000222, 0.4041666666666666741, 0.4083333333333333259, 0.4124999999999999778, 0.4166666666666666852, 0.4208333333333333370, 0.4249999999999999889, 0.4291666666666666408, 0.4333333333333333481, 0.4375000000000000000, 0.4416666666666666519, 0.4458333333333333592, 0.4500000000000000111, 0.4541666666666666630, 0.4583333333333333148, 0.4625000000000000222, 0.4666666666666666741, 0.4708333333333333259, 0.4749999999999999778, 0.4791666666666666852, 0.4833333333333333370, 0.4874999999999999889, 0.4916666666666666408, 0.4958333333333333481, 0.5000000000000000000, 0.5041666666666666519, 0.5083333333333333037, 0.5124999999999999556, 0.5166666666666667185, 0.5208333333333333703, 0.5250000000000000222, 0.5291666666666666741, 0.5333333333333333259, 0.5374999999999999778, 0.5416666666666666297, 0.5458333333333332815, 0.5500000000000000444, 0.5541666666666666963, 0.5583333333333333481, 0.5625000000000000000, 0.5666666666666666519, 0.5708333333333333037, 0.5749999999999999556, 0.5791666666666667185, 0.5833333333333333703, 0.5875000000000000222, 0.5916666666666666741, 0.5958333333333333259, 0.5999999999999999778, 0.6041666666666666297, 0.6083333333333332815, 0.6125000000000000444, 0.6166666666666666963, 0.6208333333333333481, 0.6250000000000000000, 0.6291666666666666519, 0.6333333333333333037, 0.6374999999999999556, 0.6416666666666667185, 0.6458333333333333703, 0.6500000000000000222, 0.6541666666666666741, 0.6583333333333333259, 0.6624999999999999778, 0.6666666666666666297, 0.6708333333333332815, 0.6750000000000000444, 0.6791666666666666963, 0.6833333333333333481, 0.6875000000000000000, 0.6916666666666666519, 0.6958333333333333037, 0.6999999999999999556, 0.7041666666666667185, 0.7083333333333333703, 0.7125000000000000222, 0.7166666666666666741, 0.7208333333333333259, 0.7249999999999999778, 0.7291666666666666297, 0.7333333333333332815, 0.7375000000000000444, 0.7416666666666666963, 0.7458333333333333481, 0.7500000000000000000, 0.7541666666666666519, 0.7583333333333333037, 0.7624999999999999556, 0.7666666666666667185, 0.7708333333333333703, 0.7750000000000000222, 0.7791666666666666741, 0.7833333333333333259, 0.7874999999999999778, 0.7916666666666666297, 0.7958333333333332815, 0.8000000000000000444, 0.8041666666666666963, 0.8083333333333333481, 0.8125000000000000000, 0.8166666666666666519, 0.8208333333333333037, 0.8249999999999999556, 0.8291666666666667185, 0.8333333333333333703, 0.8375000000000000222, 0.8416666666666666741, 0.8458333333333333259, 0.8499999999999999778, 0.8541666666666666297, 0.8583333333333332815, 0.8625000000000000444, 0.8666666666666666963, 0.8708333333333333481, 0.8750000000000000000, 0.8791666666666666519, 0.8833333333333333037, 0.8874999999999999556, 0.8916666666666667185, 0.8958333333333333703, 0.9000000000000000222, 0.9041666666666666741, 0.9083333333333333259, 0.9124999999999999778, 0.9166666666666666297, 0.9208333333333332815, 0.9250000000000000444, 0.9291666666666666963, 0.9333333333333333481, 0.9375000000000000000, 0.9416666666666666519, 0.9458333333333333037, 0.9499999999999999556, 0.9541666666666667185, 0.9583333333333333703, 0.9625000000000000222, 0.9666666666666666741, 0.9708333333333333259, 0.9749999999999999778, 0.9791666666666666297, 0.9833333333333332815, 0.9875000000000000444, 0.9916666666666666963, 0.9958333333333333481, 1.000000000000000000 ),
 .UNSPECIFIED. ) 
 GEOMETRIC_REPRESENTATION_ITEM ( )  RATIONAL_B_SPLINE_SURFACE ( (
 ( 1.000000000000000000, 0.8660254037844387076, 1.000000000000000000, 0.8660254037844387076, 1.000000000000000000, 0.8660254037844387076, 1.000000000000000000, 0.8660254037844387076, 1.000000000000000000, 0.8660254037844387076, 1.000000000000000000, 0.8660254037844387076, 1.000000000000000000, 0.8660254037844387076, 1.000000000000000000, 0.8660254037844387076, 1.000000000000000000, 0.8660254037844387076, 1.000000000000000000, 0.8660254037844387076, 1.000000000000000000, 0.8660254037844387076, 1.000000000000000000, 0.8660254037844387076, 1.000000000000000000, 0.8660254037844387076, 1.000000000000000000, 0.8660254037844387076, 1.000000000000000000, 0.8660254037844387076, 1.000000000000000000, 0.8660254037844387076, 1.000000000000000000, 0.8660254037844387076, 1.000000000000000000, 0.8660254037844387076, 1.000000000000000000, 0.8660254037844387076, 1.000000000000000000, 0.8660254037844387076, 1.000000000000000000, 0.8660254037844387076, 1.000000000000000000, 0.8660254037844387076, 1.000000000000000000, 0.8660254037844387076, 1.000000000000000000, 0.8660254037844387076, 1.000000000000000000, 0.8660254037844387076, 1.000000000000000000, 0.8660254037844387076, 1.000000000000000000, 0.8660254037844387076, 1.000000000000000000, 0.8660254037844387076, 1.000000000000000000, 0.8660254037844387076, 1.000000000000000000, 0.8660254037844387076, 1.000000000000000000, 0.8660254037844387076, 1.000000000000000000, 0.8660254037844387076, 1.000000000000000000, 0.8660254037844387076, 1.000000000000000000, 0.8660254037844387076, 1.000000000000000000, 0.8660254037844387076, 1.000000000000000000, 0.8660254037844387076, 1.000000000000000000, 0.8660254037844387076, 1.000000000000000000, 0.8660254037844387076, 1.000000000000000000, 0.8660254037844387076, 1.000000000000000000, 0.8660254037844387076, 1.000000000000000000, 0.8660254037844387076, 1.000000000000000000, 0.8660254037844387076, 1.000000000000000000, 0.8660254037844387076, 1.000000000000000000, 0.8660254037844387076, 1.000000000000000000, 0.8660254037844387076, 1.000000000000000000, 0.8660254037844387076, 1.000000000000000000, 0.8660254037844387076, 1.000000000000000000, 0.8660254037844387076, 1.000000000000000000, 0.8660254037844387076, 1.000000000000000000, 0.8660254037844387076, 1.000000000000000000, 0.8660254037844387076, 1.000000000000000000, 0.8660254037844387076, 1.000000000000000000, 0.8660254037844387076, 1.000000000000000000, 0.8660254037844387076, 1.000000000000000000, 0.8660254037844387076, 1.000000000000000000, 0.8660254037844387076, 1.000000000000000000, 0.8660254037844387076, 1.000000000000000000, 0.8660254037844387076, 1.000000000000000000, 0.8660254037844387076, 1.000000000000000000, 0.8660254037844387076, 1.000000000000000000, 0.8660254037844387076, 1.000000000000000000, 0.8660254037844387076, 1.000000000000000000, 0.8660254037844387076, 1.000000000000000000, 0.8660254037844387076, 1.000000000000000000, 0.8660254037844387076, 1.000000000000000000, 0.8660254037844387076, 1.000000000000000000, 0.8660254037844387076, 1.000000000000000000, 0.8660254037844387076, 1.000000000000000000, 0.8660254037844387076, 1.000000000000000000, 0.8660254037844387076, 1.000000000000000000, 0.8660254037844387076, 1.000000000000000000, 0.8660254037844387076, 1.000000000000000000, 0.8660254037844387076, 1.000000000000000000, 0.8660254037844387076, 1.000000000000000000, 0.8660254037844387076, 1.000000000000000000, 0.8660254037844387076, 1.000000000000000000, 0.8660254037844387076, 1.000000000000000000, 0.8660254037844387076, 1.000000000000000000, 0.8660254037844387076, 1.000000000000000000, 0.8660254037844387076, 1.000000000000000000, 0.8660254037844387076, 1.000000000000000000, 0.8660254037844387076, 1.000000000000000000, 0.8660254037844387076, 1.000000000000000000, 0.8660254037844387076, 1.000000000000000000, 0.8660254037844387076, 1.000000000000000000, 0.8660254037844387076, 1.000000000000000000, 0.8660254037844387076, 1.000000000000000000, 0.8660254037844387076, 1.000000000000000000, 0.8660254037844387076, 1.000000000000000000, 0.8660254037844387076, 1.000000000000000000, 0.8660254037844387076, 1.000000000000000000, 0.8660254037844387076, 1.000000000000000000, 0.8660254037844387076, 1.000000000000000000, 0.8660254037844387076, 1.000000000000000000, 0.8660254037844387076, 1.000000000000000000, 0.8660254037844387076, 1.000000000000000000, 0.8660254037844387076, 1.000000000000000000, 0.8660254037844387076, 1.000000000000000000, 0.8660254037844387076, 1.000000000000000000, 0.8660254037844387076, 1.000000000000000000, 0.8660254037844387076, 1.000000000000000000, 0.8660254037844387076, 1.000000000000000000, 0.8660254037844387076, 1.000000000000000000, 0.8660254037844387076, 1.000000000000000000, 0.8660254037844387076, 1.000000000000000000, 0.8660254037844387076, 1.000000000000000000, 0.8660254037844387076, 1.000000000000000000, 0.8660254037844387076, 1.000000000000000000, 0.8660254037844387076, 1.000000000000000000, 0.8660254037844387076, 1.000000000000000000, 0.8660254037844387076, 1.000000000000000000, 0.8660254037844387076, 1.000000000000000000, 0.8660254037844387076, 1.000000000000000000, 0.8660254037844387076, 1.000000000000000000, 0.8660254037844387076, 1.000000000000000000, 0.8660254037844387076, 1.000000000000000000, 0.8660254037844387076, 1.000000000000000000, 0.8660254037844387076, 1.000000000000000000, 0.8660254037844387076, 1.000000000000000000, 0.8660254037844387076, 1.000000000000000000, 0.8660254037844387076, 1.000000000000000000, 0.8660254037844387076, 1.000000000000000000, 0.8660254037844387076, 1.000000000000000000, 0.8660254037844387076, 1.000000000000000000, 0.8660254037844387076, 1.000000000000000000, 0.8660254037844387076, 1.000000000000000000, 0.8660254037844387076, 1.000000000000000000, 0.8660254037844387076, 1.000000000000000000, 0.8660254037844387076, 1.000000000000000000, 0.8660254037844387076, 1.000000000000000000, 0.8660254037844387076, 1.000000000000000000, 0.8660254037844387076, 1.000000000000000000, 0.8660254037844387076, 1.000000000000000000, 0.8660254037844387076, 1.000000000000000000, 0.8660254037844387076, 1.000000000000000000, 0.8660254037844387076, 1.000000000000000000, 0.8660254037844387076, 1.000000000000000000, 0.8660254037844387076, 1.000000000000000000, 0.8660254037844387076, 1.000000000000000000, 0.8660254037844387076, 1.000000000000000000, 0.8660254037844387076, 1.000000000000000000, 0.8660254037844387076, 1.000000000000000000, 0.8660254037844387076, 1.000000000000000000, 0.8660254037844387076, 1.000000000000000000, 0.8660254037844387076, 1.000000000000000000, 0.8660254037844387076, 1.000000000000000000, 0.8660254037844387076, 1.000000000000000000, 0.8660254037844387076, 1.000000000000000000, 0.8660254037844387076, 1.000000000000000000, 0.8660254037844387076, 1.000000000000000000, 0.8660254037844387076, 1.000000000000000000, 0.8660254037844387076, 1.000000000000000000, 0.8660254037844387076, 1.000000000000000000, 0.8660254037844387076, 1.000000000000000000, 0.8660254037844387076, 1.000000000000000000, 0.8660254037844387076, 1.000000000000000000, 0.8660254037844387076, 1.000000000000000000, 0.8660254037844387076, 1.000000000000000000, 0.8660254037844387076, 1.000000000000000000, 0.8660254037844387076, 1.000000000000000000, 0.8660254037844387076, 1.000000000000000000, 0.8660254037844387076, 1.000000000000000000, 0.8660254037844387076, 1.000000000000000000, 0.8660254037844387076, 1.000000000000000000, 0.8660254037844387076, 1.000000000000000000, 0.8660254037844387076, 1.000000000000000000, 0.8660254037844387076, 1.000000000000000000, 0.8660254037844387076, 1.000000000000000000, 0.8660254037844387076, 1.000000000000000000, 0.8660254037844387076, 1.000000000000000000, 0.8660254037844387076, 1.000000000000000000, 0.8660254037844387076, 1.000000000000000000, 0.8660254037844387076, 1.000000000000000000, 0.8660254037844387076, 1.000000000000000000, 0.8660254037844387076, 1.000000000000000000, 0.8660254037844387076, 1.000000000000000000, 0.8660254037844387076, 1.000000000000000000, 0.8660254037844387076, 1.000000000000000000, 0.8660254037844387076, 1.000000000000000000, 0.8660254037844387076, 1.000000000000000000, 0.8660254037844387076, 1.000000000000000000, 0.8660254037844387076, 1.000000000000000000, 0.8660254037844387076, 1.000000000000000000, 0.8660254037844387076, 1.000000000000000000, 0.8660254037844387076, 1.000000000000000000, 0.8660254037844387076, 1.000000000000000000, 0.8660254037844387076, 1.000000000000000000, 0.8660254037844387076, 1.000000000000000000, 0.8660254037844387076, 1.000000000000000000, 0.8660254037844387076, 1.000000000000000000, 0.8660254037844387076, 1.000000000000000000, 0.8660254037844387076, 1.000000000000000000, 0.8660254037844387076, 1.000000000000000000, 0.8660254037844387076, 1.000000000000000000, 0.8660254037844387076, 1.000000000000000000, 0.8660254037844387076, 1.000000000000000000, 0.8660254037844387076, 1.000000000000000000, 0.8660254037844387076, 1.000000000000000000, 0.8660254037844387076, 1.000000000000000000, 0.8660254037844387076, 1.000000000000000000, 0.8660254037844387076, 1.000000000000000000, 0.8660254037844387076, 1.000000000000000000, 0.8660254037844387076, 1.000000000000000000, 0.8660254037844387076, 1.000000000000000000, 0.8660254037844387076, 1.000000000000000000, 0.8660254037844387076, 1.000000000000000000, 0.8660254037844387076, 1.000000000000000000, 0.8660254037844387076, 1.000000000000000000, 0.8660254037844387076, 1.000000000000000000, 0.8660254037844387076, 1.000000000000000000, 0.8660254037844387076, 1.000000000000000000, 0.8660254037844387076, 1.000000000000000000, 0.8660254037844387076, 1.000000000000000000, 0.8660254037844387076, 1.000000000000000000, 0.8660254037844387076, 1.000000000000000000, 0.8660254037844387076, 1.000000000000000000, 0.8660254037844387076, 1.000000000000000000, 0.8660254037844387076, 1.000000000000000000, 0.8660254037844387076, 1.000000000000000000, 0.8660254037844387076, 1.000000000000000000, 0.8660254037844387076, 1.000000000000000000, 0.8660254037844387076, 1.000000000000000000, 0.8660254037844387076, 1.000000000000000000, 0.8660254037844387076, 1.000000000000000000, 0.8660254037844387076, 1.000000000000000000, 0.8660254037844387076, 1.000000000000000000, 0.8660254037844387076, 1.000000000000000000, 0.8660254037844387076, 1.000000000000000000, 0.8660254037844387076, 1.000000000000000000, 0.8660254037844387076, 1.000000000000000000, 0.8660254037844387076, 1.000000000000000000, 0.8660254037844387076, 1.000000000000000000, 0.8660254037844387076, 1.000000000000000000, 0.8660254037844387076, 1.000000000000000000, 0.8660254037844387076, 1.000000000000000000, 0.8660254037844387076, 1.000000000000000000, 0.8660254037844387076, 1.000000000000000000, 0.8660254037844387076, 1.000000000000000000, 0.8660254037844387076, 1.000000000000000000, 0.8660254037844387076, 1.000000000000000000),
 ( 1.000000000000000000, 0.8660254037844387076, 1.000000000000000000, 0.8660254037844387076, 1.000000000000000000, 0.8660254037844387076, 1.000000000000000000, 0.8660254037844387076, 1.000000000000000000, 0.8660254037844387076, 1.000000000000000000, 0.8660254037844387076, 1.000000000000000000, 0.8660254037844387076, 1.000000000000000000, 0.8660254037844387076, 1.000000000000000000, 0.8660254037844387076, 1.000000000000000000, 0.8660254037844387076, 1.000000000000000000, 0.8660254037844387076, 1.000000000000000000, 0.8660254037844387076, 1.000000000000000000, 0.8660254037844387076, 1.000000000000000000, 0.8660254037844387076, 1.000000000000000000, 0.8660254037844387076, 1.000000000000000000, 0.8660254037844387076, 1.000000000000000000, 0.8660254037844387076, 1.000000000000000000, 0.8660254037844387076, 1.000000000000000000, 0.8660254037844387076, 1.000000000000000000, 0.8660254037844387076, 1.000000000000000000, 0.8660254037844387076, 1.000000000000000000, 0.8660254037844387076, 1.000000000000000000, 0.8660254037844387076, 1.000000000000000000, 0.8660254037844387076, 1.000000000000000000, 0.8660254037844387076, 1.000000000000000000, 0.8660254037844387076, 1.000000000000000000, 0.8660254037844387076, 1.000000000000000000, 0.8660254037844387076, 1.000000000000000000, 0.8660254037844387076, 1.000000000000000000, 0.8660254037844387076, 1.000000000000000000, 0.8660254037844387076, 1.000000000000000000, 0.8660254037844387076, 1.000000000000000000, 0.8660254037844387076, 1.000000000000000000, 0.8660254037844387076, 1.000000000000000000, 0.8660254037844387076, 1.000000000000000000, 0.8660254037844387076, 1.000000000000000000, 0.8660254037844387076, 1.000000000000000000, 0.8660254037844387076, 1.000000000000000000, 0.8660254037844387076, 1.000000000000000000, 0.8660254037844387076, 1.000000000000000000, 0.8660254037844387076, 1.000000000000000000, 0.8660254037844387076, 1.000000000000000000, 0.8660254037844387076, 1.000000000000000000, 0.8660254037844387076, 1.000000000000000000, 0.8660254037844387076, 1.000000000000000000, 0.8660254037844387076, 1.000000000000000000, 0.8660254037844387076, 1.000000000000000000, 0.8660254037844387076, 1.000000000000000000, 0.8660254037844387076, 1.000000000000000000, 0.8660254037844387076, 1.000000000000000000, 0.8660254037844387076, 1.000000000000000000, 0.8660254037844387076, 1.000000000000000000, 0.8660254037844387076, 1.000000000000000000, 0.8660254037844387076, 1.000000000000000000, 0.8660254037844387076, 1.000000000000000000, 0.8660254037844387076, 1.000000000000000000, 0.8660254037844387076, 1.000000000000000000, 0.8660254037844387076, 1.000000000000000000, 0.8660254037844387076, 1.000000000000000000, 0.8660254037844387076, 1.000000000000000000, 0.8660254037844387076, 1.000000000000000000, 0.8660254037844387076, 1.000000000000000000, 0.8660254037844387076, 1.000000000000000000, 0.8660254037844387076, 1.000000000000000000, 0.8660254037844387076, 1.000000000000000000, 0.8660254037844387076, 1.000000000000000000, 0.8660254037844387076, 1.000000000000000000, 0.8660254037844387076, 1.000000000000000000, 0.8660254037844387076, 1.000000000000000000, 0.8660254037844387076, 1.000000000000000000, 0.8660254037844387076, 1.000000000000000000, 0.8660254037844387076, 1.000000000000000000, 0.8660254037844387076, 1.000000000000000000, 0.8660254037844387076, 1.000000000000000000, 0.8660254037844387076, 1.000000000000000000, 0.8660254037844387076, 1.000000000000000000, 0.8660254037844387076, 1.000000000000000000, 0.8660254037844387076, 1.000000000000000000, 0.8660254037844387076, 1.000000000000000000, 0.8660254037844387076, 1.000000000000000000, 0.8660254037844387076, 1.000000000000000000, 0.8660254037844387076, 1.000000000000000000, 0.8660254037844387076, 1.000000000000000000, 0.8660254037844387076, 1.000000000000000000, 0.8660254037844387076, 1.000000000000000000, 0.8660254037844387076, 1.000000000000000000, 0.8660254037844387076, 1.000000000000000000, 0.8660254037844387076, 1.000000000000000000, 0.8660254037844387076, 1.000000000000000000, 0.8660254037844387076, 1.000000000000000000, 0.8660254037844387076, 1.000000000000000000, 0.8660254037844387076, 1.000000000000000000, 0.8660254037844387076, 1.000000000000000000, 0.8660254037844387076, 1.000000000000000000, 0.8660254037844387076, 1.000000000000000000, 0.8660254037844387076, 1.000000000000000000, 0.8660254037844387076, 1.000000000000000000, 0.8660254037844387076, 1.000000000000000000, 0.8660254037844387076, 1.000000000000000000, 0.8660254037844387076, 1.000000000000000000, 0.8660254037844387076, 1.000000000000000000, 0.8660254037844387076, 1.000000000000000000, 0.8660254037844387076, 1.000000000000000000, 0.8660254037844387076, 1.000000000000000000, 0.8660254037844387076, 1.000000000000000000, 0.8660254037844387076, 1.000000000000000000, 0.8660254037844387076, 1.000000000000000000, 0.8660254037844387076, 1.000000000000000000, 0.8660254037844387076, 1.000000000000000000, 0.8660254037844387076, 1.000000000000000000, 0.8660254037844387076, 1.000000000000000000, 0.8660254037844387076, 1.000000000000000000, 0.8660254037844387076, 1.000000000000000000, 0.8660254037844387076, 1.000000000000000000, 0.8660254037844387076, 1.000000000000000000, 0.8660254037844387076, 1.000000000000000000, 0.8660254037844387076, 1.000000000000000000, 0.8660254037844387076, 1.000000000000000000, 0.8660254037844387076, 1.000000000000000000, 0.8660254037844387076, 1.000000000000000000, 0.8660254037844387076, 1.000000000000000000, 0.8660254037844387076, 1.000000000000000000, 0.8660254037844387076, 1.000000000000000000, 0.8660254037844387076, 1.000000000000000000, 0.8660254037844387076, 1.000000000000000000, 0.8660254037844387076, 1.000000000000000000, 0.8660254037844387076, 1.000000000000000000, 0.8660254037844387076, 1.000000000000000000, 0.8660254037844387076, 1.000000000000000000, 0.8660254037844387076, 1.000000000000000000, 0.8660254037844387076, 1.000000000000000000, 0.8660254037844387076, 1.000000000000000000, 0.8660254037844387076, 1.000000000000000000, 0.8660254037844387076, 1.000000000000000000, 0.8660254037844387076, 1.000000000000000000, 0.8660254037844387076, 1.000000000000000000, 0.8660254037844387076, 1.000000000000000000, 0.8660254037844387076, 1.000000000000000000, 0.8660254037844387076, 1.000000000000000000, 0.8660254037844387076, 1.000000000000000000, 0.8660254037844387076, 1.000000000000000000, 0.8660254037844387076, 1.000000000000000000, 0.8660254037844387076, 1.000000000000000000, 0.8660254037844387076, 1.000000000000000000, 0.8660254037844387076, 1.000000000000000000, 0.8660254037844387076, 1.000000000000000000, 0.8660254037844387076, 1.000000000000000000, 0.8660254037844387076, 1.000000000000000000, 0.8660254037844387076, 1.000000000000000000, 0.8660254037844387076, 1.000000000000000000, 0.8660254037844387076, 1.000000000000000000, 0.8660254037844387076, 1.000000000000000000, 0.8660254037844387076, 1.000000000000000000, 0.8660254037844387076, 1.000000000000000000, 0.8660254037844387076, 1.000000000000000000, 0.8660254037844387076, 1.000000000000000000, 0.8660254037844387076, 1.000000000000000000, 0.8660254037844387076, 1.000000000000000000, 0.8660254037844387076, 1.000000000000000000, 0.8660254037844387076, 1.000000000000000000, 0.8660254037844387076, 1.000000000000000000, 0.8660254037844387076, 1.000000000000000000, 0.8660254037844387076, 1.000000000000000000, 0.8660254037844387076, 1.000000000000000000, 0.8660254037844387076, 1.000000000000000000, 0.8660254037844387076, 1.000000000000000000, 0.8660254037844387076, 1.000000000000000000, 0.8660254037844387076, 1.000000000000000000, 0.8660254037844387076, 1.000000000000000000, 0.8660254037844387076, 1.000000000000000000, 0.8660254037844387076, 1.000000000000000000, 0.8660254037844387076, 1.000000000000000000, 0.8660254037844387076, 1.000000000000000000, 0.8660254037844387076, 1.000000000000000000, 0.8660254037844387076, 1.000000000000000000, 0.8660254037844387076, 1.000000000000000000, 0.8660254037844387076, 1.000000000000000000, 0.8660254037844387076, 1.000000000000000000, 0.8660254037844387076, 1.000000000000000000, 0.8660254037844387076, 1.000000000000000000, 0.8660254037844387076, 1.000000000000000000, 0.8660254037844387076, 1.000000000000000000, 0.8660254037844387076, 1.000000000000000000, 0.8660254037844387076, 1.000000000000000000, 0.8660254037844387076, 1.000000000000000000, 0.8660254037844387076, 1.000000000000000000, 0.8660254037844387076, 1.000000000000000000, 0.8660254037844387076, 1.000000000000000000, 0.8660254037844387076, 1.000000000000000000, 0.8660254037844387076, 1.000000000000000000, 0.8660254037844387076, 1.000000000000000000, 0.8660254037844387076, 1.000000000000000000, 0.8660254037844387076, 1.000000000000000000, 0.8660254037844387076, 1.000000000000000000, 0.8660254037844387076, 1.000000000000000000, 0.8660254037844387076, 1.000000000000000000, 0.8660254037844387076, 1.000000000000000000, 0.8660254037844387076, 1.000000000000000000, 0.8660254037844387076, 1.000000000000000000, 0.8660254037844387076, 1.000000000000000000, 0.8660254037844387076, 1.000000000000000000, 0.8660254037844387076, 1.000000000000000000, 0.8660254037844387076, 1.000000000000000000, 0.8660254037844387076, 1.000000000000000000, 0.8660254037844387076, 1.000000000000000000, 0.8660254037844387076, 1.000000000000000000, 0.8660254037844387076, 1.000000000000000000, 0.8660254037844387076, 1.000000000000000000, 0.8660254037844387076, 1.000000000000000000, 0.8660254037844387076, 1.000000000000000000, 0.8660254037844387076, 1.000000000000000000, 0.8660254037844387076, 1.000000000000000000, 0.8660254037844387076, 1.000000000000000000, 0.8660254037844387076, 1.000000000000000000, 0.8660254037844387076, 1.000000000000000000, 0.8660254037844387076, 1.000000000000000000, 0.8660254037844387076, 1.000000000000000000, 0.8660254037844387076, 1.000000000000000000, 0.8660254037844387076, 1.000000000000000000, 0.8660254037844387076, 1.000000000000000000, 0.8660254037844387076, 1.000000000000000000, 0.8660254037844387076, 1.000000000000000000, 0.8660254037844387076, 1.000000000000000000, 0.8660254037844387076, 1.000000000000000000, 0.8660254037844387076, 1.000000000000000000, 0.8660254037844387076, 1.000000000000000000, 0.8660254037844387076, 1.000000000000000000, 0.8660254037844387076, 1.000000000000000000, 0.8660254037844387076, 1.000000000000000000, 0.8660254037844387076, 1.000000000000000000, 0.8660254037844387076, 1.000000000000000000, 0.8660254037844387076, 1.000000000000000000, 0.8660254037844387076, 1.000000000000000000, 0.8660254037844387076, 1.000000000000000000, 0.8660254037844387076, 1.000000000000000000, 0.8660254037844387076, 1.000000000000000000, 0.8660254037844387076, 1.000000000000000000, 0.8660254037844387076, 1.000000000000000000, 0.8660254037844387076, 1.000000000000000000, 0.8660254037844387076, 1.000000000000000000) ) ) 
 REPRESENTATION_ITEM ( '' )  SURFACE ( )  );
#58893 = CARTESIAN_POINT ( 'NONE',  ( 1.317580156568556538, -1.924246910545416522, 0.4277698889081028577 ) ) ;
#58894 = CARTESIAN_POINT ( 'NONE',  ( 3.761887187967042134, 0.6396200178584460216, -1.802413552503052463 ) ) ;
#58895 = ORIENTED_EDGE ( 'NONE', *, *, #171975, .F. ) ;
#58896 = APPLICATION_CONTEXT ( 'automotive_design' ) ;
#58897 = CARTESIAN_POINT ( 'NONE',  ( 0.4123176713737538024, 4.000000000000008882, 0.8977835139437831957 ) ) ;
#58898 = CARTESIAN_POINT ( 'NONE',  ( 4.738697576358215535, -1.909850223682897807, -0.4806687167441258679 ) ) ;
#58899 = ORIENTED_EDGE ( 'NONE', *, *, #134279, .F. ) ;
#58900 = CARTESIAN_POINT ( 'NONE',  ( 6.075724011240296818, -1.035248994944122369, 1.642949693582099302 ) ) ;
#58901 = ORIENTED_EDGE ( 'NONE', *, *, #22449, .T. ) ;
#58902 = CARTESIAN_POINT ( 'NONE',  ( -6.771371375382467583, 6.864631124226471037, -0.7998128361456362523 ) ) ;
#58904 = CARTESIAN_POINT ( 'NONE',  ( 6.187751663909415001, 2.028806014889028120, -0.6170373231123224000 ) ) ;
#58903 = CARTESIAN_POINT ( 'NONE',  ( -5.309953438407606363, 6.223975762010839574, 1.199719254218452935 ) ) ;
#58905 = CARTESIAN_POINT ( 'NONE',  ( 7.200788982189461507, 8.533913579710086239, -1.082531754730548412 ) ) ;
#58907 = VERTEX_POINT ( 'NONE', #122392 ) ;
#58906 = CARTESIAN_POINT ( 'NONE',  ( 4.336511155197938727, 1.173803677898217712, -1.509565991254034678 ) ) ;
#58908 = CARTESIAN_POINT ( 'NONE',  ( 9.476364159883861049, 3.602179703620751905, -7.289721612074726131 ) ) ;
#58909 = CARTESIAN_POINT ( 'NONE',  ( 4.969394074578011633, -1.701821450762316612, -1.075051190359946895 ) ) ;
#58910 = DIRECTION ( 'NONE',  ( -0.3281536732072464768, -0.000000000000000000, 0.9446243521954066358 ) ) ;
#58911 = CARTESIAN_POINT ( 'NONE',  ( 5.900976575431972293, 1.489821718068456979, -1.054992404821846863 ) ) ;
#58912 = CARTESIAN_POINT ( 'NONE',  ( 1.539598694730393680, 1.913698299121506352, -0.7905179490511196061 ) ) ;
#58913 = CARTESIAN_POINT ( 'NONE',  ( -7.074657228232555717, 7.148188275893099686, 1.040834085586084257E-14 ) ) ;
#58914 = CARTESIAN_POINT ( 'NONE',  ( -5.386282318077409315, 7.574627448853999745, -1.244059264865501557 ) ) ;
#58915 = CARTESIAN_POINT ( 'NONE',  ( 6.455916552660014851, 1.865467424361374249, -0.1398750677365916961 ) ) ;
#58916 = CARTESIAN_POINT ( 'NONE',  ( 6.972971076130050072, 7.029554431773520129, 1.040834085586084257E-14 ) ) ;
#58917 = CARTESIAN_POINT ( 'NONE',  ( 5.451787166470912993, 6.493411461371761284, -1.082531754730548412 ) ) ;
#58918 = LINE ( 'NONE', #92520, #113492 ) ;
#58919 = CARTESIAN_POINT ( 'NONE',  ( -8.012344526598182026E-15, 11.85937500034140157, -1.575800808251669460 ) ) ;
#58921 = CARTESIAN_POINT ( 'NONE',  ( -7.293360289508603600, 7.473618190706972086, 0.000000000000000000 ) ) ;
#58920 = CARTESIAN_POINT ( 'NONE',  ( 6.825078400183548055, 2.461594334264828987, 2.239602747093616841 ) ) ;
#58922 = CARTESIAN_POINT ( 'NONE',  ( 4.852092609920839905, 0.1625460678297725725, -1.726498261149024271 ) ) ;
#58923 = CARTESIAN_POINT ( 'NONE',  ( -5.251085567194491155, 5.020688004682002159, -0.7998128361456221525 ) ) ;
#58924 = CARTESIAN_POINT ( 'NONE',  ( 2.588806720547200513, 2.007000696110202043, 0.5072723548179418618 ) ) ;
#58925 = CARTESIAN_POINT ( 'NONE',  ( 3.480171074976373013, -2.114893226951024108, -0.1016293738061168905 ) ) ;
#58926 = CARTESIAN_POINT ( 'NONE',  ( 8.263858322729371153, 9.599921783727809910, -1.199719254218446718 ) ) ;
#58928 = EDGE_CURVE ( 'NONE', #178928, #48080, #36260, .T. ) ;
#58927 = CARTESIAN_POINT ( 'NONE',  ( 0.08097581798159399213, -9.904508987438854106, 10.99970197202149969 ) ) ;
#58929 = CARTESIAN_POINT ( 'NONE',  ( 1.199983893365302201, 0.8030756602186311932, -1.798478550607261583 ) ) ;
#58930 = CARTESIAN_POINT ( 'NONE',  ( 6.095406204355903412, 6.027892130464396203, -0.2603320317973931153 ) ) ;
#58932 = CARTESIAN_POINT ( 'NONE',  ( 0.2461629937395051204, 0.9812432698282257393, -1.641294572782559413 ) ) ;
#58931 = CARTESIAN_POINT ( 'NONE',  ( -1.737500000000000266, -1.808333333333332016, -3.009438278150923907 ) ) ;
#58933 = CARTESIAN_POINT ( 'NONE',  ( 3.679849949768813744, -1.130634651955428671, 1.993948080406320766 ) ) ;
#58934 = CARTESIAN_POINT ( 'NONE',  ( 1.488595654847741923, -0.2661386877833260556, -1.806066791206423217 ) ) ;
#58935 = EDGE_CURVE ( 'NONE', #136464, #59550, #7448, .T. ) ;
#58936 = CARTESIAN_POINT ( 'NONE',  ( 6.367489420273535039, 7.457767740854454708, -1.199719254218452047 ) ) ;
#58937 = CARTESIAN_POINT ( 'NONE',  ( 6.819388077549422889, 8.018669514304889390, -1.082531754730543971 ) ) ;
#58938 = CARTESIAN_POINT ( 'NONE',  ( -7.049349804101573191, 10.31165964050546258, -1.199719254218440723 ) ) ;
#58939 = CARTESIAN_POINT ( 'NONE',  ( 3.217044422572811424, 1.584514289383936347, -1.241758421991135064 ) ) ;
#58940 = CARTESIAN_POINT ( 'NONE',  ( 2.166782468979636000, 1.457124453068344039, -1.313723524322525815 ) ) ;
#58941 = CARTESIAN_POINT ( 'NONE',  ( -7.472515219426274946, 11.86968485597268064, 0.000000000000000000 ) ) ;
#58942 = CARTESIAN_POINT ( 'NONE',  ( -5.982172092127739482, 8.002286745614243912, -1.599625672291263179 ) ) ;
#58943 = CARTESIAN_POINT ( 'NONE',  ( 0.07516593201273635838, 6.947014887512039216, -2.639261810199782232 ) ) ;
#58945 = CARTESIAN_POINT ( 'NONE',  ( 3.484973364136711549, 1.600408865665205571, -0.7559459569618111052 ) ) ;
#58944 = CARTESIAN_POINT ( 'NONE',  ( 4.523432754507224374, -1.286067535266706807, -1.648171318802932106 ) ) ;
#58946 = CARTESIAN_POINT ( 'NONE',  ( 0.3263184169964571946, 14.00000000000058265, 11.67999999558625213 ) ) ;
#58947 = CARTESIAN_POINT ( 'NONE',  ( 6.140627040082555332, -1.939752761746313059, 1.221158637518650503 ) ) ;
#58948 = CARTESIAN_POINT ( 'NONE',  ( 5.384588317801639157, 1.532214865288351158, -0.8252546180599307224 ) ) ;
#58949 = CARTESIAN_POINT ( 'NONE',  ( 7.239163954692881653, 10.53310948286200599, -1.199719254218441611 ) ) ;
#58950 = CARTESIAN_POINT ( 'NONE',  ( 5.906922434318937931, -1.273882657197453305, -1.913274281643152941 ) ) ;
#58951 = CARTESIAN_POINT ( 'NONE',  ( 0.1333692844072559280, 6.947498546895843674, -2.648624074793118233 ) ) ;
#58952 = CARTESIAN_POINT ( 'NONE',  ( 5.905553417332951582, 0.3413034225961882884, 1.699694455674398919 ) ) ;
#58953 = CARTESIAN_POINT ( 'NONE',  ( 6.438686429976131720, -1.555646628146038157, 1.282773817382940384 ) ) ;
#58954 = B_SPLINE_CURVE_WITH_KNOTS ( 'NONE', 3,
 ( #161999, #94871, #29861, #114370, #112238, #28788, #146827 ),
 .UNSPECIFIED., .F., .F.,
 ( 4, 3, 4 ),
 ( 0.000000000000000000, 0.0008000000000005096134, 0.002977368225425562967 ),
 .UNSPECIFIED. ) ;
#58955 =( GEOMETRIC_REPRESENTATION_CONTEXT ( 3 ) GLOBAL_UNCERTAINTY_ASSIGNED_CONTEXT ( ( #98100 ) ) GLOBAL_UNIT_ASSIGNED_CONTEXT ( ( #26746, #105919, #73355 ) ) REPRESENTATION_CONTEXT ( 'NONE', 'WORKASPACE' ) );
#58956 = CARTESIAN_POINT ( 'NONE',  ( 5.969212972359552616, 1.911920703953375655, 1.028910892658722265 ) ) ;
#58957 = DIRECTION ( 'NONE',  ( 0.000000000000000000, 0.000000000000000000, -1.000000000000000000 ) ) ;
#58958 = CARTESIAN_POINT ( 'NONE',  ( 0.1810649180928698143, 1.756560269771380911, -1.181951075121101979 ) ) ;
#58959 = CARTESIAN_POINT ( 'NONE',  ( 4.875000000000002665, 2.052068128417942727, -2.776269294175867294E-13 ) ) ;
#58960 = CARTESIAN_POINT ( 'NONE',  ( -0.1505076982584017398, 7.030243935902841912, -1.995512553310450521 ) ) ;
#58961 = CARTESIAN_POINT ( 'NONE',  ( 4.225552302291880835, -1.843726210754624173, 0.5582998813679838079 ) ) ;
#58962 = CARTESIAN_POINT ( 'NONE',  ( -0.7500000000000179856, 10.57291666734946212, 1.299038105676658228 ) ) ;
#58963 = CARTESIAN_POINT ( 'NONE',  ( 0.2764465059262249391, 2.196205179236205396, -0.3323138113263158222 ) ) ;
#58964 = ORIENTED_EDGE ( 'NONE', *, *, #200653, .F. ) ;
#58965 = CARTESIAN_POINT ( 'NONE',  ( -0.7499999999999972244, 4.858333333333353821, -1.299038105676652011 ) ) ;
#58966 = CARTESIAN_POINT ( 'NONE',  ( 5.172599298813543633, 5.993452922492633839, -1.199719254218452047 ) ) ;
#58967 = CARTESIAN_POINT ( 'NONE',  ( 6.714312387265682247, 8.856450423275211037, 1.599625672291281386 ) ) ;
#58968 = CARTESIAN_POINT ( 'NONE',  ( 2.403257875557132994, -0.3827610287685556112, -2.187935401104672994 ) ) ;
#58969 = CARTESIAN_POINT ( 'NONE',  ( -0.02900071798685524560, 2.860900941590225344, -2.661937258840251008 ) ) ;
#58970 = CARTESIAN_POINT ( 'NONE',  ( 7.646435448427411963, 8.023188899361205273, -0.7216878364870257245 ) ) ;
#58971 = CARTESIAN_POINT ( 'NONE',  ( -10.12757755928392456, 10.91785469536048758, 0.7216878364870438212 ) ) ;
#58972 = CARTESIAN_POINT ( 'NONE',  ( 7.688882512725796481, 8.142986817701137525, 0.000000000000000000 ) ) ;
#58973 = CARTESIAN_POINT ( 'NONE',  ( 1.125625214514534900, 0.3961039030971893471, 1.976955501819408711 ) ) ;
#58975 = CARTESIAN_POINT ( 'NONE',  ( 6.566849514013569866, 1.531126396248701171, -1.382332999690039754 ) ) ;
#58974 = CARTESIAN_POINT ( 'NONE',  ( 7.781490099239519509, 11.16582331816642260, 1.199719254218460707 ) ) ;
#58976 = CARTESIAN_POINT ( 'NONE',  ( 6.966220764712121927, 6.002124920821316323, 2.420000000000000373 ) ) ;
#58977 = CARTESIAN_POINT ( 'NONE',  ( 5.817857313595521163, 9.801600942587855414, -0.7216878364870458196 ) ) ;
#58978 = CARTESIAN_POINT ( 'NONE',  ( -2.044581833100346469, 2.972657967446783456, 11.47952151275213240 ) ) ;
#58979 = CARTESIAN_POINT ( 'NONE',  ( -0.6823417656250246877, 0.5510416670080897639, 1.181850606188755259 ) ) ;
#58980 = CARTESIAN_POINT ( 'NONE',  ( 1.457869587114325460, 0.7109265171535653627, 1.620852848218183873 ) ) ;
#58981 = CARTESIAN_POINT ( 'NONE',  ( 0.07093568767341934533, -0.9480374005119349690, 1.779628194860154222 ) ) ;
#58982 = CARTESIAN_POINT ( 'NONE',  ( 6.146048976554097543, 0.5551056870855082259, 1.649627438850902017 ) ) ;
#58983 = CARTESIAN_POINT ( 'NONE',  ( 4.616876278103482001, -0.1136277499396514262, 2.289655339347085317 ) ) ;
#58984 = CARTESIAN_POINT ( 'NONE',  ( -1.402160292154681736E-14, -0.05312499965857903073, -1.575800808251665908 ) ) ;
#58985 = CARTESIAN_POINT ( 'NONE',  ( 2.343484645521694887, 1.840739972059933560, 0.04548452486473342216 ) ) ;
#58986 = CARTESIAN_POINT ( 'NONE',  ( 8.550388431712704573, 13.12720360364021133, 0.000000000000000000 ) ) ;
#58987 = CARTESIAN_POINT ( 'NONE',  ( 9.086253353280454803, 13.39999999999999680, -7.838367176906162470 ) ) ;
#58988 = CARTESIAN_POINT ( 'NONE',  ( 2.713660727937649231, -1.805999004224107418, 0.2657717501357085843 ) ) ;
#58989 = CARTESIAN_POINT ( 'NONE',  ( 3.955704058034177351, -1.882473782773282700, -0.7231407674024927790 ) ) ;
#58990 = CARTESIAN_POINT ( 'NONE',  ( -9.130526383799315582, 12.73969898348616070, 1.199719254218462483 ) ) ;
#58992 = DIRECTION ( 'NONE',  ( 0.000000000000000000, 0.000000000000000000, 1.000000000000000000 ) ) ;
#58991 = CARTESIAN_POINT ( 'NONE',  ( 1.938691616020698172, 2.238021082172815479, 0.3313278802117639033 ) ) ;
#58993 = CARTESIAN_POINT ( 'NONE',  ( 5.860410395878546730, 0.8502751990519905601, 1.926866089339970056 ) ) ;
#58994 = CARTESIAN_POINT ( 'NONE',  ( 8.518320732998095224, 14.76619040281040718, 9.398253358897362020 ) ) ;
#58995 = CARTESIAN_POINT ( 'NONE',  ( 2.875506610227479332, -0.2054619808779626633, 2.060159609288146232 ) ) ;
#58996 = CARTESIAN_POINT ( 'NONE',  ( 3.493197133815315603, 7.227147089426516402, -0.7998128361456291469 ) ) ;
#58997 = CARTESIAN_POINT ( 'NONE',  ( -0.6801582343750022241, 1.130208333674734167, -1.178068619123841643 ) ) ;
#58998 = CARTESIAN_POINT ( 'NONE',  ( 4.213620120093874988, 1.703795446819071691, 1.262174061880352305 ) ) ;
#58999 = CONTEXT_DEPENDENT_SHAPE_REPRESENTATION ( #143385, #111211 ) ;
#59000 = CARTESIAN_POINT ( 'NONE',  ( 0.5746741651161955122, -1.813631458699631160, -0.6500969746191431753 ) ) ;
#59001 = CARTESIAN_POINT ( 'NONE',  ( -3.481411583659053566, 7.283673624236017830, 0.000000000000000000 ) ) ;
#59002 = CARTESIAN_POINT ( 'NONE',  ( 9.043452155515161905, 10.50944792197790889, 1.199719254218453823 ) ) ;
#59003 = CARTESIAN_POINT ( 'NONE',  ( 4.706088717274896638, 7.544168365912456764, 1.082531754730548412 ) ) ;
#59004 = CARTESIAN_POINT ( 'NONE',  ( 3.475000000000000533, -0.4520833323774166024, -2.006292185433951047 ) ) ;
#59005 = CARTESIAN_POINT ( 'NONE',  ( -5.088387723830502196, 4.830873854090670605, -0.7998128361456221525 ) ) ;
#59006 = CARTESIAN_POINT ( 'NONE',  ( 5.853796514643677007, -1.537196951383312804, -1.461068456062891041 ) ) ;
#59007 = CARTESIAN_POINT ( 'NONE',  ( 2.362460971492767570, 0.8994288142968703825, 1.904360703123770149 ) ) ;
#59008 = CARTESIAN_POINT ( 'NONE',  ( -5.010620288702242853, 8.003418215864698482, -1.199719254218453823 ) ) ;
#59009 = CARTESIAN_POINT ( 'NONE',  ( 8.911787042884274257, 9.291506392986812912, 0.7998128361456462443 ) ) ;
#59010 = CARTESIAN_POINT ( 'NONE',  ( 6.385601346537729484, -1.752585461374029929, 0.6262014864842447848 ) ) ;
#59011 = CARTESIAN_POINT ( 'NONE',  ( 6.938021921891177612, 9.117444880338284818, -1.599625672291262513 ) ) ;
#59012 = CARTESIAN_POINT ( 'NONE',  ( -6.116136693540540570, 10.14959355252370266, 0.000000000000000000 ) ) ;
#59013 = CARTESIAN_POINT ( 'NONE',  ( -9.490344339885981029, 10.17441593939621924, -0.7216878364870267237 ) ) ;
#59014 = CARTESIAN_POINT ( 'NONE',  ( 0.5102161431939798986, -0.7575819503438313562, 1.980855387931411915 ) ) ;
#59015 = CYLINDRICAL_SURFACE ( 'NONE', #116184, 2.500000000000000888 ) ;
#59017 = CARTESIAN_POINT ( 'NONE',  ( 3.859774877264535053, -0.5717695562157121270, 1.876676618968641019 ) ) ;
#59016 = CARTESIAN_POINT ( 'NONE',  ( -1.360316468750038643, 2.901041667008071645, -0.7853790794159161148 ) ) ;
#59018 = CARTESIAN_POINT ( 'NONE',  ( 0.9894095316701527754, 1.906041449620498929, -1.019753361306941386 ) ) ;
#59020 = CARTESIAN_POINT ( 'NONE',  ( -5.732528328060045197, 6.256990841418501148, 1.080875701640615638 ) ) ;
#59019 = CARTESIAN_POINT ( 'NONE',  ( -4.960304097753355457, 6.880383762169266504, 1.599625672291263179 ) ) ;
#59021 = CARTESIAN_POINT ( 'NONE',  ( -1.364683531250014514, 1.988541667008086655, -0.7879004041258289570 ) ) ;
#59022 = CARTESIAN_POINT ( 'NONE',  ( 2.360927591450364904, 1.706848764895356085, -0.3387292939842252437 ) ) ;
#59023 = CARTESIAN_POINT ( 'NONE',  ( 5.165293337126522388, 8.969999960048859577, 1.040834085586084257E-14 ) ) ;
#59024 = CARTESIAN_POINT ( 'NONE',  ( -11.31901822352654641, 5.215070234333009758, -5.710337001866061968 ) ) ;
#59025 = CARTESIAN_POINT ( 'NONE',  ( 2.618517346670693247, 0.5404096030681636575, -1.942243668081746311 ) ) ;
#59026 = CARTESIAN_POINT ( 'NONE',  ( -0.08246874231332826377, -9.908734156519553693, -10.99969088041219401 ) ) ;
#59027 = CARTESIAN_POINT ( 'NONE',  ( -4.930325137224961907, 5.781076077297750970, -1.199719254218453823 ) ) ;
#59028 = CARTESIAN_POINT ( 'NONE',  ( 2.834795904189919558, 0.2398841137210059038, 1.956746676604983248 ) ) ;
#59030 = CARTESIAN_POINT ( 'NONE',  ( -4.326460416536637155, 8.061637896019123062, 0.000000000000000000 ) ) ;
#59029 = CARTESIAN_POINT ( 'NONE',  ( 6.240485052285455581, 1.095381943021833449, -1.567431287326017664 ) ) ;
#59031 = CARTESIAN_POINT ( 'NONE',  ( -4.624739795592931912, 8.409630504918133909, -0.7216878364870338292 ) ) ;
#59032 = CARTESIAN_POINT ( 'NONE',  ( 6.713222337422018349, 7.861122810861019161, -1.199719254218452047 ) ) ;
#59033 = CARTESIAN_POINT ( 'NONE',  ( -6.631873415740034083, 7.766215735565355160, 1.199719254218452047 ) ) ;
#59034 = CARTESIAN_POINT ( 'NONE',  ( 2.508468462390922138, -2.014426205243079693, -0.1462163075645859234 ) ) ;
#59035 = DIRECTION ( 'NONE',  ( 0.000000000000000000, 1.000000000000000000, 0.000000000000000000 ) ) ;
#59036 = CARTESIAN_POINT ( 'NONE',  ( 5.175001447075725736, -2.170742607874641461, -0.7831926130325519431 ) ) ;
#59037 = CARTESIAN_POINT ( 'NONE',  ( 6.549272904993657995, 1.707534169505098953, -0.9658701945045378157 ) ) ;
#59038 = CARTESIAN_POINT ( 'NONE',  ( 3.256644689873238629, -0.5649923015349536115, -1.878667693404307171 ) ) ;
#59039 = CARTESIAN_POINT ( 'NONE',  ( 9.772729797352075920, 10.29593960653257234, -0.7998128361456281477 ) ) ;
#59040 = CARTESIAN_POINT ( 'NONE',  ( 0.9322677863709986079, -1.591319861332978425, -1.238319039483272599 ) ) ;
#59041 = ORIENTED_EDGE ( 'NONE', *, *, #95883, .T. ) ;
#59042 = CARTESIAN_POINT ( 'NONE',  ( 0.8489989883206483512, -1.916807839401615476, -0.8996751459469201073 ) ) ;
#59044 = CARTESIAN_POINT ( 'NONE',  ( -6.989391883044787868, 8.113044270762433285, -1.199719254218446718 ) ) ;
#59043 = CARTESIAN_POINT ( 'NONE',  ( -2.625475302540713152, 6.214804952939456228, -0.7998128361456281477 ) ) ;
#59045 = CARTESIAN_POINT ( 'NONE',  ( 1.851249556194194179, 1.836288347861175785, -0.1344999175661651392 ) ) ;
#59046 = VERTEX_POINT ( 'NONE', #90882 ) ;
#59047 = CARTESIAN_POINT ( 'NONE',  ( 3.081267818761534549, 1.592661989535900657, 1.236799713577160231 ) ) ;
#59048 = CARTESIAN_POINT ( 'NONE',  ( 10.80502615499130314, 9.582201645171684490, 5.117034356647724991 ) ) ;
#59049 = CARTESIAN_POINT ( 'NONE',  ( 2.549219474610735947, 0.2639673528169217964, 2.104066465523121376 ) ) ;
#59050 = CARTESIAN_POINT ( 'NONE',  ( -0.7500000000000215383, 4.972916667349482012, 1.299038105676671107 ) ) ;
#59051 = CARTESIAN_POINT ( 'NONE',  ( 7.344766530301147789, 9.591980256816594164, 1.599625672291281386 ) ) ;
#59052 = CARTESIAN_POINT ( 'NONE',  ( 7.849244587668864348, 8.122149871893999062, 0.7998128361456291469 ) ) ;
#59053 = CARTESIAN_POINT ( 'NONE',  ( 4.552062217129227761, 2.060418430787996691, -0.04653940209857834048 ) ) ;
#59054 = AXIS2_PLACEMENT_3D ( 'NONE', #13612, #48281, #98096 ) ;
#59056 = CARTESIAN_POINT ( 'NONE',  ( 1.751249726499287673, 1.836263021919124050, -0.1365115386888632321 ) ) ;
#59055 = CARTESIAN_POINT ( 'NONE',  ( -8.376239975144482486, 8.666701480623698828, 1.040834085586084257E-14 ) ) ;
#59057 = CARTESIAN_POINT ( 'NONE',  ( -1.001543065824772872E-14, 5.071875000341421469, 1.575800808251672791 ) ) ;
#59058 = CARTESIAN_POINT ( 'NONE',  ( -0.02244404828160087226, 1.995160441984781041, -2.602654351998904492 ) ) ;
#59059 = CARTESIAN_POINT ( 'NONE',  ( -9.499606442108964544, -9.900000000000005684, 0.08647222121513538362 ) ) ;
#59060 = CARTESIAN_POINT ( 'NONE',  ( 0.000000000000000000, 0.000000000000000000, 0.000000000000000000 ) ) ;
#59061 = CARTESIAN_POINT ( 'NONE',  ( 1.612255294781844706, -2.189918024983358080, 0.2725913246661854084 ) ) ;
#59062 = CARTESIAN_POINT ( 'NONE',  ( 2.671453201960610091, 0.1136055399131811194, -2.259690131287622084 ) ) ;
#59063 = CARTESIAN_POINT ( 'NONE',  ( -8.853111120043687166, 9.430977182913531820, 1.040834085586084257E-14 ) ) ;
#59064 = CARTESIAN_POINT ( 'NONE',  ( 3.216879062660949362, 1.425012358211204422, -1.118398921490076026 ) ) ;
#59065 = CARTESIAN_POINT ( 'NONE',  ( 2.975699994382564828, -0.7717752754876210375, 1.753554302899827277 ) ) ;
#59066 = CARTESIAN_POINT ( 'NONE',  ( 3.965334771736851671, 1.774175476309115984, 1.066894043611272824 ) ) ;
#59067 = CARTESIAN_POINT ( 'NONE',  ( -1.364683531249997417, 2.571875000341422357, 1.214306433183764966E-14 ) ) ;
#59068 = CARTESIAN_POINT ( 'NONE',  ( 2.535955197907293179, 0.9309914139831111379, -1.737806310995954728 ) ) ;
#59069 = CARTESIAN_POINT ( 'NONE',  ( 6.445928676245076261, 0.7346846062235148356, -1.781103304711729729 ) ) ;
#59070 = CARTESIAN_POINT ( 'NONE',  ( 3.766346201128992988, -1.256895078192099335, 1.385637336983977397 ) ) ;
#59071 = EDGE_CURVE ( 'NONE', #14623, #50335, #48924, .T. ) ;
#59073 = CARTESIAN_POINT ( 'NONE',  ( 4.730098472736550264, 8.327237590489470875, -0.7222317683119976461 ) ) ;
#59072 = CARTESIAN_POINT ( 'NONE',  ( 2.016686958704193344, -1.090287029490369930, -2.033897785187769536 ) ) ;
#59074 = CARTESIAN_POINT ( 'NONE',  ( 3.806960202730264253, -1.522499362102507359, 1.069998817686746984 ) ) ;
#59075 = CARTESIAN_POINT ( 'NONE',  ( -1.364683531250012516, 4.238541667008090208, -0.7879004041258300672 ) ) ;
#59076 = CARTESIAN_POINT ( 'NONE',  ( -5.596818484342970912, 5.424043074688562172, -0.7998128361456221525 ) ) ;
#59077 = CARTESIAN_POINT ( 'NONE',  ( 6.419949431270806528, 7.448694743692793274, 1.199719254218462483 ) ) ;
#59078 = DIRECTION ( 'NONE',  ( 0.000000000000000000, 1.000000000000000000, 0.000000000000000000 ) ) ;
#59079 = CARTESIAN_POINT ( 'NONE',  ( 0.7683615598204245334, 1.039662503867449184, 1.831484773650635223 ) ) ;
#59081 = DIRECTION ( 'NONE',  ( -1.000000000000000000, 0.000000000000000000, 4.336808689942015369E-15 ) ) ;
#59080 = CARTESIAN_POINT ( 'NONE',  ( 0.6823417656249899377, 4.488541667008086655, -1.181850606188754593 ) ) ;
#59082 = CARTESIAN_POINT ( 'NONE',  ( 6.889893180375397996, -0.9309023296741396614, 1.948985471107896439 ) ) ;
#59083 = CARTESIAN_POINT ( 'NONE',  ( 2.127334043950947606, 1.896359100603739911, 0.9491756072362851349 ) ) ;
#59084 = CARTESIAN_POINT ( 'NONE',  ( 0.1760434994887878080, 1.997199259934297366, -0.3004917578056826022 ) ) ;
#59085 = CARTESIAN_POINT ( 'NONE',  ( 1.364683531249986537, 0.1135416670080857532, 0.7879004041258500513 ) ) ;
#59086 = CARTESIAN_POINT ( 'NONE',  ( -3.443407828190963915, 6.961133532957338943, 0.7216878364870317197 ) ) ;
#59087 = CARTESIAN_POINT ( 'NONE',  ( 6.634017235788401301, 6.634108284708264414, 0.7998128361456341429 ) ) ;
#59088 = CARTESIAN_POINT ( 'NONE',  ( 0.8784639925019833706, -1.201575844224999301, 1.796657101444132154 ) ) ;
#59091 = CARTESIAN_POINT ( 'NONE',  ( 3.931501358282940117, 4.649468341827285300, -1.082531754730543083 ) ) ;
#59090 = CARTESIAN_POINT ( 'NONE',  ( -1.642778471874998480, -0.7510416661887092671, 2.845375778867863303 ) ) ;
#59089 = CARTESIAN_POINT ( 'NONE',  ( 6.119526231721748033, 8.232809585132461194, 1.599625672291269396 ) ) ;
#59092 = FACE_OUTER_BOUND ( 'NONE', #67179, .T. ) ;
#59093 = CARTESIAN_POINT ( 'NONE',  ( 4.821500071095637274, -1.429446227384461032, -1.422610148874188463 ) ) ;
#59095 = CARTESIAN_POINT ( 'NONE',  ( -5.899206235277530297, 9.896508017883515862, 0.7216878364870267237 ) ) ;
#59094 = CARTESIAN_POINT ( 'NONE',  ( -9.327646496521989405, 10.94497100310623594, -1.082531754730539753 ) ) ;
#59096 = PRESENTATION_STYLE_ASSIGNMENT (( #92694 ) ) ;
#59098 = CARTESIAN_POINT ( 'NONE',  ( -8.012344526598182026E-15, 11.04687500034139624, -1.575800808251669460 ) ) ;
#59097 = CARTESIAN_POINT ( 'NONE',  ( 0.4446536212460248105, 2.256715800172736763, 0.1630166291790128841 ) ) ;
#59099 = CARTESIAN_POINT ( 'NONE',  ( -10.62011439820619429, 11.28455497419572318, -0.7998128361456221525 ) ) ;
#59101 = CARTESIAN_POINT ( 'NONE',  ( 6.257435441360899908, 1.928747933193178721, -0.5880367767025842518 ) ) ;
#59100 = CARTESIAN_POINT ( 'NONE',  ( -5.300874872818844175, 7.207439989753867238, 1.443375672974064550 ) ) ;
#59102 = CARTESIAN_POINT ( 'NONE',  ( 0.6823417656249882723, 0.4052083336747516751, 1.181850606188755259 ) ) ;
#59103 = CARTESIAN_POINT ( 'NONE',  ( 6.883263157960358924, 4.692138088316172073, 2.616388454592593504 ) ) ;
#59104 = CARTESIAN_POINT ( 'NONE',  ( -6.009258394948636914E-15, 8.937500000000001776, -1.732050807568875195 ) ) ;
#59105 = CARTESIAN_POINT ( 'NONE',  ( 3.281609485064349130, 1.095178418435642120, 1.332575575002497681 ) ) ;
#59106 = CARTESIAN_POINT ( 'NONE',  ( 6.481679955784983349, 9.719654494127929922, -1.199719254218452047 ) ) ;
#59107 = CARTESIAN_POINT ( 'NONE',  ( 6.391743074199808916, 6.421731439513382433, -0.7998128361456481317 ) ) ;
#59108 = CARTESIAN_POINT ( 'NONE',  ( 1.229378055282577042, -1.117200307070218779, -1.372552531265440523 ) ) ;
#59110 = CARTESIAN_POINT ( 'NONE',  ( 2.227199469478642335, 1.799111979166287512, 0.9032904990664193390 ) ) ;
#59109 = AXIS2_PLACEMENT_3D ( 'NONE', #171945, #39813, #89643 ) ;
#59111 = CARTESIAN_POINT ( 'NONE',  ( 6.883263157960401557, -0.003972766660575013931, 2.046037087719231096 ) ) ;
#59112 = CARTESIAN_POINT ( 'NONE',  ( 4.753059971535213535, -1.774748228059085164, 1.311344899593884561 ) ) ;
#59113 = CIRCLE ( 'NONE', #207836, 11.09999999999999964 ) ;
#59114 = ORIENTED_EDGE ( 'NONE', *, *, #166016, .F. ) ;
#59115 = CARTESIAN_POINT ( 'NONE',  ( 0.7499999999999867883, -0.6833333333333135862, -1.299038105676652899 ) ) ;
#59117 = CARTESIAN_POINT ( 'NONE',  ( 8.893785580440313865, 9.478430720042945623, 1.040834085586084257E-14 ) ) ;
#59116 = CIRCLE ( 'NONE', #124924, 0.08000000000000040412 ) ;
#59119 = CARTESIAN_POINT ( 'NONE',  ( 2.460564738353550496, -1.930424690641812768, -0.5826366834433827080 ) ) ;
#59118 = CARTESIAN_POINT ( 'NONE',  ( 4.565154201998150363, -1.702539431995837349, 1.263830167178958463 ) ) ;
#59121 = ORIENTED_EDGE ( 'NONE', *, *, #13614, .T. ) ;
#59120 = CARTESIAN_POINT ( 'NONE',  ( 2.882852291059742278, -1.675512013591500482, -0.6893320933419128105 ) ) ;
#59122 = CARTESIAN_POINT ( 'NONE',  ( 3.874598038455354665, 7.742391154831717692, -0.7998128361456362523 ) ) ;
#59123 = VERTEX_POINT ( 'NONE', #72459 ) ;
#59124 = CARTESIAN_POINT ( 'NONE',  ( 0.1802491246630563149, -1.813337052076903877, -0.4591185353455888296 ) ) ;
#59125 = CARTESIAN_POINT ( 'NONE',  ( 5.217190183160311356, 4.981143389975473568, -0.7998128361456211532 ) ) ;
#59126 = CARTESIAN_POINT ( 'NONE',  ( 5.830640656690653678, 1.760721658632548037, 0.4824517239352192344 ) ) ;
#59128 = CARTESIAN_POINT ( 'NONE',  ( 2.729585477426241802, 0.6851132086851609015, -1.789222977413899462 ) ) ;
#59127 = DIRECTION ( 'NONE',  ( -9.436895709313856232E-16, 0.8656921114426506803, 0.5005768354468324022 ) ) ;
#59129 = FILL_AREA_STYLE_COLOUR ( '', #37434 ) ;
#59130 = CARTESIAN_POINT ( 'NONE',  ( 1.364683531249986537, 2.217708333674751398, -0.7879004041258239610 ) ) ;
#59131 = CARTESIAN_POINT ( 'NONE',  ( 0.000000000000000000, 2.999999999999999112, 0.000000000000000000 ) ) ;
#59132 = CARTESIAN_POINT ( 'NONE',  ( 6.943184063974162434, 9.193743722760251202, -1.443375672974064550 ) ) ;
#59133 = CARTESIAN_POINT ( 'NONE',  ( -3.662110889467009578, 7.286563447771212232, 0.7216878364870338292 ) ) ;
#59134 = EDGE_CURVE ( 'NONE', #83956, #75921, #139638, .T. ) ;
#59135 = CARTESIAN_POINT ( 'NONE',  ( -7.435720902452096936, 7.639705572474380091, 0.000000000000000000 ) ) ;
#59136 = CARTESIAN_POINT ( 'NONE',  ( 2.777707764728345907, 0.3069055913166895966, -2.098134212408508059 ) ) ;
#59138 = CARTESIAN_POINT ( 'NONE',  ( -9.997759874121660673, 5.662387697485826266, 5.943071269081472430 ) ) ;
#59137 = CARTESIAN_POINT ( 'NONE',  ( -0.1296875068448125057, 0.2507808023153486054, -1.861542470327881560 ) ) ;
#59139 = CARTESIAN_POINT ( 'NONE',  ( 4.762937738300905721, -1.759534068222264436, -0.8891730789123506451 ) ) ;
#59140 = CARTESIAN_POINT ( 'NONE',  ( 6.345967646908174054, -1.254484226688237447, -1.443505786478386899 ) ) ;
#59141 = VERTEX_POINT ( 'NONE', #23714 ) ;
#59142 = CARTESIAN_POINT ( 'NONE',  ( -0.03531552556956805977, -2.054970391365168680, -0.5093743926467135807 ) ) ;
#59143 = CARTESIAN_POINT ( 'NONE',  ( 3.719872605471085336, 6.605953636083950364, 2.420000000000000373 ) ) ;
#59144 = CARTESIAN_POINT ( 'NONE',  ( 1.908725956546155178, 0.6474277305483535638, 1.966616875269424192 ) ) ;
#59145 = CARTESIAN_POINT ( 'NONE',  ( 2.255715180780485607, 0.8305992003537970847, 1.755491392210324353 ) ) ;
#59146 = EDGE_LOOP ( 'NONE', ( #189951, #92646, #9762, #12088 ) ) ;
#59147 = CARTESIAN_POINT ( 'NONE',  ( 4.667750024854814050, 8.667735138964429709, -0.7998128361456381397 ) ) ;
#59148 = CARTESIAN_POINT ( 'NONE',  ( 7.062871678076271920, 7.204714810702593120, -0.7998128361456341429 ) ) ;
#59150 = CARTESIAN_POINT ( 'NONE',  ( 5.361359679200154105, 8.342337828120466980, 1.199719254218462483 ) ) ;
#59149 = CARTESIAN_POINT ( 'NONE',  ( 4.066417572287989834, -1.950679019168543471, -0.7525511210752598990 ) ) ;
#59151 = CARTESIAN_POINT ( 'NONE',  ( 5.356880090730874677, 5.422317325373725794, 0.7216878364870328300 ) ) ;
#59153 = ORIENTED_EDGE ( 'NONE', *, *, #95699, .T. ) ;
#59152 = CARTESIAN_POINT ( 'NONE',  ( 0.8909134567714148689, -0.04341352697850982267, -1.811128585712480366 ) ) ;
#59154 = CARTESIAN_POINT ( 'NONE',  ( 5.321004863918796346, 2.037934703285459115, 0.8473243778325880715 ) ) ;
#59155 = LINE ( 'NONE', #190212, #54401 ) ;
#59156 = CARTESIAN_POINT ( 'NONE',  ( 3.680891063843365174, -2.126115503207156809, -0.5908918699835326027 ) ) ;
#59157 = CARTESIAN_POINT ( 'NONE',  ( 8.609591239877852686, 10.00327685373437347, -1.199719254218445830 ) ) ;
#59158 = ADVANCED_FACE ( 'NONE', ( #124517 ), #54297, .T. ) ;
#59159 = CARTESIAN_POINT ( 'NONE',  ( 2.754443878939544454, 1.898071056134968959, 0.2320119769325945103 ) ) ;
#59160 = CARTESIAN_POINT ( 'NONE',  ( 9.908311333488716954, 10.45411806535867782, 0.7998128361456462443 ) ) ;
#59161 = CARTESIAN_POINT ( 'NONE',  ( 4.826661161267837841, -1.354893614093263254, 1.565527137264411728 ) ) ;
#59163 = CARTESIAN_POINT ( 'NONE',  ( 2.395597313961893349, 1.670541196947441520, 1.371929806955954012 ) ) ;
#59162 = CARTESIAN_POINT ( 'NONE',  ( -3.015033485013444370, 6.452462698123035523, 0.6092158896764710008 ) ) ;
#59164 = CARTESIAN_POINT ( 'NONE',  ( 5.355090213057959403, 0.4282289882464126451, -2.149144931432686256 ) ) ;
#59165 = ORIENTED_EDGE ( 'NONE', *, *, #135967, .F. ) ;
#59166 = CARTESIAN_POINT ( 'NONE',  ( 1.607015867998833336, -0.9165151389911481150, 1.199999999999999734 ) ) ;
#59167 = CARTESIAN_POINT ( 'NONE',  ( 4.492547798081839794, 6.334668079219206049, 1.599625672291262513 ) ) ;
#59168 = CARTESIAN_POINT ( 'NONE',  ( 1.001543065824772753E-15, -2.909374999522043925, 3.793834371823810780 ) ) ;
#59169 = AXIS2_PLACEMENT_3D ( 'NONE', #138947, #55544, #76059 ) ;
#59170 = CARTESIAN_POINT ( 'NONE',  ( -8.676855123066019360, 11.14608361504227574, -1.443375672974059665 ) ) ;
#59171 = CARTESIAN_POINT ( 'NONE',  ( 5.387385936583818591, 7.378645907471495846, -1.599625672291283607 ) ) ;
#59172 = CARTESIAN_POINT ( 'NONE',  ( 5.946161111532238586, -0.9360204806616537754, 1.846680006623670156 ) ) ;
#59173 = CARTESIAN_POINT ( 'NONE',  ( 4.863854859025781074, 1.905264070129700782, -0.2845116402651908794 ) ) ;
#59174 = CARTESIAN_POINT ( 'NONE',  ( 0.2457205463545810431, 1.994068899247893434, -0.2986513045247774500 ) ) ;
#59175 = CARTESIAN_POINT ( 'NONE',  ( 5.993586425693011144, 9.150212042353954800, -1.199719254218452047 ) ) ;
#59177 = EDGE_CURVE ( 'NONE', #110911, #67678, #10851, .T. ) ;
#59176 = DIRECTION ( 'NONE',  ( -0.9446243521954068578, 0.000000000000000000, -0.3281536732072456997 ) ) ;
#59178 = CARTESIAN_POINT ( 'NONE',  ( 5.629738194587773137, 1.899041559284548208, -0.5217042529989719402 ) ) ;
#59179 = B_SPLINE_CURVE_WITH_KNOTS ( 'NONE', 3,
 ( #5592, #105291, #122684, #188647, #75969, #157235, #159349, #172411, #92255, #192899 ),
 .UNSPECIFIED., .F., .F.,
 ( 4, 2, 2, 2, 4 ),
 ( 5.529431079675726716E-18, 0.0002236660844579351078, 0.0004473321689158646862, 0.0006709982533737942918, 0.0008946643378317238431 ),
 .UNSPECIFIED. ) ;
#59180 = CARTESIAN_POINT ( 'NONE',  ( 6.714806895146447907, -0.1657305019511661481, 2.255884130952827249 ) ) ;
#59181 = CARTESIAN_POINT ( 'NONE',  ( 5.180226163740526246, -1.011166736308216629, 1.519887457628710248 ) ) ;
#59182 = PRODUCT ( 'chamber', 'chamber', '', ( #102406 ) ) ;
#59183 = EDGE_CURVE ( 'NONE', #140668, #131565, #103413, .T. ) ;
#59184 = CARTESIAN_POINT ( 'NONE',  ( 4.855228407469603269, 7.718164671139588151, -1.082531754730548412 ) ) ;
#59185 = CARTESIAN_POINT ( 'NONE',  ( 4.216222583725566686, 4.981643104843690217, -1.082531754730548412 ) ) ;
#59186 = CARTESIAN_POINT ( 'NONE',  ( -5.224688093219839402, 7.188831756880171397, -1.599625672291271394 ) ) ;
#59187 = CARTESIAN_POINT ( 'NONE',  ( 4.390861645979372341, 6.216034235099629157, -1.599625672291269396 ) ) ;
#59188 = ORIENTED_EDGE ( 'NONE', *, *, #119616, .F. ) ;
#59190 = CARTESIAN_POINT ( 'NONE',  ( 0.06508986333318785011, -1.615617207129100397, 1.200762793324720690 ) ) ;
#59189 = CARTESIAN_POINT ( 'NONE',  ( 2.278628554356322500, 1.682734121078124812, -0.7478279864501293783 ) ) ;
#59191 = CARTESIAN_POINT ( 'NONE',  ( 0.5624050986996537160, 1.909334820886617656, -1.279222687617764809 ) ) ;
#59192 = CARTESIAN_POINT ( 'NONE',  ( 5.629730433169950921, 1.891637868780412068, -0.5196590155819302836 ) ) ;
#59193 = CARTESIAN_POINT ( 'NONE',  ( -4.394814349124112951, 8.279033840620114049, -0.7998128361456281477 ) ) ;
#59194 = CARTESIAN_POINT ( 'NONE',  ( -3.972702704004144714, 4.593573561881607148, 1.199719254218462483 ) ) ;
#59195 = DIRECTION ( 'NONE',  ( -5.578564026256490882E-16, -1.000000000000000000, -9.066213480720158442E-32 ) ) ;
#59196 = CARTESIAN_POINT ( 'NONE',  ( -4.502189528189771472, 7.410248995266807803, -1.199719254218453823 ) ) ;
#59198 = CARTESIAN_POINT ( 'NONE',  ( 1.147088892781012781, -1.472398045354219365, -1.153743250124287689 ) ) ;
#59197 = CARTESIAN_POINT ( 'NONE',  ( 1.066094891556510271, -1.323660828648763221, 1.618394379614082723 ) ) ;
#59199 = CARTESIAN_POINT ( 'NONE',  ( 1.757185253014027282, -2.006138798620077157, -0.2004061740628823030 ) ) ;
#59200 = CARTESIAN_POINT ( 'NONE',  ( 1.364683531249988535, 4.426041667008082214, 0.7879004041258499402 ) ) ;
#59201 = CARTESIAN_POINT ( 'NONE',  ( 2.348798421458723862, 0.4629176777091792983, -1.677682632058958845 ) ) ;
#59202 = CARTESIAN_POINT ( 'NONE',  ( 5.443762371086860341, 6.309809840144842141, 1.199719254218462483 ) ) ;
#59204 = CARTESIAN_POINT ( 'NONE',  ( 1.507330767849599962, 8.672482115169971806, 2.545833800658963142 ) ) ;
#59203 = FILL_AREA_STYLE ('',( #122169 ) ) ;
#59205 = CARTESIAN_POINT ( 'NONE',  ( 3.263966975432155415, 0.7763617936313322865, 1.540355606630551710 ) ) ;
#59206 = CARTESIAN_POINT ( 'NONE',  ( 2.577880719133851084, -1.123996537731044354, 1.881222605751430521 ) ) ;
#59207 = CARTESIAN_POINT ( 'NONE',  ( 5.145248760827346501, -1.894204247122273088, 1.132176536499051700 ) ) ;
#59208 = CARTESIAN_POINT ( 'NONE',  ( -10.20559888102932256, 5.000029895416906456, -7.525687786258633771 ) ) ;
#59209 = CARTESIAN_POINT ( 'NONE',  ( 2.624086282063769815, 2.129961278301984784, -0.4196836606994054364 ) ) ;
#59210 = CARTESIAN_POINT ( 'NONE',  ( 1.242498012622397674, 0.3540479964400863877, 1.790853789395550955 ) ) ;
#59211 = CARTESIAN_POINT ( 'NONE',  ( 3.239577248433673784, 0.5100137816880914166, -2.054909399002705861 ) ) ;
#59212 = CARTESIAN_POINT ( 'NONE',  ( 6.539320575229287336, 0.5820952121784334077, 2.049435377300548033 ) ) ;
#59213 = ORIENTED_EDGE ( 'NONE', *, *, #64826, .T. ) ;
#59215 = CARTESIAN_POINT ( 'NONE',  ( -0.6823417656250212460, 1.363541667008083547, 1.181850606188755259 ) ) ;
#59214 = CARTESIAN_POINT ( 'NONE',  ( 3.491970780479057179, -2.289775125716007054, -0.1112369151145074092 ) ) ;
#59216 = CARTESIAN_POINT ( 'NONE',  ( 6.518203450479836292, 5.167241622962441383, 2.437504649502901355 ) ) ;
#59217 = CARTESIAN_POINT ( 'NONE',  ( 2.869522067586683711, 6.499526178826442013, 0.7998128361456362523 ) ) ;
#59218 = CARTESIAN_POINT ( 'NONE',  ( 5.584718243131947091, -1.410645330893144589, 1.715908544892131626 ) ) ;
#59219 = CARTESIAN_POINT ( 'NONE',  ( -5.585596099150182958, 8.499983968108443477, -1.082531754730544860 ) ) ;
#59220 = CARTESIAN_POINT ( 'NONE',  ( 3.226477370372293763, 6.708047998835573900, 0.7216878364870317197 ) ) ;
#59221 = CARTESIAN_POINT ( 'NONE',  ( -7.009202228140755331, 8.240119356661432803, -1.082531754730543083 ) ) ;
#59222 = CARTESIAN_POINT ( 'NONE',  ( 0.000000000000000000, -9.911192131523236526, 10.91970695577495931 ) ) ;
#59223 = ORIENTED_EDGE ( 'NONE', *, *, #101206, .T. ) ;
#59224 = CARTESIAN_POINT ( 'NONE',  ( 4.623672751230786027, 0.3474658942751900903, 1.986100912583692812 ) ) ;
#59226 = CARTESIAN_POINT ( 'NONE',  ( 3.854389151762872778, -2.059979072249884080, -0.1062074158154867054 ) ) ;
#59225 = CARTESIAN_POINT ( 'NONE',  ( 6.986529229743720926, 7.045372277656132276, -0.7998128361456281477 ) ) ;
#59227 = CARTESIAN_POINT ( 'NONE',  ( 6.831329296439236032, 9.063246493969506545, -1.599625672291267398 ) ) ;
#59228 = CARTESIAN_POINT ( 'NONE',  ( 3.051993976407674225, 6.574760382535328240, -0.7216878364870338292 ) ) ;
#59229 = CARTESIAN_POINT ( 'NONE',  ( -1.642778471874998480, -2.851041666188706802, 2.845375778867863303 ) ) ;
#59230 = CARTESIAN_POINT ( 'NONE',  ( -1.364683531250010295, 5.280208333674758059, 0.7879004041258379498 ) ) ;
#59231 = CARTESIAN_POINT ( 'NONE',  ( 6.052700813158569559, -1.877759139263988297, -1.129571069393126459 ) ) ;
#59232 = CARTESIAN_POINT ( 'NONE',  ( 3.094375128876575065, -0.3905979561782264575, 1.978050703236901686 ) ) ;
#59233 = CARTESIAN_POINT ( 'NONE',  ( 2.718100415690410721, 1.734538518968967935, 0.6181264464550640936 ) ) ;
#59234 = CARTESIAN_POINT ( 'NONE',  ( 5.120175567455225618, 9.125288595339771547, -0.7998128361456281477 ) ) ;
#59235 = CARTESIAN_POINT ( 'NONE',  ( 6.458013382736495167, 1.820430347099718293, -0.1376817787434730933 ) ) ;
#59236 = CARTESIAN_POINT ( 'NONE',  ( -0.08672817704761734414, -1.422268874607252043, -1.807091132531572608 ) ) ;
#59237 = CARTESIAN_POINT ( 'NONE',  ( -8.064402442030170093, 8.302891025323665630, 0.7998128361456602331 ) ) ;
#59239 = CARTESIAN_POINT ( 'NONE',  ( -5.601453741101424022, 6.564059448486966986, -1.199719254218453823 ) ) ;
#59238 = CARTESIAN_POINT ( 'NONE',  ( 5.911039803662155201, 1.992093809783651803, 1.072660102914186897 ) ) ;
#59240 = CARTESIAN_POINT ( 'NONE',  ( 1.946058636591390334, 0.8049280153260234272, -1.946384432229040673 ) ) ;
#59241 = B_SPLINE_CURVE_WITH_KNOTS ( 'NONE', 3,
 ( #30142, #64764, #147108, #113593, #144997, #179596, #31217, #114656, #130906, #196898 ),
 .UNSPECIFIED., .F., .F.,
 ( 4, 2, 2, 2, 4 ),
 ( 7.239403734744659911E-05, 0.0003307887970069321769, 0.0005891835566664177818, 0.0008475783163259033868, 0.001105973075985389100 ),
 .UNSPECIFIED. ) ;
#59242 = CARTESIAN_POINT ( 'NONE',  ( -4.776215253764153346, 8.794277906025310898, -0.7998128361456362523 ) ) ;
#59243 = CARTESIAN_POINT ( 'NONE',  ( 9.426996880203592610, 9.892584536526015881, -0.7998128361456281477 ) ) ;
#59244 = CARTESIAN_POINT ( 'NONE',  ( 5.994113310573177422, 10.00723293906178846, 0.000000000000000000 ) ) ;
#59245 = CARTESIAN_POINT ( 'NONE',  ( -8.148614017013223076, 9.465470093725620870, -1.199719254218446718 ) ) ;
#59246 = CARTESIAN_POINT ( 'NONE',  ( -3.783109326081552037, 7.353282959184841872, -0.6894747432927388342 ) ) ;
#59247 = CARTESIAN_POINT ( 'NONE',  ( 7.659993601596707613, 9.959745173328078849, -1.443375672974058777 ) ) ;
#59248 = CARTESIAN_POINT ( 'NONE',  ( 4.035592002476674267, 7.779268892024251869, 0.4218195438757850191 ) ) ;
#59249 = CARTESIAN_POINT ( 'NONE',  ( -6.261168011412601153, 6.199117522936475666, 1.040834085586084257E-14 ) ) ;
#59251 = CARTESIAN_POINT ( 'NONE',  ( 2.672393786618231015, 2.210292516208379521, -0.2222851140616446397 ) ) ;
#59250 = CARTESIAN_POINT ( 'NONE',  ( 2.039458538997685366, 0.004855507148140979744, 2.120778211687989856 ) ) ;
#59252 = CARTESIAN_POINT ( 'NONE',  ( 0.08304785351339466493, -2.141800023564765620, -0.5316218738360134477 ) ) ;
#59253 = CARTESIAN_POINT ( 'NONE',  ( -5.204350862799341115, 7.165104988056252289, -1.599625672291271394 ) ) ;
#59254 = CARTESIAN_POINT ( 'NONE',  ( 5.443762371086860341, 6.309809840144842141, 1.199719254218462483 ) ) ;
#59255 = CARTESIAN_POINT ( 'NONE',  ( 4.475024536774164119, 1.792854848340214025, 0.7970393728587571447 ) ) ;
#59256 = CARTESIAN_POINT ( 'NONE',  ( 9.836604141914616406, 11.43479190611061647, 1.199719254218452047 ) ) ;
#59257 = CARTESIAN_POINT ( 'NONE',  ( -4.868194452378435955, 6.719997196398590056, 1.250117667640719077 ) ) ;
#59258 = CARTESIAN_POINT ( 'NONE',  ( -1.580803134831892276, 0.9624764945123778226, 1.305310695360494710 ) ) ;
#59259 = CARTESIAN_POINT ( 'NONE',  ( -1.402160292154681736E-14, 0.4468750003414233563, -1.575800808251665908 ) ) ;
#59260 = EDGE_CURVE ( 'NONE', #86738, #159273, #114387, .T. ) ;
#59261 = CARTESIAN_POINT ( 'NONE',  ( -5.533136088152923904, 6.588318536667425285, 1.082531754730549078 ) ) ;
#59263 = ORIENTED_EDGE ( 'NONE', *, *, #124881, .F. ) ;
#59262 = CARTESIAN_POINT ( 'NONE',  ( -6.738039156311804945, 6.963393225226301553, 1.040834085586084257E-14 ) ) ;
#59264 = AXIS2_PLACEMENT_3D ( 'NONE', #145111, #128901, #194882 ) ;
#59265 = CARTESIAN_POINT ( 'NONE',  ( 3.375340920106313813, -1.871962376360849056, -0.9962781187466958066 ) ) ;
#59266 = CARTESIAN_POINT ( 'NONE',  ( -4.437261413422502798, 8.398831758960053406, 0.000000000000000000 ) ) ;
#59267 = CARTESIAN_POINT ( 'NONE',  ( 5.278265135069068137, -1.204163492603943064, 1.795060720813673738 ) ) ;
#59268 = CARTESIAN_POINT ( 'NONE',  ( 4.089279031174639201, -0.7008038172400687937, 1.702867937621636463 ) ) ;
#59269 = CARTESIAN_POINT ( 'NONE',  ( 4.909388789075159742, -1.913262893431907141, 0.6371506334161003426 ) ) ;
#59270 = MECHANICAL_DESIGN_GEOMETRIC_PRESENTATION_REPRESENTATION (  '', ( #118249 ), #183877 ) ;
#59271 = CARTESIAN_POINT ( 'NONE',  ( -5.901816349531303629, 6.006251404816039141, -0.1731548415426099052 ) ) ;
#59272 = CARTESIAN_POINT ( 'NONE',  ( -1.364683531250012516, 0.8427083336747532849, 0.7879004041258379498 ) ) ;
#59273 = CARTESIAN_POINT ( 'NONE',  ( 6.544851825567233661, -1.402524398529688021, -1.030163739638074727 ) ) ;
#59274 = CARTESIAN_POINT ( 'NONE',  ( 6.827182134110200806, 1.308106637204756728, 1.828351192278207638 ) ) ;
#59275 = CARTESIAN_POINT ( 'NONE',  ( 4.690757960648234359, 4.574898496952131133, 0.7216878364870317197 ) ) ;
#59276 = CARTESIAN_POINT ( 'NONE',  ( 7.960204194457795477E-17, 13.49999999999999822, 0.6500000000000000222 ) ) ;
#59277 = CARTESIAN_POINT ( 'NONE',  ( 4.557600102482579629, 0.4766696971462945909, -2.108333899287537339 ) ) ;
#59278 = CARTESIAN_POINT ( 'NONE',  ( 5.202499893966790800, -1.423744420606623429, -1.427717849564233532 ) ) ;
#59279 = CARTESIAN_POINT ( 'NONE',  ( -7.334597914868722590, 11.50085530074811935, -0.7216878364870267237 ) ) ;
#59280 = CARTESIAN_POINT ( 'NONE',  ( 3.186554565756247737, -2.129457467500107004, -0.3711038070777841202 ) ) ;
#59281 =( BOUNDED_SURFACE ( )  B_SPLINE_SURFACE ( 3, 2, ( 
 ( #25533, #92701, #158747 ),
 ( #93767, #208534, #202 ),
 ( #147576, #64189, #163829 ),
 ( #115128, #181123, #60170 ),
 ( #132420, #91641, #157694 ),
 ( #207483, #43946, #80431 ),
 ( #146531, #130330, #196319 ),
 ( #15407, #81498, #99881 ) ),
 .UNSPECIFIED., .F., .F., .T. ) 
 B_SPLINE_SURFACE_WITH_KNOTS ( ( 4, 2, 2, 4 ),
 ( 3, 3 ),
 ( 5.963111948670274387E-19, 0.0002475938981900011613, 0.0004951877963800016720, 0.0009903755927600026935 ),
 ( 0.000000000000000000, 1.000000000000000000 ),
 .UNSPECIFIED. ) 
 GEOMETRIC_REPRESENTATION_ITEM ( )  RATIONAL_B_SPLINE_SURFACE ( (
 ( 1.000000000000000000, 0.9238795325112872936, 1.000000000000000000),
 ( 1.000000000000000000, 0.9248499699753846004, 1.000000000000000000),
 ( 1.000000000000000000, 0.9171047238582999972, 1.000000000000000000),
 ( 1.000000000000000000, 0.8907236462369912955, 1.000000000000000000),
 ( 1.000000000000000000, 0.8725411758594774358, 1.000000000000000000),
 ( 1.000000000000000000, 0.8105159241142789739, 1.000000000000000000),
 ( 1.000000000000000000, 0.7599483315140537210, 1.000000000000000000),
 ( 1.000000000000000000, 0.7045118851637761637, 1.000000000000000000) ) ) 
 REPRESENTATION_ITEM ( '' )  SURFACE ( )  );
#59282 = CARTESIAN_POINT ( 'NONE',  ( 3.673081450605990117, 0.05180205286909286139, -1.970847691630872811 ) ) ;
#59283 = CARTESIAN_POINT ( 'NONE',  ( 0.2401087780563165297, 2.186128513634697512, 0.1550312349237955856 ) ) ;
#59284 = CARTESIAN_POINT ( 'NONE',  ( 0.9214421848816763960, 2.133375822355741303, 0.8800392910873405805 ) ) ;
#59285 = CARTESIAN_POINT ( 'NONE',  ( 2.952472966291960876, 0.6911811108033919515, 1.941568756818631725 ) ) ;
#59286 = CARTESIAN_POINT ( 'NONE',  ( 5.108904621496645149, -0.2812511558281989288, 1.921465535368711786 ) ) ;
#59289 = EDGE_LOOP ( 'NONE', ( #129581, #211528, #175477 ) ) ;
#59288 = CARTESIAN_POINT ( 'NONE',  ( 11.41381675112453387, 12.69999999999999929, -3.704697986577184299 ) ) ;
#59287 = CARTESIAN_POINT ( 'NONE',  ( -7.971831134711019118, 12.24429405723079967, 0.000000000000000000 ) ) ;
#59290 = CARTESIAN_POINT ( 'NONE',  ( -5.108390017298964914, 9.181815130149269422, 0.000000000000000000 ) ) ;
#59291 = CARTESIAN_POINT ( 'NONE',  ( -11.92045683181315674, 12.44724072120513547, 1.382340670101856350 ) ) ;
#59293 = ORIENTED_EDGE ( 'NONE', *, *, #45047, .F. ) ;
#59292 = CARTESIAN_POINT ( 'NONE',  ( -3.305155586681401303, 7.078041627762083898, 0.7998128361456352531 ) ) ;
#59294 = CARTESIAN_POINT ( 'NONE',  ( -8.039621902779392926, 9.442275643739831636, 1.082531754730558626 ) ) ;
#59295 = CARTESIAN_POINT ( 'NONE',  ( 2.028631293930313717, 1.270571802522667992, -1.804104215285810886 ) ) ;
#59296 = CARTESIAN_POINT ( 'NONE',  ( 0.000000000000000000, -3.084374999522042859, -3.793834371823813001 ) ) ;
#59297 = CARTESIAN_POINT ( 'NONE',  ( 6.543807102324334934, 1.350441955444921849, 1.423202910149905298 ) ) ;
#59298 =( BOUNDED_SURFACE ( )  B_SPLINE_SURFACE ( 3, 2, ( 
 ( #162172, #178421, #157912 ),
 ( #177350, #127622, #175231 ),
 ( #206629, #27892, #12686 ),
 ( #9507, #75579, #43106 ) ),
 .UNSPECIFIED., .F., .F., .F. ) 
 B_SPLINE_SURFACE_WITH_KNOTS ( ( 4, 4 ),
 ( 3, 3 ),
 ( 0.01126995942960227343, 0.01373815140602661217 ),
 ( 0.000000000000000000, 1.000000000000000000 ),
 .UNSPECIFIED. ) 
 GEOMETRIC_REPRESENTATION_ITEM ( )  RATIONAL_B_SPLINE_SURFACE ( (
 ( 1.000000000000000000, 0.6947640035331654751, 1.000000000000000000),
 ( 1.000000000000000000, 0.6955505939616328792, 1.000000000000000000),
 ( 1.000000000000000000, 0.6961913616428423435, 1.000000000000000000),
 ( 1.000000000000000000, 0.6967468848049983565, 1.000000000000000000) ) ) 
 REPRESENTATION_ITEM ( '' )  SURFACE ( )  );
#59299 = CARTESIAN_POINT ( 'NONE',  ( 9.093502852636627054, 1.000000000000000888, 7.666967846417570343 ) ) ;
#59300 = CARTESIAN_POINT ( 'NONE',  ( -1.201851678989727383E-14, 4.618750000682821266, -1.732050807568863648 ) ) ;
#59301 = CARTESIAN_POINT ( 'NONE',  ( 4.254006295369892499, 7.509857431501010261, -1.008242097476583554 ) ) ;
#59303 = CARTESIAN_POINT ( 'NONE',  ( -1.436838838544729491, 7.449283400311743186, -4.203727439823575551 ) ) ;
#59302 = CARTESIAN_POINT ( 'NONE',  ( 0.1749903794560410675, 1.362372954287846882, -2.209288650253756536 ) ) ;
#59304 = CARTESIAN_POINT ( 'NONE',  ( 5.718664505737725001, -0.04093049815006092468, 1.840854889930729543 ) ) ;
#59305 = ORIENTED_EDGE ( 'NONE', *, *, #185371, .T. ) ;
#59306 = CARTESIAN_POINT ( 'NONE',  ( 2.764585236803930979, -1.422233405468891210, 1.491712647946776826 ) ) ;
#59307 = CARTESIAN_POINT ( 'NONE',  ( 1.360316468749981800, -1.005208332991882614, 0.7853790794158560518 ) ) ;
#59308 = CARTESIAN_POINT ( 'NONE',  ( -6.181627972826976958, 9.299317504018391745, 1.199719254218452047 ) ) ;
#59309 = CARTESIAN_POINT ( 'NONE',  ( 10.91944941500665855, -9.999999999999994671, -0.1017788107271373199 ) ) ;
#59310 = CARTESIAN_POINT ( 'NONE',  ( 6.398696098476772676, -2.079943653215409416, -0.4123558718646391785 ) ) ;
#59311 = CARTESIAN_POINT ( 'NONE',  ( 11.71312635250765055, 6.993950423356553259, 2.415994165151631901 ) ) ;
#59312 = CARTESIAN_POINT ( 'NONE',  ( 4.527533231959700366, 7.369540306339926516, 1.199719254218462483 ) ) ;
#59313 = EDGE_CURVE ( 'NONE', #42674, #177025, #33585, .T. ) ;
#59314 = CARTESIAN_POINT ( 'NONE',  ( 0.6025036485793239249, -0.6938342907959176298, -1.940726168717278322 ) ) ;
#59315 =( BOUNDED_SURFACE ( )  B_SPLINE_SURFACE ( 3, 2, ( 
 ( #113569, #194740, #77795 ),
 ( #14902, #97266, #142839 ),
 ( #112496, #46377, #143914 ),
 ( #125572, #95138, #212037 ),
 ( #60475, #177439, #209909 ),
 ( #13843, #178506, #163322 ),
 ( #61546, #162257, #141780 ),
 ( #126633, #191533, #193673 ) ),
 .UNSPECIFIED., .F., .F., .F. ) 
 B_SPLINE_SURFACE_WITH_KNOTS ( ( 4, 2, 2, 4 ),
 ( 3, 3 ),
 ( 5.421010862427522170E-20, 0.0005123566476021758223, 0.0007685349714032637877, 0.001024713295204351645 ),
 ( 0.000000000000000000, 1.000000000000000000 ),
 .UNSPECIFIED. ) 
 GEOMETRIC_REPRESENTATION_ITEM ( )  RATIONAL_B_SPLINE_SURFACE ( (
 ( 1.000000000000000000, 0.7100530722026823227, 1.000000000000000000),
 ( 1.000000000000000000, 0.7667719522827172174, 1.000000000000000000),
 ( 1.000000000000000000, 0.8160440554223276077, 1.000000000000000000),
 ( 1.000000000000000000, 0.8737249316769536422, 1.000000000000000000),
 ( 1.000000000000000000, 0.8903164784319999026, 1.000000000000000000),
 ( 1.000000000000000000, 0.9150853305241253288, 1.000000000000000000),
 ( 1.000000000000000000, 0.9227739504732664910, 1.000000000000000000),
 ( 1.000000000000000000, 0.9238795325112855172, 1.000000000000000000) ) ) 
 REPRESENTATION_ITEM ( '' )  SURFACE ( )  );
#59318 = CARTESIAN_POINT ( 'NONE',  ( 4.686955257832659427, 1.367739038236553517, 1.232883728221023212 ) ) ;
#59317 = CARTESIAN_POINT ( 'NONE',  ( 2.347915429038241353, -0.7989592750466242288, 1.680985684562475990 ) ) ;
#59316 = CARTESIAN_POINT ( 'NONE',  ( -10.58872653680447939, -6.465328379374283507, 1.138412281109779656E-15 ) ) ;
#59319 = CARTESIAN_POINT ( 'NONE',  ( 6.877010230629674759, 9.046264573866535486, 1.599625672291281386 ) ) ;
#59320 = CARTESIAN_POINT ( 'NONE',  ( -6.024157315724540496, 15.51887179519442306, 10.38786933647550192 ) ) ;
#59321 = CARTESIAN_POINT ( 'NONE',  ( -5.956828388357799042, 8.042995434541133193, 1.599625672291263179 ) ) ;
#59323 = ORIENTED_EDGE ( 'NONE', *, *, #1599, .F. ) ;
#59322 = CARTESIAN_POINT ( 'NONE',  ( -11.37385970535894231, 1.000000000000000888, 3.825613075418397457 ) ) ;
#59324 = CARTESIAN_POINT ( 'NONE',  ( 4.371826309796801979, 2.140994599346605742, -0.5347268394074317088 ) ) ;
#59325 = CARTESIAN_POINT ( 'NONE',  ( 6.397788901632932124, -0.7711469528366134973, 2.127058432633963658 ) ) ;
#59326 = CARTESIAN_POINT ( 'NONE',  ( -5.260200412422208593, 7.159986452624450770, -1.443375672974053447 ) ) ;
#59327 = CARTESIAN_POINT ( 'NONE',  ( 0.5625819312903357350, 0.5574351770905332515, 1.829310545699929458 ) ) ;
#59328 = CARTESIAN_POINT ( 'NONE',  ( 0.1632964843477149597, 1.879801964727344732, -0.7303121171872913875 ) ) ;
#59329 = EDGE_CURVE ( 'NONE', #81332, #57617, #150018, .T. ) ;
#59330 = FACE_OUTER_BOUND ( 'NONE', #164123, .T. ) ;
#59331 = CARTESIAN_POINT ( 'NONE',  ( -11.86239285000045918, 11.37999999999999901, -1.812080536912752837 ) ) ;
#59332 = EDGE_CURVE ( 'NONE', #206986, #166319, #74621, .T. ) ;
#59333 = CARTESIAN_POINT ( 'NONE',  ( 5.901015568784107046, -0.2851453878830525479, -1.890788771128081969 ) ) ;
#59334 = CARTESIAN_POINT ( 'NONE',  ( 4.017000712418451691, 7.784014420058316119, -0.3037147205706329789 ) ) ;
#59335 = AXIS2_PLACEMENT_3D ( 'NONE', #23111, #70790, #5783 ) ;
#59336 = CARTESIAN_POINT ( 'NONE',  ( 0.7076149179639171782, -1.862046558926268913, 0.1791945732521060819 ) ) ;
#59337 = CARTESIAN_POINT ( 'NONE',  ( 2.958220528980558761, -1.197304571117228100, 1.622486353517027968 ) ) ;
#59339 = CARTESIAN_POINT ( 'NONE',  ( 4.160836958300685673, -1.560740793797481318, 1.414261741400888006 ) ) ;
#59338 = CARTESIAN_POINT ( 'NONE',  ( -7.991641480251377772, 11.41099992934688956, 1.199719254218453823 ) ) ;
#59340 = CARTESIAN_POINT ( 'NONE',  ( 9.108380270282433244, 9.520865158284665952, 1.040834085586084257E-14 ) ) ;
#59342 = CARTESIAN_POINT ( 'NONE',  ( -8.474009703741204547, 9.845098394908269768, -1.199719254218446718 ) ) ;
#59341 = CARTESIAN_POINT ( 'NONE',  ( -1.402160292154681736E-14, 0.08750000000001964540, -1.732050807568870754 ) ) ;
#59343 = CARTESIAN_POINT ( 'NONE',  ( 0.000000000000000000, 4.446955548196733332, 0.000000000000000000 ) ) ;
#59344 = CARTESIAN_POINT ( 'NONE',  ( 3.164323975240455944, 2.019972749466778073, -0.004219792236043878007 ) ) ;
#59345 = CARTESIAN_POINT ( 'NONE',  ( 1.364683531249990311, 5.363541667008086655, 0.7879004041258500513 ) ) ;
#59346 = CARTESIAN_POINT ( 'NONE',  ( 9.598809568795314107, 10.30095870645710754, -0.7216878364870257245 ) ) ;
#59347 = CARTESIAN_POINT ( 'NONE',  ( 4.059979352932830743, 2.145800628424157974, -0.2601280725000321148 ) ) ;
#59348 = CARTESIAN_POINT ( 'NONE',  ( -1.001543065824772872E-14, 5.712500000000021672, 1.732050807568877637 ) ) ;
#59349 = CARTESIAN_POINT ( 'NONE',  ( 4.505052181490820651, 8.477920988373101707, -0.7998128361456381397 ) ) ;
#59350 = CARTESIAN_POINT ( 'NONE',  ( 7.226132685959389512, 11.37431253368722750, -0.7216878364870267237 ) ) ;
#59352 = CARTESIAN_POINT ( 'NONE',  ( -0.1645940602202590475, -7.825441678136469292, 10.99897937609845044 ) ) ;
#59351 = CARTESIAN_POINT ( 'NONE',  ( 2.295604378506800103, -1.940070289243904567, 0.9748468494522060102 ) ) ;
#59354 = CARTESIAN_POINT ( 'NONE',  ( 0.8547319020580852467, 0.3593373433725781108, -1.805665335529122784 ) ) ;
#59353 = CARTESIAN_POINT ( 'NONE',  ( -5.910991785878170646, 7.919243054989755670, -1.443375672974059665 ) ) ;
#59355 = CARTESIAN_POINT ( 'NONE',  ( 1.364683531249986537, 1.405208333674755838, -0.7879004041258239610 ) ) ;
#59356 = CARTESIAN_POINT ( 'NONE',  ( 1.663894474538109236, 1.130263417742288112, 1.877492182091732076 ) ) ;
#59357 = CARTESIAN_POINT ( 'NONE',  ( 6.983263157960331036, 2.967600560354208383, 2.406739638166929041 ) ) ;
#59358 = CARTESIAN_POINT ( 'NONE',  ( 3.256942907105137230, -1.714491093362701335, 1.476422526664717072 ) ) ;
#59359 = CARTESIAN_POINT ( 'NONE',  ( -5.910464900553636269, 8.982960586366182554, -1.199719254218440723 ) ) ;
#59360 = CARTESIAN_POINT ( 'NONE',  ( 4.487517715496184501, -0.5331711073110931842, 1.944729879240604253 ) ) ;
#59361 = CARTESIAN_POINT ( 'NONE',  ( -1.364683531249997417, 5.071875000341417916, 1.214306433183764966E-14 ) ) ;
#59362 = CARTESIAN_POINT ( 'NONE',  ( 5.542547785767838242, 7.428594929708664196, 1.247761615041423244 ) ) ;
#59363 = CIRCLE ( 'NONE', #190772, 0.08000000000000012657 ) ;
#59364 = CARTESIAN_POINT ( 'NONE',  ( 0.7500000000000006661, 12.16666666666666607, -1.299038105676657340 ) ) ;
#59365 = CARTESIAN_POINT ( 'NONE',  ( 7.187230829020129441, 8.518095734345896730, 1.082531754730549967 ) ) ;
#59366 = CARTESIAN_POINT ( 'NONE',  ( 4.815556489234497306, -1.735627832820924477, 0.3447801454335273630 ) ) ;
#59367 =( BOUNDED_CURVE ( )  B_SPLINE_CURVE ( 2, ( #145401, #211401, #63030, #129197, #25190, #157352, #8941, #207142, #58766 ),
 .UNSPECIFIED., .F., .T. ) 
 B_SPLINE_CURVE_WITH_KNOTS ( ( 3, 2, 2, 2, 3 ),
 ( 0.6875000000000000000, 0.6944444444444444198, 0.7083333333333333703, 0.7222222222222222099, 0.7246580528728726600 ),
 .UNSPECIFIED. ) 
 CURVE ( )  GEOMETRIC_REPRESENTATION_ITEM ( )  RATIONAL_B_SPLINE_CURVE ( ( 0.9330127018922194093, 0.9330127018922194093, 1.000000000000000000, 0.8660254037844387076, 1.000000000000000000, 0.8660254037844387076, 1.000000000000000000, 0.9765035611933325921, 0.9612487241856686460 ) ) 
 REPRESENTATION_ITEM ( '' )  );
#59368 = CARTESIAN_POINT ( 'NONE',  ( 10.23370702021670020, 10.83374636654133383, 0.7998128361456462443 ) ) ;
#59369 = CARTESIAN_POINT ( 'NONE',  ( 0.2179827029432715169, -2.065224962065722369, 0.4112614876821736321 ) ) ;
#59371 = CARTESIAN_POINT ( 'NONE',  ( 1.499999999999987121, 1.754166666666691521, 0.8660254037844524744 ) ) ;
#59370 = CARTESIAN_POINT ( 'NONE',  ( -1.402160292154681736E-14, 11.17187500034139802, 1.575800808251682339 ) ) ;
#59372 = CARTESIAN_POINT ( 'NONE',  ( -6.310394152517827315, 6.326824364217716656, 0.7998128361456281477 ) ) ;
#59373 = CARTESIAN_POINT ( 'NONE',  ( 6.503528962204017994, -1.955192063461574259, 0.4926555484118036454 ) ) ;
#59375 = ORIENTED_EDGE ( 'NONE', *, *, #201642, .T. ) ;
#59374 = CARTESIAN_POINT ( 'NONE',  ( 5.273626195773981173, 0.3454419319289269708, -1.778163250140889717 ) ) ;
#59376 = CARTESIAN_POINT ( 'NONE',  ( 7.456621297836078632, 8.762108271306003004, 1.082531754730558626 ) ) ;
#59377 = CIRCLE ( 'NONE', #90478, 11.54340198673881979 ) ;
#59378 = CARTESIAN_POINT ( 'NONE',  ( 10.09812548408005384, 10.67556790771522124, -0.7998128361456281477 ) ) ;
#59379 = CARTESIAN_POINT ( 'NONE',  ( 4.153091690245942047, -1.555063956268587066, -1.039456662654779207 ) ) ;
#59380 = CARTESIAN_POINT ( 'NONE',  ( 4.082924941702062327, 1.964217522864346810, 0.6541895251909736198 ) ) ;
#59381 = CARTESIAN_POINT ( 'NONE',  ( -4.787437638956920871, 8.599444655509458357, -0.7216878364870338292 ) ) ;
#59382 = CARTESIAN_POINT ( 'NONE',  ( -1.833030277982348411, 0.000000000000000000, 2.500000000000000444 ) ) ;
#59383 = CARTESIAN_POINT ( 'NONE',  ( 8.860417081730671995, 10.29590700256267155, 1.199719254218453823 ) ) ;
#59384 = CARTESIAN_POINT ( 'NONE',  ( -9.236128959407555072, 11.79856975744075598, -1.599625672291263179 ) ) ;
#59385 = DIRECTION ( 'NONE',  ( 0.000000000000000000, 1.000000000000000000, 0.000000000000000000 ) ) ;
#59386 = LINE ( 'NONE', #174237, #128586 ) ;
#59387 = CARTESIAN_POINT ( 'NONE',  ( -0.6823417656249969321, 5.780208333674756283, -1.181850606188749264 ) ) ;
#59388 = CARTESIAN_POINT ( 'NONE',  ( 3.859774877264535053, -0.5717695562157121270, 1.876676618968641019 ) ) ;
#59389 = CARTESIAN_POINT ( 'NONE',  ( 1.511092056569414366, 2.013677475703846476, 0.1017375232199163593 ) ) ;
#59390 = ADVANCED_FACE ( 'NONE', ( #165190 ), #187278, .T. ) ;
#59391 = CARTESIAN_POINT ( 'NONE',  ( -3.975492009593180942, 7.849578277493553635, 0.1138384667214070584 ) ) ;
#59392 = CARTESIAN_POINT ( 'NONE',  ( 7.523999700038789484, -5.166862915010145052, 8.024744567526242989 ) ) ;
#59393 = CARTESIAN_POINT ( 'NONE',  ( 0.8076147168173102298, -1.862120749842037570, 0.1771838942275505424 ) ) ;
#59394 = CARTESIAN_POINT ( 'NONE',  ( -0.6823417656250212460, 4.301041667008085767, 1.181850606188767472 ) ) ;
#59395 = CARTESIAN_POINT ( 'NONE',  ( 3.287361135653954491, 0.04523670859641867187, -2.012844072734306433 ) ) ;
#59397 = CARTESIAN_POINT ( 'NONE',  ( 3.831750911750389399, 0.7112487137725398423, -1.994330698664834589 ) ) ;
#59396 = CARTESIAN_POINT ( 'NONE',  ( -5.748293942514172805, 8.689798118699771479, -1.082531754730538864 ) ) ;
#59398 = DIRECTION ( 'NONE',  ( 0.000000000000000000, 0.000000000000000000, 1.000000000000000000 ) ) ;
#59399 = CARTESIAN_POINT ( 'NONE',  ( 5.406714943436663035, 0.5975561702324573288, 1.982271326387271770 ) ) ;
#59400 = CARTESIAN_POINT ( 'NONE',  ( 8.018721507839716267, 8.319872945426633137, -0.7998128361456341429 ) ) ;
#59402 = CARTESIAN_POINT ( 'NONE',  ( 3.083589872104280705, 5.684939719841914929, 1.199719254218450271 ) ) ;
#59401 = CARTESIAN_POINT ( 'NONE',  ( 0.1344724916707736029, 0.3614680779570299540, 2.059103226732065028 ) ) ;
#59404 = EDGE_LOOP ( 'NONE', ( #2649, #18087, #42529, #37923 ) ) ;
#59403 = CARTESIAN_POINT ( 'NONE',  ( 5.157177646623883227, -1.542991646335686973, -0.9753701268572569916 ) ) ;
#59405 = CARTESIAN_POINT ( 'NONE',  ( 7.404724451357931336, 11.79059562655963056, 0.7998128361456462443 ) ) ;
#59406 = CARTESIAN_POINT ( 'NONE',  ( 2.065088895208815334, 8.523968132013772347, -2.459875961809442124 ) ) ;
#59407 = CARTESIAN_POINT ( 'NONE',  ( 9.692997807120237397, 13.38204337665774624, -8.150562841249751500 ) ) ;
#59408 = CARTESIAN_POINT ( 'NONE',  ( -10.68898853036274055, 3.992937990999307907, 4.901699750972148273 ) ) ;
#59409 = CARTESIAN_POINT ( 'NONE',  ( 1.364683531250000748, 12.06770833367473195, -0.7879004041258355073 ) ) ;
#59410 = CARTESIAN_POINT ( 'NONE',  ( 6.445967652843097362, -1.252902786447611883, -1.444740716957277904 ) ) ;
#59411 = CARTESIAN_POINT ( 'NONE',  ( -7.309817376062285099, 11.67987070538135264, 0.000000000000000000 ) ) ;
#59412 = CARTESIAN_POINT ( 'NONE',  ( 6.440286661691305703, 7.472421512516709718, 1.199719254218462483 ) ) ;
#59413 = AXIS2_PLACEMENT_3D ( 'NONE', #96492, #15184, #81274 ) ;
#59414 = CARTESIAN_POINT ( 'NONE',  ( -11.88156762547253997, 11.37999991545968115, -1.686557021358706221 ) ) ;
#59415 = CARTESIAN_POINT ( 'NONE',  ( 5.002595493318194642, 4.938708951733754127, -0.7216878364870197293 ) ) ;
#59416 = DIRECTION ( 'NONE',  ( -0.5620411653108187133, 0.8271092603133257670, -5.421010862427498504E-15 ) ) ;
#59417 = CARTESIAN_POINT ( 'NONE',  ( 4.416205349749311004, 6.175325546172740765, 1.599625672291267398 ) ) ;
#59418 = ORIENTED_EDGE ( 'NONE', *, *, #4565, .T. ) ;
#59419 = CARTESIAN_POINT ( 'NONE',  ( -7.045397100956844127, 8.248660034984974132, -1.199719254218452047 ) ) ;
#59421 = CARTESIAN_POINT ( 'NONE',  ( 6.475954649182838807, 7.584310507915338562, 1.199719254218452047 ) ) ;
#59420 = CARTESIAN_POINT ( 'NONE',  ( 0.07995206772519822258, -9.200995477224008567, -9.499751636909056884 ) ) ;
#59422 = DIRECTION ( 'NONE',  ( 0.000000000000000000, -1.000000000000000000, 0.000000000000000000 ) ) ;
#59423 = CARTESIAN_POINT ( 'NONE',  ( -0.1405533004718495238, 2.888985375434447889, -2.209311699518405447 ) ) ;
#59424 = CARTESIAN_POINT ( 'NONE',  ( -6.399085315970151733, 7.528316292462387871, -1.082531754730544860 ) ) ;
#59425 = CARTESIAN_POINT ( 'NONE',  ( 2.523789150438203510, 6.096171108819874007, 0.7998128361456462443 ) ) ;
#59426 = CARTESIAN_POINT ( 'NONE',  ( 2.026157484158600752, 1.007934145216189625, 1.691802187876802810 ) ) ;
#59427 = CARTESIAN_POINT ( 'NONE',  ( 3.234000073275579812, 2.016598147164900823, -0.002828922958116042007 ) ) ;
#59428 = CARTESIAN_POINT ( 'NONE',  ( -8.030507057996002729, 8.263346410617135263, 1.040834085586084257E-14 ) ) ;
#59430 = EDGE_CURVE ( 'NONE', #123166, #193490, #76423, .T. ) ;
#59429 = CARTESIAN_POINT ( 'NONE',  ( 6.727182134110222478, 4.688348259194305534, 2.751590707055273199 ) ) ;
#59431 = CARTESIAN_POINT ( 'NONE',  ( 3.627062487484993714, -2.024900418628313936, 0.8384617360315260726 ) ) ;
#59432 = CARTESIAN_POINT ( 'NONE',  ( 4.509216530447271332, 8.500000000000010658, -0.05037230876976211968 ) ) ;
#59433 = CARTESIAN_POINT ( 'NONE',  ( 1.922754896507544720, 1.796626380246616028, 0.6955005520668521291 ) ) ;
#59434 = CARTESIAN_POINT ( 'NONE',  ( -8.134002093194872884, 11.57708731111429401, 1.199719254218453823 ) ) ;
#59435 = CARTESIAN_POINT ( 'NONE',  ( 1.451998047843343409, 7.315968950353815892, -4.301760722578415574 ) ) ;
#59436 = CARTESIAN_POINT ( 'NONE',  ( 0.2331563151865486683, 0.2490001740663889407, -1.980811336351681273 ) ) ;
#59437 = EDGE_CURVE ( 'NONE', #24390, #70986, #206597, .T. ) ;
#59438 = CARTESIAN_POINT ( 'NONE',  ( 6.421758314367153275, 10.64380180007036891, -0.7998128361456291469 ) ) ;
#59439 = CARTESIAN_POINT ( 'NONE',  ( 5.229694566569264680, 7.124396299129368337, 1.599625672291267398 ) ) ;
#59440 = CARTESIAN_POINT ( 'NONE',  ( -6.808607288253732293, -8.010031549403114681, 6.625366561259686371 ) ) ;
#59441 = CARTESIAN_POINT ( 'NONE',  ( 4.421367491832258523, 8.172362817197399210, 0.7216878364870257245 ) ) ;
#59442 = EDGE_LOOP ( 'NONE', ( #112457, #105785, #62102, #71886 ) ) ;
#59444 = CARTESIAN_POINT ( 'NONE',  ( 2.666654630192913267, 0.6802043231916419241, 1.894807776549158218 ) ) ;
#59443 = CARTESIAN_POINT ( 'NONE',  ( 5.530750200611445067, -1.661959182355336795, 0.7928504710919548337 ) ) ;
#59445 = CARTESIAN_POINT ( 'NONE',  ( 4.253462032731039066, -2.272626950162641268, -0.3425954598320450906 ) ) ;
#59447 = CARTESIAN_POINT ( 'NONE',  ( 3.555356577358064207, 1.464247429212956808, 1.148356018212342233 ) ) ;
#59446 = CARTESIAN_POINT ( 'NONE',  ( -0.1291982275798807533, 5.720674304969967316, -2.668085245563474484 ) ) ;
#59448 = FACE_OUTER_BOUND ( 'NONE', #127417, .T. ) ;
#59450 = EDGE_CURVE ( 'NONE', #185927, #82118, #83532, .T. ) ;
#59449 = FACE_OUTER_BOUND ( 'NONE', #75379, .T. ) ;
#59451 = CARTESIAN_POINT ( 'NONE',  ( 6.398695753475230674, -1.876852914212179035, -0.3660984893600614520 ) ) ;
#59452 = CARTESIAN_POINT ( 'NONE',  ( -6.561256274009600986, 9.742217188731485678, -1.199719254218440723 ) ) ;
#59453 = CARTESIAN_POINT ( 'NONE',  ( -5.072158865288277418, 7.010880990960010273, 1.443375672974058777 ) ) ;
#59454 = CARTESIAN_POINT ( 'NONE',  ( 5.882390464068013358, -0.3075192527470702042, -2.067890480286633803 ) ) ;
#59455 = CARTESIAN_POINT ( 'NONE',  ( 6.982085921357777281, 7.248114451113292667, 1.040834085586084257E-14 ) ) ;
#59456 = CARTESIAN_POINT ( 'NONE',  ( 2.977454500823585093, 6.499579965040511276, -0.5808385047149626779 ) ) ;
#59457 = CARTESIAN_POINT ( 'NONE',  ( -11.86145016429273191, 13.40000000000000036, -1.180000000000002158 ) ) ;
#59458 = CARTESIAN_POINT ( 'NONE',  ( 5.918504666124354330, 1.153338095414379261, -1.282764499605532738 ) ) ;
#59459 = CARTESIAN_POINT ( 'NONE',  ( -3.913499895838973508, 7.717500311787445000, 1.040834085586084257E-14 ) ) ;
#59460 = CARTESIAN_POINT ( 'NONE',  ( 1.687715598229572844, 1.441817134274174794, 0.9631580532376384784 ) ) ;
#59461 = DIRECTION ( 'NONE',  ( 0.000000000000000000, 0.000000000000000000, 1.000000000000000000 ) ) ;
#59462 = DIRECTION ( 'NONE',  ( -0.6507913734559688246, -0.7592566023652963514, 0.000000000000000000 ) ) ;
#59463 = LINE ( 'NONE', #211025, #141697 ) ;
#59464 = CARTESIAN_POINT ( 'NONE',  ( 5.998927374810688384, 0.4157333352466702769, 2.130747042934706403 ) ) ;
#59465 = CARTESIAN_POINT ( 'NONE',  ( 4.019992336727182369, -0.9402185374879183932, -1.564826772493657536 ) ) ;
#59466 = CARTESIAN_POINT ( 'NONE',  ( 2.412880707699780025, -1.519673801815585312, 1.240645658979570909 ) ) ;
#59467 = CARTESIAN_POINT ( 'NONE',  ( 9.333041836227126353, 3.553052365627043407, 7.472413793103448221 ) ) ;
#59468 = CARTESIAN_POINT ( 'NONE',  ( -1.499999999999997780, 5.650000000000023448, 1.214306433183764966E-14 ) ) ;
#59469 = CARTESIAN_POINT ( 'NONE',  ( 6.577677080924314801, 10.82570702772039262, 1.040834085586084257E-14 ) ) ;
#59470 = CARTESIAN_POINT ( 'NONE',  ( 2.192179715818479036, 1.306768369893403170, 1.669877806752372740 ) ) ;
#59471 = CARTESIAN_POINT ( 'NONE',  ( -3.145128448690323264, 4.692402494937224056, -1.443375672974059665 ) ) ;
#59472 = FILL_AREA_STYLE ('',( #58416 ) ) ;
#59473 = EDGE_CURVE ( 'NONE', #133087, #160120, #16784, .T. ) ;
#59474 = CARTESIAN_POINT ( 'NONE',  ( -5.609265928939476176, 6.186647267178685183, -0.8691123025580966832 ) ) ;
#59475 = CARTESIAN_POINT ( 'NONE',  ( 0.5673436759025469733, 1.799520464221905369, 1.023488823764052480 ) ) ;
#59477 = CARTESIAN_POINT ( 'NONE',  ( -6.009258394948636914E-15, 13.46875000068279604, -1.732050807568875195 ) ) ;
#59476 = CARTESIAN_POINT ( 'NONE',  ( -10.14265820453532818, 3.662953273883144512, 6.345113228764306612 ) ) ;
#59479 = VERTEX_POINT ( 'NONE', #50377 ) ;
#59478 = CARTESIAN_POINT ( 'NONE',  ( 3.475417139410865275, -1.959577385150832907, -1.046020024706290297 ) ) ;
#59480 = CARTESIAN_POINT ( 'NONE',  ( 0.4582085974003520801, -2.167260061518965664, -0.7665384626166712456 ) ) ;
#59482 = CARTESIAN_POINT ( 'NONE',  ( 6.877782380132525297, -2.002170498271789167, 0.4952429967341723804 ) ) ;
#59481 = CARTESIAN_POINT ( 'NONE',  ( 8.568389894156670294, 12.94027927658408217, -0.7216878364870257245 ) ) ;
#59484 = CARTESIAN_POINT ( 'NONE',  ( 1.737500000000001155, -0.5833333333333314830, 3.009438278150922130 ) ) ;
#59483 = CARTESIAN_POINT ( 'NONE',  ( 4.903208829997618423, 5.749440385532527564, -1.199719254218450271 ) ) ;
#59485 = LINE ( 'NONE', #155934, #44080 ) ;
#59486 = CARTESIAN_POINT ( 'NONE',  ( -10.91970695577496997, -5.907420853759282053, 5.204170427930421283E-15 ) ) ;
#59487 = CARTESIAN_POINT ( 'NONE',  ( -0.2102771530458094895, 2.860119660625429550, -2.691685224125789588 ) ) ;
#59488 = CARTESIAN_POINT ( 'NONE',  ( 2.520142033498268486, 1.128878695625197492, -1.304093658461308980 ) ) ;
#59489 = CARTESIAN_POINT ( 'NONE',  ( 0.7785302072789467287, -0.4946362931835950327, -1.954778448132548752 ) ) ;
#59490 = CARTESIAN_POINT ( 'NONE',  ( 3.235276958591898566, 2.298851035330526038, -0.002058992973525546142 ) ) ;
#59491 = CARTESIAN_POINT ( 'NONE',  ( 2.987861924072153563, 1.597690390425403173, 1.602079265715735223 ) ) ;
#59492 = CARTESIAN_POINT ( 'NONE',  ( 5.303390785913836503, 1.721067984382893545, 1.213575365270858075 ) ) ;
#59493 = CARTESIAN_POINT ( 'NONE',  ( -5.587368702607575344, 8.572328348800551723, 1.082531754730550855 ) ) ;
#59494 = CARTESIAN_POINT ( 'NONE',  ( 4.112378888775404917, 1.252788995219549895, -1.250258383314418520 ) ) ;
#59496 = CARTESIAN_POINT ( 'NONE',  ( 6.480031627576305020, -2.247188937338239434, -0.4521185302251101157 ) ) ;
#59495 = CARTESIAN_POINT ( 'NONE',  ( 4.380693030546916944, 6.204170850428461392, 1.443375672974058777 ) ) ;
#59497 = CARTESIAN_POINT ( 'NONE',  ( 5.120983416928425846, -1.747193932927636029, 0.5808180576658967809 ) ) ;
#59498 = CARTESIAN_POINT ( 'NONE',  ( -5.382750679825375251, 6.238629533673094585, -1.199719254218446718 ) ) ;
#59499 = CARTESIAN_POINT ( 'NONE',  ( 5.965224399888476192, 6.061776009399090448, 1.040834085586084257E-14 ) ) ;
#59500 = CARTESIAN_POINT ( 'NONE',  ( 1.499999999999987121, 3.545833333333356041, -0.8660254037844262731 ) ) ;
#59501 = CARTESIAN_POINT ( 'NONE',  ( 4.804715953495782621, 1.905792977913090214, 1.081705336968781239 ) ) ;
#59502 = FACE_OUTER_BOUND ( 'NONE', #11025, .T. ) ;
#59503 = DIRECTION ( 'NONE',  ( -0.000000000000000000, -1.000000000000000000, -0.000000000000000000 ) ) ;
#59504 = CARTESIAN_POINT ( 'NONE',  ( 5.758279222819879806, -2.070544812512797428, -0.003756845764937844813 ) ) ;
#59505 = CARTESIAN_POINT ( 'NONE',  ( -0.08279552664090458758, -1.841734517378278424, 0.8216794407479923734 ) ) ;
#59506 = CARTESIAN_POINT ( 'NONE',  ( -0.6823417656250212460, 4.301041667008085767, 1.181850606188767472 ) ) ;
#59507 = CARTESIAN_POINT ( 'NONE',  ( 3.457566480858861091, 0.4672022665876771619, -1.868877010067309330 ) ) ;
#59508 = CARTESIAN_POINT ( 'NONE',  ( 1.364683531249997417, 10.23437500034139802, 2.602085213965210642E-15 ) ) ;
#59509 = CARTESIAN_POINT ( 'NONE',  ( -4.473827502829599290, 4.321812962830357208, 0.7216878364870317197 ) ) ;
#59510 = CARTESIAN_POINT ( 'NONE',  ( -0.2102771530458277249, -0.008943344768331040057, -2.203482896658352175 ) ) ;
#59511 = EDGE_LOOP ( 'NONE', ( #17340, #139094, #212369, #50372 ) ) ;
#59513 = LINE ( 'NONE', #191632, #94901 ) ;
#59512 = CARTESIAN_POINT ( 'NONE',  ( 1.499999999999990896, 8.627523663848661428, -2.579999999999989413 ) ) ;
#59514 = CARTESIAN_POINT ( 'NONE',  ( 5.352771719296971042, 5.139321848801576387, 0.7998128361456341429 ) ) ;
#59515 = CARTESIAN_POINT ( 'NONE',  ( 2.969872605471108873, 6.605953636083950364, -2.420000000000002149 ) ) ;
#59516 = CARTESIAN_POINT ( 'NONE',  ( -5.181758602633715682, 4.945385036406048762, 2.419999999999998597 ) ) ;
#59517 = CARTESIAN_POINT ( 'NONE',  ( 1.284279953904121641, 3.034610286488902187, 0.7750000000000117906 ) ) ;
#59518 = CARTESIAN_POINT ( 'NONE',  ( 8.229436053370658755, 12.54483312900040026, 0.7216878364870438212 ) ) ;
#59519 = CARTESIAN_POINT ( 'NONE',  ( 0.7484013653801385724, -1.946605496936428370, -0.2438083268051088881 ) ) ;
#59520 = CARTESIAN_POINT ( 'NONE',  ( -0.6823417656250212460, 1.363541667008083547, 1.181850606188755259 ) ) ;
#59521 = CARTESIAN_POINT ( 'NONE',  ( 0.7499999999999902300, 3.733333333333352488, 1.299038105676669330 ) ) ;
#59522 = CARTESIAN_POINT ( 'NONE',  ( 5.125427350195786325, 0.1941421753944693185, -1.952251141935714696 ) ) ;
#59523 = CARTESIAN_POINT ( 'NONE',  ( -9.169391961543940539, 9.592045464756413509, 1.040834085586084257E-14 ) ) ;
#59524 = CARTESIAN_POINT ( 'NONE',  ( -5.761852095683518193, 6.784877535461274256, 1.082531754730546636 ) ) ;
#59525 = CARTESIAN_POINT ( 'NONE',  ( 6.403215362905616992, 1.794359850238020693, 1.205212418099836480 ) ) ;
#59527 = ORIENTED_EDGE ( 'NONE', *, *, #90996, .F. ) ;
#59526 = CARTESIAN_POINT ( 'NONE',  ( 0.04341786867403699124, -5.575210796978269379, -11.00023563321887643 ) ) ;
#59528 = CARTESIAN_POINT ( 'NONE',  ( -1.364683531250010295, 5.280208333674758059, 0.7879004041258379498 ) ) ;
#59529 = CARTESIAN_POINT ( 'NONE',  ( 6.731714608790520415, -1.285842040959904287, -1.494388255172361513 ) ) ;
#59530 = CARTESIAN_POINT ( 'NONE',  ( 6.011065113327825671, 1.732079373560748481, 0.08140909068810914251 ) ) ;
#59532 = CARTESIAN_POINT ( 'NONE',  ( 2.771223791512751333, 2.080116120148074010, -0.6901165687889164735 ) ) ;
#59531 = CARTESIAN_POINT ( 'NONE',  ( 1.360316468749949825, 0.2447916670081152490, 0.7853790794158741484 ) ) ;
#59533 = CARTESIAN_POINT ( 'NONE',  ( 4.173124822893734986, -2.151704308474690741, -0.8341741560445140591 ) ) ;
#59534 = CARTESIAN_POINT ( 'NONE',  ( 5.712203248095857333, -0.9225367590200548307, -1.842806303608224949 ) ) ;
#59535 = CARTESIAN_POINT ( 'NONE',  ( 1.868985280173897756, 1.858391233338702042, -0.5634987755925959796 ) ) ;
#59536 = CARTESIAN_POINT ( 'NONE',  ( -5.721177634842498527, 5.777054783512106440, 0.000000000000000000 ) ) ;
#59537 = CARTESIAN_POINT ( 'NONE',  ( 0.000000000000000000, 0.000000000000000000, 0.000000000000000000 ) ) ;
#59538 = CARTESIAN_POINT ( 'NONE',  ( 5.133110336712339183, 1.960249873928998410, 0.8093987030339530042 ) ) ;
#59539 = FILL_AREA_STYLE_COLOUR ( '', #143530 ) ;
#59540 = CARTESIAN_POINT ( 'NONE',  ( 3.358046224211252095, 0.04667712216412447934, -2.016033814150198999 ) ) ;
#59541 = CARTESIAN_POINT ( 'NONE',  ( -5.599154252319524794, 6.595063384869953360, 1.082531754730546636 ) ) ;
#59542 = EDGE_CURVE ( 'NONE', #61441, #30537, #113447, .T. ) ;
#59543 = CARTESIAN_POINT ( 'NONE',  ( -6.071018923869249129, 10.30488218781460574, 0.7998128361456291469 ) ) ;
#59545 =( BOUNDED_SURFACE ( )  B_SPLINE_SURFACE ( 3, 2, ( 
 ( #209538, #127340, #15605 ),
 ( #129475, #32948, #146730 ),
 ( #94772, #212748, #64382 ),
 ( #130527, #213792, #196518 ),
 ( #31894, #114273, #47086 ),
 ( #131564, #180270, #111064 ),
 ( #197565, #62250, #115329 ),
 ( #181320, #99022, #193310 ),
 ( #177070, #28686, #112140 ),
 ( #160820, #12412, #78492 ),
 ( #144609, #210624, #128411 ),
 ( #194378, #29758, #95843 ),
 ( #133682, #135787, #38277 ),
 ( #149906, #152035, #148827 ),
 ( #34002, #153095, #100076 ),
 ( #83813, #116384, #68614 ),
 ( #132612, #3606, #85960 ),
 ( #87023, #170399, #136856 ) ),
 .UNSPECIFIED., .F., .F., .F. ) 
 B_SPLINE_SURFACE_WITH_KNOTS ( ( 4, 2, 2, 2, 2, 2, 2, 2, 4 ),
 ( 3, 3 ),
 ( 0.000000000000000000, 8.835779872240032032E-05, 0.0001767155974448006406, 0.0003534311948896012813, 0.0007068623897792025625, 0.001060293584668803735, 0.001237009182113604430, 0.001325366980836004778, 0.001413724779558405125 ),
 ( 0.000000000000000000, 1.000000000000000000 ),
 .UNSPECIFIED. ) 
 GEOMETRIC_REPRESENTATION_ITEM ( )  RATIONAL_B_SPLINE_SURFACE ( (
 ( 1.000000000000000000, 0.8509629433930272491, 1.000000000000000000),
 ( 1.000000000000000000, 0.8498006689636994349, 1.000000000000000000),
 ( 1.000000000000000000, 0.8320552335758597540, 1.000000000000000000),
 ( 1.000000000000000000, 0.8099185496503389370, 1.000000000000000000),
 ( 1.000000000000000000, 0.8026556248207100674, 1.000000000000000000),
 ( 1.000000000000000000, 0.7864057361306107108, 1.000000000000000000),
 ( 1.000000000000000000, 0.7820376696873353461, 1.000000000000000000),
 ( 1.000000000000000000, 0.7712304172370865185, 1.000000000000000000),
 ( 1.000000000000000000, 0.7693781127550674004, 1.000000000000000000),
 ( 1.000000000000000000, 0.7693828318334674510, 1.000000000000000000),
 ( 1.000000000000000000, 0.7713025106554596277, 1.000000000000000000),
 ( 1.000000000000000000, 0.7820120509638822659, 1.000000000000000000),
 ( 1.000000000000000000, 0.7865355379946432635, 1.000000000000000000),
 ( 1.000000000000000000, 0.8025478250466264729, 1.000000000000000000),
 ( 1.000000000000000000, 0.8098425558904723820, 1.000000000000000000),
 ( 1.000000000000000000, 0.8320142513982312638, 1.000000000000000000),
 ( 1.000000000000000000, 0.8496692043554369134, 1.000000000000000000),
 ( 1.000000000000000000, 0.8509629433917196284, 1.000000000000000000) ) ) 
 REPRESENTATION_ITEM ( '' )  SURFACE ( )  );
#59544 = CARTESIAN_POINT ( 'NONE',  ( 9.856941372335116469, 11.45851867493453291, 1.199719254218450271 ) ) ;
#59546 = CARTESIAN_POINT ( 'NONE',  ( 0.4162703231485806454, 1.261427835099769634, -1.320066674804179385 ) ) ;
#59547 = CARTESIAN_POINT ( 'NONE',  ( -7.273023059088104425, 7.449891421883056530, 0.000000000000000000 ) ) ;
#59548 = CARTESIAN_POINT ( 'NONE',  ( -5.764151584465413869, 6.753873599078290546, -1.199719254218453823 ) ) ;
#59549 = CARTESIAN_POINT ( 'NONE',  ( -5.698737662929126202, 7.345098442806643924, 1.271001439489399809 ) ) ;
#59550 = VERTEX_POINT ( 'NONE', #38387 ) ;
#59551 = CARTESIAN_POINT ( 'NONE',  ( 5.454002199308585652, 2.058645617578058751, -0.09870700237277732492 ) ) ;
#59552 = CARTESIAN_POINT ( 'NONE',  ( -7.390603132780795725, 8.755363422066633206, -1.082531754730549967 ) ) ;
#59553 = CARTESIAN_POINT ( 'NONE',  ( 7.471952054462754234, 8.850270497362297206, 1.082531754730549078 ) ) ;
#59554 = CARTESIAN_POINT ( 'NONE',  ( -4.172158584703340445, 5.890604320285754980, -1.599625672291256295 ) ) ;
#59555 = FACE_OUTER_BOUND ( 'NONE', #61720, .T. ) ;
#59556 = CARTESIAN_POINT ( 'NONE',  ( 4.969401683643670076, -1.707372507963246022, -1.078548144515010909 ) ) ;
#59558 = ORIENTED_EDGE ( 'NONE', *, *, #176737, .T. ) ;
#59557 = CARTESIAN_POINT ( 'NONE',  ( 1.499999999999987121, 1.504166666666690411, 0.8660254037844524744 ) ) ;
#59560 = CARTESIAN_POINT ( 'NONE',  ( 9.571693261567961741, 11.22969222899322617, 1.082531754730548412 ) ) ;
#59559 = CARTESIAN_POINT ( 'NONE',  ( -4.522526758610270647, 7.433975764090723359, -1.199719254218453823 ) ) ;
#59561 = CARTESIAN_POINT ( 'NONE',  ( 5.982172092127724383, 8.002286745614243912, -1.599625672291262513 ) ) ;
#59562 = CARTESIAN_POINT ( 'NONE',  ( 4.539950165727339559, 0.8829098278404916567, -1.862335138179547211 ) ) ;
#59563 = CARTESIAN_POINT ( 'NONE',  ( 3.076796235938106694, -0.8146265060355702969, 1.844709937164575875 ) ) ;
#59564 = ORIENTED_EDGE ( 'NONE', *, *, #6657, .F. ) ;
#59565 = DIRECTION ( 'NONE',  ( 1.000000000000000000, 0.000000000000000000, 0.000000000000000000 ) ) ;
#59566 = CARTESIAN_POINT ( 'NONE',  ( 4.436542580169809291, 6.199052314996659874, 1.599625672291267398 ) ) ;
#59567 = CARTESIAN_POINT ( 'NONE',  ( 3.257046257486408969, 0.04465439498414420366, -2.016188763087948033 ) ) ;
#59568 = VECTOR ( 'NONE', #206828, 1000.000000000000000 ) ;
#59570 = VERTEX_POINT ( 'NONE', #187827 ) ;
#59569 = CARTESIAN_POINT ( 'NONE',  ( 0.004619473214107315887, 7.151453204069587066, -1.999995854215781410 ) ) ;
#59571 = CARTESIAN_POINT ( 'NONE',  ( 3.339220083777879378, -1.203169880011810022, 1.617570133648409847 ) ) ;
#59572 = CARTESIAN_POINT ( 'NONE',  ( 2.132514540308296791, -1.644867172388216003, 0.8273176719292076875 ) ) ;
#59573 = AXIS2_PLACEMENT_3D ( 'NONE', #8995, #141183, #128182 ) ;
#59574 = CARTESIAN_POINT ( 'NONE',  ( 1.419075709855713630, 1.546787523640520856, -1.712735560227249820 ) ) ;
#59575 = CARTESIAN_POINT ( 'NONE',  ( 5.682802662783380754, 6.658966523782627434, 1.199719254218452935 ) ) ;
#59576 = CARTESIAN_POINT ( 'NONE',  ( 3.356853517036356038, -1.639235867460669072, 1.409173823127254366 ) ) ;
#59577 = CARTESIAN_POINT ( 'NONE',  ( 9.610031953988080744, 10.10612545594124967, -0.7998128361456281477 ) ) ;
#59578 = CARTESIAN_POINT ( 'NONE',  ( -6.575868197828002693, 7.630599971342813426, 1.199719254218450271 ) ) ;
#59579 = EDGE_CURVE ( 'NONE', #58812, #80737, #38571, .T. ) ;
#59580 = CARTESIAN_POINT ( 'NONE',  ( 3.093437905492165907, 1.279035344561373355, -1.909460003155829311 ) ) ;
#59581 = ORIENTED_EDGE ( 'NONE', *, *, #134736, .T. ) ;
#59582 = FACE_OUTER_BOUND ( 'NONE', #191759, .T. ) ;
#59583 = CARTESIAN_POINT ( 'NONE',  ( 1.217418975555501826, -1.825842229346545498, 0.4062821374252246764 ) ) ;
#59584 = CARTESIAN_POINT ( 'NONE',  ( 5.559438140644474835, 0.3852295531507047843, -1.933300702130675397 ) ) ;
#59586 = CARTESIAN_POINT ( 'NONE',  ( 7.904040366642684390, 11.20483561351640844, 1.082531754730558626 ) ) ;
#59585 = CARTESIAN_POINT ( 'NONE',  ( -1.364683531249997417, 4.759375000341424133, 1.214306433183764966E-14 ) ) ;
#59588 = CARTESIAN_POINT ( 'NONE',  ( 0.8564375766340023288, 2.204168734417511821, -0.1118928034387969561 ) ) ;
#59587 = CARTESIAN_POINT ( 'NONE',  ( -6.033542053281340856, 6.997886136038390603, -1.199719254218446718 ) ) ;
#59589 = CARTESIAN_POINT ( 'NONE',  ( 10.38819714233658686, 3.487142912321096855, -5.997628416523089534 ) ) ;
#59590 = CARTESIAN_POINT ( 'NONE',  ( 4.873266149108180123, 7.772895376346490970, 1.199719254218462483 ) ) ;
#59591 = CARTESIAN_POINT ( 'NONE',  ( -6.410307701162927252, 6.373113827645189744, -0.7998128361456291469 ) ) ;
#59592 = CARTESIAN_POINT ( 'NONE',  ( 6.539320575229292665, 2.014857154840712372, 2.506613887083661840 ) ) ;
#59593 = CARTESIAN_POINT ( 'NONE',  ( 5.330923369760363961, 0.1444485787395009269, 1.966219458991929514 ) ) ;
#59594 = CARTESIAN_POINT ( 'NONE',  ( 5.127664261384059508, -2.192653808335935928, 0.7197182627937804833 ) ) ;
#59595 = CARTESIAN_POINT ( 'NONE',  ( 6.092234697878679661, 0.9164522128973868753, -1.619700000576968391 ) ) ;
#59596 = CARTESIAN_POINT ( 'NONE',  ( 3.502832280938583676, 0.4964207669093263497, 2.001847840641638232 ) ) ;
#59597 = CARTESIAN_POINT ( 'NONE',  ( 7.470179451449751262, 7.817556902887268677, 1.040834085586084257E-14 ) ) ;
#59598 = EDGE_CURVE ( 'NONE', #144530, #12134, #31763, .T. ) ;
#59599 = CARTESIAN_POINT ( 'NONE',  ( 4.692003678781083487, 7.631698837623355658, -1.199719254218450271 ) ) ;
#59600 = CARTESIAN_POINT ( 'NONE',  ( 3.562760505341037831, 7.378580699531681830, -1.734723475976807094E-15 ) ) ;
#59601 = CARTESIAN_POINT ( 'NONE',  ( 0.6823417656249899377, 1.405208333674752508, 1.181850606188755259 ) ) ;
#59602 = CARTESIAN_POINT ( 'NONE',  ( -4.288887917185465248, 14.55258240538958425, 11.16905078721341837 ) ) ;
#59603 = CARTESIAN_POINT ( 'NONE',  ( 6.941411460072420603, 7.200660912947041581, 1.040834085586084257E-14 ) ) ;
#59605 = CARTESIAN_POINT ( 'NONE',  ( 3.046111529846948329, 0.9110102549910354952, 1.799122713138465279 ) ) ;
#59604 = CARTESIAN_POINT ( 'NONE',  ( 5.600102540861260358, 0.8850759393619503923, -1.982774263332246489 ) ) ;
#59606 = CARTESIAN_POINT ( 'NONE',  ( 0.4254946254913888892, 3.044090126848115307, -0.4192457809237770117 ) ) ;
#59608 = CARTESIAN_POINT ( 'NONE',  ( 4.124425300631988200, 0.09459923933386081563, 1.838956108544815171 ) ) ;
#59607 = CARTESIAN_POINT ( 'NONE',  ( -3.551873057100300990, 5.166937871415542283, 1.443375672974064550 ) ) ;
#59610 = CARTESIAN_POINT ( 'NONE',  ( 6.620655732516613767, 2.976578140159558128, 2.379908536877679559 ) ) ;
#59609 = CARTESIAN_POINT ( 'NONE',  ( -1.364683531249997417, 5.759375000341418804, 1.214306433183764966E-14 ) ) ;
#59611 = CARTESIAN_POINT ( 'NONE',  ( 6.146043800834426918, 0.6857851511376764631, 2.081541312870714311 ) ) ;
#59612 = CARTESIAN_POINT ( 'NONE',  ( 0.1247927721447598948, 7.629137130509083597, -2.455404827119290978 ) ) ;
#59613 = CARTESIAN_POINT ( 'NONE',  ( 0.5622849326936694148, 2.237558834470813274, -0.3334926475991057959 ) ) ;
#59614 = CARTESIAN_POINT ( 'NONE',  ( -4.061770719603903679, 7.733366158448967909, -0.6361108440643822304 ) ) ;
#59615 = DIRECTION ( 'NONE',  ( -0.6507913734559658270, 0.7592566023652989049, 0.000000000000000000 ) ) ;
#59616 = CARTESIAN_POINT ( 'NONE',  ( 6.598740849494261873, 6.770918179921630475, -0.1579934589533253664 ) ) ;
#59617 = AXIS2_PLACEMENT_3D ( 'NONE', #76459, #123187, #189148 ) ;
#59618 = CARTESIAN_POINT ( 'NONE',  ( -3.472296738431328134, 7.065113604896248845, 0.000000000000000000 ) ) ;
#59619 = CARTESIAN_POINT ( 'NONE',  ( -3.128512303076027123, 6.140441835863033049, 0.8630319677947241308 ) ) ;
#59620 = CARTESIAN_POINT ( 'NONE',  ( 0.7074158718562081338, -1.761916611671160204, 0.1673130110368889201 ) ) ;
#59621 = CARTESIAN_POINT ( 'NONE',  ( 5.443998933236983362, -1.278728028966215957, -1.554778559382914871 ) ) ;
#59622 = CARTESIAN_POINT ( 'NONE',  ( 7.318703993278529829, 7.432909501780090800, 1.040834085586084257E-14 ) ) ;
#59623 = CARTESIAN_POINT ( 'NONE',  ( 4.172956468465331525, -1.964154803760146617, -0.7601757144085323770 ) ) ;
#59624 = CARTESIAN_POINT ( 'NONE',  ( 3.690956203553748427, 1.644769065816154008, 0.9816995294186120491 ) ) ;
#59625 = CARTESIAN_POINT ( 'NONE',  ( 4.545333244533083850, 1.760332640988309993, -0.8834868730601146414 ) ) ;
#59626 = CARTESIAN_POINT ( 'NONE',  ( 5.572523036771587890, 0.8223149429010238043, 1.845017218462653208 ) ) ;
#59627 = CARTESIAN_POINT ( 'NONE',  ( 1.955717210371358483, 1.865846021326333926, -0.1348392221205765851 ) ) ;
#59629 = CARTESIAN_POINT ( 'NONE',  ( 1.494246876672610025, -1.020364814108923213, 1.617233793950809906 ) ) ;
#59628 = CARTESIAN_POINT ( 'NONE',  ( 4.705503516419368815, -0.4560151319670002756, 1.663429522189649790 ) ) ;
#59631 = CARTESIAN_POINT ( 'NONE',  ( 3.958617665510264949, 5.641473247893851628, -1.443375672974051449 ) ) ;
#59630 = CARTESIAN_POINT ( 'NONE',  ( 2.262606014870732096, 0.9450075053254001212, 1.994452002680577429 ) ) ;
#59632 = CARTESIAN_POINT ( 'NONE',  ( -0.6823417656250212460, 2.613541667008084879, 1.181850606188767472 ) ) ;
#59633 = CARTESIAN_POINT ( 'NONE',  ( 6.619590441841329387, 0.3365870006281460047, -1.932621868259084330 ) ) ;
#59634 = CARTESIAN_POINT ( 'NONE',  ( 7.507464373665139412, 9.781794407407920389, 1.599625672291281386 ) ) ;
#59635 = CARTESIAN_POINT ( 'NONE',  ( -7.580882385731715800, -6.105993949506102858, 7.580882385731741557 ) ) ;
#59636 = CARTESIAN_POINT ( 'NONE',  ( 0.03866526371284223496, -9.261493551422342208, -9.500000000000152767 ) ) ;
#59637 = CARTESIAN_POINT ( 'NONE',  ( -4.741601036477307574, 6.554953847355395880, 1.599625672291267175 ) ) ;
#59638 = DIRECTION ( 'NONE',  ( 0.000000000000000000, 0.000000000000000000, -1.000000000000000000 ) ) ;
#59639 = AXIS2_PLACEMENT_3D ( 'NONE', #98850, #29579, #80456 ) ;
#59640 = EDGE_LOOP ( 'NONE', ( #203963, #35157, #96208 ) ) ;
#59641 = CARTESIAN_POINT ( 'NONE',  ( 2.225130849662222410, -1.891980959128433781, -0.8411517639917851508 ) ) ;
#59642 = CARTESIAN_POINT ( 'NONE',  ( -1.500000000000013101, 2.879166666666688634, -0.8660254037844313801 ) ) ;
#59643 = CARTESIAN_POINT ( 'NONE',  ( 4.625302960556422427, 8.547937220624488575, 1.040834085586084257E-14 ) ) ;
#59644 = CARTESIAN_POINT ( 'NONE',  ( -8.037286134802835491, 8.271255333558444889, -0.7998128361456291469 ) ) ;
#59645 = CARTESIAN_POINT ( 'NONE',  ( 2.891631901464575272, 6.595597328342462262, 0.000000000000000000 ) ) ;
#59646 = CARTESIAN_POINT ( 'NONE',  ( 0.08268334464456467137, -1.317614589208983444, 1.530782303595918714 ) ) ;
#59647 = FACE_OUTER_BOUND ( 'NONE', #78633, .T. ) ;
#59648 = CARTESIAN_POINT ( 'NONE',  ( -0.6823417656250003738, 1.967708333674753174, -1.181850606188749264 ) ) ;
#59650 = CARTESIAN_POINT ( 'NONE',  ( 4.532503425670185493, 4.182342172903648070, 1.214306433183764966E-14 ) ) ;
#59649 = CARTESIAN_POINT ( 'NONE',  ( 11.48243876534946217, 11.37999999999999901, -3.200000000000001510 ) ) ;
#59651 = CARTESIAN_POINT ( 'NONE',  ( 5.114611164699836010, 0.6351010243071940620, -1.913510948406547563 ) ) ;
#59652 = EDGE_CURVE ( 'NONE', #52415, #24930, #84973, .T. ) ;
#59653 = CARTESIAN_POINT ( 'NONE',  ( 4.487445792895001340, -0.5051273088985311910, 1.847880739403139572 ) ) ;
#59654 = SURFACE_STYLE_FILL_AREA ( #104153 ) ;
#59655 = CARTESIAN_POINT ( 'NONE',  ( 2.788834510562918645, 1.878274557074947948, -1.128960604485473862 ) ) ;
#59656 = DIRECTION ( 'NONE',  ( 0.000000000000000000, -1.000000000000000000, 0.000000000000000000 ) ) ;
#59657 = CARTESIAN_POINT ( 'NONE',  ( 1.499999999999987121, 0.5354166673494816786, 0.8660254037844524744 ) ) ;
#59658 = CARTESIAN_POINT ( 'NONE',  ( 5.484640381798278952, -1.273743769317101648, 1.559065439997550762 ) ) ;
#59659 = CARTESIAN_POINT ( 'NONE',  ( 1.494246876672610025, -1.020364814108923213, 1.617233793950809906 ) ) ;
#59660 = CARTESIAN_POINT ( 'NONE',  ( -4.232116505760120440, 8.089219690028791376, -0.7998128361456281477 ) ) ;
#59661 = CARTESIAN_POINT ( 'NONE',  ( 0.2808753465170962249, 1.674874268995883320, -1.122520385770640061 ) ) ;
#59662 = CARTESIAN_POINT ( 'NONE',  ( 1.364683531250000303, 9.817708333674735499, -0.7879004041258355073 ) ) ;
#59664 = CARTESIAN_POINT ( 'NONE',  ( -6.282224075085783177, 8.422623735723785643, 1.599625672291269396 ) ) ;
#59663 = CARTESIAN_POINT ( 'NONE',  ( 3.491813360781896858, -2.088456202509383797, -0.1002299605681444133 ) ) ;
#59666 = EDGE_LOOP ( 'NONE', ( #171321, #54544, #72722, #110004 ) ) ;
#59665 = CARTESIAN_POINT ( 'NONE',  ( 1.746655555778130253, -1.459509165399446529, 0.9187280511932097715 ) ) ;
#59667 = CARTESIAN_POINT ( 'NONE',  ( 5.555090253297246150, 7.504024600312024340, 1.599625672291267398 ) ) ;
#59668 = CIRCLE ( 'NONE', #128852, 0.5000000000000004441 ) ;
#59669 = CARTESIAN_POINT ( 'NONE',  ( 11.01135777277262306, 12.59375064782103948, 1.399999999999998357 ) ) ;
#59670 = CARTESIAN_POINT ( 'NONE',  ( 7.346809171966843799, -6.836568542494916301, 8.002408263929979171 ) ) ;
#59671 = CARTESIAN_POINT ( 'NONE',  ( 11.48767021851168124, 9.769957725361692269, -3.470194894594655910 ) ) ;
#59672 = CARTESIAN_POINT ( 'NONE',  ( 4.320244504248938355, 8.192035688265757898, 1.040834085586084257E-14 ) ) ;
#59673 = ORIENTED_EDGE ( 'NONE', *, *, #156259, .T. ) ;
#59674 = CARTESIAN_POINT ( 'NONE',  ( 1.266973501737285845, 3.918521279025124482, -0.4964169966120777766 ) ) ;
#59675 = CARTESIAN_POINT ( 'NONE',  ( 3.176200218816268350, 0.8167180202140277290, 1.616994655555709981 ) ) ;
#59676 = ORIENTED_EDGE ( 'NONE', *, *, #70880, .T. ) ;
#59677 = CARTESIAN_POINT ( 'NONE',  ( 4.216749469050096621, 4.878294787768598262, -1.199719254218452047 ) ) ;
#59678 = CARTESIAN_POINT ( 'NONE',  ( 5.734172623936983904, 5.654565914206774124, 0.7998128361456352531 ) ) ;
#59679 = CARTESIAN_POINT ( 'NONE',  ( 4.160681542540445754, 0.4872625442002316287, 1.744618836514327587 ) ) ;
#59680 = DIRECTION ( 'NONE',  ( -1.000000000000000000, 7.771561172376097755E-16, 4.440892098500627148E-16 ) ) ;
#59681 = CARTESIAN_POINT ( 'NONE',  ( -10.99574878476023976, -7.889012432655405860, 0.3098035853330368128 ) ) ;
#59682 = CARTESIAN_POINT ( 'NONE',  ( 5.580611138136594818, 6.171711880978127063, 0.8815597724760818599 ) ) ;
#59683 = CARTESIAN_POINT ( 'NONE',  ( 4.193699477585779434, -1.282400645549033547, -1.348940618851623974 ) ) ;
#59684 = CARTESIAN_POINT ( 'NONE',  ( 1.546349530022947727, -1.353405651413071453, 1.355934989043396044 ) ) ;
#59685 = CARTESIAN_POINT ( 'NONE',  ( 0.4811275135914867551, 1.705355465787803393, -0.6520327999673739550 ) ) ;
#59686 = DIRECTION ( 'NONE',  ( 0.000000000000000000, 1.000000000000000000, 0.000000000000000000 ) ) ;
#59687 = CARTESIAN_POINT ( 'NONE',  ( 4.789099507923308963, 8.141322699134850183, 0.8117711051834965996 ) ) ;
#59688 = CARTESIAN_POINT ( 'NONE',  ( -0.4019237886467001974, 8.551335450315372455, 1.500000000000001998 ) ) ;
#59689 = CARTESIAN_POINT ( 'NONE',  ( 0.07999999999999327094, -9.999999999999994671, 10.99970695577496294 ) ) ;
#59690 = CARTESIAN_POINT ( 'NONE',  ( 1.833030277982334422, 2.531131934864056632, -2.500000000000000444 ) ) ;
#59691 = CARTESIAN_POINT ( 'NONE',  ( 7.131225611108079399, 11.26358761302737754, 0.7216878364870438212 ) ) ;
#59692 = CARTESIAN_POINT ( 'NONE',  ( 5.998876245820001785, 0.3805640578184403822, 1.932138370648580628 ) ) ;
#59693 = CARTESIAN_POINT ( 'NONE',  ( -6.078132937628113908, 5.985576603521232109, 1.040834085586084257E-14 ) ) ;
#59694 = CARTESIAN_POINT ( 'NONE',  ( -3.824766175154623582, 7.348582304423016964, -0.7466790275774716212 ) ) ;
#59695 = ADVANCED_FACE ( 'NONE', ( #122941 ), #121856, .T. ) ;
#59696 = CARTESIAN_POINT ( 'NONE',  ( 0.7793769126323678575, 1.405529721366456597, 1.547827308177295746 ) ) ;
#59697 = CARTESIAN_POINT ( 'NONE',  ( 7.853197290813620945, 10.18514947741448573, 1.599625672291281386 ) ) ;
#59698 = CARTESIAN_POINT ( 'NONE',  ( 5.122061974917812677, -1.030465543002171858, -1.627433240741954723 ) ) ;
#59699 = CARTESIAN_POINT ( 'NONE',  ( -5.422371370461663176, 8.413518134592214537, -1.199719254218446718 ) ) ;
#59700 = CARTESIAN_POINT ( 'NONE',  ( 1.694096453153286497, -1.816434584207878622, -0.1825648128309723117 ) ) ;
#59701 = CARTESIAN_POINT ( 'NONE',  ( 1.717678464306471087, -0.2677704892378242607, 2.190511422692428045 ) ) ;
#59702 = DIRECTION ( 'NONE',  ( 0.000000000000000000, 0.000000000000000000, 1.000000000000000000 ) ) ;
#59703 = CARTESIAN_POINT ( 'NONE',  ( 0.6680393924826667496, 1.910109291395128972, -0.09634788558426229943 ) ) ;
#59704 = EDGE_CURVE ( 'NONE', #197566, #192999, #172671, .T. ) ;
#59705 = ORIENTED_EDGE ( 'NONE', *, *, #122310, .T. ) ;
#59706 = CARTESIAN_POINT ( 'NONE',  ( 6.877801621836153068, -1.911143888484008846, 0.4753377615324301253 ) ) ;
#59707 = CARTESIAN_POINT ( 'NONE',  ( 2.929168808825276749, -1.306124965484034117, -1.437377093338227496 ) ) ;
#59708 = ORIENTED_EDGE ( 'NONE', *, *, #154260, .F. ) ;
#59709 = CARTESIAN_POINT ( 'NONE',  ( 0.9310172746952742884, 0.9912447863934905623, 1.755501862388042067 ) ) ;
#59711 = CARTESIAN_POINT ( 'NONE',  ( 6.104338052012460381, 1.858797879379699536, 0.09248701691148655812 ) ) ;
#59710 = CARTESIAN_POINT ( 'NONE',  ( -6.330731382938325602, 6.350551133041632212, 0.7998128361456281477 ) ) ;
#59712 = CARTESIAN_POINT ( 'NONE',  ( 4.549643065837591038, 7.465611455855944101, -1.199719254218452047 ) ) ;
#59714 = EDGE_CURVE ( 'NONE', #1142, #55184, #24248, .T. ) ;
#59713 = CARTESIAN_POINT ( 'NONE',  ( 0.000000000000000000, 8.920000000000001705, 0.000000000000000000 ) ) ;
#59715 = CARTESIAN_POINT ( 'NONE',  ( 9.103410076571945453, 12.70806329172093818, 1.199719254218450271 ) ) ;
#59716 = CARTESIAN_POINT ( 'NONE',  ( -5.915435094264120508, 5.795762452929912101, 0.000000000000000000 ) ) ;
#59717 = CARTESIAN_POINT ( 'NONE',  ( -5.855142236255304944, 7.924361590421551860, -1.599625672291271394 ) ) ;
#59718 = CARTESIAN_POINT ( 'NONE',  ( 2.964592600559623037, -2.025863808726846127, -0.8364240203130177687 ) ) ;
#59719 = CARTESIAN_POINT ( 'NONE',  ( 2.548569689688999329, 5.917155704705049146, -0.7216878364870267237 ) ) ;
#59720 = FACE_OUTER_BOUND ( 'NONE', #45976, .T. ) ;
#59721 = LINE ( 'NONE', #189716, #9641 ) ;
#59722 = CARTESIAN_POINT ( 'NONE',  ( 2.437895498511342574, 0.8609710149188254391, -1.609920059450341778 ) ) ;
#59723 = CARTESIAN_POINT ( 'NONE',  ( 7.721398836998401904, -6.134628647623499909, 7.721398836998376147 ) ) ;
#59724 = CARTESIAN_POINT ( 'NONE',  ( -4.172158584703340445, 5.890604320285754980, -1.599625672291256295 ) ) ;
#59725 = AXIS2_PLACEMENT_3D ( 'NONE', #23277, #184712, #87235 ) ;
#59726 = CARTESIAN_POINT ( 'NONE',  ( -5.233950224509621663, 7.808013953112580730, -1.290304472045332496 ) ) ;
#59727 = CARTESIAN_POINT ( 'NONE',  ( -0.02968770228140016343, 0.003472272166151618711, -1.826291111852257343 ) ) ;
#59728 = CARTESIAN_POINT ( 'NONE',  ( 9.725276259704228821, 10.24057714594344048, 0.7998128361456462443 ) ) ;
#59729 = AXIS2_PLACEMENT_3D ( 'NONE', #198660, #130570, #48202 ) ;
#59730 = CARTESIAN_POINT ( 'NONE',  ( 0.5043604530000692643, -0.6477430859608296343, -1.814464506502324159 ) ) ;
#59731 = CARTESIAN_POINT ( 'NONE',  ( 5.735196368693616265, -0.04450293679344322767, -1.961403813732150780 ) ) ;
#59732 = CARTESIAN_POINT ( 'NONE',  ( -1.500000000000001110, 15.02083333333333570, 0.8660254037844419273 ) ) ;
#59733 = CARTESIAN_POINT ( 'NONE',  ( -6.028571859570855729, 10.18508426947466816, 0.000000000000000000 ) ) ;
#59734 = CARTESIAN_POINT ( 'NONE',  ( 4.473300617505036492, 7.306268922809479704, -1.199719254218452047 ) ) ;
#59735 = CARTESIAN_POINT ( 'NONE',  ( 4.739868811304373430, 2.185674081084403753, 0.1610935195608814985 ) ) ;
#59736 = EDGE_CURVE ( 'NONE', #163352, #44633, #142889, .T. ) ;
#59737 = CARTESIAN_POINT ( 'NONE',  ( 3.659811400685081040, 6.357198169852855685, -1.199719254218446718 ) ) ;
#59738 = CARTESIAN_POINT ( 'NONE',  ( 3.959880360806608213, -0.6057208360459276353, 1.979630382156400303 ) ) ;
#59740 = CARTESIAN_POINT ( 'NONE',  ( -0.6823417656250003738, 2.780208333674753618, -1.181850606188749264 ) ) ;
#59739 = CARTESIAN_POINT ( 'NONE',  ( 7.308564027072312008, 14.53708027256903712, 9.465002577604847644 ) ) ;
#59741 = ORIENTED_EDGE ( 'NONE', *, *, #144973, .T. ) ;
#59742 = CARTESIAN_POINT ( 'NONE',  ( 4.500793239850611194, -2.254531372669385636, 0.4477389049844481272 ) ) ;
#59743 = CARTESIAN_POINT ( 'NONE',  ( 8.134528978519385944, 8.592631351135175066, -0.7216878364870267237 ) ) ;
#59744 = CARTESIAN_POINT ( 'NONE',  ( 4.909461021924244051, 6.821066840368686712, 1.443375672974065660 ) ) ;
#59745 = CARTESIAN_POINT ( 'NONE',  ( 0.2348727637096776621, 0.3982709639365061838, 2.257261336973298338 ) ) ;
#59746 = CARTESIAN_POINT ( 'NONE',  ( 6.620655732516645742, 3.706282450693794139, 2.340867613974298767 ) ) ;
#59747 = CARTESIAN_POINT ( 'NONE',  ( -7.425025402139490360, 8.691559719698066289, 1.199719254218452047 ) ) ;
#59748 = CARTESIAN_POINT ( 'NONE',  ( 5.050698599679353862, -1.641444558978710555, -1.037428038565652466 ) ) ;
#59749 = ORIENTED_EDGE ( 'NONE', *, *, #88437, .T. ) ;
#59750 = CARTESIAN_POINT ( 'NONE',  ( 9.883530794237934458, 10.63313346947350269, -0.7216878364870257245 ) ) ;
#59751 = ORIENTED_EDGE ( 'NONE', *, *, #34448, .F. ) ;
#59752 = CARTESIAN_POINT ( 'NONE',  ( 5.361546783204238942, -1.511448857895525855, -1.171587532507123441 ) ) ;
#59753 = CARTESIAN_POINT ( 'NONE',  ( 6.036138234293757954, 0.8456279901550376454, -1.503183349252550371 ) ) ;
#59754 = CARTESIAN_POINT ( 'NONE',  ( 5.208220363674559650, 1.197307938467083055, -1.622483861274232719 ) ) ;
#59756 = CARTESIAN_POINT ( 'NONE',  ( -4.855228407469635243, 4.837057028235559386, 0.7216878364870257245 ) ) ;
#59755 = CARTESIAN_POINT ( 'NONE',  ( -9.287498920561160887, 10.79416914786490089, -1.199719254218441611 ) ) ;
#59757 = CARTESIAN_POINT ( 'NONE',  ( 2.520460663003311730, -4.179124451297094645, -2.338645729556988240 ) ) ;
#59759 = CARTESIAN_POINT ( 'NONE',  ( 6.678955280633751102, -0.08981333502068940267, -1.767555964166868998 ) ) ;
#59758 = CARTESIAN_POINT ( 'NONE',  ( 1.869195317527425404, 2.000202809997845499, -0.6082070056973082339 ) ) ;
#59760 = CARTESIAN_POINT ( 'NONE',  ( 5.326796142270829648, 0.8146286751641409474, -1.844708973168760924 ) ) ;
#59762 = CARTESIAN_POINT ( 'NONE',  ( 3.222906779550426926, 0.05642716604136116532, 2.291727194984194860 ) ) ;
#59761 = CARTESIAN_POINT ( 'NONE',  ( 3.888156192069020634, 7.758209000714329839, 1.040834085586084257E-14 ) ) ;
#59763 = CARTESIAN_POINT ( 'NONE',  ( 1.728031430807571267, 0.1683455491279534644, 1.732166925338991303 ) ) ;
#59764 = AXIS2_PLACEMENT_3D ( 'NONE', #166529, #136180, #135120 ) ;
#59765 = CARTESIAN_POINT ( 'NONE',  ( 3.023802379225454473, -0.4096935937694180518, 2.080477853870852378 ) ) ;
#59766 = CARTESIAN_POINT ( 'NONE',  ( -2.641766398689996187, -0.3984423641809051175, -0.1533590935930825572 ) ) ;
#59767 = CARTESIAN_POINT ( 'NONE',  ( 2.688496201417677867, -0.9952141288376895600, -1.419535560660119655 ) ) ;
#59768 = CARTESIAN_POINT ( 'NONE',  ( -6.960724307482170605E-14, 1.484375000341481066, 1.570758158831758289 ) ) ;
#59769 = CARTESIAN_POINT ( 'NONE',  ( 1.486513762117396498, 1.792272468715813138, 0.5009694556475997596 ) ) ;
#59770 = CARTESIAN_POINT ( 'NONE',  ( 2.313135284333038832, -1.679484837851461965, 1.376015783590480934 ) ) ;
#59771 = CARTESIAN_POINT ( 'NONE',  ( 3.837125247982266174, -1.679222704393277921, -1.116210984008485507 ) ) ;
#59772 = CARTESIAN_POINT ( 'NONE',  ( 5.000000000000003553, -2.717005030479747438E-13, -2.052068128417942727 ) ) ;
#59773 = CARTESIAN_POINT ( 'NONE',  ( -0.7500000000000215383, 1.972916667349486453, 1.299038105676659116 ) ) ;
#59774 = CARTESIAN_POINT ( 'NONE',  ( 6.586557377926046897, -1.889895688126231876, -0.3729288831034789364 ) ) ;
#59775 = ADVANCED_FACE ( 'NONE', ( #138037 ), #204050, .T. ) ;
#59777 = B_SPLINE_CURVE_WITH_KNOTS ( 'NONE', 3,
 ( #131334, #197328, #143301, #127096 ),
 .UNSPECIFIED., .F., .F.,
 ( 4, 4 ),
 ( 0.000000000000000000, 0.0007228752909667262921 ),
 .UNSPECIFIED. ) ;
#59776 = CARTESIAN_POINT ( 'NONE',  ( 1.364683531250000303, 14.75520833367472839, -0.7879004041258355073 ) ) ;
#59778 = CARTESIAN_POINT ( 'NONE',  ( 3.568779976319371272, 0.8023129380761647722, 2.071619486725768677 ) ) ;
#59779 = ORIENTED_EDGE ( 'NONE', *, *, #155510, .F. ) ;
#59780 =( NAMED_UNIT ( * ) SI_UNIT ( $, .STERADIAN. ) SOLID_ANGLE_UNIT ( ) );
#59781 = CARTESIAN_POINT ( 'NONE',  ( -0.7500000000000006661, 0.3583333333333563187, -1.299038105676652011 ) ) ;
#59782 = CARTESIAN_POINT ( 'NONE',  ( 8.925345196497941558, 9.307324238869423283, 1.040834085586084257E-14 ) ) ;
#59783 = CARTESIAN_POINT ( 'NONE',  ( 1.364683531249986537, -0.8447916663252468261, -0.7879004041258309554 ) ) ;
#59784 = CARTESIAN_POINT ( 'NONE',  ( 6.099871961099720963, 1.531114646448136218, 1.609653004599376658 ) ) ;
#59785 = CARTESIAN_POINT ( 'NONE',  ( 4.738696794244872557, -1.902450960283699422, -0.4786090228221794307 ) ) ;
#59787 = CARTESIAN_POINT ( 'NONE',  ( -4.921246572080546500, 8.685278734161874681, 1.214306433183764966E-14 ) ) ;
#59786 = CARTESIAN_POINT ( 'NONE',  ( 4.518945272056516416, 4.166524327021037699, 0.7998128361456341429 ) ) ;
#59788 = CARTESIAN_POINT ( 'NONE',  ( 11.01135777277262306, 10.19999999999999929, -1.400000000000001910 ) ) ;
#59789 = CARTESIAN_POINT ( 'NONE',  ( 6.046200420459929781, 2.259369630126391471, 0.1200006983746708389 ) ) ;
#59790 = CIRCLE ( 'NONE', #70113, 0.5000000000000022204 ) ;
#59791 = TOROIDAL_SURFACE ( 'NONE', #166955, 3.599999999999999201, 0.4999999999999998890 ) ;
#59792 = CARTESIAN_POINT ( 'NONE',  ( 2.629405133799759486, 0.1038056934173016560, -2.060197576267445818 ) ) ;
#59793 = CARTESIAN_POINT ( 'NONE',  ( -5.018489415352746619, 9.006654751220198207, 0.7998128361456481317 ) ) ;
#59794 = ORIENTED_EDGE ( 'NONE', *, *, #79457, .F. ) ;
#59795 = CARTESIAN_POINT ( 'NONE',  ( -0.7500000000000215383, 2.472916667349486897, 1.299038105676671107 ) ) ;
#59796 = CARTESIAN_POINT ( 'NONE',  ( 4.130043426961079511, 1.002751595458702738, -1.578879078160302818 ) ) ;
#59797 = CARTESIAN_POINT ( 'NONE',  ( 2.566726881135486416, -0.8894074178381355944, 1.488501414198806883 ) ) ;
#59798 = CARTESIAN_POINT ( 'NONE',  ( 0.04695162158900589161, -1.836028162657590501, 1.372410674757597704 ) ) ;
#59799 = CARTESIAN_POINT ( 'NONE',  ( 1.097021799178355739, -0.5375665728563282508, -2.140183485690804410 ) ) ;
#59800 = CARTESIAN_POINT ( 'NONE',  ( 6.246037776718591061, 0.6113502166280659900, 1.843275756764614082 ) ) ;
#59802 = EDGE_LOOP ( 'NONE', ( #205695, #113982, #71531, #28758 ) ) ;
#59801 = CARTESIAN_POINT ( 'NONE',  ( 8.230252249265882725, 15.15998367271711622, 8.673456544423645553 ) ) ;
#59803 = CARTESIAN_POINT ( 'NONE',  ( 0.1874999572450692098, -1.451030237095527475, 1.451031289061128993 ) ) ;
#59804 = CARTESIAN_POINT ( 'NONE',  ( 0.1764080092822375156, 1.496053712750060383, 1.352152247781977179 ) ) ;
#59805 = FILL_AREA_STYLE ('',( #91267 ) ) ;
#59806 = DIRECTION ( 'NONE',  ( -3.330669073875478989E-16, 3.330669073875478989E-16, 1.000000000000000000 ) ) ;
#59808 = CARTESIAN_POINT ( 'NONE',  ( 6.399064592084179992, -0.9530083391863402031, -1.777013033299412292 ) ) ;
#59807 = CIRCLE ( 'NONE', #198315, 11.09999999999999964 ) ;
#59809 = CARTESIAN_POINT ( 'NONE',  ( -10.00321840878439339, 10.56484298653695397, 1.040834085586084257E-14 ) ) ;
#59810 = CARTESIAN_POINT ( 'NONE',  ( 6.608709811657416999, 9.797579649320619311, -1.199719254218440723 ) ) ;
#59811 = CARTESIAN_POINT ( 'NONE',  ( 2.651186565980344856, -0.4067314603539678441, -0.1428011528578489453 ) ) ;
#59812 = CARTESIAN_POINT ( 'NONE',  ( 4.934128534657983067, 0.9357288403324083292, -1.567518238613223813 ) ) ;
#59813 = CARTESIAN_POINT ( 'NONE',  ( 1.958336283151569157, 2.200835622443702011, -0.1624582802550941507 ) ) ;
#59814 = ORIENTED_EDGE ( 'NONE', *, *, #107076, .T. ) ;
#59815 = CARTESIAN_POINT ( 'NONE',  ( -4.136646265500970365, 5.919449624541475607, -1.443375672974066548 ) ) ;
#59816 = UNCERTAINTY_MEASURE_WITH_UNIT (LENGTH_MEASURE( 1.000000000000000082E-05 ), #155137, 'distance_accuracy_value', 'NONE');
#59817 = CARTESIAN_POINT ( 'NONE',  ( 1.642778471875001811, -1.480208332855375453, 2.845375778867859751 ) ) ;
#59818 = CARTESIAN_POINT ( 'NONE',  ( -6.347188469492005325, 10.55680364771601809, -0.7998128361456291469 ) ) ;
#59819 = CARTESIAN_POINT ( 'NONE',  ( 0.8264327134144221487, -0.9118592345104499231, -1.802339519251413780 ) ) ;
#59821 = CARTESIAN_POINT ( 'NONE',  ( 0.000000000000000000, 8.600000000000017408, -0.3999999999999819811 ) ) ;
#59820 =( GEOMETRIC_REPRESENTATION_CONTEXT ( 3 ) GLOBAL_UNCERTAINTY_ASSIGNED_CONTEXT ( ( #117724 ) ) GLOBAL_UNIT_ASSIGNED_CONTEXT ( ( #20792, #39202, #157239 ) ) REPRESENTATION_CONTEXT ( 'NONE', 'WORKASPACE' ) );
#59822 = CARTESIAN_POINT ( 'NONE',  ( -3.149236820124241110, 6.896136400112061970, -0.7998128361456481317 ) ) ;
#59823 = CARTESIAN_POINT ( 'NONE',  ( 2.957670719111748614, -0.5886736602933821949, 1.765425544305933014 ) ) ;
#59824 = CARTESIAN_POINT ( 'NONE',  ( 9.459838494033030898, 12.05956421450382088, 1.599625672291281386 ) ) ;
#59825 = CARTESIAN_POINT ( 'NONE',  ( 5.836564609439236939, 0.5826586670559866787, -1.930416874340326938 ) ) ;
#59826 = VERTEX_POINT ( 'NONE', #139105 ) ;
#59827 = EDGE_LOOP ( 'NONE', ( #183848, #92999, #36762, #117836, #179058, #23243, #32799, #202169 ) ) ;
#59828 = CARTESIAN_POINT ( 'NONE',  ( -9.671043645249580933, 10.17730576241299900, 0.7998128361456462443 ) ) ;
#59829 = CARTESIAN_POINT ( 'NONE',  ( 4.195794211080963620, -0.6966935528937777677, 1.687730213881050600 ) ) ;
#59831 = CARTESIAN_POINT ( 'NONE',  ( -4.816275411463948330, 6.948951914485960835, -1.437501944199247372 ) ) ;
#59830 = CARTESIAN_POINT ( 'NONE',  ( -5.978219388983010418, 5.939287140093762574, -0.7998128361456362523 ) ) ;
#59832 = CARTESIAN_POINT ( 'NONE',  ( 5.662876554447811017, 7.443216037249618999, -1.326882488215734845 ) ) ;
#59833 = CARTESIAN_POINT ( 'NONE',  ( 6.608749954595573683, 0.7741944705832277673, -1.861732896133998727 ) ) ;
#59834 = CARTESIAN_POINT ( 'NONE',  ( 5.613187951484799321, -1.795345830453990654, 0.4073638586896133340 ) ) ;
#59835 = CARTESIAN_POINT ( 'NONE',  ( 4.670747285963097184, -1.509779504925019999, 1.745381082733918676 ) ) ;
#59836 = CARTESIAN_POINT ( 'NONE',  ( 3.555981428534177091, 7.370671776590375757, 0.7998128361456271485 ) ) ;
#59837 = CARTESIAN_POINT ( 'NONE',  ( 6.802040682177005415, -2.161276877365316818, 0.04550429416337595928 ) ) ;
#59838 = CARTESIAN_POINT ( 'NONE',  ( 1.944774020950320592, -1.561091384877069554, -1.155077030050962295 ) ) ;
#59839 = ADVANCED_FACE ( 'NONE', ( #90351 ), #164986, .T. ) ;
#59840 = CARTESIAN_POINT ( 'NONE',  ( 5.975955848901470802, 2.022625890308630048, 1.091648031176053468 ) ) ;
#59841 = DIRECTION ( 'NONE',  ( 0.000000000000000000, 0.000000000000000000, -1.000000000000000000 ) ) ;
#59842 = CARTESIAN_POINT ( 'NONE',  ( -8.086512275908061653, 8.398962174839683215, 0.000000000000000000 ) ) ;
#59843 = CARTESIAN_POINT ( 'NONE',  ( 4.153091690245942047, -1.555063956268587066, -1.039456662654779207 ) ) ;
#59844 = VERTEX_POINT ( 'NONE', #177580 ) ;
#59847 = CARTESIAN_POINT ( 'NONE',  ( -6.147696309153835692, 6.137010213626392208, 0.7998128361456281477 ) ) ;
#59846 = CARTESIAN_POINT ( 'NONE',  ( 1.499999999999987121, 1.327083334016149641, -0.8660254037844253849 ) ) ;
#59845 = CARTESIAN_POINT ( 'NONE',  ( 2.795058504854182946, -0.1448928079688660830, -1.906987441340234568 ) ) ;
#59848 = CARTESIAN_POINT ( 'NONE',  ( 4.354274438496381627, 2.206422198305586058, -0.05263853172451230661 ) ) ;
#59849 = CARTESIAN_POINT ( 'NONE',  ( -0.6125000000000089262, 0.02083333401611819902, -1.060881119635969094 ) ) ;
#59850 = FACE_OUTER_BOUND ( 'NONE', #20221, .T. ) ;
#59851 = CARTESIAN_POINT ( 'NONE',  ( 5.858531774436539052, 6.007577623030311287, 0.000000000000000000 ) ) ;
#59852 = CARTESIAN_POINT ( 'NONE',  ( -5.980555156959541208, 7.110307450275150210, 1.082531754730549078 ) ) ;
#59853 = CARTESIAN_POINT ( 'NONE',  ( 1.985558396190547858, 1.356547016436062014, 1.430631702862941168 ) ) ;
#59854 = CARTESIAN_POINT ( 'NONE',  ( 2.292384291596425427, -0.9864983578860975211, 2.086231237977907327 ) ) ;
#59855 = CARTESIAN_POINT ( 'NONE',  ( 3.051168888765115828, 1.684027830550902882, -1.006202029777767848 ) ) ;
#59856 = CARTESIAN_POINT ( 'NONE',  ( -5.207729805571693404, 7.804368671438548510, -1.360913387355301207 ) ) ;
#59857 = CARTESIAN_POINT ( 'NONE',  ( 6.104357437187505120, 2.059938769829409377, 0.1070097549743902060 ) ) ;
#59858 = CARTESIAN_POINT ( 'NONE',  ( 4.256897045010922476, 5.029096643009940415, -1.082531754730548412 ) ) ;
#59859 = CARTESIAN_POINT ( 'NONE',  ( 4.048064755690682581, 0.9548552675892291175, 1.776167154503265566 ) ) ;
#59860 = CARTESIAN_POINT ( 'NONE',  ( 3.770049233051776749, 6.556085317605844232, 1.199719254218451159 ) ) ;
#59861 = ORIENTED_EDGE ( 'NONE', *, *, #11172, .T. ) ;
#59862 = CARTESIAN_POINT ( 'NONE',  ( 4.663296154398564042, 1.879804967172087782, -0.7303043177912388328 ) ) ;
#59863 = CARTESIAN_POINT ( 'NONE',  ( -1.001543065824772872E-14, 5.384375000341415252, 1.575800808251672791 ) ) ;
#59864 = CARTESIAN_POINT ( 'NONE',  ( -1.115562610750309283E-14, 10.09375000068279782, 1.500000000000001554 ) ) ;
#59865 = DIRECTION ( 'NONE',  ( 3.330669073875479482E-16, -3.330669073875479482E-16, -1.000000000000000000 ) ) ;
#59866 = CARTESIAN_POINT ( 'NONE',  ( 8.048736748007069508, 12.54194330598362406, -0.7998128361456352531 ) ) ;
#59867 = CARTESIAN_POINT ( 'NONE',  ( 2.044024736616629312, 1.494777392302085062, 1.574780046323517313 ) ) ;
#59868 = CARTESIAN_POINT ( 'NONE',  ( 5.204350862799327793, 7.165104988056252289, -1.599625672291281386 ) ) ;
#59869 = CARTESIAN_POINT ( 'NONE',  ( 4.008199524592567897, 7.584238231759597326, 0.2402771892247856922 ) ) ;
#59870 = CARTESIAN_POINT ( 'NONE',  ( 2.794054307841778773, -1.865266697571519972, -0.1415833504254116748 ) ) ;
#59871 = CARTESIAN_POINT ( 'NONE',  ( 6.468072252983536607, 1.105043713804385153, 1.857642994352682653 ) ) ;
#59873 = CARTESIAN_POINT ( 'NONE',  ( 6.827182134110172385, 0.001020705822878456353, 1.910856149448317165 ) ) ;
#59872 = CARTESIAN_POINT ( 'NONE',  ( -0.02244404828160087226, 6.946777552644228138, -2.784171975256703124 ) ) ;
#59874 = CARTESIAN_POINT ( 'NONE',  ( -1.201851678989727383E-14, 1.321875000341419248, 1.575800808251672791 ) ) ;
#59875 = CARTESIAN_POINT ( 'NONE',  ( -0.1409997244346088141, 7.629137130509076492, -2.600278764091648487 ) ) ;
#59876 = CARTESIAN_POINT ( 'NONE',  ( 3.914637684252043393, -0.6027250981219151038, -1.814865640613130493 ) ) ;
#59877 = VECTOR ( 'NONE', #81248, 1000.000000000000000 ) ;
#59878 = CARTESIAN_POINT ( 'NONE',  ( 4.012378993168019825, 1.251447367628313767, -1.251755930634059100 ) ) ;
#59879 = CARTESIAN_POINT ( 'NONE',  ( 1.928230879603441750, -0.9027140558476205445, -1.685813393195116694 ) ) ;
#59880 = AXIS2_PLACEMENT_3D ( 'NONE', #25007, #142006, #110607 ) ;
#59881 = CARTESIAN_POINT ( 'NONE',  ( -3.554208825076827782, 7.298327395898266623, 0.7998128361456341429 ) ) ;
#59883 = CARTESIAN_POINT ( 'NONE',  ( 6.450803866275835574, -1.753708343991422502, -0.7711757456045026382 ) ) ;
#59882 = LINE ( 'NONE', #58818, #14563 ) ;
#59884 = CARTESIAN_POINT ( 'NONE',  ( -1.500000000000013101, -0.3291666666666463459, 0.8660254037844403729 ) ) ;
#59885 = CARTESIAN_POINT ( 'NONE',  ( 1.293514844328220281, -1.872496763586928514, 0.8835221827151735763 ) ) ;
#59886 = CARTESIAN_POINT ( 'NONE',  ( -1.364683531250014514, -1.157291666325248158, 0.7879004041258379498 ) ) ;
#59887 = CARTESIAN_POINT ( 'NONE',  ( 6.578970801323708706, -0.09418725797194843485, -1.868394071727994543 ) ) ;
#59888 = CARTESIAN_POINT ( 'NONE',  ( 1.541335573940459058, -1.321205422867760548, -1.260230113935792318 ) ) ;
#59890 = CARTESIAN_POINT ( 'NONE',  ( 4.646267551848549004, 8.309382712783076386, 0.4446711254955729165 ) ) ;
#59889 = CARTESIAN_POINT ( 'NONE',  ( 6.129534211984397629, -2.079372889712034489, 0.7396383780838566846 ) ) ;
#59891 = CARTESIAN_POINT ( 'NONE',  ( -1.364683531249997417, 5.571875000341417916, 1.214306433183764966E-14 ) ) ;
#59892 = CARTESIAN_POINT ( 'NONE',  ( 3.104023224481029519, 0.7448178976848550681, -1.923671348419103921 ) ) ;
#59893 = CARTESIAN_POINT ( 'NONE',  ( -6.191269702934848240, 10.37489842006599616, 0.000000000000000000 ) ) ;
#59894 = CARTESIAN_POINT ( 'NONE',  ( 8.269583629331492602, 11.73526576994040482, 1.199719254218450271 ) ) ;
#59895 = CARTESIAN_POINT ( 'NONE',  ( 1.500389033793473992, 3.249152749159987419, 0.07878897303667579954 ) ) ;
#59896 = CARTESIAN_POINT ( 'NONE',  ( 0.4917760118960182170, 1.601382895956671826, 1.452064325093614716 ) ) ;
#59897 = CARTESIAN_POINT ( 'NONE',  ( 7.340813827156391191, 7.528980651296110160, 0.7998128361456281477 ) ) ;
#59898 = ORIENTED_EDGE ( 'NONE', *, *, #130874, .T. ) ;
#59899 = CARTESIAN_POINT ( 'NONE',  ( 4.844224204019831781, -0.9789346907586125024, 1.824324395707350943 ) ) ;
#59900 = CARTESIAN_POINT ( 'NONE',  ( -1.364683531250014514, 0.05104166700808546175, -0.7879004041258359514 ) ) ;
#59901 = CARTESIAN_POINT ( 'NONE',  ( 2.741676502816026595, -1.599691942034554337, -1.453933697666408120 ) ) ;
#59902 = CARTESIAN_POINT ( 'NONE',  ( -4.652699544748355898, 8.322425126176462129, -0.4365168051920116365 ) ) ;
#59903 = CARTESIAN_POINT ( 'NONE',  ( 2.947920495102425154, -1.358134161044775245, -1.495000266999703564 ) ) ;
#59904 = CARTESIAN_POINT ( 'NONE',  ( 6.620655732516651071, 2.021119449029490589, 2.477762541108457839 ) ) ;
#59906 = CARTESIAN_POINT ( 'NONE',  ( 5.504247177468168495, 9.365446107114122398, 0.7216878364870438212 ) ) ;
#59905 = CARTESIAN_POINT ( 'NONE',  ( 1.737500000000001155, -1.633333333333333748, 3.009438278150922130 ) ) ;
#59907 = CARTESIAN_POINT ( 'NONE',  ( -5.935437387732586778, 10.14670372898850381, -0.7998128361456362523 ) ) ;
#59908 = CARTESIAN_POINT ( 'NONE',  ( 1.059780186608853203, 1.205045252304644210, 1.616690996016925563 ) ) ;
#59910 = CARTESIAN_POINT ( 'NONE',  ( 5.671465802443460547, 1.304529079428708549, 1.760837017921567771 ) ) ;
#59909 = CARTESIAN_POINT ( 'NONE',  ( -5.253948220495577637, 6.088359997788290734, 1.199719254218450271 ) ) ;
#59911 = CARTESIAN_POINT ( 'NONE',  ( 5.115449499555525747, 1.566912803841558732, 1.096118974231160781 ) ) ;
#59912 = CARTESIAN_POINT ( 'NONE',  ( -11.97178994924802353, 12.22000006202794609, 0.8322011300497199615 ) ) ;
#59913 = CARTESIAN_POINT ( 'NONE',  ( 5.978782553502139940, 6.077593855281705260, -0.7216878364870257245 ) ) ;
#59915 = CARTESIAN_POINT ( 'NONE',  ( 3.427361390312729572, -1.528753972193249933, -1.314983687342549556 ) ) ;
#59914 = CARTESIAN_POINT ( 'NONE',  ( -10.26315909542058336, 11.07603315418659840, -0.7216878364870267237 ) ) ;
#59916 = CARTESIAN_POINT ( 'NONE',  ( 1.364683531250000303, 13.31770833367472839, -0.7879004041258355073 ) ) ;
#59917 = B_SPLINE_CURVE_WITH_KNOTS ( 'NONE', 3,
 ( #135269, #3080, #34538, #947, #182923, #35601, #153637, #52926, #20414, #168809 ),
 .UNSPECIFIED., .F., .F.,
 ( 4, 3, 3, 4 ),
 ( 0.000000000000000000, 0.0001748898611877313010, 0.0003306773789565961162, 0.0004872651007806716407 ),
 .UNSPECIFIED. ) ;
#59918 = CARTESIAN_POINT ( 'NONE',  ( 5.825168945638790063, -0.03770542841243298970, 1.724543776939557960 ) ) ;
#59919 = CARTESIAN_POINT ( 'NONE',  ( 5.203297092594585393, 9.292540051327542017, 0.7998128361456341429 ) ) ;
#59920 = STYLED_ITEM ( 'NONE', ( #170797 ), #30374 ) ;
#59921 = CARTESIAN_POINT ( 'NONE',  ( 10.08690309888728187, 10.87040115823107911, -0.7216878364870257245 ) ) ;
#59922 = CARTESIAN_POINT ( 'NONE',  ( -11.52469724861193967, 11.37999993351231254, -3.346365485506884063 ) ) ;
#59923 = CARTESIAN_POINT ( 'NONE',  ( 4.077312411328878561, 1.762187477035919603, -0.6278270876356045749 ) ) ;
#59924 = CARTESIAN_POINT ( 'NONE',  ( 7.065207446497155708, 9.336104335703744539, 0.000000000000000000 ) ) ;
#59925 = CARTESIAN_POINT ( 'NONE',  ( 1.129834432590616000, 1.996231214973245516, -0.5485114149718293142 ) ) ;
#59926 = CARTESIAN_POINT ( 'NONE',  ( -11.52463353791760348, 12.21999999999998110, 3.346594096177640143 ) ) ;
#59927 = ORIENTED_EDGE ( 'NONE', *, *, #35402, .T. ) ;
#59928 = CARTESIAN_POINT ( 'NONE',  ( 6.252603509501785339, 1.792834410666717337, 0.2582872775454737591 ) ) ;
#59929 = CARTESIAN_POINT ( 'NONE',  ( 2.905190055078214595, 6.611415174225076186, 0.7998128361456271485 ) ) ;
#59930 = CARTESIAN_POINT ( 'NONE',  ( -0.08826282632121498772, -1.242921985031696153, -1.588411632956095110 ) ) ;
#59931 = CARTESIAN_POINT ( 'NONE',  ( 0.1756362645438137582, 1.791864648875134636, -0.2657654445481233418 ) ) ;
#59932 = CARTESIAN_POINT ( 'NONE',  ( 4.489158259456265121, 7.291082831790689056, -1.082531754730548412 ) ) ;
#59933 = CARTESIAN_POINT ( 'NONE',  ( 9.428250952287722697, 13.54490846161957585, -7.423481931054030092 ) ) ;
#59934 = VERTEX_POINT ( 'NONE', #94214 ) ;
#59935 = CARTESIAN_POINT ( 'NONE',  ( 7.578644679914694926, 11.78557652663510424, 0.7216878364870438212 ) ) ;
#59937 = CARTESIAN_POINT ( 'NONE',  ( 7.914208982075123799, 10.25632978388623684, -1.599625672291262513 ) ) ;
#59936 = CARTESIAN_POINT ( 'NONE',  ( 1.047228354049560828, 1.731870006261830630, -0.9216698261682305660 ) ) ;
#59938 = CARTESIAN_POINT ( 'NONE',  ( 4.851152330137978197, 0.1832884931825354280, -1.906798003172151867 ) ) ;
#59939 = AXIS2_PLACEMENT_3D ( 'NONE', #82112, #49620, #148205 ) ;
#59940 = CARTESIAN_POINT ( 'NONE',  ( 6.827182134110195477, 0.006757161851597697118, 1.710856279483467857 ) ) ;
#59941 = CARTESIAN_POINT ( 'NONE',  ( -5.568215224448921141, 7.423109701660543180, 1.245465753432648093 ) ) ;
#59942 = B_SPLINE_CURVE_WITH_KNOTS ( 'NONE', 3,
 ( #181314, #5468, #169067, #16665 ),
 .UNSPECIFIED., .F., .F.,
 ( 4, 4 ),
 ( 1.083473084032624673E-15, 8.505390839925406612E-05 ),
 .UNSPECIFIED. ) ;
#59944 = EDGE_LOOP ( 'NONE', ( #60880, #207493, #176440, #157755, #73241 ) ) ;
#59943 = CARTESIAN_POINT ( 'NONE',  ( 5.680503174445848735, 5.729601246382692636, 1.040834085586084257E-14 ) ) ;
#59945 = CARTESIAN_POINT ( 'NONE',  ( -8.839552966430007430, 11.33589776563360019, -1.443375672974059665 ) ) ;
#59946 = CARTESIAN_POINT ( 'NONE',  ( 1.745224485312408813, -1.826185749030174499, 1.156423465944363294 ) ) ;
#59947 = CARTESIAN_POINT ( 'NONE',  ( -4.146814880933400005, 5.931313009212638931, 1.599625672291270506 ) ) ;
#59948 = CARTESIAN_POINT ( 'NONE',  ( 7.512626515748113576, 7.937354821227203594, 0.7216878364870267237 ) ) ;
#59949 = CARTESIAN_POINT ( 'NONE',  ( 0.05319811239242258627, 0.3688592364489845510, 2.088132107045739705 ) ) ;
#59950 = CARTESIAN_POINT ( 'NONE',  ( 4.348545414961950684, 0.4871326187540457875, 1.759326811173238303 ) ) ;
#59951 = AXIS2_PLACEMENT_3D ( 'NONE', #39590, #72065, #105694 ) ;
#59952 = CARTESIAN_POINT ( 'NONE',  ( 8.358788729863725564, 13.10643031998909258, -8.536585299322529963 ) ) ;
#59953 = CARTESIAN_POINT ( 'NONE',  ( 1.581257511629934775, 1.823016439315219062, -0.7507060404894276839 ) ) ;
#59954 = CARTESIAN_POINT ( 'NONE',  ( 3.287273477832891366, 0.04233216220104508987, -1.912079899511004433 ) ) ;
#59955 = ORIENTED_EDGE ( 'NONE', *, *, #122422, .F. ) ;
#59956 = DIRECTION ( 'NONE',  ( 1.000000000000000000, 0.000000000000000000, 0.000000000000000000 ) ) ;
#59957 = CARTESIAN_POINT ( 'NONE',  ( 4.123468233510577896, 0.2432657155154849538, -1.954413393957514788 ) ) ;
#59958 = EDGE_LOOP ( 'NONE', ( #175177, #175570, #88728, #105076 ) ) ;
#59959 = CARTESIAN_POINT ( 'NONE',  ( 5.812047917624927784, 1.301047364602755829, -1.442011890679588904 ) ) ;
#59960 = ORIENTED_EDGE ( 'NONE', *, *, #84325, .F. ) ;
#59961 = CARTESIAN_POINT ( 'NONE',  ( -6.947627372360122955, 7.070263120700404968, 0.000000000000000000 ) ) ;
#59963 = CARTESIAN_POINT ( 'NONE',  ( 6.956254272497339741, -6.713678229395078745, -6.457408393014691050 ) ) ;
#59962 = CARTESIAN_POINT ( 'NONE',  ( -5.123001941117347080, 7.070197912760590064, 1.599625672291263179 ) ) ;
#59965 = ADVANCED_FACE ( 'NONE', ( #160254 ), #11855, .F. ) ;
#59964 = CARTESIAN_POINT ( 'NONE',  ( 5.682275777458829502, 9.643422483761748154, 0.7216878364870317197 ) ) ;
#59966 = CARTESIAN_POINT ( 'NONE',  ( 4.459560945705238311, -1.480416612418914424, -1.210464771850598975 ) ) ;
#59967 = CARTESIAN_POINT ( 'NONE',  ( 6.983263157960366563, -0.003091553303710344557, 1.945923119799706669 ) ) ;
#59968 = DIRECTION ( 'NONE',  ( 0.000000000000000000, -1.000000000000000000, 0.000000000000000000 ) ) ;
#59969 = DIRECTION ( 'NONE',  ( 1.000000000000000000, -0.000000000000000000, 1.224646799147353207E-16 ) ) ;
#59970 = CARTESIAN_POINT ( 'NONE',  ( 5.426436493548534301, -0.9073095142285032555, -1.797119830347380542 ) ) ;
#59972 =( BOUNDED_CURVE ( )  B_SPLINE_CURVE ( 3, ( #119046, #20403, #102741, #168796 ),
 .UNSPECIFIED., .F., .T. ) 
 B_SPLINE_CURVE_WITH_KNOTS ( ( 4, 4 ),
 ( 4.082329036743725936, 4.712388980384688786 ),
 .UNSPECIFIED. ) 
 CURVE ( )  GEOMETRIC_REPRESENTATION_ITEM ( )  RATIONAL_B_SPLINE_CURVE ( ( 1.000000000000000000, 0.9671913951488946282, 0.9671913951488946282, 1.000000000000000000 ) ) 
 REPRESENTATION_ITEM ( '' )  );
#59971 = CARTESIAN_POINT ( 'NONE',  ( -1.734723475976807094E-15, 2.999999999999988898, -6.938893903907228378E-15 ) ) ;
#59973 = CARTESIAN_POINT ( 'NONE',  ( 6.445924739416000193, 0.6936395621829589686, -1.688995215704327313 ) ) ;
#59974 = CARTESIAN_POINT ( 'NONE',  ( 2.049362625460974030, 1.802418521853879962, -1.018503948505583789 ) ) ;
#59975 = CARTESIAN_POINT ( 'NONE',  ( -6.399085315970132193, 10.40942393536641397, -0.7216878364870278340 ) ) ;
#59976 = CARTESIAN_POINT ( 'NONE',  ( -6.300768610526733760, 6.888587422923714954, -0.7334343799849201151 ) ) ;
#59977 = FACE_BOUND ( 'NONE', #54233, .T. ) ;
#59978 = CARTESIAN_POINT ( 'NONE',  ( 6.332864056472936376, 0.1854757364097951722, 1.861418627818342664 ) ) ;
#59979 = CARTESIAN_POINT ( 'NONE',  ( 4.798696304233017074, 7.685897223992134819, -1.199719254218452047 ) ) ;
#59980 = CARTESIAN_POINT ( 'NONE',  ( -4.623494077460110319, 5.352830164246910272, 1.199719254218462483 ) ) ;
#59981 = CARTESIAN_POINT ( 'NONE',  ( 4.245111494854632461, 7.966730820723463502, 0.000000000000000000 ) ) ;
#59982 = CARTESIAN_POINT ( 'NONE',  ( 3.216308754939877446, 4.775446185561722956, -1.599625672291262513 ) ) ;
#59983 = CARTESIAN_POINT ( 'NONE',  ( 1.364683531250000303, 11.81770833367472839, -0.7879004041258355073 ) ) ;
#59984 = CARTESIAN_POINT ( 'NONE',  ( -4.731959306369413198, 5.479372931307791461, -1.199719254218446718 ) ) ;
#59986 = CARTESIAN_POINT ( 'NONE',  ( -5.661411662158206681, 8.762674818229999829, -1.199719254218452047 ) ) ;
#59985 = LINE ( 'NONE', #143415, #186772 ) ;
#59987 = CARTESIAN_POINT ( 'NONE',  ( 3.973097536218972436, -1.716008982208137468, -0.2490561736530460535 ) ) ;
#59988 = CARTESIAN_POINT ( 'NONE',  ( -4.391951695823077984, 7.211361847513815704, 1.199719254218464037 ) ) ;
#59989 = CARTESIAN_POINT ( 'NONE',  ( 2.202089267374872872, 0.7962392033929905910, -1.911209141678638090 ) ) ;
#59990 = EDGE_CURVE ( 'NONE', #152119, #127188, #211563, .T. ) ;
#59991 = CARTESIAN_POINT ( 'NONE',  ( 3.620818518838536004, 0.3129716219542731936, 2.093870907184330221 ) ) ;
#59992 = CARTESIAN_POINT ( 'NONE',  ( 8.046927864910717432, 9.346836249606042202, 1.199719254218462483 ) ) ;
#59993 = CARTESIAN_POINT ( 'NONE',  ( 0.6823417656249917140, 3.342708333674754506, 1.181850606188765695 ) ) ;
#59994 = CARTESIAN_POINT ( 'NONE',  ( 1.323035253951538426, -1.778235669024318177, -0.8468731209588018505 ) ) ;
#59995 = CARTESIAN_POINT ( 'NONE',  ( 6.112956004491900686, 6.016961049888108981, 0.08799760576284378077 ) ) ;
#59996 = CARTESIAN_POINT ( 'NONE',  ( 3.334942599281629949, 5.874221551595115720, -1.082531754730543083 ) ) ;
#59998 = CARTESIAN_POINT ( 'NONE',  ( -0.1933232215488022709, -0.4202133615931051835, -1.872389726556406897 ) ) ;
#59997 = CARTESIAN_POINT ( 'NONE',  ( 0.000000000000000000, -2.537500000000000977, -4.012584370867899430 ) ) ;
#59999 = CARTESIAN_POINT ( 'NONE',  ( 3.521668038933927658, -1.364967583988693889, -1.841414078927001041 ) ) ;
#60000 = CARTESIAN_POINT ( 'NONE',  ( 0.2580658466875830337, 0.6954254843183352852, 1.688255465954719536 ) ) ;
#60001 = CARTESIAN_POINT ( 'NONE',  ( 2.847809051801777791, -1.287500320553297994, -1.414207669007704116 ) ) ;
#60002 = CARTESIAN_POINT ( 'NONE',  ( 4.857564175446106525, 8.889184981320973122, 0.7998128361456331437 ) ) ;
#60003 = CARTESIAN_POINT ( 'NONE',  ( 6.602457619730760285, 8.725953194484466380, 1.443375672974076540 ) ) ;
#60004 = CARTESIAN_POINT ( 'NONE',  ( -9.020252271793614440, 9.418049160047695878, 0.7998128361456462443 ) ) ;
#60005 = CARTESIAN_POINT ( 'NONE',  ( 1.318609283782465003, -0.7284450440303428254, -1.876953636963938354 ) ) ;
#60006 = CARTESIAN_POINT ( 'NONE',  ( 2.114041031776827673, 1.956853317873577414, -0.1391692324632237410 ) ) ;
#60007 = CARTESIAN_POINT ( 'NONE',  ( -8.779068160048691283, 10.20099992726700933, -1.199719254218446718 ) ) ;
#60008 = CARTESIAN_POINT ( 'NONE',  ( -4.876128802409253282, 8.840567369452784874, 0.7998128361456481317 ) ) ;
#60009 = CARTESIAN_POINT ( 'NONE',  ( 1.836970198721030181E-16, 13.49999999999999822, 1.500000000000000222 ) ) ;
#60011 = CARTESIAN_POINT ( 'NONE',  ( 3.608038473134207891, -0.7167157551234564217, -1.618410677222481553 ) ) ;
#60010 = CARTESIAN_POINT ( 'NONE',  ( 4.646477879911859787, -1.679251869332079483, 1.245118527403435094 ) ) ;
#60012 = CARTESIAN_POINT ( 'NONE',  ( -6.671583288098690723, 14.00000000000246381, 9.747470831330483421 ) ) ;
#60013 = CARTESIAN_POINT ( 'NONE',  ( 0.1995291103054769866, -0.5802879427523646161, 2.113158525371459096 ) ) ;
#60014 = CARTESIAN_POINT ( 'NONE',  ( 5.208843366089195293, -0.2500283176610699210, 1.722145524253251514 ) ) ;
#60015 = CARTESIAN_POINT ( 'NONE',  ( 8.613507663383630941, 8.943513783569379427, -0.7998128361456221525 ) ) ;
#60016 = CARTESIAN_POINT ( 'NONE',  ( 6.293571109369822558, 1.706569967861866877, -1.540138442258129459 ) ) ;
#60017 = DIRECTION ( 'NONE',  ( 0.000000000000000000, -1.000000000000000000, 0.000000000000000000 ) ) ;
#60018 = CARTESIAN_POINT ( 'NONE',  ( 5.343005094570719038, -0.9615459055183853687, 1.442522970604209531 ) ) ;
#60019 =( GEOMETRIC_REPRESENTATION_CONTEXT ( 3 ) GLOBAL_UNCERTAINTY_ASSIGNED_CONTEXT ( ( #210303 ) ) GLOBAL_UNIT_ASSIGNED_CONTEXT ( ( #71987, #184678, #200914 ) ) REPRESENTATION_CONTEXT ( 'NONE', 'WORKASPACE' ) );
#60020 = CARTESIAN_POINT ( 'NONE',  ( 6.320782530974223157, -1.539933897815339403, 1.530818809132200142 ) ) ;
#60021 = CARTESIAN_POINT ( 'NONE',  ( -0.3282377607281422582, 2.948664549684636427, -1.225000000000019851 ) ) ;
#60022 = CARTESIAN_POINT ( 'NONE',  ( 0.1459223332197969736, 2.093306735845179567, -0.3175718533311999714 ) ) ;
#60023 = CARTESIAN_POINT ( 'NONE',  ( 4.625000000000002665, -2.052068128417944504, 2.503915141160646116E-13 ) ) ;
#60024 =( GEOMETRIC_REPRESENTATION_CONTEXT ( 3 ) GLOBAL_UNCERTAINTY_ASSIGNED_CONTEXT ( ( #123041 ) ) GLOBAL_UNIT_ASSIGNED_CONTEXT ( ( #21195, #88372, #184777 ) ) REPRESENTATION_CONTEXT ( 'NONE', 'WORKASPACE' ) );
#60025 = DIRECTION ( 'NONE',  ( 8.638326563840814399E-31, 0.000000000000000000, 1.000000000000000000 ) ) ;
#60026 = CARTESIAN_POINT ( 'NONE',  ( 3.047785661706010174, 0.6947733606382737737, -1.796906316042534923 ) ) ;
#60027 = CARTESIAN_POINT ( 'NONE',  ( 1.500000000000001332, 11.65625000068279427, 0.000000000000000000 ) ) ;
#60028 = CARTESIAN_POINT ( 'NONE',  ( 0.4346306299643958315, -1.193539479193185038, -1.873246666896864143 ) ) ;
#60029 = VERTEX_POINT ( 'NONE', #97410 ) ;
#60030 = CARTESIAN_POINT ( 'NONE',  ( 0.7499999999999902300, 5.066666666666684193, -1.299038105676658228 ) ) ;
#60031 = CARTESIAN_POINT ( 'NONE',  ( 5.508690485854129903, 5.321227076451600091, 1.040834085586084257E-14 ) ) ;
#60032 = CARTESIAN_POINT ( 'NONE',  ( 7.820355676984174664, 8.018169799436671852, -0.7998128361456281477 ) ) ;
#60033 = CARTESIAN_POINT ( 'NONE',  ( 2.086886708931742884, -1.363721155840109889, 1.753348597404544185 ) ) ;
#60034 = CARTESIAN_POINT ( 'NONE',  ( 5.504247177468168495, 9.365446107114122398, 0.7216878364870438212 ) ) ;
#60035 = CARTESIAN_POINT ( 'NONE',  ( -9.463228032214294316, 10.14278024711257764, 1.040834085586084257E-14 ) ) ;
#60036 = CIRCLE ( 'NONE', #146516, 1.600000000000005196 ) ;
#60037 = CARTESIAN_POINT ( 'NONE',  ( 6.699137298928153683, 7.948653282571920720, 1.082531754730549967 ) ) ;
#60038 = CARTESIAN_POINT ( 'NONE',  ( 1.231092510272915552, 2.014232830173094513, 0.09613330637052441840 ) ) ;
#60040 = CARTESIAN_POINT ( 'NONE',  ( 5.371554553765571782, -0.3061699256626281840, 2.039728424269163121 ) ) ;
#60039 = CARTESIAN_POINT ( 'NONE',  ( 9.915090410295563927, 10.46202698829998567, -0.7998128361456281477 ) ) ;
#60041 = FILL_AREA_STYLE_COLOUR ( '', #19622 ) ;
#60042 = CARTESIAN_POINT ( 'NONE',  ( -2.252626078164912560, 5.779814191167667481, 0.7998128361456341429 ) ) ;
#60043 = PRESENTATION_STYLE_ASSIGNMENT (( #56845 ) ) ;
#60044 = CARTESIAN_POINT ( 'NONE',  ( -1.364683531250014514, 1.238541667008091096, -0.7879004041258289570 ) ) ;
#60045 = CARTESIAN_POINT ( 'NONE',  ( 0.3327835722091445070, -1.621720136574826610, 0.7089735832957798634 ) ) ;
#60046 = CARTESIAN_POINT ( 'NONE',  ( 6.152912852923398290, 0.8997199139058277284, 1.482343192998013537 ) ) ;
#60047 = CARTESIAN_POINT ( 'NONE',  ( 5.688919983501732780, 1.323409507385058914, 1.130498143038612513 ) ) ;
#60048 = CARTESIAN_POINT ( 'NONE',  ( 2.665910428807946708, 1.228978066529669899, 1.934933738419620575 ) ) ;
#60049 = CARTESIAN_POINT ( 'NONE',  ( 0.6823417656249864960, -0.5739583329919112353, -1.181850606188749264 ) ) ;
#60050 = CARTESIAN_POINT ( 'NONE',  ( 2.167674216824653222, -1.133089441918342599, 1.451089449600144521 ) ) ;
#60051 = CARTESIAN_POINT ( 'NONE',  ( 9.317477881089539338, 11.89347683273640932, 1.599625672291279388 ) ) ;
#60052 = CARTESIAN_POINT ( 'NONE',  ( -10.71870444596734195, 5.124999999999999112, 5.395310463726811001 ) ) ;
#60053 = CARTESIAN_POINT ( 'NONE',  ( 2.573050890253928635, 0.09191801231544714790, -1.823395950357763695 ) ) ;
#60054 = CARTESIAN_POINT ( 'NONE',  ( 3.815077410725797424, 1.076317812134291119, -1.704938119663282903 ) ) ;
#60055 = CARTESIAN_POINT ( 'NONE',  ( -2.616360457312984167, 5.996244933599686355, -0.7216878364870257245 ) ) ;
#60056 = DIRECTION ( 'NONE',  ( 1.000000000000000000, -0.000000000000000000, 1.224646799147353207E-16 ) ) ;
#60057 = CARTESIAN_POINT ( 'NONE',  ( 4.946364073002400552, 2.100128792357182750, 0.1576013620808654481 ) ) ;
#60058 = CARTESIAN_POINT ( 'NONE',  ( -5.225778143063529946, 8.184159369294361497, 1.199719254218452047 ) ) ;
#60059 = CARTESIAN_POINT ( 'NONE',  ( 10.00008462853139690, 14.27679787173769910, 7.523198333661912152 ) ) ;
#60060 = CARTESIAN_POINT ( 'NONE',  ( 2.049362625460974030, 1.802418521853879962, -1.018503948505583789 ) ) ;
#60061 = CARTESIAN_POINT ( 'NONE',  ( 3.785751206713845018, 5.439795712631356750, 1.599625672291267398 ) ) ;
#60062 = CARTESIAN_POINT ( 'NONE',  ( -2.353626204688216217E-14, 0.1093750003414345612, -1.570758158831782270 ) ) ;
#60063 = CARTESIAN_POINT ( 'NONE',  ( 4.459710115430675081, -1.639780234044617035, -1.344486126324248465 ) ) ;
#60064 = CARTESIAN_POINT ( 'NONE',  ( 1.365712245162364225, 1.898099017218597195, -0.3287360691993664874 ) ) ;
#60065 = ORIENTED_EDGE ( 'NONE', *, *, #154260, .T. ) ;
#60066 = CARTESIAN_POINT ( 'NONE',  ( -3.332271893908731464, 7.109677319527304640, -0.7998128361456481317 ) ) ;
#60067 = CARTESIAN_POINT ( 'NONE',  ( 9.582915646760733708, 10.07448976417602893, 0.7998128361456462443 ) ) ;
#60068 = CARTESIAN_POINT ( 'NONE',  ( 5.356880090730863131, 7.343055753976412525, 1.443375672974064550 ) ) ;
#60069 = CARTESIAN_POINT ( 'NONE',  ( 3.475000000000000533, -0.5104166657107496174, 2.006292185433948827 ) ) ;
#60070 = CARTESIAN_POINT ( 'NONE',  ( -3.893162665418476109, 7.693773542963529444, 1.040834085586084257E-14 ) ) ;
#60071 = CARTESIAN_POINT ( 'NONE',  ( 6.047156637250688860, 0.2094617991648151656, 2.110256208591613003 ) ) ;
#60072 = CARTESIAN_POINT ( 'NONE',  ( 2.766744854014174138, -1.453255750356880371, 1.524405782528108766 ) ) ;
#60073 = CARTESIAN_POINT ( 'NONE',  ( -5.143339171537843590, 7.093924681584509173, 1.599625672291263179 ) ) ;
#60074 = CARTESIAN_POINT ( 'NONE',  ( 8.589254009457354400, 9.979550084910457031, -1.199719254218446718 ) ) ;
#60075 = CARTESIAN_POINT ( 'NONE',  ( 5.998848716047340268, 0.3616406339099677014, 1.825274704766747913 ) ) ;
#60076 = CARTESIAN_POINT ( 'NONE',  ( 8.260995669428309540, 8.532249790621511565, 0.7998128361456481317 ) ) ;
#60077 = CARTESIAN_POINT ( 'NONE',  ( -4.146814880933400005, 5.931313009212638931, 1.599625672291270506 ) ) ;
#60078 = CARTESIAN_POINT ( 'NONE',  ( -9.978437869977950569, 11.70422760547153906, -1.082531754730539753 ) ) ;
#60079 = CARTESIAN_POINT ( 'NONE',  ( 0.1059362375676886209, 1.575662574916199210, 1.419458935296296520 ) ) ;
#60080 = FACE_OUTER_BOUND ( 'NONE', #105441, .T. ) ;
#60082 = CARTESIAN_POINT ( 'NONE',  ( 2.541395235131336694, 1.794889867694851260, -0.7924082849640816661 ) ) ;
#60081 = CARTESIAN_POINT ( 'NONE',  ( -4.356712336337761644E-14, 2.859375000341351392, -1.570758158831810247 ) ) ;
#60083 = CARTESIAN_POINT ( 'NONE',  ( 1.182749364907993206, -2.109161078630458430, -0.4729781282231394490 ) ) ;
#60085 = CARTESIAN_POINT ( 'NONE',  ( -5.926191280687664431, 6.129739482751896062, 0.8152664440823562675 ) ) ;
#60084 = CARTESIAN_POINT ( 'NONE',  ( -5.041653019435350380, 6.975290837464928728, -1.599625672291271394 ) ) ;
#60086 = CARTESIAN_POINT ( 'NONE',  ( -1.402160292154681736E-14, 1.196875000341419026, -1.575800808251659024 ) ) ;
#60087 = CARTESIAN_POINT ( 'NONE',  ( 2.519154997858559231, -1.001672848371559787, -1.422942596517995817 ) ) ;
#60088 = CARTESIAN_POINT ( 'NONE',  ( 6.968527767744104651, 8.192665819532020777, 1.082531754730558626 ) ) ;
#60089 = CARTESIAN_POINT ( 'NONE',  ( -11.68462027884434917, 8.171766027648200037, -4.455682980299036089 ) ) ;
#60090 = EDGE_CURVE ( 'NONE', #138365, #40935, #31610, .T. ) ;
#60091 = AXIS2_PLACEMENT_3D ( 'NONE', #198380, #18571, #86784 ) ;
#60092 = CARTESIAN_POINT ( 'NONE',  ( 2.284529629648517801, -1.956262009633228605, 0.4871271731112236658 ) ) ;
#60093 = CARTESIAN_POINT ( 'NONE',  ( -0.02968770228139669398, 7.629137130509076492, -2.426318643530885222 ) ) ;
#60095 = MECHANICAL_DESIGN_GEOMETRIC_PRESENTATION_REPRESENTATION (  '', ( #91194 ), #49729 ) ;
#60094 = CARTESIAN_POINT ( 'NONE',  ( -5.171509248969888617, 4.998125310078441075, 0.7998128361456281477 ) ) ;
#60096 = CARTESIAN_POINT ( 'NONE',  ( 1.832829291326312005, 0.1914625595707402927, 1.962137882790424559 ) ) ;
#60097 = AXIS2_PLACEMENT_3D ( 'NONE', #36074, #186597, #134688 ) ;
#60099 = CARTESIAN_POINT ( 'NONE',  ( -6.021229618244897885, 7.157760988441397743, 1.082531754730548412 ) ) ;
#60098 = CARTESIAN_POINT ( 'NONE',  ( 5.554919272666569263, 0.3793472168572444292, 1.874222000232607765 ) ) ;
#60100 = CARTESIAN_POINT ( 'NONE',  ( -5.275531169048909952, 7.248148678680751189, -1.443375672974066548 ) ) ;
#60101 = CARTESIAN_POINT ( 'NONE',  ( 6.547661840756936691, 6.603636667163397256, 0.7998128361456352531 ) ) ;
#60102 = EDGE_CURVE ( 'NONE', #124676, #39684, #118243, .T. ) ;
#60103 = CARTESIAN_POINT ( 'NONE',  ( -5.661411662158206681, 8.762674818229999829, -1.199719254218452047 ) ) ;
#60104 = CARTESIAN_POINT ( 'NONE',  ( 1.154951149459724880, 0.3962062163746901677, 1.980246309512444070 ) ) ;
#60105 = FILL_AREA_STYLE_COLOUR ( '', #118455 ) ;
#60106 = CARTESIAN_POINT ( 'NONE',  ( 6.194374175331438082, -2.295634644278636394, -0.2347168956345067892 ) ) ;
#60107 = CARTESIAN_POINT ( 'NONE',  ( 5.793401095800717826, -1.774274828963496198, 0.8374297333502839225 ) ) ;
#60108 = CARTESIAN_POINT ( 'NONE',  ( 3.080854412065773928, 1.845568107317007822, 0.6654098317215583203 ) ) ;
#60109 = CARTESIAN_POINT ( 'NONE',  ( 8.072990401933337168, 11.50590700464255356, -1.199719254218446718 ) ) ;
#60110 = CARTESIAN_POINT ( 'NONE',  ( 0.6861729220449981348, 1.650083401500940239, 1.158686392676591570 ) ) ;
#60111 = ORIENTED_EDGE ( 'NONE', *, *, #187238, .T. ) ;
#60112 = CARTESIAN_POINT ( 'NONE',  ( 1.218125882790439762, 1.038422275552937757, -1.845119264165562711 ) ) ;
#60114 = CARTESIAN_POINT ( 'NONE',  ( -6.073162743917628781, 9.172774736957510555, -1.199719254218440723 ) ) ;
#60113 = CARTESIAN_POINT ( 'NONE',  ( -3.623053363349869382, 5.249981562040033189, 1.599625672291267398 ) ) ;
#60115 = CARTESIAN_POINT ( 'NONE',  ( 1.552429278155377679, -1.578373273985161473, -0.9476568548090894550 ) ) ;
#60116 = ORIENTED_EDGE ( 'NONE', *, *, #42362, .F. ) ;
#60117 = CARTESIAN_POINT ( 'NONE',  ( 11.15024502828561559, 9.129283359492950112, 4.439156027159579132 ) ) ;
#60118 = CARTESIAN_POINT ( 'NONE',  ( 3.006218798242997980, -0.8556837461295877523, 1.940463308995137526 ) ) ;
#60119 = CARTESIAN_POINT ( 'NONE',  ( -0.7500000000000215383, 4.472916667349482012, 1.299038105676671107 ) ) ;
#60120 = CARTESIAN_POINT ( 'NONE',  ( 8.209625708274705502, 9.536650400197368427, 1.199719254218462483 ) ) ;
#60121 = CARTESIAN_POINT ( 'NONE',  ( 5.989670002187236442, 10.20997511251894529, -0.7998128361456481317 ) ) ;
#60122 = CARTESIAN_POINT ( 'NONE',  ( 3.778635366994155032, -1.985013167256908240, -0.5533215937988352762 ) ) ;
#60124 = CARTESIAN_POINT ( 'NONE',  ( 0.6789530235665336422, 1.236279375446739603, 1.364625092910062953 ) ) ;
#60123 = CARTESIAN_POINT ( 'NONE',  ( -8.864333505236459132, 9.236143932397675727, 1.040834085586084257E-14 ) ) ;
#60125 = CARTESIAN_POINT ( 'NONE',  ( -1.364683531250010295, 4.280208333674753618, 0.7879004041258379498 ) ) ;
#60126 = FACE_OUTER_BOUND ( 'NONE', #126371, .T. ) ;
#60127 = CARTESIAN_POINT ( 'NONE',  ( 1.392249819062528537, 4.335314676365917386, 0.1369250707804057221 ) ) ;
#60128 = CARTESIAN_POINT ( 'NONE',  ( 0.8388348947251201837, 2.174866457552121268, 0.3736606161612308630 ) ) ;
#60129 = CARTESIAN_POINT ( 'NONE',  ( 2.108995328314038353, 1.677457623459570168, -1.518302342262042304 ) ) ;
#60130 = CARTESIAN_POINT ( 'NONE',  ( -9.164948653158003111, 9.794787638213568570, -0.7216878364870267237 ) ) ;
#60132 = EDGE_CURVE ( 'NONE', #163314, #135251, #144497, .T. ) ;
#60131 = CARTESIAN_POINT ( 'NONE',  ( 2.724650786558381999, 1.309284593816659736, -1.252271045645783065 ) ) ;
#60133 = CARTESIAN_POINT ( 'NONE',  ( 3.169047557264609072, 1.729775434385946831, -0.8236773211035466336 ) ) ;
#60134 = CARTESIAN_POINT ( 'NONE',  ( 4.510256325466165173, 2.069976601481211542, -0.04757507122059301263 ) ) ;
#60135 = CARTESIAN_POINT ( 'NONE',  ( -1.364683531250000748, 2.321875000341422357, 1.214306433183764966E-14 ) ) ;
#60136 = CARTESIAN_POINT ( 'NONE',  ( 2.746899856880557600, -1.639987585725300123, 1.093844759732710781 ) ) ;
#60137 = CARTESIAN_POINT ( 'NONE',  ( 6.481085492957645577, -0.09751705652460275486, -1.924153034975156995 ) ) ;
#60138 = CARTESIAN_POINT ( 'NONE',  ( 2.992876365407059147, 1.605230647100181596, -0.9602576221170722182 ) ) ;
#60140 = CARTESIAN_POINT ( 'NONE',  ( 4.601768607255383614, 8.481659704624913587, -0.1707596084408805059 ) ) ;
#60139 = CARTESIAN_POINT ( 'NONE',  ( 1.770602872417438967, 1.189155993293121716, 1.977591576486624314 ) ) ;
#60141 = CARTESIAN_POINT ( 'NONE',  ( 4.070637595011177723, 1.317219721392929310, -1.314973792616628945 ) ) ;
#60142 = CARTESIAN_POINT ( 'NONE',  ( -0.6823417656249969321, 3.467708333674754506, -1.181850606188749264 ) ) ;
#60143 = CARTESIAN_POINT ( 'NONE',  ( 6.848098694195379643, -0.8844518680410964340, 1.861345814548149624 ) ) ;
#60144 = CARTESIAN_POINT ( 'NONE',  ( -4.517891501851816649, 6.293959390292322986, -1.599625672291256295 ) ) ;
#60145 = CARTESIAN_POINT ( 'NONE',  ( 5.425234023762710578, 9.481190127698507553, -0.7998128361456291469 ) ) ;
#60146 = CARTESIAN_POINT ( 'NONE',  ( -1.500236433942644609, 3.349270317293938870, -0.06629318219674300294 ) ) ;
#60147 = CARTESIAN_POINT ( 'NONE',  ( 0.6628876427188118425, -1.523960678047535877, 1.453889595790233802 ) ) ;
#60148 = EDGE_CURVE ( 'NONE', #144331, #186972, #152653, .T. ) ;
#60149 = CARTESIAN_POINT ( 'NONE',  ( 0.6823417656249899377, 3.738541667008085767, -1.181850606188754593 ) ) ;
#60150 = CARTESIAN_POINT ( 'NONE',  ( 6.257120919624137301, -1.850417449585840313, -1.117149918570578437 ) ) ;
#60151 = CARTESIAN_POINT ( 'NONE',  ( -0.1052055632086721232, -1.960199907271743314, -0.4866737942672630379 ) ) ;
#60152 = CARTESIAN_POINT ( 'NONE',  ( -0.6823417656250003738, -0.2822916663252489355, -1.181850606188749264 ) ) ;
#60153 = CARTESIAN_POINT ( 'NONE',  ( -4.961921032921567054, 4.891255414604337659, 0.7216878364870317197 ) ) ;
#60154 = EDGE_CURVE ( 'NONE', #149077, #4563, #149245, .T. ) ;
#60157 = CARTESIAN_POINT ( 'NONE',  ( 3.050221373394638835, 6.502416002361635528, 0.000000000000000000 ) ) ;
#60156 = CARTESIAN_POINT ( 'NONE',  ( 6.825078400183553384, 0.5907600490881077526, 1.908621492364571903 ) ) ;
#60155 = CARTESIAN_POINT ( 'NONE',  ( 6.713222337422018349, 7.861122810861019161, -1.199719254218452047 ) ) ;
#60158 =( BOUNDED_CURVE ( )  B_SPLINE_CURVE ( 2, ( #170233, #5565, #205927, #105260, #171301 ),
 .UNSPECIFIED., .F., .T. ) 
 B_SPLINE_CURVE_WITH_KNOTS ( ( 3, 2, 3 ),
 ( 0.000000000000000000, 0.5732952876205078541, 1.000000000000000000 ),
 .UNSPECIFIED. ) 
 CURVE ( )  GEOMETRIC_REPRESENTATION_ITEM ( )  RATIONAL_B_SPLINE_CURVE ( ( 0.9706336853805221931, 0.9832135787375378966, 1.000000000000000000, 0.9875058365010993544, 0.9773420270535906340 ) ) 
 REPRESENTATION_ITEM ( '' )  );
#60159 = CARTESIAN_POINT ( 'NONE',  ( -3.305155586681401303, 7.078041627762083898, 0.7998128361456352531 ) ) ;
#60160 = CARTESIAN_POINT ( 'NONE',  ( 5.050017674172561755, 0.9981218692422781924, 1.752141108012375437 ) ) ;
#60162 = CARTESIAN_POINT ( 'NONE',  ( -6.495764994278840021, 8.671754808115688107, 1.443375672974064550 ) ) ;
#60161 = CARTESIAN_POINT ( 'NONE',  ( -9.246297574839990929, 11.81043314211192019, 1.443375672974076540 ) ) ;
#60163 = APPLICATION_CONTEXT ( 'automotive_design' ) ;
#60165 = CARTESIAN_POINT ( 'NONE',  ( -0.6823417656250039265, 10.06770833367473550, -1.181850606188755259 ) ) ;
#60164 = CARTESIAN_POINT ( 'NONE',  ( 6.455963997168007396, 2.156291961557708525, -0.1537611777119098910 ) ) ;
#60166 = CARTESIAN_POINT ( 'NONE',  ( -8.109748439268576803, 12.61312361245537517, 0.7998128361456481317 ) ) ;
#60168 = CARTESIAN_POINT ( 'NONE',  ( 0.2103571609669597775, 1.833310535235525673, 0.5554914372104239328 ) ) ;
#60167 = CARTESIAN_POINT ( 'NONE',  ( -5.951666246274811556, 7.966696592119163256, 1.443375672974064550 ) ) ;
#60169 = CARTESIAN_POINT ( 'NONE',  ( 1.364683531249986537, 0.4677083336747514530, -0.7879004041258309554 ) ) ;
#60170 = CARTESIAN_POINT ( 'NONE',  ( 0.1833053738655651410, -5.341077028191773657, 10.96562622554680821 ) ) ;
#60171 = FACE_OUTER_BOUND ( 'NONE', #162743, .T. ) ;
#60172 = CARTESIAN_POINT ( 'NONE',  ( 1.646655695949898135, -1.458533453692168358, 0.9204839396419748354 ) ) ;
#60173 = CARTESIAN_POINT ( 'NONE',  ( 7.828907357248368726, 8.098423103070084395, 0.7998128361456281477 ) ) ;
#60174 = CARTESIAN_POINT ( 'NONE',  ( 4.342354338126830804, 8.288106837781779035, -0.7998128361456381397 ) ) ;
#60175 = CARTESIAN_POINT ( 'NONE',  ( -1.364683531250000748, -0.6781249996585803075, 0.000000000000000000 ) ) ;
#60176 = CARTESIAN_POINT ( 'NONE',  ( 0.6492013947936903229, 0.5632195774387914744, -1.677790250104938874 ) ) ;
#60177 = CARTESIAN_POINT ( 'NONE',  ( 1.735022414761304921, 1.879166562360615966, 0.7224556781355166990 ) ) ;
#60178 = CARTESIAN_POINT ( 'NONE',  ( 3.891806949550260519, 1.596497936513015192, 1.523729906679156754 ) ) ;
#60179 = CARTESIAN_POINT ( 'NONE',  ( 4.856392247755495717, -2.170420479375735123, -0.05992511257937349622 ) ) ;
#60180 = ORIENTED_EDGE ( 'NONE', *, *, #23157, .F. ) ;
#60181 = CARTESIAN_POINT ( 'NONE',  ( -1.500000000000013101, -0.3291666666666463459, 0.8660254037844403729 ) ) ;
#60183 = CARTESIAN_POINT ( 'NONE',  ( 2.583611426500436625, -0.6298568260672476882, 1.915607262459443572 ) ) ;
#60182 = CARTESIAN_POINT ( 'NONE',  ( 2.860144583491229131, 0.7611018733697445526, -1.979373954265637892 ) ) ;
#60185 = VERTEX_POINT ( 'NONE', #13979 ) ;
#60184 = CARTESIAN_POINT ( 'NONE',  ( 3.550846374533889183, 0.2710319999918932021, 1.791078082347187683 ) ) ;
#60186 = CARTESIAN_POINT ( 'NONE',  ( 4.877901405866606588, 8.912911750144889567, 0.7998128361456341429 ) ) ;
#60187 = ORIENTED_EDGE ( 'NONE', *, *, #176622, .F. ) ;
#60188 = CARTESIAN_POINT ( 'NONE',  ( 0.7955152940811484052, -0.6771210053572243037, 1.743984199989514927 ) ) ;
#60189 = CARTESIAN_POINT ( 'NONE',  ( 6.173040012923759257, 6.096301524699504704, -0.7998128361456281477 ) ) ;
#60190 = CARTESIAN_POINT ( 'NONE',  ( 6.393173274427864428, 1.585754722747900969, -0.9045919592586546543 ) ) ;
#60192 = CARTESIAN_POINT ( 'NONE',  ( 1.024461926017742996, 0.3770999164835596162, 1.878046770817816791 ) ) ;
#60191 = CARTESIAN_POINT ( 'NONE',  ( -4.274898507010545856, 3.881803101134051470, -0.7998128361456221525 ) ) ;
#60193 = CARTESIAN_POINT ( 'NONE',  ( 0.000000000000000000, 8.999999999999998224, 0.000000000000000000 ) ) ;
#60194 = B_SPLINE_CURVE_WITH_KNOTS ( 'NONE', 3,
 ( #45978, #178102, #112099, #29718, #95800, #161856 ),
 .UNSPECIFIED., .F., .F.,
 ( 4, 2, 4 ),
 ( 0.000000000000000000, 0.0003239988925529259205, 0.0006479977851058518409 ),
 .UNSPECIFIED. ) ;
#60195 = CARTESIAN_POINT ( 'NONE',  ( -1.364683531250000748, 1.821875000341421913, 0.000000000000000000 ) ) ;
#60196 = FACE_OUTER_BOUND ( 'NONE', #124500, .T. ) ;
#60197 = CARTESIAN_POINT ( 'NONE',  ( 5.278265135069068137, -1.204163492603943064, 1.795060720813673738 ) ) ;
#60198 = CARTESIAN_POINT ( 'NONE',  ( -4.746763178560296836, 6.631252689777363152, 1.443375672974058777 ) ) ;
#60199 = CARTESIAN_POINT ( 'NONE',  ( -6.668631453075260396, 8.873432343378178544, -1.599625672291271394 ) ) ;
#60200 = CARTESIAN_POINT ( 'NONE',  ( 2.601940685209406467, 1.502730264585940168, 1.496503045097858697 ) ) ;
#60202 = CARTESIAN_POINT ( 'NONE',  ( -10.99298880388840338, 6.209297407268072888, -6.173882299569079635 ) ) ;
#60201 = CARTESIAN_POINT ( 'NONE',  ( -0.02988540731101250320, 5.726092063503692486, -2.320384613474982594 ) ) ;
#60203 = CARTESIAN_POINT ( 'NONE',  ( 4.587161778375014265, 1.762195453814468182, -0.8837856115832108950 ) ) ;
#60204 = CARTESIAN_POINT ( 'NONE',  ( -0.2106854629475244378, -0.004120941679102134263, -1.996958217618934661 ) ) ;
#60205 = ORIENTED_EDGE ( 'NONE', *, *, #197807, .F. ) ;
#60206 = CARTESIAN_POINT ( 'NONE',  ( 5.454358448847595575, -1.341013495729547644, 1.638584853213326031 ) ) ;
#60207 = PLANE ( 'NONE',  #21397 ) ;
#60208 = CARTESIAN_POINT ( 'NONE',  ( 0.8540665308606997241, -0.7467690478978536994, 1.931163149162813619 ) ) ;
#60209 = CARTESIAN_POINT ( 'NONE',  ( 3.117060223387691398, -1.871409496450952226, 0.5184039432134399661 ) ) ;
#60210 = ORIENTED_EDGE ( 'NONE', *, *, #129019, .T. ) ;
#60211 = CARTESIAN_POINT ( 'NONE',  ( 4.694866332082116678, 8.699370830729650450, 0.7998128361456341429 ) ) ;
#60212 = CARTESIAN_POINT ( 'NONE',  ( 7.361151057576892143, 7.552707420120024828, 0.7998128361456291469 ) ) ;
#60214 = CARTESIAN_POINT ( 'NONE',  ( 6.654354466208897811, 6.657835053532175529, 0.7998128361456341429 ) ) ;
#60213 = CARTESIAN_POINT ( 'NONE',  ( 3.855486427358902013, 2.074851370404519280, -0.2558628111340756628 ) ) ;
#60217 = EDGE_CURVE ( 'NONE', #73782, #110797, #209250, .T. ) ;
#60216 = VECTOR ( 'NONE', #24001, 1000.000000000000000 ) ;
#60215 = CARTESIAN_POINT ( 'NONE',  ( 4.882344714252594642, 4.868692719482363707, 0.000000000000000000 ) ) ;
#60219 = EDGE_LOOP ( 'NONE', ( #125900, #13078, #16346, #55754 ) ) ;
#60218 = CARTESIAN_POINT ( 'NONE',  ( 0.5217373455332212639, -1.802923944912222520, 0.1758665181858156124 ) ) ;
#60220 = CARTESIAN_POINT ( 'NONE',  ( 5.637410271038987730, -1.996576301129053377, 0.9405272304151902629 ) ) ;
#60221 = CARTESIAN_POINT ( 'NONE',  ( -1.020505294851981049E-14, -6.134628647623514119, -10.91970695577493977 ) ) ;
#60222 = CARTESIAN_POINT ( 'NONE',  ( 3.100804818134130780, -0.6391501652806098610, -2.112195066926086273 ) ) ;
#60223 = CARTESIAN_POINT ( 'NONE',  ( -6.138157471807708987, 5.995865026538652387, 1.148737437293850421E-12 ) ) ;
#60224 = CARTESIAN_POINT ( 'NONE',  ( 2.139182944796279351, 0.001596215867826628054, 1.912461472203148771 ) ) ;
#60225 = CARTESIAN_POINT ( 'NONE',  ( 9.772729797352075920, 10.29593960653257234, -0.7998128361456281477 ) ) ;
#60226 = CARTESIAN_POINT ( 'NONE',  ( 5.723117673755029777, -1.870111591731966616, -0.8886290660751752224 ) ) ;
#60228 = CARTESIAN_POINT ( 'NONE',  ( 2.817419395390472037, -0.2130390993498078311, 2.151187356804876050 ) ) ;
#60227 = CARTESIAN_POINT ( 'NONE',  ( 1.517589660447897781, 8.687973171320628296, -2.529458313501610434 ) ) ;
#60229 = CARTESIAN_POINT ( 'NONE',  ( 5.232042516939362287, 2.159042084939459816, 0.3751777721049884273 ) ) ;
#60230 = ORIENTED_EDGE ( 'NONE', *, *, #12290, .T. ) ;
#60231 = DIRECTION ( 'NONE',  ( -0.6507913734559641616, -0.7592566023653004592, 0.000000000000000000 ) ) ;
#60232 = CARTESIAN_POINT ( 'NONE',  ( -15.75000000000000000, 13.39999999999998259, 1.399999999999998579 ) ) ;
#60233 = CARTESIAN_POINT ( 'NONE',  ( -0.006800380015323652903, 7.009756401597622144, 1.999988438675414759 ) ) ;
#60234 = CARTESIAN_POINT ( 'NONE',  ( 3.223806664999388172, 6.983134552466421674, -0.7998128361456362523 ) ) ;
#60235 = CARTESIAN_POINT ( 'NONE',  ( 1.364683531250000303, 15.06770833367473017, -0.7879004041258355073 ) ) ;
#60236 = EDGE_CURVE ( 'NONE', #157004, #24729, #172853, .T. ) ;
#60237 = AXIS2_PLACEMENT_3D ( 'NONE', #121408, #107272, #137590 ) ;
#60238 = CARTESIAN_POINT ( 'NONE',  ( -9.164948653157999559, 10.75515685251491504, -1.082531754730539753 ) ) ;
#60239 = CARTESIAN_POINT ( 'NONE',  ( 4.980641328173811999, 6.904110530993182948, 1.599625672291269396 ) ) ;
#60240 = CARTESIAN_POINT ( 'NONE',  ( 6.280147189154119403, -1.145143509460907039, -1.724508502191648862 ) ) ;
#60241 = CARTESIAN_POINT ( 'NONE',  ( 3.861874329138580197, 1.911805356762337205, -0.2370204922254297297 ) ) ;
#60242 = CARTESIAN_POINT ( 'NONE',  ( 6.362923164919582319, -0.1041218986313949546, -2.114803170081226646 ) ) ;
#60243 = STYLED_ITEM ( 'NONE', ( #59096 ), #185241 ) ;
#60244 = PRESENTATION_STYLE_ASSIGNMENT (( #9365 ) ) ;
#60245 = CARTESIAN_POINT ( 'NONE',  ( 6.308621549060418054, 6.254479983525607523, 0.7998128361456341429 ) ) ;
#60246 = CARTESIAN_POINT ( 'NONE',  ( 1.499999999999996891, 13.14583333333333393, -0.8660254037844378194 ) ) ;
#60247 = CARTESIAN_POINT ( 'NONE',  ( 4.926587155384105188, -1.289601243782242834, 1.488548236191704177 ) ) ;
#60248 = CARTESIAN_POINT ( 'NONE',  ( 0.2170718473699268514, -0.1031819972749977166, 2.189145592210713698 ) ) ;
#60249 = CARTESIAN_POINT ( 'NONE',  ( 4.336427269025699971, 1.790907886515300085, 0.3537760332646966432 ) ) ;
#60250 = EDGE_CURVE ( 'NONE', #27864, #189856, #136794, .T. ) ;
#60251 = CARTESIAN_POINT ( 'NONE',  ( 6.943184063974162434, 9.193743722760251202, -1.443375672974064550 ) ) ;
#60252 = CARTESIAN_POINT ( 'NONE',  ( 2.697709378994964879, 6.091152008895348580, 0.7216878364870338292 ) ) ;
#60253 = CARTESIAN_POINT ( 'NONE',  ( -6.794571259104023930, 7.956029886156682274, 1.199719254218452047 ) ) ;
#60254 = CARTESIAN_POINT ( 'NONE',  ( 5.337069745634900997, 6.255611453776062980, 1.199719254218452047 ) ) ;
#60255 = VERTEX_POINT ( 'NONE', #165586 ) ;
#60257 = CARTESIAN_POINT ( 'NONE',  ( 5.238544184099147571, 1.195677241517135281, -1.619561112405358827 ) ) ;
#60256 = CARTESIAN_POINT ( 'NONE',  ( 2.665370095338463585, 0.9869154847663293983, 1.554228294351194473 ) ) ;
#60258 = CARTESIAN_POINT ( 'NONE',  ( 1.107258645251009144, 0.9300933289658299685, -2.101954592823534362 ) ) ;
#60259 = CARTESIAN_POINT ( 'NONE',  ( 5.823093080589802462, -1.771997608643091304, -0.8420800316405114838 ) ) ;
#60260 = CARTESIAN_POINT ( 'NONE',  ( -6.579784621333750749, 6.570836901177822931, 0.7998128361456341429 ) ) ;
#60261 = CARTESIAN_POINT ( 'NONE',  ( -4.118112554246268431, 7.605586660457912984, -0.5892100532764152909 ) ) ;
#60262 = CARTESIAN_POINT ( 'NONE',  ( -4.406563619641430840, 5.099744630125142564, -1.199719254218446718 ) ) ;
#60263 = CARTESIAN_POINT ( 'NONE',  ( 0.4497787391488928810, 1.533077660697563793, 1.391591089521776681 ) ) ;
#60264 = CARTESIAN_POINT ( 'NONE',  ( -5.483346782084204563, 5.361935765378481378, 0.000000000000000000 ) ) ;
#60266 = CARTESIAN_POINT ( 'NONE',  ( 0.1626889888870358680, -1.668787113083155305, -0.8454427722031019332 ) ) ;
#60265 = CARTESIAN_POINT ( 'NONE',  ( 1.681308932615958041, 1.444198878393717411, 1.512019500502481018 ) ) ;
#60267 = CARTESIAN_POINT ( 'NONE',  ( -8.923337013803626760, 2.630042260599928294, -8.023366178422991268 ) ) ;
#60268 = VERTEX_POINT ( 'NONE', #69124 ) ;
#60269 = CARTESIAN_POINT ( 'NONE',  ( -0.1102773484823963285, 5.719690680991945442, -2.797532285072940272 ) ) ;
#60270 = CARTESIAN_POINT ( 'NONE',  ( 1.803882474592255258, 1.289405681850508190, -1.169162514946599174 ) ) ;
#60271 = CARTESIAN_POINT ( 'NONE',  ( 4.299907273828439180, 8.168308919441841454, 1.040834085586084257E-14 ) ) ;
#60273 = CARTESIAN_POINT ( 'NONE',  ( 1.545144449789729091, 8.695096949162934408, 2.507961912884413280 ) ) ;
#60272 = CARTESIAN_POINT ( 'NONE',  ( -11.43209210103587914, 13.65596075983916080, -3.649125173352125273 ) ) ;
#60274 = CARTESIAN_POINT ( 'NONE',  ( 2.648709078547459850, -1.434216206362935564, 0.9578970732360950757 ) ) ;
#60275 = CARTESIAN_POINT ( 'NONE',  ( 2.911879292414458309, -1.082406496695037301, -1.905547650945007776 ) ) ;
#60276 = CARTESIAN_POINT ( 'NONE',  ( 5.690102719724574598, -0.9953569382129350274, 1.969734210959340093 ) ) ;
#60277 = CARTESIAN_POINT ( 'NONE',  ( -10.76260246389097297, 4.190717020667873882, -6.707086991120802644 ) ) ;
#60278 = CARTESIAN_POINT ( 'NONE',  ( 2.940461416894753377, -1.119856305176626821, 1.859859765203975890 ) ) ;
#60279 = CARTESIAN_POINT ( 'NONE',  ( 0.6623940301842005107, -1.324425631624454036, 1.256838194884236204 ) ) ;
#60280 = CARTESIAN_POINT ( 'NONE',  ( 3.626253288856711610, 2.107507776945900524, 0.2035006255925037866 ) ) ;
#60281 = CARTESIAN_POINT ( 'NONE',  ( 6.639320575229278099, 1.279659970127836388, 2.012538313910294807 ) ) ;
#60282 = VERTEX_POINT ( 'NONE', #134187 ) ;
#60284 = CARTESIAN_POINT ( 'NONE',  ( -0.6823417656250212460, 1.113541667008083325, 1.181850606188755259 ) ) ;
#60283 = CARTESIAN_POINT ( 'NONE',  ( 3.861076399890978283, 0.2801353988391065419, -2.275111823818583456 ) ) ;
#60285 = CARTESIAN_POINT ( 'NONE',  ( 4.867540842506059562, 5.637551390133895168, -1.199719254218452047 ) ) ;
#60286 = CARTESIAN_POINT ( 'NONE',  ( 6.252596820807392319, 2.196675488376065744, 0.3289990992049235397 ) ) ;
#60287 = CARTESIAN_POINT ( 'NONE',  ( -6.480434237652138663, 8.583592582059388576, 1.443375672974078761 ) ) ;
#60288 = EDGE_CURVE ( 'NONE', #181670, #91753, #101653, .T. ) ;
#60289 = CARTESIAN_POINT ( 'NONE',  ( 5.016153647376217606, 4.954526798134778254, 0.7216878364870317197 ) ) ;
#60290 = CARTESIAN_POINT ( 'NONE',  ( -5.680503174001480637, 9.571078103069643461, 0.7216878364870458196 ) ) ;
#60291 = CARTESIAN_POINT ( 'NONE',  ( 0.000000000000000000, 19.00000000000000000, -12.00000000000000178 ) ) ;
#60292 = VECTOR ( 'NONE', #56384, 1000.000000000000000 ) ;
#60293 = ORIENTED_EDGE ( 'NONE', *, *, #27811, .T. ) ;
#60294 = CARTESIAN_POINT ( 'NONE',  ( 4.360000113718985659, -0.002809843368253156070, -2.016597020062675050 ) ) ;
#60296 = CARTESIAN_POINT ( 'NONE',  ( 2.448158969691970555, -0.8859891528392377369, 1.862743816677481679 ) ) ;
#60295 = CARTESIAN_POINT ( 'NONE',  ( 6.810273232766058449, 6.839740281182199233, 1.040834085586084257E-14 ) ) ;
#60297 = CARTESIAN_POINT ( 'NONE',  ( -3.004347502343385212, 6.455130793263525568, -0.4817541042819983854 ) ) ;
#60298 = CARTESIAN_POINT ( 'NONE',  ( 3.892599500454941630, 6.595097612955829192, 1.082531754730549078 ) ) ;
#60299 = CARTESIAN_POINT ( 'NONE',  ( 1.642778471875000035, -3.026041666188708401, -2.845375778867859751 ) ) ;
#60300 = CARTESIAN_POINT ( 'NONE',  ( 1.364683531249990311, 4.613541667008083103, 0.7879004041258500513 ) ) ;
#60301 = CARTESIAN_POINT ( 'NONE',  ( 5.279302027902110339, 1.469929824498400039, 1.625505876179579534 ) ) ;
#60302 = CARTESIAN_POINT ( 'NONE',  ( 3.692029868468839737, 1.730865839653324079, 1.034166058993556181 ) ) ;
#60303 = CARTESIAN_POINT ( 'NONE',  ( 1.997363575765517485, -1.840834563946552649, 0.04656924640939614363 ) ) ;
#60304 = CARTESIAN_POINT ( 'NONE',  ( 7.318703993278529829, 7.432909501780090800, 1.040834085586084257E-14 ) ) ;
#60305 = CARTESIAN_POINT ( 'NONE',  ( 6.774438514930277933, -1.120217847261167243, 1.442041797927499980 ) ) ;
#60306 = CARTESIAN_POINT ( 'NONE',  ( -6.226218857173722476, 8.287007971501239467, 1.599625672291283607 ) ) ;
#60308 = CARTESIAN_POINT ( 'NONE',  ( -5.167592825464113915, 6.057888380243431570, 1.199719254218452935 ) ) ;
#60307 = CARTESIAN_POINT ( 'NONE',  ( 5.594667793837476033, -0.5436135106791986082, -2.196135934016548052 ) ) ;
#60309 = CARTESIAN_POINT ( 'NONE',  ( 1.453890484719716492, 0.6100395758942640523, -2.015780296659912985 ) ) ;
#60310 = CARTESIAN_POINT ( 'NONE',  ( -6.947627372360122955, 7.070263120700404968, 0.000000000000000000 ) ) ;
#60311 = CARTESIAN_POINT ( 'NONE',  ( 8.158255747121103241, 10.54105100977322174, 1.599625672291281386 ) ) ;
#60312 = CARTESIAN_POINT ( 'NONE',  ( 0.000000000000000000, 0.2000000000000057288, 8.300000000000000711 ) ) ;
#60313 = CARTESIAN_POINT ( 'NONE',  ( -8.213542131780492639, 8.476887330032372603, 1.040834085586084257E-14 ) ) ;
#60314 = CARTESIAN_POINT ( 'NONE',  ( 3.215772567386471437, 6.427315425527130088, -0.8732430475888957044 ) ) ;
#60315 = EDGE_CURVE ( 'NONE', #127879, #183272, #2477, .T. ) ;
#60316 = CARTESIAN_POINT ( 'NONE',  ( 7.904040366642699489, 8.323727970612377902, 0.7216878364870458196 ) ) ;
#60317 = CARTESIAN_POINT ( 'NONE',  ( 4.202513864555980305, 7.333163887849894813, -0.8510647575735978965 ) ) ;
#60318 = CARTESIAN_POINT ( 'NONE',  ( -8.188761592974040937, 11.53701037756964887, -1.082531754730543971 ) ) ;
#60319 = CARTESIAN_POINT ( 'NONE',  ( 2.461440635673370014, -1.844245817859784031, 1.238046099332066108 ) ) ;
#60320 = CARTESIAN_POINT ( 'NONE',  ( 0.7157882511714327434, -0.3199875008889854766, 2.183444778895065941 ) ) ;
#60321 = CARTESIAN_POINT ( 'NONE',  ( -6.608673532018475960, 6.674816973635147477, -0.7998128361456362523 ) ) ;
#60322 = CARTESIAN_POINT ( 'NONE',  ( 6.148786358997489820, 7.132337826040578754, -1.199719254218446718 ) ) ;
#60323 = CARTESIAN_POINT ( 'NONE',  ( 3.965250677406896962, 1.681448970545707855, 1.010551734412237446 ) ) ;
#60324 = CARTESIAN_POINT ( 'NONE',  ( 7.865701674222579598, 12.32840238656838139, -0.7998128361456352531 ) ) ;
#60325 = CARTESIAN_POINT ( 'NONE',  ( -4.511607644515479798, 7.038970647229928268, 1.150300019105324978 ) ) ;
#60326 = CARTESIAN_POINT ( 'NONE',  ( 2.198393463710220264, 5.716542807637226886, 0.7998128361456462443 ) ) ;
#60327 = CARTESIAN_POINT ( 'NONE',  ( 0.6823417656249899377, 0.8427083336747520637, 1.181850606188755259 ) ) ;
#60328 = CARTESIAN_POINT ( 'NONE',  ( -5.641601317062248988, 6.714861303728305586, -1.082531754730549967 ) ) ;
#60330 = ORIENTED_EDGE ( 'NONE', *, *, #19714, .T. ) ;
#60329 = CARTESIAN_POINT ( 'NONE',  ( -5.368665641331555882, 8.246898433986675769, 1.082531754730548412 ) ) ;
#60331 = CARTESIAN_POINT ( 'NONE',  ( 3.058948843759463188, 0.5191580478346514704, 2.055925682384197373 ) ) ;
#60332 = CARTESIAN_POINT ( 'NONE',  ( -4.990283058281743678, 7.979691447040783814, -1.199719254218453823 ) ) ;
#60333 = CARTESIAN_POINT ( 'NONE',  ( 3.942369626403975147, 2.151062187213080623, 0.2142938780915065733 ) ) ;
#60334 = CARTESIAN_POINT ( 'NONE',  ( 4.247483403459266782, 1.840758003770435414, -0.04960325993209198370 ) ) ;
#60335 = CARTESIAN_POINT ( 'NONE',  ( -5.227141986104622440, 6.445127484965264664, 1.169998774669118946 ) ) ;
#60336 = CARTESIAN_POINT ( 'NONE',  ( 1.364683531249988757, 0.4468750003414206917, 0.000000000000000000 ) ) ;
#60337 = EDGE_CURVE ( 'NONE', #170914, #24109, #36642, .T. ) ;
#60338 = CARTESIAN_POINT ( 'NONE',  ( 5.718645868333249283, -0.03627580822302550745, 1.740135244698801431 ) ) ;
#60339 = CARTESIAN_POINT ( 'NONE',  ( 6.727182134110196721, 2.084960209934753284, 2.120171393779949565 ) ) ;
#60340 = CARTESIAN_POINT ( 'NONE',  ( 2.901081683644319842, 5.368050483351580304, 1.082531754730548412 ) ) ;
#60341 = CARTESIAN_POINT ( 'NONE',  ( 11.99988598803232875, 6.571561536565357464, 0.5026004568578228415 ) ) ;
#60342 = CARTESIAN_POINT ( 'NONE',  ( 3.292016909520224743, -0.8776455207864016783, 1.975710135277891633 ) ) ;
#60343 = CARTESIAN_POINT ( 'NONE',  ( 5.817732461567613811, -1.591073081590412830, 1.238133459405404757 ) ) ;
#60344 = CARTESIAN_POINT ( 'NONE',  ( -9.314088342463968218, 9.968783942403868892, 0.7216878364870438212 ) ) ;
#60345 = CARTESIAN_POINT ( 'NONE',  ( 2.676834871759771417, -2.068302492614528365, -0.6285112194897370941 ) ) ;
#60346 = CARTESIAN_POINT ( 'NONE',  ( 4.182859841474963147, -0.1902271694152017079, -1.962134583082324024 ) ) ;
#60347 = CARTESIAN_POINT ( 'NONE',  ( 0.08191350661116909848, -1.027414926483052326, 1.935800647029708443 ) ) ;
#60348 = CARTESIAN_POINT ( 'NONE',  ( 0.8687466845767909396, 1.140460243972157395, 2.005982166855703852 ) ) ;
#60349 = CARTESIAN_POINT ( 'NONE',  ( 4.722180519508206054, 1.859554500701779745, 0.5601121866093302648 ) ) ;
#60352 = VERTEX_POINT ( 'NONE', #180764 ) ;
#60351 = LINE ( 'NONE', #161067, #42753 ) ;
#60350 = CARTESIAN_POINT ( 'NONE',  ( -9.137832345486311070, 9.763151945929928743, 1.040834085586084257E-14 ) ) ;
#60353 = CARTESIAN_POINT ( 'NONE',  ( -5.769876891067536206, 8.889217585290882795, 1.199719254218454489 ) ) ;
#60354 = CARTESIAN_POINT ( 'NONE',  ( -11.92619526913700057, 12.57218333338755123, 1.328859060402684644 ) ) ;
#60355 = ADVANCED_FACE ( 'NONE', ( #32392 ), #111295, .T. ) ;
#60357 = ORIENTED_EDGE ( 'NONE', *, *, #80161, .T. ) ;
#60356 = CARTESIAN_POINT ( 'NONE',  ( -4.145761110728687804, 8.058748072483927771, -0.7998128361456481317 ) ) ;
#60358 = CARTESIAN_POINT ( 'NONE',  ( -8.988692655735990300, 9.589155641221221771, 0.7216878364870438212 ) ) ;
#60359 = CARTESIAN_POINT ( 'NONE',  ( 1.817678338065799704, -0.2697497798337232244, 2.190168480848574628 ) ) ;
#60360 = CARTESIAN_POINT ( 'NONE',  ( 0.000000000000000000, -1.946874999522044014, -3.793834371823813001 ) ) ;
#60361 = CARTESIAN_POINT ( 'NONE',  ( 6.789906393989944888, -1.279003670332454989, -1.487618534420580119 ) ) ;
#60362 = CARTESIAN_POINT ( 'NONE',  ( 1.364683531249988535, 4.967708333674756283, -0.7879004041258300672 ) ) ;
#60363 = CARTESIAN_POINT ( 'NONE',  ( 1.499999999999990896, 3.806250000682819046, 1.214306433183764966E-14 ) ) ;
#60364 = CARTESIAN_POINT ( 'NONE',  ( 4.877963630130927264, 6.902327454639943127, -1.420620101560632342 ) ) ;
#60366 = CARTESIAN_POINT ( 'NONE',  ( -5.179808110042967151, 6.342388681160900710, -1.197525655462832406 ) ) ;
#60365 = CARTESIAN_POINT ( 'NONE',  ( 6.021229617800532452, 6.197391773621639288, 0.000000000000000000 ) ) ;
#60367 = CARTESIAN_POINT ( 'NONE',  ( 5.578019757025042047, -1.797138167560994759, -0.3993771437491022702 ) ) ;
#60368 = ORIENTED_EDGE ( 'NONE', *, *, #140315, .F. ) ;
#60369 = CARTESIAN_POINT ( 'NONE',  ( -1.360316468750006225, -0.3593749996585737794, -1.734723475976807094E-15 ) ) ;
#60370 = CARTESIAN_POINT ( 'NONE',  ( -6.509886312855995172, 10.74661779830734254, -0.7998128361456291469 ) ) ;
#60371 = LINE ( 'NONE', #48418, #72290 ) ;
#60372 = CARTESIAN_POINT ( 'NONE',  ( 6.011998765391792787, -0.7129019540204998284, 1.997330473063135381 ) ) ;
#60373 = CARTESIAN_POINT ( 'NONE',  ( -2.540289672789929121, -0.3621416576072680749, -0.2590487051680252506 ) ) ;
#60374 = CARTESIAN_POINT ( 'NONE',  ( 6.010342169559767633, 5.906487374108181143, -0.7998128361456281477 ) ) ;
#60375 = CARTESIAN_POINT ( 'NONE',  ( 0.2685257609614790097, -1.346659848514593305, 1.560126313484144545 ) ) ;
#60378 = CARTESIAN_POINT ( 'NONE',  ( 4.862772069579198941, 0.1752732939881325724, -1.832877676746891726 ) ) ;
#60377 = CARTESIAN_POINT ( 'NONE',  ( 2.400643840759258740, 0.4042734059873221986, 1.816444493264858906 ) ) ;
#60376 = CARTESIAN_POINT ( 'NONE',  ( -10.29981080141455685, 4.865373709629901455, 6.164441567520336562 ) ) ;
#60379 = CARTESIAN_POINT ( 'NONE',  ( 7.983053520348166288, 8.207983950027992748, -0.7998128361456281477 ) ) ;
#60380 = CARTESIAN_POINT ( 'NONE',  ( -4.911709678547487634, 4.704967246051090513, 0.3769511059573752432 ) ) ;
#60381 = CARTESIAN_POINT ( 'NONE',  ( -6.577640801285370209, 7.702944352034914566, -1.199719254218452047 ) ) ;
#60383 = ORIENTED_EDGE ( 'NONE', *, *, #135546, .F. ) ;
#60382 = CARTESIAN_POINT ( 'NONE',  ( -6.758184431511294221, -6.900108348305955097, -6.825879202496253129 ) ) ;
#60384 = CARTESIAN_POINT ( 'NONE',  ( 4.213639274598267370, -0.3785452818781535611, 2.174016619501429215 ) ) ;
#60385 = CARTESIAN_POINT ( 'NONE',  ( 6.573497657123517079, 2.167905964706399846, -0.6471699410235329797 ) ) ;
#60386 = CARTESIAN_POINT ( 'NONE',  ( -4.921246572080546500, 8.685278734161874681, 1.214306433183764966E-14 ) ) ;
#60387 = CARTESIAN_POINT ( 'NONE',  ( 5.607607993782223410, 1.377354484090735243, 1.176896650239395603 ) ) ;
#60388 = CARTESIAN_POINT ( 'NONE',  ( 5.981633625760849782, -0.6386546108097415075, 1.806296054365429393 ) ) ;
#60389 = CARTESIAN_POINT ( 'NONE',  ( 4.000000000000012434, 5.999999999999998224, 0.7500000000000006661 ) ) ;
#60390 = CARTESIAN_POINT ( 'NONE',  ( 6.819227946136852125, -0.1326586024288610444, 1.840611662119538749 ) ) ;
#60391 = CARTESIAN_POINT ( 'NONE',  ( 5.180287844241702189, 0.9460499258955605839, 1.661804969971327983 ) ) ;
#60392 =( NAMED_UNIT ( * ) PLANE_ANGLE_UNIT ( ) SI_UNIT ( $, .RADIAN. ) );
#60393 = AXIS2_PLACEMENT_3D ( 'NONE', #136726, #187585, #203816 ) ;
#60394 = CARTESIAN_POINT ( 'NONE',  ( 0.1978467685152424937, -1.870139902624564865, -0.05068021481659244765 ) ) ;
#60395 = CARTESIAN_POINT ( 'NONE',  ( 2.712125330650519750, 1.116209241849321465, -1.679223868463100011 ) ) ;
#60397 = CARTESIAN_POINT ( 'NONE',  ( 3.844438321715905715, 2.095922912919225389, 0.2063985846082766473 ) ) ;
#60396 = CARTESIAN_POINT ( 'NONE',  ( -8.455481356417053007, 13.01647868246193518, 0.7998128361456341429 ) ) ;
#60398 = PRESENTATION_LAYER_ASSIGNMENT (  '', '', ( #133108 ) ) ;
#60399 = EDGE_CURVE ( 'NONE', #127447, #93714, #138915, .T. ) ;
#60400 = CARTESIAN_POINT ( 'NONE',  ( 9.935427640716063991, 10.48575375712389679, -0.7998128361456281477 ) ) ;
#60402 = CARTESIAN_POINT ( 'NONE',  ( -7.395082721250053837, 10.71501471051202614, -1.199719254218446718 ) ) ;
#60401 = CARTESIAN_POINT ( 'NONE',  ( 1.499999999999987566, -0.7249999999999825473, 0.000000000000000000 ) ) ;
#60403 = CARTESIAN_POINT ( 'NONE',  ( 3.058857861556500968, 0.4949273143410140574, 1.958058250343613693 ) ) ;
#60404 = B_SPLINE_CURVE_WITH_KNOTS ( 'NONE', 1,
 ( #2326, #104136 ),
 .UNSPECIFIED., .F., .F.,
 ( 2, 2 ),
 ( 0.2143153648627418029, 0.6378831769527100182 ),
 .UNSPECIFIED. ) ;
#60405 = CARTESIAN_POINT ( 'NONE',  ( -1.364683531250012516, 2.988541667008091096, -0.7879004041258289570 ) ) ;
#60406 = ADVANCED_FACE ( 'NONE', ( #98458, #181817 ), #150421, .F. ) ;
#60407 = CARTESIAN_POINT ( 'NONE',  ( 2.198393463710220264, 5.716542807637226886, 0.7998128361456462443 ) ) ;
#60408 = CARTESIAN_POINT ( 'NONE',  ( 3.919328646192806520, -0.1633067429045453600, 2.155504054270485970 ) ) ;
#60409 = CARTESIAN_POINT ( 'NONE',  ( -3.475000000000000533, -1.735416665710752149, -2.006292185433948827 ) ) ;
#60410 = CARTESIAN_POINT ( 'NONE',  ( -1.500000000000011324, 5.379166666666692187, -0.8660254037844313801 ) ) ;
#60412 = CARTESIAN_POINT ( 'NONE',  ( 3.469446951953614189E-15, 5.227586206896610577, 1.214306433183764966E-14 ) ) ;
#60411 = CARTESIAN_POINT ( 'NONE',  ( 6.505933609711257226, 8.683618192786854095, -1.599625672291281386 ) ) ;
#60413 = CARTESIAN_POINT ( 'NONE',  ( 8.148087131688683371, 10.52918762510205042, -1.443375672974063439 ) ) ;
#60415 = CARTESIAN_POINT ( 'NONE',  ( 9.218433053458319648, 14.16038166358193884, -7.683070978493945269 ) ) ;
#60414 = CARTESIAN_POINT ( 'NONE',  ( 1.610090671168771470, 0.6309225058772853778, -2.077463247357013820 ) ) ;
#60416 = TOROIDAL_SURFACE ( 'NONE', #25776, 12.18000000000000149, 0.5000000000000008882 ) ;
#60418 = CARTESIAN_POINT ( 'NONE',  ( 0.7668492355173107677, 1.774547462407764842, -0.4907661837717376407 ) ) ;
#60417 = CARTESIAN_POINT ( 'NONE',  ( -7.239690840017442675, 7.548653522882887934, 0.7216878364870317197 ) ) ;
#60419 = CARTESIAN_POINT ( 'NONE',  ( -1.201851678989727383E-14, 2.071875000341422801, 1.575800808251672791 ) ) ;
#60420 = CARTESIAN_POINT ( 'NONE',  ( 2.033021410476544943, -1.955939774129427988, 0.9887309579383956049 ) ) ;
#60421 = CARTESIAN_POINT ( 'NONE',  ( 6.883263157960358924, 4.692138088316172073, 2.616388454592593504 ) ) ;
#60422 = CARTESIAN_POINT ( 'NONE',  ( 2.782378429719241986, -1.163933448739282062, 1.940043740367594305 ) ) ;
#60423 = CARTESIAN_POINT ( 'NONE',  ( -6.073162743917628781, 9.172774736957510555, -1.199719254218440723 ) ) ;
#60424 = CARTESIAN_POINT ( 'NONE',  ( -0.6823417656249969321, 4.530208333674755394, -1.181850606188749264 ) ) ;
#60425 = CARTESIAN_POINT ( 'NONE',  ( 6.059270238282111087, 7.038290852966752276, 1.014332888565868229 ) ) ;
#60426 = CARTESIAN_POINT ( 'NONE',  ( 0.7500000000000006661, 12.33333333333333570, 1.299038105676657340 ) ) ;
#60427 = CARTESIAN_POINT ( 'NONE',  ( 5.560252395380206103, 8.540692657035327429, 1.082531754730547524 ) ) ;
#60428 = CARTESIAN_POINT ( 'NONE',  ( 4.727684277059563733, -1.088367244632810094, -1.395429379651995649 ) ) ;
#60429 = CARTESIAN_POINT ( 'NONE',  ( 7.886038904643079661, 12.35212915539230139, -0.7998128361456352531 ) ) ;
#60430 = CARTESIAN_POINT ( 'NONE',  ( 0.7101633350218137242, -2.095805943121428427, 0.2063731196077517871 ) ) ;
#60432 = CARTESIAN_POINT ( 'NONE',  ( 1.499999999999987121, 0.7958333333333510451, -0.8660254037844253849 ) ) ;
#60431 = CARTESIAN_POINT ( 'NONE',  ( 0.6823417656249934904, 10.69270833367473550, 1.181850606188764807 ) ) ;
#60433 = CARTESIAN_POINT ( 'NONE',  ( -3.962726036944197894, 7.845207153068690431, -0.7998128361456481317 ) ) ;
#60434 = CARTESIAN_POINT ( 'NONE',  ( 6.204703874486805049, 1.882480396761162744, 0.7231267579426368108 ) ) ;
#60436 = ORIENTED_EDGE ( 'NONE', *, *, #64698, .F. ) ;
#60435 = CARTESIAN_POINT ( 'NONE',  ( 5.080233222017616512, 0.8995743074830947483, 1.572398339973365422 ) ) ;
#60437 = CARTESIAN_POINT ( 'NONE',  ( 10.23370702021670020, 10.83374636654133383, 0.7998128361456462443 ) ) ;
#60438 = CARTESIAN_POINT ( 'NONE',  ( 3.731198135974967300, -1.728734619261709682, 0.7151963084984153118 ) ) ;
#60439 = CARTESIAN_POINT ( 'NONE',  ( 4.504778988403771223, 0.5471568804141565545, 1.996604337080605474 ) ) ;
#60440 = CARTESIAN_POINT ( 'NONE',  ( -5.600926855776882540, 8.588146194164741232, -1.082531754730549967 ) ) ;
#60442 = COLOUR_RGB ( '', 0.08235294, 0.09019608, 0.10196078) ;
#60441 = CARTESIAN_POINT ( 'NONE',  ( -2.788906526875773208E-15, 10.71875000068279604, -1.499999999999998446 ) ) ;
#60443 = CARTESIAN_POINT ( 'NONE',  ( 9.413438726589914651, 9.876766690643398405, 0.000000000000000000 ) ) ;
#60444 = CARTESIAN_POINT ( 'NONE',  ( -1.517589660447928868, 8.687973171320628296, 2.529458313501630418 ) ) ;
#60445 = CARTESIAN_POINT ( 'NONE',  ( 5.671053392266061977, 9.838255734277600695, 0.7998128361456331437 ) ) ;
#60446 = CARTESIAN_POINT ( 'NONE',  ( 0.000000000000000000, 4.500000000000003553, 0.000000000000000000 ) ) ;
#60447 = CARTESIAN_POINT ( 'NONE',  ( 1.364683531249986537, -0.8447916663252468261, -0.7879004041258309554 ) ) ;
#60448 = CIRCLE ( 'NONE', #5223, 11.95586206896558146 ) ;
#60449 = CARTESIAN_POINT ( 'NONE',  ( 3.683996026499200660, -1.166640140252427793, -1.577160851978461009 ) ) ;
#60450 = CARTESIAN_POINT ( 'NONE',  ( 0.5442957877539145173, 1.882187304385819493, -0.7230256762977352869 ) ) ;
#60451 = CARTESIAN_POINT ( 'NONE',  ( -4.821859908315634158, 5.654533310236863564, 1.199719254218452935 ) ) ;
#60453 = CARTESIAN_POINT ( 'NONE',  ( -2.680963302752292332, 0.4788041664876945269, -8.638326563840810896E-32 ) ) ;
#60452 = CARTESIAN_POINT ( 'NONE',  ( 7.425061681778431399, 11.81432239538354345, 0.7998128361456462443 ) ) ;
#60454 = CARTESIAN_POINT ( 'NONE',  ( 1.282252794574537447, -1.823689378192733912, -0.4153219600965887826 ) ) ;
#60455 = CARTESIAN_POINT ( 'NONE',  ( -1.001543065824772872E-14, 4.321875000341417916, 1.575800808251672791 ) ) ;
#60456 = CARTESIAN_POINT ( 'NONE',  ( 3.551042609437846220, 0.2996916850201857829, 1.990680017358969600 ) ) ;
#60458 = CARTESIAN_POINT ( 'NONE',  ( 3.884452219389774363, -0.6659801820031689967, -2.009805269316313314 ) ) ;
#60457 = CARTESIAN_POINT ( 'NONE',  ( -5.585596099150191840, 7.539614753807099667, -1.443375672974052559 ) ) ;
#60459 = CARTESIAN_POINT ( 'NONE',  ( 5.639828713160493834, 5.682147708216442439, 1.040834085586084257E-14 ) ) ;
#60460 = CARTESIAN_POINT ( 'NONE',  ( 4.721179655770254335, -1.847879960204744432, -0.9338546512941485744 ) ) ;
#60461 = CARTESIAN_POINT ( 'NONE',  ( 3.923105346307896202, 5.670318552149568703, -1.599625672291269396 ) ) ;
#60463 = CARTESIAN_POINT ( 'NONE',  ( 3.029357257649615054, 5.621668336311468117, -1.199719254218446718 ) ) ;
#60462 = CARTESIAN_POINT ( 'NONE',  ( 6.667919252303131650, -1.287369299672879830, 1.647753151290908047 ) ) ;
#60465 = ORIENTED_EDGE ( 'NONE', *, *, #204199, .T. ) ;
#60464 = CARTESIAN_POINT ( 'NONE',  ( 4.823181420811452291, -0.08861582515604787824, 1.823562061424352621 ) ) ;
#60466 = CARTESIAN_POINT ( 'NONE',  ( 7.065770611016287006, 11.39514947949436774, 1.040834085586084257E-14 ) ) ;
#60467 = DIRECTION ( 'NONE',  ( 0.000000000000000000, 0.000000000000000000, -1.000000000000000000 ) ) ;
#60468 = CARTESIAN_POINT ( 'NONE',  ( 10.28744933574984799, 12.75976789843056203, -6.941907919544356709 ) ) ;
#60469 = CARTESIAN_POINT ( 'NONE',  ( 6.686557766011572923, -2.162873314485185272, -0.4371622687903350957 ) ) ;
#60470 = CARTESIAN_POINT ( 'NONE',  ( -0.6823417656250003738, 12.21354166700806765, 1.181850606188754593 ) ) ;
#60471 = CARTESIAN_POINT ( 'NONE',  ( 5.109976026518994630, -0.6845719981980763480, 1.785733525123212928 ) ) ;
#60472 = CARTESIAN_POINT ( 'NONE',  ( -7.862839020921525091, 11.26073039346208660, -1.199719254218446718 ) ) ;
#60473 = CARTESIAN_POINT ( 'NONE',  ( 5.307127064745490230, 8.279066444590018392, -1.199719254218452935 ) ) ;
#60474 = CARTESIAN_POINT ( 'NONE',  ( 1.360316468749961594, 2.817708333674743049, -0.7853790794159141164 ) ) ;
#60475 = CARTESIAN_POINT ( 'NONE',  ( 9.531438498077132948, -8.057097448493882652, -0.1980946632348720704 ) ) ;
#60476 = CARTESIAN_POINT ( 'NONE',  ( 5.332434488876471868, 5.115595079977664383, 0.7998128361456341429 ) ) ;
#60477 = ORIENTED_EDGE ( 'NONE', *, *, #132683, .F. ) ;
#60478 = CARTESIAN_POINT ( 'NONE',  ( -7.099629715411508890, 8.311931418515415615, 1.199719254218452047 ) ) ;
#60479 = CARTESIAN_POINT ( 'NONE',  ( -0.02299388927988389730, 6.948790505698306141, -2.506045543530223352 ) ) ;
#60480 = CARTESIAN_POINT ( 'NONE',  ( 5.006703865196457492, 9.063181286029688977, 0.000000000000000000 ) ) ;
#60481 = CARTESIAN_POINT ( 'NONE',  ( 3.050221373394638835, 6.502416002361635528, 0.000000000000000000 ) ) ;
#60482 = CIRCLE ( 'NONE', #91613, 0.8299999999999999600 ) ;
#60483 = CARTESIAN_POINT ( 'NONE',  ( 0.1394461523057136665, 2.058909413595513715, -2.136561586061051621 ) ) ;
#60484 = CARTESIAN_POINT ( 'NONE',  ( -4.744990575102892905, 8.479646737687938085, 0.7216878364870458196 ) ) ;
#60485 = CARTESIAN_POINT ( 'NONE',  ( 3.551346171775753735, 6.230655402791975384, 1.199719254218462483 ) ) ;
#60486 = CARTESIAN_POINT ( 'NONE',  ( 2.764455286864405004, -0.7492524419267130309, -1.821560881719074709 ) ) ;
#60487 = CARTESIAN_POINT ( 'NONE',  ( 3.515250061227533696, -1.862011288300661871, 0.7743320027404425598 ) ) ;
#60488 = CARTESIAN_POINT ( 'NONE',  ( -7.477485413136760073, 8.682486722536401302, -1.199719254218446718 ) ) ;
#60489 = CARTESIAN_POINT ( 'NONE',  ( 5.825163275726873202, 6.825053905550038991, 1.199719254218452047 ) ) ;
#60490 = CARTESIAN_POINT ( 'NONE',  ( 6.727182134110234024, 7.051482179251418181, 2.887205776801844426 ) ) ;
#60491 = CARTESIAN_POINT ( 'NONE',  ( 3.275498427308475069, 1.390425696708731396, 1.693851754907250928 ) ) ;
#60492 = CARTESIAN_POINT ( 'NONE',  ( 1.817283056450700318, -0.2383884500203499179, 1.911531453543861225 ) ) ;
#60493 = CARTESIAN_POINT ( 'NONE',  ( -8.779068160048691283, 10.20099992726700933, -1.199719254218446718 ) ) ;
#60494 = DIRECTION ( 'NONE',  ( 0.000000000000000000, -1.000000000000000000, 0.000000000000000000 ) ) ;
#60495 = CARTESIAN_POINT ( 'NONE',  ( 0.1329588055935760349, 6.948069629093068578, -2.440977959956799115 ) ) ;
#60496 = CARTESIAN_POINT ( 'NONE',  ( 3.268924434670684498, 6.827845917175511481, -1.734723475976807094E-15 ) ) ;
#60497 = CARTESIAN_POINT ( 'NONE',  ( 8.633844893804129228, 8.967240552393299424, -0.7998128361456211532 ) ) ;
#60498 = CARTESIAN_POINT ( 'NONE',  ( 4.473300617505036492, 7.306268922809479704, -1.199719254218452047 ) ) ;
#60499 = CYLINDRICAL_SURFACE ( 'NONE', #5106, 4.500000000000000000 ) ;
#60500 = CARTESIAN_POINT ( 'NONE',  ( 6.373741612200174878, 6.608655767087927124, 0.7216878364870328300 ) ) ;
#60501 = ORIENTED_EDGE ( 'NONE', *, *, #129048, .F. ) ;
#60503 = CARTESIAN_POINT ( 'NONE',  ( 3.053387886640859694, -1.774279702891886190, 0.9510675200815300601 ) ) ;
#60502 = CARTESIAN_POINT ( 'NONE',  ( 6.110883706712432861, -0.2185277653131960651, 1.828168259763853776 ) ) ;
#60504 = CARTESIAN_POINT ( 'NONE',  ( 4.552342272275657464, 2.055464322635578878, -1.028527531867760914 ) ) ;
#60506 = CARTESIAN_POINT ( 'NONE',  ( 1.832617572280154539, -1.765004919984759058, -0.5899526775028116621 ) ) ;
#60505 = CARTESIAN_POINT ( 'NONE',  ( -0.1288028175206725467, 0.2223783146117243037, -2.307352578052775272 ) ) ;
#60507 = CARTESIAN_POINT ( 'NONE',  ( -1.642778471875000035, -2.617708332855375186, -2.845375778867859751 ) ) ;
#60508 = CARTESIAN_POINT ( 'NONE',  ( -10.95308175811721085, 12.30000000000000071, -1.800000000000001155 ) ) ;
#60509 = CARTESIAN_POINT ( 'NONE',  ( 6.469012471580376733, -1.473683540339595810, 1.218514635347216046 ) ) ;
#60510 = CARTESIAN_POINT ( 'NONE',  ( -7.857113714319432063, 9.125386407249497012, 1.199719254218462483 ) ) ;
#60511 = CARTESIAN_POINT ( 'NONE',  ( -5.316205630334255972, 8.255971431148344308, -1.082531754730549967 ) ) ;
#60513 = CARTESIAN_POINT ( 'NONE',  ( 3.186256133050053840, -1.842714570631575510, -0.3211874441736498054 ) ) ;
#60512 = CARTESIAN_POINT ( 'NONE',  ( 4.985920054561153059, -2.075123007882358817, -0.2543892858761549469 ) ) ;
#60514 = CARTESIAN_POINT ( 'NONE',  ( 7.470179451449751262, 7.817556902887268677, 1.040834085586084257E-14 ) ) ;
#60515 = VERTEX_POINT ( 'NONE', #68049 ) ;
#60516 = EDGE_CURVE ( 'NONE', #201330, #204988, #167855, .T. ) ;
#60517 = CARTESIAN_POINT ( 'NONE',  ( 2.975337776247584998, 6.515577267086843705, -0.5540753762497061530 ) ) ;
#60518 = CARTESIAN_POINT ( 'NONE',  ( -3.782361668532609134, 7.356579680022602652, 1.040834085586084257E-14 ) ) ;
#60519 = CARTESIAN_POINT ( 'NONE',  ( 6.199779612253428773, -0.5740575353240050527, 1.626695425327763678 ) ) ;
#60520 = CARTESIAN_POINT ( 'NONE',  ( -4.550733115681270036, 8.460939068270139529, 0.7998128361456481317 ) ) ;
#60521 = CARTESIAN_POINT ( 'NONE',  ( 1.810757103121255707, 0.9981641815470091439, -1.417837687506792621 ) ) ;
#60522 = CARTESIAN_POINT ( 'NONE',  ( -1.992711204631002198E-15, 2.999999999999989342, 1.224999999999989875 ) ) ;
#60523 = CYLINDRICAL_SURFACE ( 'NONE', #112420, 0.4000000000000001332 ) ;
#60524 = CARTESIAN_POINT ( 'NONE',  ( -1.249999999999966471, 8.500000000000000000, 9.921567416492214520 ) ) ;
#60525 = CARTESIAN_POINT ( 'NONE',  ( 6.262575984712966282, -0.7736541179628317888, -2.028742479192620518 ) ) ;
#60526 = CARTESIAN_POINT ( 'NONE',  ( 4.652862234063231739, -1.464609733205827879, 1.089778014065109657 ) ) ;
#60527 = CARTESIAN_POINT ( 'NONE',  ( 2.782025223480470544, -1.125517505138178942, -1.606590762409945583 ) ) ;
#60528 = CARTESIAN_POINT ( 'NONE',  ( 6.350787976822619640, -1.936633936377421206, -0.8562603515115329023 ) ) ;
#60529 = EDGE_CURVE ( 'NONE', #181670, #170139, #166566, .T. ) ;
#60530 = DIRECTION ( 'NONE',  ( 5.551115123125764829E-17, 0.000000000000000000, -1.000000000000000000 ) ) ;
#60531 = CARTESIAN_POINT ( 'NONE',  ( -8.482597663644387609, 13.04811437422715414, -0.7998128361456281477 ) ) ;
#60532 = CARTESIAN_POINT ( 'NONE',  ( 6.916630921265960019, 11.22115317478565188, 0.7998128361456462443 ) ) ;
#60533 = CARTESIAN_POINT ( 'NONE',  ( 3.000754678503589012, -2.089479603458433754, -0.3603616953608209661 ) ) ;
#60534 = CARTESIAN_POINT ( 'NONE',  ( -0.3000000000000103140, 3.322650755865456773, 0.5865692111442551981 ) ) ;
#60535 = ADVANCED_FACE ( 'NONE', ( #149339 ), #66986, .T. ) ;
#60536 = CARTESIAN_POINT ( 'NONE',  ( -4.567562471335953944, 6.984949105684680859, -1.180336305634868577 ) ) ;
#60537 =( BOUNDED_CURVE ( )  B_SPLINE_CURVE ( 2, ( #152756, #155967, #170063, #36860, #4339, #203610, #56330, #37945, #153833 ),
 .UNSPECIFIED., .F., .T. ) 
 B_SPLINE_CURVE_WITH_KNOTS ( ( 3, 2, 2, 2, 3 ),
 ( 0.5625000000000000000, 0.5694444444444444198, 0.5833333333333333703, 0.5972222222222222099, 0.6041666666666667407 ),
 .UNSPECIFIED. ) 
 CURVE ( )  GEOMETRIC_REPRESENTATION_ITEM ( )  RATIONAL_B_SPLINE_CURVE ( ( 0.9330127018922194093, 0.9330127018922194093, 1.000000000000000000, 0.8660254037844387076, 1.000000000000000000, 0.8660254037844387076, 1.000000000000000000, 0.9330127018922187432, 0.9330127018922192983 ) ) 
 REPRESENTATION_ITEM ( '' )  );
#60538 = CARTESIAN_POINT ( 'NONE',  ( 0.2509399751232620490, -0.4509356589572112162, -2.027996233343106081 ) ) ;
#60540 = CARTESIAN_POINT ( 'NONE',  ( -6.009258394948636914E-15, 13.96875000068279782, -1.732050807568875195 ) ) ;
#60539 = CARTESIAN_POINT ( 'NONE',  ( -10.84194200455609725, 4.687741901903320851, 5.144714966584626126 ) ) ;
#60543 = ORIENTED_EDGE ( 'NONE', *, *, #94600, .T. ) ;
#60542 = CARTESIAN_POINT ( 'NONE',  ( 3.053626115265011709, -1.958026000861570415, 1.048987487942198094 ) ) ;
#60541 = COLOUR_RGB ( '', 0.09019608, 0.27058824, 0.51372549) ;
#60544 = CARTESIAN_POINT ( 'NONE',  ( 0.8799778958844242105, -0.5652253508772618895, -2.228020342328890901 ) ) ;
#60546 = CARTESIAN_POINT ( 'NONE',  ( 5.418824339757763120, -1.497735668165665723, 1.418348116948890736 ) ) ;
#60545 = CARTESIAN_POINT ( 'NONE',  ( 3.521367211247359741, 5.131347717920458962, -1.599625672291262513 ) ) ;
#60548 = CARTESIAN_POINT ( 'NONE',  ( -3.475000000000000533, -1.049999999999998934, 0.000000000000000000 ) ) ;
#60547 = CARTESIAN_POINT ( 'NONE',  ( 5.415556014015861841, 5.282846535965431300, -0.7998128361456481317 ) ) ;
#60549 = CYLINDRICAL_SURFACE ( 'NONE', #23312, 0.07999999999999998779 ) ;
#60550 = CARTESIAN_POINT ( 'NONE',  ( 5.618664544990171095, -0.03892770779775727580, 1.841008343696965310 ) ) ;
#60551 = DIRECTION ( 'NONE',  ( -0.000000000000000000, 0.000000000000000000, -1.000000000000000000 ) ) ;
#60552 = CARTESIAN_POINT ( 'NONE',  ( -0.1102773484824301209, 0.2280386113255315761, -2.237141580442712829 ) ) ;
#60553 = CARTESIAN_POINT ( 'NONE',  ( 3.153030191819999217, -1.409141575680799230, -0.9942448187586181430 ) ) ;
#60554 = CARTESIAN_POINT ( 'NONE',  ( 1.745327705122714956, 0.3399549603602426417, -1.987498286102694411 ) ) ;
#60555 = CARTESIAN_POINT ( 'NONE',  ( 3.375889859521400194, -0.4501408176796182770, -2.254053602989118499 ) ) ;
#60556 =( BOUNDED_CURVE ( )  B_SPLINE_CURVE ( 2, ( #19222, #99427, #82091, #150321, #166557, #83155, #85300, #51749, #84233, #809, #165481, #151386, #185987, #36542, #52799, #116794, #134092, #67947, #37621, #17077, #182791, #65813, #102629, #4022, #100481, #149235, #2956, #135144, #53878, #201160, #118938, #50668, #86374, #214185, #33345, #103701, #133022, #152443, #70091, #34409, #131960, #136206, #202224, #169752, #148184, #49601, #115725, #199021, #24556, #90663, #39763, #105868, #171894, #123243, #91740, #58143, #156725, #139409, #109098, #137277, #23491, #189207, #205443, #89597, #154585, #38696, #106953, #59200, #190261, #206512, #56012, #73307, #155647, #125357, #104774, #122165, #174055, #203297, #170823, #54944, #57079, #7230, #40845, #207580, #172977, #8316, #204355, #74401, #153516, #187063, #191320, #88523, #140501, #124302, #188132, #71160, #41919, #108030, #121096, #22414, #25628, #157793, #9389, #75460, #141573, #42987, #21340, #87448, #5085, #6162, #72231, #138338, #210781, #128567, #194532, #208636, #158846, #176174, #97068, #26700, #80797, #145832, #76515 ),
 .UNSPECIFIED., .F., .T. ) 
 B_SPLINE_CURVE_WITH_KNOTS ( ( 3, 2, 2, 2, 2, 2, 2, 2, 2, 2, 2, 2, 2, 2, 2, 2, 2, 2, 2, 2, 2, 2, 2, 2, 2, 2, 2, 2, 2, 2, 2, 2, 2, 2, 2, 2, 2, 2, 2, 2, 2, 2, 2, 2, 2, 2, 2, 2, 2, 2, 2, 2, 2, 2, 2, 2, 2, 2, 2, 2, 2, 3 ),
 ( 0.000000000000000000, 0.005952380952380951183, 0.01190476190476190237, 0.01785714285714285615, 0.02380952380952380473, 0.02976190476190476372, 0.03571428571428571230, 0.04166666666666666435, 0.04761904761904760947, 0.05357142857142857539, 0.05952380952380952744, 0.06547619047619047949, 0.07142857142857142461, 0.07738095238095238360, 0.08333333333333332871, 0.08928571428571428770, 0.09523809523809521893, 0.1011904761904761918, 0.1071428571428571508, 0.1130952380952380959, 0.1190476190476190549, 0.1250000000000000000, 0.1309523809523809590, 0.1369047619047619180, 0.1428571428571428492, 0.1488095238095238082, 0.1547619047619047672, 0.1607142857142857262, 0.1666666666666666574, 0.1726190476190476164, 0.1785714285714285754, 0.1845238095238095621, 0.1904761904761904379, 0.1964285714285714246, 0.2023809523809523836, 0.2083333333333333703, 0.2142857142857143016, 0.2202380952380952328, 0.2261904761904761918, 0.2321428571428571785, 0.2380952380952381098, 0.2440476190476190410, 0.2500000000000000000, 0.2559523809523809312, 0.2619047619047619180, 0.2678571428571428492, 0.2738095238095238360, 0.2797619047619047672, 0.2857142857142856984, 0.2916666666666666852, 0.2976190476190476164, 0.3035714285714285476, 0.3095238095238095344, 0.3154761904761904656, 0.3214285714285714524, 0.3273809523809523836, 0.3333333333333333148, 0.3392857142857143016, 0.3452380952380952328, 0.3511904761904762196, 0.3571428571428571508, 0.3602579105411656268 ),
 .UNSPECIFIED. ) 
 CURVE ( )  GEOMETRIC_REPRESENTATION_ITEM ( )  RATIONAL_B_SPLINE_CURVE ( ( 1.000000000000000000, 0.8660254037844387076, 1.000000000000000000, 0.8660254037844387076, 1.000000000000000000, 0.8660254037844387076, 1.000000000000000000, 0.8660254037844387076, 1.000000000000000000, 0.8660254037844387076, 1.000000000000000000, 0.8660254037844387076, 1.000000000000000000, 0.8660254037844387076, 1.000000000000000000, 0.8660254037844387076, 1.000000000000000000, 0.8660254037844387076, 1.000000000000000000, 0.8660254037844387076, 1.000000000000000000, 0.8660254037844387076, 1.000000000000000000, 0.8660254037844387076, 1.000000000000000000, 0.8660254037844387076, 1.000000000000000000, 0.8660254037844387076, 1.000000000000000000, 0.8660254037844387076, 1.000000000000000000, 0.8660254037844387076, 1.000000000000000000, 0.8660254037844387076, 1.000000000000000000, 0.8660254037844387076, 1.000000000000000000, 0.8660254037844387076, 1.000000000000000000, 0.8660254037844387076, 1.000000000000000000, 0.8660254037844387076, 1.000000000000000000, 0.8660254037844387076, 1.000000000000000000, 0.8660254037844387076, 1.000000000000000000, 0.8660254037844387076, 1.000000000000000000, 0.8660254037844387076, 1.000000000000000000, 0.8660254037844387076, 1.000000000000000000, 0.8660254037844387076, 1.000000000000000000, 0.8660254037844387076, 1.000000000000000000, 0.8660254037844387076, 1.000000000000000000, 0.8660254037844387076, 1.000000000000000000, 0.8660254037844387076, 1.000000000000000000, 0.8660254037844387076, 1.000000000000000000, 0.8660254037844387076, 1.000000000000000000, 0.8660254037844387076, 1.000000000000000000, 0.8660254037844387076, 1.000000000000000000, 0.8660254037844387076, 1.000000000000000000, 0.8660254037844387076, 1.000000000000000000, 0.8660254037844387076, 1.000000000000000000, 0.8660254037844387076, 1.000000000000000000, 0.8660254037844387076, 1.000000000000000000, 0.8660254037844387076, 1.000000000000000000, 0.8660254037844387076, 1.000000000000000000, 0.8660254037844387076, 1.000000000000000000, 0.8660254037844387076, 1.000000000000000000, 0.8660254037844387076, 1.000000000000000000, 0.8660254037844387076, 1.000000000000000000, 0.8660254037844387076, 1.000000000000000000, 0.8660254037844387076, 1.000000000000000000, 0.8660254037844387076, 1.000000000000000000, 0.8660254037844387076, 1.000000000000000000, 0.8660254037844387076, 1.000000000000000000, 0.8660254037844387076, 1.000000000000000000, 0.8660254037844387076, 1.000000000000000000, 0.8660254037844387076, 1.000000000000000000, 0.8660254037844387076, 1.000000000000000000, 0.8660254037844387076, 1.000000000000000000, 0.8660254037844387076, 1.000000000000000000, 0.8660254037844387076, 1.000000000000000000, 0.8660254037844387076, 1.000000000000000000, 0.8660254037844387076, 1.000000000000000000, 0.9298872124336470257, 0.9331585307975728272 ) ) 
 REPRESENTATION_ITEM ( '' )  );
#60557 = CARTESIAN_POINT ( 'NONE',  ( 2.653932422735814978, 0.6056841677779849498, -2.179737047031413244 ) ) ;
#60558 = CARTESIAN_POINT ( 'NONE',  ( 5.619784395276031574, -2.055015178219528948, 0.4601488667864346849 ) ) ;
#60559 = CARTESIAN_POINT ( 'NONE',  ( -7.268579750702168774, 7.652633595340216921, -0.7216878364870338292 ) ) ;
#60560 = CARTESIAN_POINT ( 'NONE',  ( 4.077242326343363032, 1.667005924876462597, -0.5946135600440533020 ) ) ;
#60562 = CARTESIAN_POINT ( 'NONE',  ( 6.356980026238091774, 0.3966049396831958229, -2.257653707126358267 ) ) ;
#60561 = CARTESIAN_POINT ( 'NONE',  ( 4.923019175093585886, 5.876515471431535076, -1.082531754730548412 ) ) ;
#60563 = CARTESIAN_POINT ( 'NONE',  ( 4.171694865975253741, -1.058263924308279424, 1.506412014522513720 ) ) ;
#60564 = CARTESIAN_POINT ( 'NONE',  ( -5.461236948206312114, 5.265864615862458464, 0.7998128361456341429 ) ) ;
#60565 = CARTESIAN_POINT ( 'NONE',  ( 6.277061933002788585, 6.425586464699131639, 0.7216878364870317197 ) ) ;
#60566 = CARTESIAN_POINT ( 'NONE',  ( 0.7499999999999902300, 3.733333333333352488, 1.299038105676669330 ) ) ;
#60567 = CARTESIAN_POINT ( 'NONE',  ( 4.910206770677443266, 1.512653250323254817, -1.585896273577400484 ) ) ;
#60568 = CARTESIAN_POINT ( 'NONE',  ( -5.759516327706961647, 5.613857225279885732, -0.7998128361456221525 ) ) ;
#60569 = CARTESIAN_POINT ( 'NONE',  ( 0.1479172090190853939, 8.281400213891396689, -2.000566733410582554 ) ) ;
#60570 =( BOUNDED_CURVE ( )  B_SPLINE_CURVE ( 2, ( #102835, #20494, #56215, #173184, #156930, #136415, #72442 ),
 .UNSPECIFIED., .F., .T. ) 
 B_SPLINE_CURVE_WITH_KNOTS ( ( 3, 2, 2, 3 ),
 ( 0.2000000000000000944, 0.2041666666666667185, 0.2083333333333333981, 0.2125000000000000222 ),
 .UNSPECIFIED. ) 
 CURVE ( )  GEOMETRIC_REPRESENTATION_ITEM ( )  RATIONAL_B_SPLINE_CURVE ( ( 0.9999999999999973355, 0.8660254037844413721, 1.000000000000000000, 0.8660254037844387076, 1.000000000000000000, 0.8660254037844378194, 1.000000000000000888 ) ) 
 REPRESENTATION_ITEM ( '' )  );
#60571 = CARTESIAN_POINT ( 'NONE',  ( 5.266107318980479235, -2.060723932065291031, 0.1993833602659672022 ) ) ;
#60572 = CARTESIAN_POINT ( 'NONE',  ( 0.2863426850727782136, -0.6839425765656822476, -1.897108587135355684 ) ) ;
#60573 = CARTESIAN_POINT ( 'NONE',  ( 0.6823417656249917140, 4.592708333674755394, 1.181850606188765695 ) ) ;
#60574 = CARTESIAN_POINT ( 'NONE',  ( 3.246621724073412096, 0.4685524532376301177, 1.868535087029847386 ) ) ;
#60575 = CARTESIAN_POINT ( 'NONE',  ( -0.6823417656250003738, 9.651041667008065872, 1.181850606188754593 ) ) ;
#60577 = CARTESIAN_POINT ( 'NONE',  ( -2.765500147507697459, 5.209872024525476597, 1.082531754730560403 ) ) ;
#60576 = MECHANICAL_DESIGN_GEOMETRIC_PRESENTATION_REPRESENTATION (  '', ( #153990 ), #12036 ) ;
#60578 = CARTESIAN_POINT ( 'NONE',  ( 0.05339833992625257070, 0.3882609103176749010, 2.187096328411592516 ) ) ;
#60579 = ORIENTED_EDGE ( 'NONE', *, *, #35402, .F. ) ;
#60581 = FACE_OUTER_BOUND ( 'NONE', #197364, .T. ) ;
#60580 = CARTESIAN_POINT ( 'NONE',  ( -4.556949027968976829, 5.449433633119473264, 1.082531754730549078 ) ) ;
#60582 = CARTESIAN_POINT ( 'NONE',  ( 4.813308228051395687, 5.574280006603454574, 1.199719254218462483 ) ) ;
#60583 = CARTESIAN_POINT ( 'NONE',  ( 7.876942567271134621, -5.350481869465718354, -7.629869294364563181 ) ) ;
#60584 = PRESENTATION_STYLE_ASSIGNMENT (( #194852 ) ) ;
#60585 = CARTESIAN_POINT ( 'NONE',  ( 4.905139262582266291, 4.827437033166341429, 0.6004564335717228474 ) ) ;
#60586 = CARTESIAN_POINT ( 'NONE',  ( -5.060975816087005974, 7.500583322029065414, -1.217465846647723282 ) ) ;
#60587 = CARTESIAN_POINT ( 'NONE',  ( 1.803102349535959714, -1.659081995624330563, 1.046767247423967095 ) ) ;
#60588 = CARTESIAN_POINT ( 'NONE',  ( -0.6823417656250003738, 0.7802083336747520637, -1.181850606188749264 ) ) ;
#60589 = CARTESIAN_POINT ( 'NONE',  ( 6.420800710400103917, 2.015122584031241004, 0.7829223626853940576 ) ) ;
#60590 = CARTESIAN_POINT ( 'NONE',  ( 5.494571831323358246, 1.932540981948445147, 0.3370517209014682325 ) ) ;
#60591 = CARTESIAN_POINT ( 'NONE',  ( -10.29471871147821282, 10.90492667301307605, -0.7998128361456291469 ) ) ;
#60592 = CARTESIAN_POINT ( 'NONE',  ( -6.683806541412780078, 6.900121841177441873, -0.7216878364870267237 ) ) ;
#60593 = CARTESIAN_POINT ( 'NONE',  ( 5.752838164830007983, -1.706859214253673152, 1.326403591387192771 ) ) ;
#60595 = VERTEX_POINT ( 'NONE', #100585 ) ;
#60594 = CARTESIAN_POINT ( 'NONE',  ( -0.1178541238725513418, -5.389012432655349016, -10.99948089704805199 ) ) ;
#60596 = CARTESIAN_POINT ( 'NONE',  ( -0.6823417656250212460, 4.051041667008085767, 1.181850606188767472 ) ) ;
#60597 = CARTESIAN_POINT ( 'NONE',  ( 6.802032592820894230, -1.970958832386409565, 0.04617810802716794394 ) ) ;
#60598 = CARTESIAN_POINT ( 'NONE',  ( 6.626334403847231158, 0.2915952204957816263, -1.708955668912811587 ) ) ;
#60600 = CARTESIAN_POINT ( 'NONE',  ( 3.614928802375876771, -0.1595779646587774658, 2.185787688459623901 ) ) ;
#60599 = CARTESIAN_POINT ( 'NONE',  ( -1.360316468750046859, 0.6197916670081009549, -0.7853790794159322131 ) ) ;
#60601 = CARTESIAN_POINT ( 'NONE',  ( 4.770747201329826659, -1.511217855519477293, 1.743977600800976857 ) ) ;
#60602 = CARTESIAN_POINT ( 'NONE',  ( 5.852824474907069252, -1.627199953678662991, 1.264450640605979892 ) ) ;
#60603 = CARTESIAN_POINT ( 'NONE',  ( 1.077954490650166575, -1.894526023430597617, -0.4258829084243920260 ) ) ;
#60604 = CARTESIAN_POINT ( 'NONE',  ( -6.033015167956805591, 8.061603667414825480, -1.443375672974058777 ) ) ;
#60605 = AXIS2_PLACEMENT_3D ( 'NONE', #143948, #78883, #145006 ) ;
#60606 = DIRECTION ( 'NONE',  ( 0.000000000000000000, 1.000000000000000000, 0.000000000000000000 ) ) ;
#60607 = EDGE_CURVE ( 'NONE', #50335, #159873, #166659, .T. ) ;
#60608 = CARTESIAN_POINT ( 'NONE',  ( 4.605793411009856619, 1.573235607984494688, 1.422142093439874522 ) ) ;
#60609 = PRESENTATION_STYLE_ASSIGNMENT (( #28114 ) ) ;
#60610 = CARTESIAN_POINT ( 'NONE',  ( 2.215470409936692420, 1.956561601830292485, 0.4872017847364697452 ) ) ;
#60611 = CARTESIAN_POINT ( 'NONE',  ( -4.731432421044873493, 7.503459676985569260, -1.082531754730548412 ) ) ;
#60612 = CARTESIAN_POINT ( 'NONE',  ( 5.614374367772542840, -0.9875226594672004143, -1.973556357105679115 ) ) ;
#60613 = CARTESIAN_POINT ( 'NONE',  ( -7.632314129850253259, 7.869064337772231355, 0.7998128361456341429 ) ) ;
#60614 = CARTESIAN_POINT ( 'NONE',  ( 0.3776192402222087741, 3.049641483663570352, -0.4287046358292833648 ) ) ;
#60615 = CARTESIAN_POINT ( 'NONE',  ( 0.3108172448005979138, 1.586703044182024458, 0.9029097728878652251 ) ) ;
#60616 = CARTESIAN_POINT ( 'NONE',  ( -6.882699257592852504, 8.058845884393651460, -1.199719254218452047 ) ) ;
#60617 = CARTESIAN_POINT ( 'NONE',  ( -4.681723370323557454, 8.380211346474826684, 0.6239904028470877329 ) ) ;
#60618 = CARTESIAN_POINT ( 'NONE',  ( -9.587704862635016312, 4.026159954882873926, 6.671158199369250141 ) ) ;
#60619 = VERTEX_POINT ( 'NONE', #21437 ) ;
#60620 = CARTESIAN_POINT ( 'NONE',  ( 5.418845456765190249, 1.903306360667684993, 0.7908678518537788360 ) ) ;
#60621 = DIRECTION ( 'NONE',  ( 3.347138415753903010E-16, 0.6000000000000018652, -0.7999999999999984901 ) ) ;
#60622 = CARTESIAN_POINT ( 'NONE',  ( 0.1520312049661921572, -8.104757123234346494, 9.499050059654537748 ) ) ;
#60623 = CARTESIAN_POINT ( 'NONE',  ( -2.578021764892882040, 6.159442492350315490, 0.7998128361456341429 ) ) ;
#60624 = CARTESIAN_POINT ( 'NONE',  ( -3.546339698426324460, 6.295090860542775779, -1.199719254218450271 ) ) ;
#60625 = CARTESIAN_POINT ( 'NONE',  ( 4.529947673531667718, -1.980263497020241292, 0.3961197999026391248 ) ) ;
#60626 = CARTESIAN_POINT ( 'NONE',  ( -0.7500000000000006661, 1.108333333333356929, -1.299038105676652011 ) ) ;
#60628 = CARTESIAN_POINT ( 'NONE',  ( 8.107412671292022921, 12.40247251657532956, 0.7216878364870438212 ) ) ;
#60627 = CARTESIAN_POINT ( 'NONE',  ( -4.411198876399886615, 6.239761003923544713, -1.599625672291271394 ) ) ;
#60629 = CARTESIAN_POINT ( 'NONE',  ( 7.253775878511261155, 8.421492265473332850, 1.199719254218462483 ) ) ;
#60630 = CARTESIAN_POINT ( 'NONE',  ( 4.223548136977580469, -1.972658117897459151, 0.5965803236557595257 ) ) ;
#60631 = CARTESIAN_POINT ( 'NONE',  ( 2.971327447312217540, -1.987046587055636859, -0.3419355124290661685 ) ) ;
#60632 = ORIENTED_EDGE ( 'NONE', *, *, #176386, .F. ) ;
#60633 = CARTESIAN_POINT ( 'NONE',  ( 1.904329973710251034, 3.286760881231379106, -0.4119279214153375723 ) ) ;
#60634 = CARTESIAN_POINT ( 'NONE',  ( 3.897079088924235712, 6.634010472798538949, 1.199719254218462483 ) ) ;
#60635 =( BOUNDED_SURFACE ( )  B_SPLINE_SURFACE ( 1, 2, ( 
 ( #28943, #129727, #93966, #192486, #179465, #11608, #45211, #10539, #76613, #61436, #146981, #97162, #26793, #79812, #209800, #111326, #176268, #44138, #126525, #145924, #177329, #210873, #48412, #31090, #211936, #46273, #114524, #92898, #62498, #110259, #128663, #95027, #112389, #194631, #208735, #160007, #158944, #96097, #178401, #161077, #78742, #60362, #63571, #143803, #195711, #47346, #127602, #27870, #163217, #113460, #14800, #142726, #80891, #212998, #64635, #130774, #196769, #213163, #46433, #129889, #97325, #148200, #116809, #162312, #33361, #114688, #130937, #128814, #146082, #13897, #196930, #83170, #16021, #96260, #78904, #79979, #30171, #164435, #195873, #17092, #12830, #145026, #113624, #179628, #212094, #149254, #197987, #99443, #211030, #48568, #62656, #63730, #65830, #64793, #199036, #214200, #47512, #133037, #31249, #180680, #115740, #165499, #131979, #194796, #112551, #181730, #178562, #827, #14955, #163381, #81053, #66897, #147137, #32305, #49615, #98372, #82107, #50684, #161243, #182809, #34426, #137294, #136220, #117887, #134107, #103716, #202240, #102645, #53892, #168701, #54962, #21357, #85319, #121114, #187079, #52816, #38712, #169767, #183880, #200116, #151402, #35492, #101570, #4038, #138356, #2974, #87463, #154601, #69042, #118954, #167637, #100499, #84250, #20305, #19239, #135159, #150336, #122183, #184933, #201178, #120027, #36557, #86390, #152458, #166575, #153531, #71176, #70107, #186003, #104792, #37638, #5100, #67963, #203312, #170838, #22429, #88539, #6180, #72248, #18162, #204373, #56030, #188149, #1904, #51767, #11531, #108047, #43002, #125373, #10459, #7247, #175129, #93888, #92818, #76532, #127521, #171911, #190277, #89613, #207596, #26716, #75477, #74417, #110180, #209717, #105886, #141589, #140516, #124318, #189224, #109115, #8332, #156742, #158862, #59215, #61362, #90681, #206528, #157808, #142645, #208653, #191336, #57094, #126442, #40864, #58160, #60284, #41934, #192405, #39780, #44060, #176190, #27790, #159928, #77601, #174072, #143724, #155664, #106969, #23508, #172993, #139426, #24574, #25644, #91755, #9406, #73324, #205461, #123259, #213962, #113381, #82920, #148993, #179388, #80810, #144789, #146900, #29934, #46193, #65582, #47266, #131729, #31008, #32055, #568, #97083, #66635, #15778, #96018, #165244, #181487, #197734, #62419, #130697, #193492, #196689, #163135, #16838, #94948, #45134, #28861, #160996, #162071, #98143, #14719, #111244, #180438, #49375, #115492, #177249, #212920, #78661, #13660, #129647, #164192, #12588, #81864, #210796, #33116, #147948, #48328, #114438, #99193, #64554, #128583, #194549, #112311, #178326, #79732, #145848, #211855, #63491, #195632, #118689, #103446, #135953, #169506, #153256, #52557, #22150, #88265, #184673, #20040, #83984, #86127, #183619, #199859, #4831, #200908, #70911, #36295, #185737, #154333, #102371, #5908, #21088, #35226 ),
 ( #51502, #150072, #137021, #117628, #85056, #116551, #182543, #167382, #38443, #1644, #152200, #170568, #198783, #2709, #67702, #133849, #17898, #119758, #68783, #168441, #132780, #203048, #53626, #3767, #50432, #34169, #69842, #101302, #201968, #151142, #37370, #87191, #100241, #18972, #54689, #166309, #134902, #120840, #186815, #104523, #60030, #108850, #158605, #55756, #41674, #138091, #139157, #191078, #124056, #109922, #58965, #205187, #43809, #73058, #190022, #26456, #10204, #125120, #204104, #187881, #92565, #39508, #76279, #140247, #56828, #8067, #142387, #90408, #6977, #42745, #74153, #107785, #9145, #71981, #23235, #206268, #174876, #173810, #25389, #106700, #208396, #27526, #121912, #91488, #172725, #156478, #122998, #141330, #40595, #188955, #207344, #157549, #93625, #24303, #57893, #75219, #126181, #192145, #175933, #89346, #159667, #105607, #171638, #155395, #194297, #196438, #32867, #97890, #64305, #14460, #146648, #162881, #145601, #48082, #61101, #160737, #212663, #144532, #110983, #12331, #211596, #178061, #63232, #114193, #80551, #180193, #31814, #129395, #115249, #181239, #195374, #113122, #176989, #179128, #62175, #78411, #163951, #79482, #15526, #47006, #130450, #98943, #30750, #11269, #81612, #128334, #197489, #213714, #147696, #94696, #65337, #77347, #131484, #96831, #49131, #127260, #143459, #193231, #44878, #45942, #209457, #28607, #210541, #112061, #29679, #95763, #161816, #13406, #50186, #133605, #101052, #151958, #120597, #166066, #37123, #118446, #134664, #132542, #149828, #17653, #200667, #86948, #19798, #99999, #82670, #83736, #33925, #168199, #1398, #164997, #136776, #18726, #85882, #36050, #135710, #198540, #3528, #4592, #69603, #201736, #38202, #148754, #167141, #324, #184433, #53377, #70666, #119512, #185498, #16588, #66394, #84810, #116307, #102130, #103202, #52317, #199610, #20850, #186574, #182297, #169264, #51253, #34981, #67459, #153016, #117378, #183375, #202805, #54454, #150899, #2460, #68536, #7813, #91240, #107535, #189776, #121672, #190833, #39265, #204940, #41427, #72819, #74969, #125938, #42492, #157300, #173567, #25138, #8890, #24067, #141079, #154089, #105359, #207088, #22987, #203872, #171396, #90170, #56591, #156236, #58717, #124867, #108601, #174629, #73906, #208151, #59781, #139999, #206020, #55516, #57656, #155159, #89105, #26205, #172480, #92322, #123815, #158364, #191896, #9956, #104276, #76033, #6741, #142136, #170320, #21908, #187638, #88018, #5657, #71737, #137851, #138923, #122752, #188714, #40350, #106456, #94444, #96578, #177810, #131244, #30494, #113940, #47828, #15273, #95517, #143217, #12090, #194037, #162625, #213464, #44620, #130193, #211348, #13153, #11014, #28348, #110735, #79230, #179935, #112867, #192967, #175681, #176735, #127009, #46756, #160483, #43558, #81360, #111804, #178882, #129142, #14201, #77090, #80295, #78157, #128081, #144288 ) ),
 .UNSPECIFIED., .F., .F., .T. ) 
 B_SPLINE_SURFACE_WITH_KNOTS ( ( 2, 2 ),
 ( 3, 2, 2, 2, 2, 2, 2, 2, 2, 2, 2, 2, 2, 2, 2, 2, 2, 2, 2, 2, 2, 2, 2, 2, 2, 2, 2, 2, 2, 2, 2, 2, 2, 2, 2, 2, 2, 2, 2, 2, 2, 2, 2, 2, 2, 2, 2, 2, 2, 2, 2, 2, 2, 2, 2, 2, 2, 2, 2, 2, 2, 2, 2, 2, 2, 2, 2, 2, 2, 2, 2, 2, 2, 2, 2, 2, 2, 2, 2, 2, 2, 2, 2, 2, 2, 2, 2, 2, 2, 2, 2, 2, 2, 2, 2, 2, 2, 2, 2, 2, 2, 2, 2, 2, 2, 2, 2, 2, 2, 2, 2, 2, 2, 2, 2, 2, 2, 2, 2, 2, 2, 2, 2, 2, 2, 2, 2, 2, 2, 2, 2, 2, 2, 2, 2, 2, 2, 2, 2, 2, 2, 2, 2, 2, 2, 2, 2, 2, 2, 2, 2, 2, 2, 2, 2, 2, 2, 2, 2, 2, 2, 2, 2, 2, 2, 2, 2, 2, 3 ),
 ( 0.000000000000000000, 1.000000000000000000 ),
 ( 0.000000000000000000, 0.005952380952380952051, 0.01190476190476190410, 0.01785714285714285615, 0.02380952380952380820, 0.02976190476190476025, 0.03571428571428571230, 0.04166666666666666435, 0.04761904761904761640, 0.05357142857142856845, 0.05952380952380952051, 0.06547619047619047949, 0.07142857142857142461, 0.07738095238095238360, 0.08333333333333332871, 0.08928571428571428770, 0.09523809523809523281, 0.1011904761904761918, 0.1071428571428571369, 0.1130952380952380959, 0.1190476190476190410, 0.1250000000000000000, 0.1309523809523809590, 0.1369047619047619180, 0.1428571428571428492, 0.1488095238095238082, 0.1547619047619047672, 0.1607142857142857262, 0.1666666666666666574, 0.1726190476190476164, 0.1785714285714285754, 0.1845238095238095344, 0.1904761904761904656, 0.1964285714285714246, 0.2023809523809523836, 0.2083333333333333426, 0.2142857142857142738, 0.2202380952380952328, 0.2261904761904761918, 0.2321428571428571508, 0.2380952380952380820, 0.2440476190476190410, 0.2500000000000000000, 0.2559523809523809312, 0.2619047619047619180, 0.2678571428571428492, 0.2738095238095238360, 0.2797619047619047672, 0.2857142857142856984, 0.2916666666666666852, 0.2976190476190476164, 0.3035714285714285476, 0.3095238095238095344, 0.3154761904761904656, 0.3214285714285714524, 0.3273809523809523836, 0.3333333333333333148, 0.3392857142857143016, 0.3452380952380952328, 0.3511904761904761640, 0.3571428571428571508, 0.3630952380952380820, 0.3690476190476190688, 0.3750000000000000000, 0.3809523809523809312, 0.3869047619047619180, 0.3928571428571428492, 0.3988095238095238360, 0.4047619047619047672, 0.4107142857142856984, 0.4166666666666666852, 0.4226190476190476164, 0.4285714285714285476, 0.4345238095238095344, 0.4404761904761904656, 0.4464285714285714524, 0.4523809523809523836, 0.4583333333333333148, 0.4642857142857143016, 0.4702380952380952328, 0.4761904761904761640, 0.4821428571428571508, 0.4880952380952380820, 0.4940476190476190688, 0.5000000000000000000, 0.5059523809523809312, 0.5119047619047618625, 0.5178571428571429047, 0.5238095238095238360, 0.5297619047619047672, 0.5357142857142856984, 0.5416666666666666297, 0.5476190476190476719, 0.5535714285714286031, 0.5595238095238095344, 0.5654761904761904656, 0.5714285714285713969, 0.5773809523809523281, 0.5833333333333333703, 0.5892857142857143016, 0.5952380952380952328, 0.6011904761904761640, 0.6071428571428570953, 0.6130952380952381375, 0.6190476190476190688, 0.6250000000000000000, 0.6309523809523809312, 0.6369047619047618625, 0.6428571428571429047, 0.6488095238095238360, 0.6547619047619047672, 0.6607142857142856984, 0.6666666666666666297, 0.6726190476190476719, 0.6785714285714286031, 0.6845238095238095344, 0.6904761904761904656, 0.6964285714285713969, 0.7023809523809523281, 0.7083333333333333703, 0.7142857142857143016, 0.7202380952380952328, 0.7261904761904761640, 0.7321428571428570953, 0.7380952380952381375, 0.7440476190476190688, 0.7500000000000000000, 0.7559523809523809312, 0.7619047619047618625, 0.7678571428571429047, 0.7738095238095238360, 0.7797619047619047672, 0.7857142857142856984, 0.7916666666666666297, 0.7976190476190476719, 0.8035714285714286031, 0.8095238095238095344, 0.8154761904761904656, 0.8214285714285713969, 0.8273809523809523281, 0.8333333333333333703, 0.8392857142857143016, 0.8452380952380952328, 0.8511904761904761640, 0.8571428571428570953, 0.8630952380952381375, 0.8690476190476190688, 0.8750000000000000000, 0.8809523809523809312, 0.8869047619047618625, 0.8928571428571429047, 0.8988095238095238360, 0.9047619047619047672, 0.9107142857142856984, 0.9166666666666666297, 0.9226190476190476719, 0.9285714285714286031, 0.9345238095238095344, 0.9404761904761904656, 0.9464285714285713969, 0.9523809523809523281, 0.9583333333333333703, 0.9642857142857143016, 0.9702380952380952328, 0.9761904761904761640, 0.9821428571428570953, 0.9880952380952381375, 0.9940476190476190688, 1.000000000000000000 ),
 .UNSPECIFIED. ) 
 GEOMETRIC_REPRESENTATION_ITEM ( )  RATIONAL_B_SPLINE_SURFACE ( (
 ( 1.000000000000000000, 0.8660254037844387076, 1.000000000000000000, 0.8660254037844387076, 1.000000000000000000, 0.8660254037844387076, 1.000000000000000000, 0.8660254037844387076, 1.000000000000000000, 0.8660254037844387076, 1.000000000000000000, 0.8660254037844387076, 1.000000000000000000, 0.8660254037844387076, 1.000000000000000000, 0.8660254037844387076, 1.000000000000000000, 0.8660254037844387076, 1.000000000000000000, 0.8660254037844387076, 1.000000000000000000, 0.8660254037844387076, 1.000000000000000000, 0.8660254037844387076, 1.000000000000000000, 0.8660254037844387076, 1.000000000000000000, 0.8660254037844387076, 1.000000000000000000, 0.8660254037844387076, 1.000000000000000000, 0.8660254037844387076, 1.000000000000000000, 0.8660254037844387076, 1.000000000000000000, 0.8660254037844387076, 1.000000000000000000, 0.8660254037844387076, 1.000000000000000000, 0.8660254037844387076, 1.000000000000000000, 0.8660254037844387076, 1.000000000000000000, 0.8660254037844387076, 1.000000000000000000, 0.8660254037844387076, 1.000000000000000000, 0.8660254037844387076, 1.000000000000000000, 0.8660254037844387076, 1.000000000000000000, 0.8660254037844387076, 1.000000000000000000, 0.8660254037844387076, 1.000000000000000000, 0.8660254037844387076, 1.000000000000000000, 0.8660254037844387076, 1.000000000000000000, 0.8660254037844387076, 1.000000000000000000, 0.8660254037844387076, 1.000000000000000000, 0.8660254037844387076, 1.000000000000000000, 0.8660254037844387076, 1.000000000000000000, 0.8660254037844387076, 1.000000000000000000, 0.8660254037844387076, 1.000000000000000000, 0.8660254037844387076, 1.000000000000000000, 0.8660254037844387076, 1.000000000000000000, 0.8660254037844387076, 1.000000000000000000, 0.8660254037844387076, 1.000000000000000000, 0.8660254037844387076, 1.000000000000000000, 0.8660254037844387076, 1.000000000000000000, 0.8660254037844387076, 1.000000000000000000, 0.8660254037844387076, 1.000000000000000000, 0.8660254037844387076, 1.000000000000000000, 0.8660254037844387076, 1.000000000000000000, 0.8660254037844387076, 1.000000000000000000, 0.8660254037844387076, 1.000000000000000000, 0.8660254037844387076, 1.000000000000000000, 0.8660254037844387076, 1.000000000000000000, 0.8660254037844387076, 1.000000000000000000, 0.8660254037844387076, 1.000000000000000000, 0.8660254037844387076, 1.000000000000000000, 0.8660254037844387076, 1.000000000000000000, 0.8660254037844387076, 1.000000000000000000, 0.8660254037844387076, 1.000000000000000000, 0.8660254037844387076, 1.000000000000000000, 0.8660254037844387076, 1.000000000000000000, 0.8660254037844387076, 1.000000000000000000, 0.8660254037844387076, 1.000000000000000000, 0.8660254037844387076, 1.000000000000000000, 0.8660254037844387076, 1.000000000000000000, 0.8660254037844387076, 1.000000000000000000, 0.8660254037844387076, 1.000000000000000000, 0.8660254037844387076, 1.000000000000000000, 0.8660254037844387076, 1.000000000000000000, 0.8660254037844387076, 1.000000000000000000, 0.8660254037844387076, 1.000000000000000000, 0.8660254037844387076, 1.000000000000000000, 0.8660254037844387076, 1.000000000000000000, 0.8660254037844387076, 1.000000000000000000, 0.8660254037844387076, 1.000000000000000000, 0.8660254037844387076, 1.000000000000000000, 0.8660254037844387076, 1.000000000000000000, 0.8660254037844387076, 1.000000000000000000, 0.8660254037844387076, 1.000000000000000000, 0.8660254037844387076, 1.000000000000000000, 0.8660254037844387076, 1.000000000000000000, 0.8660254037844387076, 1.000000000000000000, 0.8660254037844387076, 1.000000000000000000, 0.8660254037844387076, 1.000000000000000000, 0.8660254037844387076, 1.000000000000000000, 0.8660254037844387076, 1.000000000000000000, 0.8660254037844387076, 1.000000000000000000, 0.8660254037844387076, 1.000000000000000000, 0.8660254037844387076, 1.000000000000000000, 0.8660254037844387076, 1.000000000000000000, 0.8660254037844387076, 1.000000000000000000, 0.8660254037844387076, 1.000000000000000000, 0.8660254037844387076, 1.000000000000000000, 0.8660254037844387076, 1.000000000000000000, 0.8660254037844387076, 1.000000000000000000, 0.8660254037844387076, 1.000000000000000000, 0.8660254037844387076, 1.000000000000000000, 0.8660254037844387076, 1.000000000000000000, 0.8660254037844387076, 1.000000000000000000, 0.8660254037844387076, 1.000000000000000000, 0.8660254037844387076, 1.000000000000000000, 0.8660254037844387076, 1.000000000000000000, 0.8660254037844387076, 1.000000000000000000, 0.8660254037844387076, 1.000000000000000000, 0.8660254037844387076, 1.000000000000000000, 0.8660254037844387076, 1.000000000000000000, 0.8660254037844387076, 1.000000000000000000, 0.8660254037844387076, 1.000000000000000000, 0.8660254037844387076, 1.000000000000000000, 0.8660254037844387076, 1.000000000000000000, 0.8660254037844387076, 1.000000000000000000, 0.8660254037844387076, 1.000000000000000000, 0.8660254037844387076, 1.000000000000000000, 0.8660254037844387076, 1.000000000000000000, 0.8660254037844387076, 1.000000000000000000, 0.8660254037844387076, 1.000000000000000000, 0.8660254037844387076, 1.000000000000000000, 0.8660254037844387076, 1.000000000000000000, 0.8660254037844387076, 1.000000000000000000, 0.8660254037844387076, 1.000000000000000000, 0.8660254037844387076, 1.000000000000000000, 0.8660254037844387076, 1.000000000000000000, 0.8660254037844387076, 1.000000000000000000, 0.8660254037844387076, 1.000000000000000000, 0.8660254037844387076, 1.000000000000000000, 0.8660254037844387076, 1.000000000000000000, 0.8660254037844387076, 1.000000000000000000, 0.8660254037844387076, 1.000000000000000000, 0.8660254037844387076, 1.000000000000000000, 0.8660254037844387076, 1.000000000000000000, 0.8660254037844387076, 1.000000000000000000, 0.8660254037844387076, 1.000000000000000000, 0.8660254037844387076, 1.000000000000000000, 0.8660254037844387076, 1.000000000000000000, 0.8660254037844387076, 1.000000000000000000, 0.8660254037844387076, 1.000000000000000000, 0.8660254037844387076, 1.000000000000000000, 0.8660254037844387076, 1.000000000000000000, 0.8660254037844387076, 1.000000000000000000, 0.8660254037844387076, 1.000000000000000000, 0.8660254037844387076, 1.000000000000000000, 0.8660254037844387076, 1.000000000000000000, 0.8660254037844387076, 1.000000000000000000, 0.8660254037844387076, 1.000000000000000000, 0.8660254037844387076, 1.000000000000000000, 0.8660254037844387076, 1.000000000000000000, 0.8660254037844387076, 1.000000000000000000, 0.8660254037844387076, 1.000000000000000000, 0.8660254037844387076, 1.000000000000000000, 0.8660254037844387076, 1.000000000000000000, 0.8660254037844387076, 1.000000000000000000, 0.8660254037844387076, 1.000000000000000000, 0.8660254037844387076, 1.000000000000000000, 0.8660254037844387076, 1.000000000000000000, 0.8660254037844387076, 1.000000000000000000, 0.8660254037844387076, 1.000000000000000000, 0.8660254037844387076, 1.000000000000000000, 0.8660254037844387076, 1.000000000000000000, 0.8660254037844387076, 1.000000000000000000, 0.8660254037844387076, 1.000000000000000000, 0.8660254037844387076, 1.000000000000000000, 0.8660254037844387076, 1.000000000000000000, 0.8660254037844387076, 1.000000000000000000, 0.8660254037844387076, 1.000000000000000000, 0.8660254037844387076, 1.000000000000000000, 0.8660254037844387076, 1.000000000000000000, 0.8660254037844387076, 1.000000000000000000, 0.8660254037844387076, 1.000000000000000000, 0.8660254037844387076, 1.000000000000000000, 0.8660254037844387076, 1.000000000000000000, 0.8660254037844387076, 1.000000000000000000, 0.8660254037844387076, 1.000000000000000000),
 ( 1.000000000000000000, 0.8660254037844387076, 1.000000000000000000, 0.8660254037844387076, 1.000000000000000000, 0.8660254037844387076, 1.000000000000000000, 0.8660254037844387076, 1.000000000000000000, 0.8660254037844387076, 1.000000000000000000, 0.8660254037844387076, 1.000000000000000000, 0.8660254037844387076, 1.000000000000000000, 0.8660254037844387076, 1.000000000000000000, 0.8660254037844387076, 1.000000000000000000, 0.8660254037844387076, 1.000000000000000000, 0.8660254037844387076, 1.000000000000000000, 0.8660254037844387076, 1.000000000000000000, 0.8660254037844387076, 1.000000000000000000, 0.8660254037844387076, 1.000000000000000000, 0.8660254037844387076, 1.000000000000000000, 0.8660254037844387076, 1.000000000000000000, 0.8660254037844387076, 1.000000000000000000, 0.8660254037844387076, 1.000000000000000000, 0.8660254037844387076, 1.000000000000000000, 0.8660254037844387076, 1.000000000000000000, 0.8660254037844387076, 1.000000000000000000, 0.8660254037844387076, 1.000000000000000000, 0.8660254037844387076, 1.000000000000000000, 0.8660254037844387076, 1.000000000000000000, 0.8660254037844387076, 1.000000000000000000, 0.8660254037844387076, 1.000000000000000000, 0.8660254037844387076, 1.000000000000000000, 0.8660254037844387076, 1.000000000000000000, 0.8660254037844387076, 1.000000000000000000, 0.8660254037844387076, 1.000000000000000000, 0.8660254037844387076, 1.000000000000000000, 0.8660254037844387076, 1.000000000000000000, 0.8660254037844387076, 1.000000000000000000, 0.8660254037844387076, 1.000000000000000000, 0.8660254037844387076, 1.000000000000000000, 0.8660254037844387076, 1.000000000000000000, 0.8660254037844387076, 1.000000000000000000, 0.8660254037844387076, 1.000000000000000000, 0.8660254037844387076, 1.000000000000000000, 0.8660254037844387076, 1.000000000000000000, 0.8660254037844387076, 1.000000000000000000, 0.8660254037844387076, 1.000000000000000000, 0.8660254037844387076, 1.000000000000000000, 0.8660254037844387076, 1.000000000000000000, 0.8660254037844387076, 1.000000000000000000, 0.8660254037844387076, 1.000000000000000000, 0.8660254037844387076, 1.000000000000000000, 0.8660254037844387076, 1.000000000000000000, 0.8660254037844387076, 1.000000000000000000, 0.8660254037844387076, 1.000000000000000000, 0.8660254037844387076, 1.000000000000000000, 0.8660254037844387076, 1.000000000000000000, 0.8660254037844387076, 1.000000000000000000, 0.8660254037844387076, 1.000000000000000000, 0.8660254037844387076, 1.000000000000000000, 0.8660254037844387076, 1.000000000000000000, 0.8660254037844387076, 1.000000000000000000, 0.8660254037844387076, 1.000000000000000000, 0.8660254037844387076, 1.000000000000000000, 0.8660254037844387076, 1.000000000000000000, 0.8660254037844387076, 1.000000000000000000, 0.8660254037844387076, 1.000000000000000000, 0.8660254037844387076, 1.000000000000000000, 0.8660254037844387076, 1.000000000000000000, 0.8660254037844387076, 1.000000000000000000, 0.8660254037844387076, 1.000000000000000000, 0.8660254037844387076, 1.000000000000000000, 0.8660254037844387076, 1.000000000000000000, 0.8660254037844387076, 1.000000000000000000, 0.8660254037844387076, 1.000000000000000000, 0.8660254037844387076, 1.000000000000000000, 0.8660254037844387076, 1.000000000000000000, 0.8660254037844387076, 1.000000000000000000, 0.8660254037844387076, 1.000000000000000000, 0.8660254037844387076, 1.000000000000000000, 0.8660254037844387076, 1.000000000000000000, 0.8660254037844387076, 1.000000000000000000, 0.8660254037844387076, 1.000000000000000000, 0.8660254037844387076, 1.000000000000000000, 0.8660254037844387076, 1.000000000000000000, 0.8660254037844387076, 1.000000000000000000, 0.8660254037844387076, 1.000000000000000000, 0.8660254037844387076, 1.000000000000000000, 0.8660254037844387076, 1.000000000000000000, 0.8660254037844387076, 1.000000000000000000, 0.8660254037844387076, 1.000000000000000000, 0.8660254037844387076, 1.000000000000000000, 0.8660254037844387076, 1.000000000000000000, 0.8660254037844387076, 1.000000000000000000, 0.8660254037844387076, 1.000000000000000000, 0.8660254037844387076, 1.000000000000000000, 0.8660254037844387076, 1.000000000000000000, 0.8660254037844387076, 1.000000000000000000, 0.8660254037844387076, 1.000000000000000000, 0.8660254037844387076, 1.000000000000000000, 0.8660254037844387076, 1.000000000000000000, 0.8660254037844387076, 1.000000000000000000, 0.8660254037844387076, 1.000000000000000000, 0.8660254037844387076, 1.000000000000000000, 0.8660254037844387076, 1.000000000000000000, 0.8660254037844387076, 1.000000000000000000, 0.8660254037844387076, 1.000000000000000000, 0.8660254037844387076, 1.000000000000000000, 0.8660254037844387076, 1.000000000000000000, 0.8660254037844387076, 1.000000000000000000, 0.8660254037844387076, 1.000000000000000000, 0.8660254037844387076, 1.000000000000000000, 0.8660254037844387076, 1.000000000000000000, 0.8660254037844387076, 1.000000000000000000, 0.8660254037844387076, 1.000000000000000000, 0.8660254037844387076, 1.000000000000000000, 0.8660254037844387076, 1.000000000000000000, 0.8660254037844387076, 1.000000000000000000, 0.8660254037844387076, 1.000000000000000000, 0.8660254037844387076, 1.000000000000000000, 0.8660254037844387076, 1.000000000000000000, 0.8660254037844387076, 1.000000000000000000, 0.8660254037844387076, 1.000000000000000000, 0.8660254037844387076, 1.000000000000000000, 0.8660254037844387076, 1.000000000000000000, 0.8660254037844387076, 1.000000000000000000, 0.8660254037844387076, 1.000000000000000000, 0.8660254037844387076, 1.000000000000000000, 0.8660254037844387076, 1.000000000000000000, 0.8660254037844387076, 1.000000000000000000, 0.8660254037844387076, 1.000000000000000000, 0.8660254037844387076, 1.000000000000000000, 0.8660254037844387076, 1.000000000000000000, 0.8660254037844387076, 1.000000000000000000, 0.8660254037844387076, 1.000000000000000000, 0.8660254037844387076, 1.000000000000000000, 0.8660254037844387076, 1.000000000000000000, 0.8660254037844387076, 1.000000000000000000, 0.8660254037844387076, 1.000000000000000000, 0.8660254037844387076, 1.000000000000000000, 0.8660254037844387076, 1.000000000000000000, 0.8660254037844387076, 1.000000000000000000, 0.8660254037844387076, 1.000000000000000000, 0.8660254037844387076, 1.000000000000000000, 0.8660254037844387076, 1.000000000000000000, 0.8660254037844387076, 1.000000000000000000, 0.8660254037844387076, 1.000000000000000000, 0.8660254037844387076, 1.000000000000000000, 0.8660254037844387076, 1.000000000000000000, 0.8660254037844387076, 1.000000000000000000, 0.8660254037844387076, 1.000000000000000000, 0.8660254037844387076, 1.000000000000000000, 0.8660254037844387076, 1.000000000000000000, 0.8660254037844387076, 1.000000000000000000, 0.8660254037844387076, 1.000000000000000000, 0.8660254037844387076, 1.000000000000000000, 0.8660254037844387076, 1.000000000000000000, 0.8660254037844387076, 1.000000000000000000, 0.8660254037844387076, 1.000000000000000000, 0.8660254037844387076, 1.000000000000000000, 0.8660254037844387076, 1.000000000000000000, 0.8660254037844387076, 1.000000000000000000, 0.8660254037844387076, 1.000000000000000000, 0.8660254037844387076, 1.000000000000000000, 0.8660254037844387076, 1.000000000000000000, 0.8660254037844387076, 1.000000000000000000, 0.8660254037844387076, 1.000000000000000000, 0.8660254037844387076, 1.000000000000000000, 0.8660254037844387076, 1.000000000000000000, 0.8660254037844387076, 1.000000000000000000, 0.8660254037844387076, 1.000000000000000000, 0.8660254037844387076, 1.000000000000000000, 0.8660254037844387076, 1.000000000000000000) ) ) 
 REPRESENTATION_ITEM ( '' )  SURFACE ( )  );
#60637 = ORIENTED_EDGE ( 'NONE', *, *, #144738, .F. ) ;
#60636 = CARTESIAN_POINT ( 'NONE',  ( -0.5050423914800155067, 7.726475908227449452, -1.936073478083378596 ) ) ;
#60638 = CARTESIAN_POINT ( 'NONE',  ( 3.075545897833771747, 1.462222457232667416, -1.388272539953112839 ) ) ;
#60639 = CARTESIAN_POINT ( 'NONE',  ( 2.941158370608713213, 0.6622022323767087215, -1.718108305994885177 ) ) ;
#60640 = CARTESIAN_POINT ( 'NONE',  ( 0.8390048429645606820, 2.274487955075610301, 0.3892829850337137243 ) ) ;
#60641 = CARTESIAN_POINT ( 'NONE',  ( 5.734172623936983904, 5.654565914206774124, 0.7998128361456352531 ) ) ;
#60642 = CARTESIAN_POINT ( 'NONE',  ( 2.759224924868249662, -1.879262701025650850, -1.068020781904190253 ) ) ;
#60643 = CARTESIAN_POINT ( 'NONE',  ( -6.762819695118240659, 6.784377820593065600, 0.7998128361456341429 ) ) ;
#60644 = CARTESIAN_POINT ( 'NONE',  ( 2.390373184264094952, -0.001117755346285650552, 2.298542322714514530 ) ) ;
#60645 = EDGE_LOOP ( 'NONE', ( #8863, #188447, #129299, #112662 ) ) ;
#60646 = CARTESIAN_POINT ( 'NONE',  ( 1.252583056964752029, -1.476889893665521925, 1.148006582770304096 ) ) ;
#60647 = CARTESIAN_POINT ( 'NONE',  ( 5.383651750111712708, 1.323420565077202182, 1.461416689776244615 ) ) ;
#60649 = CARTESIAN_POINT ( 'NONE',  ( 9.097157884645296733, 10.67606762258344055, -1.082531754730543083 ) ) ;
#60648 = CARTESIAN_POINT ( 'NONE',  ( 1.364683531249990311, 3.634375000341416584, 1.214306433183764966E-14 ) ) ;
#60651 = CARTESIAN_POINT ( 'NONE',  ( 0.9794701899953797142, -0.05759512415488829418, -2.206297691287119722 ) ) ;
#60650 = CARTESIAN_POINT ( 'NONE',  ( -7.874588291438845644, 8.081441182967111558, -0.7998128361456291469 ) ) ;
#60652 = ADVANCED_FACE ( 'NONE', ( #140601 ), #121193, .F. ) ;
#60653 = CARTESIAN_POINT ( 'NONE',  ( 3.669453130792974971, 7.432779085900453886, 1.040834085586084257E-14 ) ) ;
#60654 = CARTESIAN_POINT ( 'NONE',  ( -5.117312914154178216, 8.057616602233474978, -1.199719254218452047 ) ) ;
#60655 = CARTESIAN_POINT ( 'NONE',  ( 6.639320575229286092, 4.689090874229541406, 2.765823994384248419 ) ) ;
#60656 = CARTESIAN_POINT ( 'NONE',  ( 4.504732016840462983, 1.524723275766314279, -1.249774587014943483 ) ) ;
#60657 = CARTESIAN_POINT ( 'NONE',  ( 0.1234922912959918878, 1.848187084301698757, 1.039613981531524400 ) ) ;
#60658 = CARTESIAN_POINT ( 'NONE',  ( 4.828937647557053126, 2.207305988086407655, 0.6732806465959675357 ) ) ;
#60659 = ADVANCED_FACE ( 'NONE', ( #22512 ), #159308, .F. ) ;
#60660 = CARTESIAN_POINT ( 'NONE',  ( 3.221586243988622034, 0.3073416805365276061, -2.039453084318449072 ) ) ;
#60661 = CARTESIAN_POINT ( 'NONE',  ( 5.965224400332808763, 9.903252867122883885, -0.7216878364870267237 ) ) ;
#60662 = CARTESIAN_POINT ( 'NONE',  ( 4.030516805012513082, 7.924296382481737844, 0.000000000000000000 ) ) ;
#60663 = CARTESIAN_POINT ( 'NONE',  ( 4.573896719763862251, 6.429575154514868274, -1.599625672291273171 ) ) ;
#60664 = CARTESIAN_POINT ( 'NONE',  ( 1.364683531249988757, 1.946875000341415030, 0.000000000000000000 ) ) ;
#60665 = CARTESIAN_POINT ( 'NONE',  ( 3.770049233051776749, 6.556085317605844232, 1.199719254218451159 ) ) ;
#60666 = CARTESIAN_POINT ( 'NONE',  ( 5.544921637864819175, 7.492161215640853023, -1.443375672974057666 ) ) ;
#60667 = CARTESIAN_POINT ( 'NONE',  ( 5.494640824104591204, 2.138133990741352353, 0.3765844856341519775 ) ) ;
#60669 = CARTESIAN_POINT ( 'NONE',  ( 4.159580895514263688, 0.8717668643758098579, 1.621812032879976329 ) ) ;
#60668 = CARTESIAN_POINT ( 'NONE',  ( -3.145128448690310830, 6.613140923539910787, -0.7216878364870267237 ) ) ;
#60670 = B_SPLINE_CURVE_WITH_KNOTS ( 'NONE', 3,
 ( #100346, #167485, #201015, #150182, #6017, #55861, #138198, #204208, #68885, #22262, #203155, #184776, #71013, #135004 ),
 .UNSPECIFIED., .F., .F.,
 ( 4, 2, 2, 2, 2, 2, 4 ),
 ( 0.0002398601398896809181, 0.09869445199344967223, 0.1971490438470096807, 0.2956036357005696891, 0.3202172836639597397, 0.3448309316273497904, 0.3940582275541297808 ),
 .UNSPECIFIED. ) ;
#60672 = CARTESIAN_POINT ( 'NONE',  ( 6.720655732516671144, 1.288224904612661925, 1.942155157606942240 ) ) ;
#60671 = LINE ( 'NONE', #77991, #168638 ) ;
#60673 = CARTESIAN_POINT ( 'NONE',  ( 5.689076433642084041, 1.658752129386225516, 1.432425853890168188 ) ) ;
#60674 = CARTESIAN_POINT ( 'NONE',  ( 0.4461838333974484927, 2.877219473291486640, 1.949594826320268481 ) ) ;
#60675 = CARTESIAN_POINT ( 'NONE',  ( 6.614178507701674370, -1.059427008983104601, -1.999161347636166930 ) ) ;
#60676 = CARTESIAN_POINT ( 'NONE',  ( -3.980123661693549142, 7.843117270353603843, 0.1539385989055529202 ) ) ;
#60677 = CARTESIAN_POINT ( 'NONE',  ( 0.000000000000000000, 4.000000000000003553, 0.000000000000000000 ) ) ;
#60678 = CARTESIAN_POINT ( 'NONE',  ( 4.595841027163160675, 8.489102040997540399, 0.04885061651019838302 ) ) ;
#60679 = CARTESIAN_POINT ( 'NONE',  ( -4.787437638956935082, 6.678706226906775179, -1.443375672974066548 ) ) ;
#60680 = CARTESIAN_POINT ( 'NONE',  ( -6.511381374296909996, -8.144978210217297843, -6.953912913643677030 ) ) ;
#60681 = CARTESIAN_POINT ( 'NONE',  ( 0.7425837709835466649, -1.521049679623546425, 0.9045992453171716186 ) ) ;
#60682 = CARTESIAN_POINT ( 'NONE',  ( 5.039702193125279450, -1.910865547410881549, 0.6335069822010936935 ) ) ;
#60683 = CARTESIAN_POINT ( 'NONE',  ( 4.971035877704902184, 8.951292290631053916, 1.040834085586084257E-14 ) ) ;
#60684 = CARTESIAN_POINT ( 'NONE',  ( 3.628042789974804450, -1.253006538321174146, -1.692492853607285630 ) ) ;
#60685 = CARTESIAN_POINT ( 'NONE',  ( 2.706530202829552145, 1.804627309565815185, 0.6429686382581675241 ) ) ;
#60686 = FACE_OUTER_BOUND ( 'NONE', #195532, .T. ) ;
#60687 = CARTESIAN_POINT ( 'NONE',  ( 4.053143702687862060, 1.665121224333296235, -1.051576502219366605 ) ) ;
#60688 = CARTESIAN_POINT ( 'NONE',  ( 5.976820969762068003, -1.425406409037911937, 1.431266451708369303 ) ) ;
#60689 = CARTESIAN_POINT ( 'NONE',  ( 1.340467186903429253, 0.3614942610149494695, 1.835218787103513050 ) ) ;
#60692 = VERTEX_POINT ( 'NONE', #12092 ) ;
#60691 = CARTESIAN_POINT ( 'NONE',  ( 1.722773492080275748, 1.414811824084385661, -1.286832238068566392 ) ) ;
#60690 = CARTESIAN_POINT ( 'NONE',  ( 4.635198054048816019, -1.575417825122129134, 0.7027606912313691945 ) ) ;
#60694 = CARTESIAN_POINT ( 'NONE',  ( 3.551873057100274789, 7.087676300018221021, 0.7216878364870298324 ) ) ;
#60693 = CARTESIAN_POINT ( 'NONE',  ( 1.014635385311330795, -0.9952708415592588231, -1.969785480804244315 ) ) ;
#60695 = CARTESIAN_POINT ( 'NONE',  ( -1.364683531250012516, 1.592708333674756727, 0.7879004041258379498 ) ) ;
#60696 = CARTESIAN_POINT ( 'NONE',  ( 8.263858322729371153, 9.599921783727809910, -1.199719254218446718 ) ) ;
#60698 = CARTESIAN_POINT ( 'NONE',  ( 6.684453402082995765, -1.835023323784425342, -0.3624468955198830167 ) ) ;
#60697 = COLOUR_RGB ( '', 0.72549020, 0.75294118, 0.79215686) ;
#60699 = CARTESIAN_POINT ( 'NONE',  ( 0.4588732745636386334, 6.941177932071661338, -3.888237242762151435 ) ) ;
#60700 = CARTESIAN_POINT ( 'NONE',  ( 3.009546912109283934, 6.454962464195385330, 0.000000000000000000 ) ) ;
#60701 = CARTESIAN_POINT ( 'NONE',  ( 6.801849727211993546, -7.605490242344523644, 7.458876343102490480 ) ) ;
#60702 = CARTESIAN_POINT ( 'NONE',  ( 1.592325325408463055, 1.022198633559557646, -1.800363622228560168 ) ) ;
#60704 = CARTESIAN_POINT ( 'NONE',  ( 1.499999999999989120, 2.504166666666687302, 0.8660254037844524744 ) ) ;
#60703 = AXIS2_PLACEMENT_3D ( 'NONE', #171912, #204374, #123260 ) ;
#60705 = CARTESIAN_POINT ( 'NONE',  ( 5.503720292143644777, 8.508425209887878538, 1.199719254218462483 ) ) ;
#60706 = CARTESIAN_POINT ( 'NONE',  ( -7.877450944739929461, 9.149113176073413456, 1.199719254218462483 ) ) ;
#60707 = CARTESIAN_POINT ( 'NONE',  ( 3.040771591214902259, 6.769593633051179005, -0.7998128361456362523 ) ) ;
#60708 = CARTESIAN_POINT ( 'NONE',  ( 0.2408861781304712513, 1.933338575160881367, 0.5842326518414300285 ) ) ;
#60709 = CARTESIAN_POINT ( 'NONE',  ( 1.499999999999956257, 5.795833333333352044, -0.8660254037844512531 ) ) ;
#60710 = CARTESIAN_POINT ( 'NONE',  ( 0.6823417656249882723, 2.676041667008084879, -1.181850606188749264 ) ) ;
#60711 = ORIENTED_EDGE ( 'NONE', *, *, #159948, .F. ) ;
#60713 = CARTESIAN_POINT ( 'NONE',  ( 3.521367211247359741, 5.131347717920458962, -1.599625672291262513 ) ) ;
#60712 = CARTESIAN_POINT ( 'NONE',  ( -0.7500000000000006661, 11.70833333333333393, -1.299038105676657340 ) ) ;
#60714 = CARTESIAN_POINT ( 'NONE',  ( 4.165388622617651748, -0.6297791189726584804, -1.915306643112117291 ) ) ;
#60715 = CARTESIAN_POINT ( 'NONE',  ( 4.821452977306352139, -1.359283356373307328, -1.350213215339219897 ) ) ;
#60716 = FACE_OUTER_BOUND ( 'NONE', #178809, .T. ) ;
#60717 = CARTESIAN_POINT ( 'NONE',  ( 2.525153347276567484, -2.043736813514348771, 0.7916865192442237298 ) ) ;
#60718 = CARTESIAN_POINT ( 'NONE',  ( -1.859587702710848944, 3.245828361968106535, 0.3999999999999837574 ) ) ;
#60719 = CARTESIAN_POINT ( 'NONE',  ( 1.499999999999987121, 1.077083334016148308, -0.8660254037844253849 ) ) ;
#60720 = CARTESIAN_POINT ( 'NONE',  ( 5.660407656431548418, 2.011079132963066840, 0.09461074985974733675 ) ) ;
#60721 = CARTESIAN_POINT ( 'NONE',  ( -5.696397096036042385, 9.797547045350714967, -0.7998128361456231517 ) ) ;
#60723 = CARTESIAN_POINT ( 'NONE',  ( 6.433232048832024930, -1.700592621796994441, -1.261046147972416875 ) ) ;
#60722 = CARTESIAN_POINT ( 'NONE',  ( -2.155383234892699562, 5.458438174109348395, 1.040834085586084257E-14 ) ) ;
#60724 = CARTESIAN_POINT ( 'NONE',  ( -1.364683531250000748, 9.421875000341396245, 0.000000000000000000 ) ) ;
#60726 = CARTESIAN_POINT ( 'NONE',  ( -4.858757509019083543, 5.629766575900002401, -2.500000000000000444 ) ) ;
#60725 = CARTESIAN_POINT ( 'NONE',  ( 3.456657222422593545, -1.844998171120499020, -0.9834188347317989187 ) ) ;
#60728 = VERTEX_POINT ( 'NONE', #131247 ) ;
#60727 = CARTESIAN_POINT ( 'NONE',  ( 1.834533585138716782, 0.1645414454686990324, 1.716894335133994698 ) ) ;
#60729 = CARTESIAN_POINT ( 'NONE',  ( -1.237941840313982578, -1.374772708486751593, 1.500000000000001332 ) ) ;
#60730 = CARTESIAN_POINT ( 'NONE',  ( 6.823831386379729302, 6.855558127064808716, -0.7998128361456281477 ) ) ;
#60731 = CARTESIAN_POINT ( 'NONE',  ( 11.01135777277262306, 12.69999999999998153, 1.399999999999998579 ) ) ;
#60732 = CARTESIAN_POINT ( 'NONE',  ( 0.04698948850440434755, -9.984793193541563028, 9.579582872750577849 ) ) ;
#60733 = CARTESIAN_POINT ( 'NONE',  ( 6.932145363377535396, -8.169775483750580491, -6.496114076516128932 ) ) ;
#60734 = CARTESIAN_POINT ( 'NONE',  ( 6.928380191783277908, 8.041863964290678624, 1.199719254218462483 ) ) ;
#60735 = EDGE_LOOP ( 'NONE', ( #162963, #188874, #210804, #205757, #137240, #124223 ) ) ;
#60736 = CARTESIAN_POINT ( 'NONE',  ( 1.286813488861806354, 4.047007041464545374, -0.4595522011843541366 ) ) ;
#60737 = ADVANCED_FACE ( 'NONE', ( #114991 ), #45692, .F. ) ;
#60738 = CARTESIAN_POINT ( 'NONE',  ( 2.596125760314275777, -0.9296622322433767405, 1.554548433350180225 ) ) ;
#60740 = CARTESIAN_POINT ( 'NONE',  ( -7.067878151425722955, 7.140279352951794500, 0.7998128361456341429 ) ) ;
#60739 = AXIS2_PLACEMENT_3D ( 'NONE', #94617, #210459, #74073 ) ;
#60741 = ORIENTED_EDGE ( 'NONE', *, *, #123262, .T. ) ;
#60742 = CARTESIAN_POINT ( 'NONE',  ( 5.027376032568989572, 4.759693547618927489, 0.7998128361456341429 ) ) ;
#60743 = ORIENTED_EDGE ( 'NONE', *, *, #44167, .T. ) ;
#60744 = CARTESIAN_POINT ( 'NONE',  ( 4.817943484809818600, 6.714296380401858499, 1.599625672291269396 ) ) ;
#60745 = CARTESIAN_POINT ( 'NONE',  ( 3.896947601784990223, -0.1811674076915045506, -1.802394175579679958 ) ) ;
#60746 = CARTESIAN_POINT ( 'NONE',  ( 6.539320575229287336, 0.5820952121784334077, 2.049435377300548033 ) ) ;
#60747 = SURFACE_STYLE_FILL_AREA ( #210183 ) ;
#60748 = CARTESIAN_POINT ( 'NONE',  ( 4.171261675657679469, 7.370687464442305270, 0.7961138118306176903 ) ) ;
#60749 = ORIENTED_EDGE ( 'NONE', *, *, #83855, .F. ) ;
#60750 = CARTESIAN_POINT ( 'NONE',  ( 4.070637595011177723, 1.317219721392929310, -1.314973792616628945 ) ) ;
#60751 = CARTESIAN_POINT ( 'NONE',  ( 1.933070621186453897, -1.539717990624125621, -1.139454883405303098 ) ) ;
#60752 = CARTESIAN_POINT ( 'NONE',  ( 0.4283665542385572955, 1.745377284433462295, 0.5351633580037706839 ) ) ;
#60753 = CARTESIAN_POINT ( 'NONE',  ( -1.500000000000039524, 7.750000000000000000, -10.86128356754322688 ) ) ;
#60754 = CYLINDRICAL_SURFACE ( 'NONE', #181795, 0.08000000000000020983 ) ;
#60755 = B_SPLINE_CURVE_WITH_KNOTS ( 'NONE', 3,
 ( #105495, #43693, #188847, #156364 ),
 .UNSPECIFIED., .F., .F.,
 ( 4, 4 ),
 ( 0.001768109493081024492, 0.002022414007280575604 ),
 .UNSPECIFIED. ) ;
#60756 = AXIS2_PLACEMENT_3D ( 'NONE', #76997, #75944, #158277 ) ;
#60757 = CARTESIAN_POINT ( 'NONE',  ( 5.840936731490688594, 7.196517624969346549, 1.161314407385056313 ) ) ;
#60758 = CARTESIAN_POINT ( 'NONE',  ( 9.410656278130334229, 14.12788591601509758, 8.484697815724119963 ) ) ;
#60759 = CARTESIAN_POINT ( 'NONE',  ( -3.946537740505278613, 2.817530495244580102, 0.7750000000000135669 ) ) ;
#60760 = CARTESIAN_POINT ( 'NONE',  ( -4.121315508874276112, 4.870918184183829602, -1.082531754730549967 ) ) ;
#60761 = CARTESIAN_POINT ( 'NONE',  ( 7.537970219518073556, 9.817384560903001045, -1.443375672974057666 ) ) ;
#60762 = CARTESIAN_POINT ( 'NONE',  ( 5.436368237181718577, -1.097297496841664444, 1.635214795183062675 ) ) ;
#60763 = CARTESIAN_POINT ( 'NONE',  ( -5.427341564172148303, 5.226320001155936090, 0.000000000000000000 ) ) ;
#60764 = CARTESIAN_POINT ( 'NONE',  ( -3.951451420331601128, 7.320064228719081356, -0.7343074186010454252 ) ) ;
#60765 = CIRCLE ( 'NONE', #1814, 10.99999999999733369 ) ;
#60766 = CARTESIAN_POINT ( 'NONE',  ( 0.6387612955554131666, -1.792149412372344042, 1.076304641864724410 ) ) ;
#60767 = CARTESIAN_POINT ( 'NONE',  ( 6.923409998072794558, 11.22906209772695618, 1.040834085586084257E-14 ) ) ;
#60768 = CARTESIAN_POINT ( 'NONE',  ( 5.420897863522853299, 1.779935589243306859, 0.7372156234431108679 ) ) ;
#60769 = CARTESIAN_POINT ( 'NONE',  ( -5.717788096661253761, 7.693838750903348789, 1.599625672291269396 ) ) ;
#60770 = CARTESIAN_POINT ( 'NONE',  ( 0.9733497034139363402, 1.760643049788807257, -0.4823509818385819936 ) ) ;
#60771 = CARTESIAN_POINT ( 'NONE',  ( 2.192262590105994668, -0.9421081357594159877, 1.995820444975453745 ) ) ;
#60772 = EDGE_CURVE ( 'NONE', #4563, #48008, #20518, .T. ) ;
#60773 = CARTESIAN_POINT ( 'NONE',  ( 11.86687215968023601, 12.49057787694218824, 1.056395335932121871 ) ) ;
#60774 = CARTESIAN_POINT ( 'NONE',  ( 0.5977379272000953314, 1.286164058678052946, 1.415416067018962165 ) ) ;
#60775 = VERTEX_POINT ( 'NONE', #211351 ) ;
#60776 = CARTESIAN_POINT ( 'NONE',  ( 0.8363043462186695587, -1.097040784323728424, 1.635518954194992824 ) ) ;
#60777 = CARTESIAN_POINT ( 'NONE',  ( 3.087376005906359744, -0.7846555324184587565, 1.776656735299622980 ) ) ;
#60778 = ORIENTED_EDGE ( 'NONE', *, *, #117565, .F. ) ;
#60779 = CARTESIAN_POINT ( 'NONE',  ( 1.335314297916901927, -1.281167425915705316, 1.556668322744148014 ) ) ;
#60781 = CARTESIAN_POINT ( 'NONE',  ( 5.032013264887808646, 1.069401199365666688, 1.522792188549914272 ) ) ;
#60780 = CARTESIAN_POINT ( 'NONE',  ( -4.633854640820660009, 8.628190524257904670, -0.7998128361456362523 ) ) ;
#60782 = CARTESIAN_POINT ( 'NONE',  ( 3.888156192069020634, 7.758209000714329839, 1.040834085586084257E-14 ) ) ;
#60783 = DIRECTION ( 'NONE',  ( -0.9999980456341538426, 0.000000000000000000, -0.001977050295941262543 ) ) ;
#60784 = CARTESIAN_POINT ( 'NONE',  ( 9.154780037725547714, 11.70366268214508487, 1.599625672291279388 ) ) ;
#60785 = CARTESIAN_POINT ( 'NONE',  ( -3.581325132304157943, 7.329963087663487364, -0.7998128361456281477 ) ) ;
#60786 = CARTESIAN_POINT ( 'NONE',  ( -5.738844160334429567, 9.917344963690652548, 0.000000000000000000 ) ) ;
#60787 = CARTESIAN_POINT ( 'NONE',  ( 1.277182604683280598, 2.023070758711601691, -0.8431670391453591762 ) ) ;
#60788 = CARTESIAN_POINT ( 'NONE',  ( 3.497640442645619796, 6.064035702186436616, -1.082531754730543083 ) ) ;
#60789 = CARTESIAN_POINT ( 'NONE',  ( -10.50000000000000000, 12.69999999999999929, -3.600000000000000977 ) ) ;
#60790 = DIRECTION ( 'NONE',  ( 0.000000000000000000, 0.000000000000000000, 1.000000000000000000 ) ) ;
#60791 = CARTESIAN_POINT ( 'NONE',  ( 2.947667120405720986, 0.6567698719579934119, -1.703645827024417914 ) ) ;
#60792 = CARTESIAN_POINT ( 'NONE',  ( -2.449219305563052895, 6.009172956465517856, 1.040834085586084257E-14 ) ) ;
#60793 = CARTESIAN_POINT ( 'NONE',  ( -4.627410500965859264, 4.293067094081919777, 0.7998128361456341429 ) ) ;
#60794 = CARTESIAN_POINT ( 'NONE',  ( -5.645675577465527617, 7.454724071444114308, -1.341317915573495334 ) ) ;
#60795 = CARTESIAN_POINT ( 'NONE',  ( -0.02968770228137587730, 6.948707269782667062, -2.421356871654921417 ) ) ;
#60796 = CARTESIAN_POINT ( 'NONE',  ( 9.215791728987056786, 11.77484298861683598, -1.599625672291262513 ) ) ;
#60797 = CARTESIAN_POINT ( 'NONE',  ( 0.6625679566808447829, -1.396226752684716521, 1.327616383781888176 ) ) ;
#60798 = CARTESIAN_POINT ( 'NONE',  ( 5.612146373276853950, 1.959670608579218376, -0.09257137562097839112 ) ) ;
#60799 = ADVANCED_FACE ( 'NONE', ( #110737 ), #28351, .F. ) ;
#60800 = CARTESIAN_POINT ( 'NONE',  ( -6.009258394948636914E-15, 15.43750000000000178, -1.732050807568875195 ) ) ;
#60801 = CARTESIAN_POINT ( 'NONE',  ( -7.888146445052511169, 8.097259028849730811, 1.040834085586084257E-14 ) ) ;
#60802 = CARTESIAN_POINT ( 'NONE',  ( 6.173040012923759257, 6.096301524699504704, -0.7998128361456281477 ) ) ;
#60803 = CARTESIAN_POINT ( 'NONE',  ( 5.038714576072483631, -1.879839391954684746, 1.126354835186346603 ) ) ;
#60804 = CARTESIAN_POINT ( 'NONE',  ( 4.241125740018336643, -0.1978421677554068614, -2.060750949040678570 ) ) ;
#60806 = CARTESIAN_POINT ( 'NONE',  ( -1.201851678989727383E-14, 0.8843750003414173610, 1.575800808251672791 ) ) ;
#60805 =( LENGTH_UNIT ( ) NAMED_UNIT ( * ) SI_UNIT ( .MILLI., .METRE. ) );
#60807 = ORIENTED_EDGE ( 'NONE', *, *, #59736, .F. ) ;
#60808 = CARTESIAN_POINT ( 'NONE',  ( 4.430533913404213209, -1.776825693393409455, -1.458421372522151538 ) ) ;
#60810 = ORIENTED_EDGE ( 'NONE', *, *, #7913, .T. ) ;
#60809 = CARTESIAN_POINT ( 'NONE',  ( 5.992340707560141588, 9.934888558888093968, 0.7216878364870438212 ) ) ;
#60812 = CARTESIAN_POINT ( 'NONE',  ( 0.3282377607281167786, 1.323664549684625324, 1.224999999999979217 ) ) ;
#60811 = CARTESIAN_POINT ( 'NONE',  ( 4.855228407469603269, 7.718164671139588151, -1.082531754730548412 ) ) ;
#60813 = CARTESIAN_POINT ( 'NONE',  ( -7.834948825496938163, -5.907420853759296264, -7.720982897393567690 ) ) ;
#60814 = CARTESIAN_POINT ( 'NONE',  ( -9.766653781993813510, 4.463134066693873692, -6.897859727666959095 ) ) ;
#60815 = CARTESIAN_POINT ( 'NONE',  ( 4.101460596356475641, -1.936652220471976937, 0.1442349196467233863 ) ) ;
#60816 = EDGE_LOOP ( 'NONE', ( #185921, #209169, #32202, #9675 ) ) ;
#60817 = CARTESIAN_POINT ( 'NONE',  ( 9.042925270190625753, 11.57316545335434199, 1.443375672974076540 ) ) ;
#60818 = EDGE_CURVE ( 'NONE', #104249, #50012, #620, .T. ) ;
#60819 = EDGE_LOOP ( 'NONE', ( #26352, #46444, #198613, #158604 ) ) ;
#60820 = CARTESIAN_POINT ( 'NONE',  ( 5.027564050633359649, -0.2746679736120913318, 1.892429487827557599 ) ) ;
#60821 = CARTESIAN_POINT ( 'NONE',  ( 6.387718858896353602, 1.193691027695796825, 1.245227284122518485 ) ) ;
#60822 = CARTESIAN_POINT ( 'NONE',  ( 4.786342355033275986, -0.6839347017603313317, -1.897111394664739104 ) ) ;
#60823 = DIRECTION ( 'NONE',  ( 1.000000000000000000, 0.000000000000000000, -1.224646799147353207E-16 ) ) ;
#60824 = CARTESIAN_POINT ( 'NONE',  ( 1.366164030173490973, 2.173753390890633685, -0.3800739277931909355 ) ) ;
#60826 = DIRECTION ( 'NONE',  ( -5.578564026256490882E-16, -1.000000000000000000, -9.066213480720158442E-32 ) ) ;
#60825 = CARTESIAN_POINT ( 'NONE',  ( -9.317477881089553549, 11.89347683273641820, 1.599625672291281386 ) ) ;
#60828 = CARTESIAN_POINT ( 'NONE',  ( 6.520749347316099787, 1.652272609716086249, 0.6344386834381664508 ) ) ;
#60827 = CARTESIAN_POINT ( 'NONE',  ( 1.658266814308974268, -1.477475772113973740, 1.479395487768909501 ) ) ;
#60829 = CARTESIAN_POINT ( 'NONE',  ( 6.170546107226446253, 1.392543322632183722, 1.458558933167881211 ) ) ;
#60831 = CARTESIAN_POINT ( 'NONE',  ( 3.187719515414323190, -0.9288583595017800842, 2.095805606604860039 ) ) ;
#60830 = CARTESIAN_POINT ( 'NONE',  ( 3.739016502318667445, 7.584212696005614873, 0.7998128361456271485 ) ) ;
#60832 = CARTESIAN_POINT ( 'NONE',  ( 0.6732859938517594678, -0.9703907760119870884, 1.444448127723398478 ) ) ;
#60833 = CARTESIAN_POINT ( 'NONE',  ( 2.637105894733019262, 1.998242115483703341, 0.7103459930332192140 ) ) ;
#60834 = DIRECTION ( 'NONE',  ( 0.000000000000000000, 0.000000000000000000, -1.000000000000000000 ) ) ;
#60835 = CARTESIAN_POINT ( 'NONE',  ( 0.5261554912905551662, 1.716204961384654171, -0.2456527019241669663 ) ) ;
#60836 = CARTESIAN_POINT ( 'NONE',  ( -3.355169270512988773E-14, 1.234375000341463968, 1.570758158831764062 ) ) ;
#60837 = CARTESIAN_POINT ( 'NONE',  ( 2.172091045797384989, -0.8737597001905510474, -1.643165899227620796 ) ) ;
#60838 = CARTESIAN_POINT ( 'NONE',  ( 1.047617182619766885, 1.914800503461089543, -1.023450759211230521 ) ) ;
#60839 = CARTESIAN_POINT ( 'NONE',  ( 2.940638933469359895, -1.523795050681177710, 1.320827213682006285 ) ) ;
#60840 = CARTESIAN_POINT ( 'NONE',  ( 4.937500000000003553, 1.451031289060916496, -1.451031289061313512 ) ) ;
#60841 = CARTESIAN_POINT ( 'NONE',  ( -1.402160292154681736E-14, 1.618750000682814827, -1.732050807568863648 ) ) ;
#60842 = CARTESIAN_POINT ( 'NONE',  ( 6.463506663115213158, 0.3265968279197262181, -1.898468693527188389 ) ) ;
#60843 = CARTESIAN_POINT ( 'NONE',  ( -1.364683531250010295, 13.13020833367472839, 0.7879004041258445001 ) ) ;
#60844 = CARTESIAN_POINT ( 'NONE',  ( 3.709420277874009297, 1.875127481890274561, -1.190789481685197604 ) ) ;
#60845 = ORIENTED_EDGE ( 'NONE', *, *, #196992, .F. ) ;
#60846 = CARTESIAN_POINT ( 'NONE',  ( -0.2110808730067326444, 6.948329377029001996, -2.392166167428900536 ) ) ;
#60847 = CARTESIAN_POINT ( 'NONE',  ( 7.832860060393120882, 10.16142270859057462, 1.599625672291281386 ) ) ;
#60848 = CARTESIAN_POINT ( 'NONE',  ( 1.364683531249988757, -0.8656249996585805295, 0.000000000000000000 ) ) ;
#60849 = CARTESIAN_POINT ( 'NONE',  ( 6.110887277445514520, -0.2035749799894230883, 1.728432721540203998 ) ) ;
#60850 = CARTESIAN_POINT ( 'NONE',  ( 4.580490334204036174, 1.208584658811951762, -1.545285769342201965 ) ) ;
#60852 = CARTESIAN_POINT ( 'NONE',  ( -6.561783159334145132, 6.757761228752363181, -0.7216878364870278340 ) ) ;
#60851 = CARTESIAN_POINT ( 'NONE',  ( 9.029367117021314115, 12.51771682229149008, -1.082531754730543083 ) ) ;
#60853 = CARTESIAN_POINT ( 'NONE',  ( 0.000000000000000000, 3.000000000000002665, 0.000000000000000000 ) ) ;
#60854 = CARTESIAN_POINT ( 'NONE',  ( 6.098944901167723032, 1.854799121126067485, -1.295245758874500996 ) ) ;
#60855 = AXIS2_PLACEMENT_3D ( 'NONE', #183452, #200746, #50266 ) ;
#60856 = CARTESIAN_POINT ( 'NONE',  ( 2.523947517756039982, 2.023366295090854194, -0.3999800566471324315 ) ) ;
#60857 = CARTESIAN_POINT ( 'NONE',  ( -6.507023659554960204, 9.678945805201045971, 1.199719254218452047 ) ) ;
#60858 = TOROIDAL_SURFACE ( 'NONE', #116269, 6.330000000000000959, 0.08000000000000000167 ) ;
#60859 = ORIENTED_EDGE ( 'NONE', *, *, #213533, .F. ) ;
#60860 = CARTESIAN_POINT ( 'NONE',  ( -1.201851678989727383E-14, 1.743750000682815493, 1.732050807568877637 ) ) ;
#60861 = CARTESIAN_POINT ( 'NONE',  ( 4.217926093758464390, -0.9595593063399066036, -1.605508702137818045 ) ) ;
#60862 = CARTESIAN_POINT ( 'NONE',  ( 2.390900936787855091, -0.6653014413638760338, -1.601662460290956380 ) ) ;
#60863 = CARTESIAN_POINT ( 'NONE',  ( 5.952700804540857149, -1.878875186057769486, -1.127905468421293689 ) ) ;
#60864 = CARTESIAN_POINT ( 'NONE',  ( 0.7630613749609324037, -1.597064910551798667, 1.523150255686569254 ) ) ;
#60865 = CARTESIAN_POINT ( 'NONE',  ( 3.608425205800522839, -0.8741791752944136906, -1.977237025433141504 ) ) ;
#60866 = CARTESIAN_POINT ( 'NONE',  ( 5.191327941051770978, -0.6971716684453888035, 1.812662890818200756 ) ) ;
#60869 = ORIENTED_EDGE ( 'NONE', *, *, #192668, .T. ) ;
#60868 = UNCERTAINTY_MEASURE_WITH_UNIT (LENGTH_MEASURE( 1.000000000000000082E-05 ), #184179, 'distance_accuracy_value', 'NONE');
#60867 = CARTESIAN_POINT ( 'NONE',  ( 0.000000000000000000, -3.499999999999999556, 0.000000000000000000 ) ) ;
#60870 = CARTESIAN_POINT ( 'NONE',  ( 0.000000000000000000, -7.246166700194011767, 9.579665964935665912 ) ) ;
#60871 = EDGE_CURVE ( 'NONE', #142717, #34845, #87093, .T. ) ;
#60872 = DIRECTION ( 'NONE',  ( 0.000000000000000000, 0.000000000000000000, 1.000000000000000000 ) ) ;
#60873 = CARTESIAN_POINT ( 'NONE',  ( -1.360316468750006225, 2.640625000341401130, 3.469446951953614189E-15 ) ) ;
#60874 = CARTESIAN_POINT ( 'NONE',  ( 5.502577337681268332, -1.966645332631598908, 0.4444998760482973821 ) ) ;
#60875 = CARTESIAN_POINT ( 'NONE',  ( -7.330154606482786050, 11.70359747420527619, 0.000000000000000000 ) ) ;
#60876 = CARTESIAN_POINT ( 'NONE',  ( 7.579171565239241737, 8.801120566655981747, 1.199719254218462483 ) ) ;
#60877 = DIRECTION ( 'NONE',  ( 0.000000000000000000, -1.000000000000000000, 0.000000000000000000 ) ) ;
#60878 = CARTESIAN_POINT ( 'NONE',  ( 3.351995281737112364, 1.825872481133209879, -0.0009662468829912954560 ) ) ;
#60879 = CARTESIAN_POINT ( 'NONE',  ( 1.712255133470397261, -2.190042126362458319, 0.2705847154940849153 ) ) ;
#60880 = ORIENTED_EDGE ( 'NONE', *, *, #13865, .F. ) ;
#60881 = CARTESIAN_POINT ( 'NONE',  ( -4.462041952228944730, 7.259447140025469203, -1.082531754730549967 ) ) ;
#60882 = CARTESIAN_POINT ( 'NONE',  ( 1.642778471875001811, -3.230208332855373676, 2.845375778867859751 ) ) ;
#60883 = CARTESIAN_POINT ( 'NONE',  ( -8.843996274815957293, 9.212417163573759282, 1.040834085586084257E-14 ) ) ;
#60884 = CARTESIAN_POINT ( 'NONE',  ( 0.6858141477139628739, 1.945346236745447488, -0.5429362378739016615 ) ) ;
#60885 = CARTESIAN_POINT ( 'NONE',  ( 1.243013918421622455, 2.044566944090483229, 0.5621290157047582614 ) ) ;
#60886 = CARTESIAN_POINT ( 'NONE',  ( 0.9999999999999833467, 9.200000000000018829, 0.4000000000000144551 ) ) ;
#60887 = CARTESIAN_POINT ( 'NONE',  ( -5.581116510680924847, 6.540332679663050541, -1.199719254218453823 ) ) ;
#60888 = CARTESIAN_POINT ( 'NONE',  ( 1.797469275952040979, -1.343413903288761313, -1.288013994602929646 ) ) ;
#60889 = CARTESIAN_POINT ( 'NONE',  ( 4.192495815123822744, 5.914331089109666983, -1.599625672291255185 ) ) ;
#60890 = CARTESIAN_POINT ( 'NONE',  ( 1.077287230265553397, -0.05381693868444264311, -2.161191418701657430 ) ) ;
#60891 = CARTESIAN_POINT ( 'NONE',  ( 5.783827325522512552, 1.646840809264274119, -1.163266671679111353 ) ) ;
#60892 = ORIENTED_EDGE ( 'NONE', *, *, #76698, .T. ) ;
#60893 = CARTESIAN_POINT ( 'NONE',  ( -4.608882153641705059, 7.464447381635583412, -1.199719254218452047 ) ) ;
#60894 = CARTESIAN_POINT ( 'NONE',  ( 3.147653791585693028, 8.999999999999998224, 2.419999999999999485 ) ) ;
#60895 = CARTESIAN_POINT ( 'NONE',  ( 3.791466046568803705, 1.323482414808102137, 1.257835202898072380 ) ) ;
#60896 = MECHANICAL_DESIGN_GEOMETRIC_PRESENTATION_REPRESENTATION (  '', ( #33216 ), #19282 ) ;
#60899 = ORIENTED_EDGE ( 'NONE', *, *, #147535, .T. ) ;
#60898 = CARTESIAN_POINT ( 'NONE',  ( -4.798872725802947770, 6.964071866812478362, -1.434128239971976138 ) ) ;
#60897 = CARTESIAN_POINT ( 'NONE',  ( -4.294900800479008574, 8.232744377192641849, 0.000000000000000000 ) ) ;
#60900 = CARTESIAN_POINT ( 'NONE',  ( 5.796475149741596056, 7.337953333587568849, -1.293683646293428913 ) ) ;
#60901 = CARTESIAN_POINT ( 'NONE',  ( 6.222029796014385106, -1.727739227931901489, -1.038831587593692873 ) ) ;
#60902 = CARTESIAN_POINT ( 'NONE',  ( 6.035073252477260120, -1.336788798515762489, -1.266260169258619284 ) ) ;
#60903 = CARTESIAN_POINT ( 'NONE',  ( -10.99976498415366954, -5.359187537802505119, 0.08336379702154585181 ) ) ;
#60904 = CARTESIAN_POINT ( 'NONE',  ( 4.160959874251066282, -1.711463231979272859, 1.548185629304731581 ) ) ;
#60905 = CARTESIAN_POINT ( 'NONE',  ( 6.017840079619279692, 8.114175741012878973, -1.599625672291281386 ) ) ;
#60906 = CARTESIAN_POINT ( 'NONE',  ( 6.134075720976177593, 1.071308383804179476, -1.877395391766012445 ) ) ;
#60907 = CARTESIAN_POINT ( 'NONE',  ( 7.305145839664861640, 7.417091655897478653, 0.7998128361456341429 ) ) ;
#60908 = CARTESIAN_POINT ( 'NONE',  ( 1.927192517792934101, -1.269957001497720395, -1.469349730274618571 ) ) ;
#60909 = CARTESIAN_POINT ( 'NONE',  ( 4.745672437882476835, -2.227950070917711134, -0.5642311211754289513 ) ) ;
#60910 = CARTESIAN_POINT ( 'NONE',  ( 1.854049621773927514, 5.499999999999998224, 0.7500000000000006661 ) ) ;
#60911 = CARTESIAN_POINT ( 'NONE',  ( -5.887983850084758330, 10.09134126839936840, 0.7998128361456291469 ) ) ;
#60912 = AXIS2_PLACEMENT_3D ( 'NONE', #150577, #70342, #21582 ) ;
#60913 = CARTESIAN_POINT ( 'NONE',  ( 4.469519713540137218, 1.814478506493342191, -0.4545110902946307152 ) ) ;
#60914 = VERTEX_POINT ( 'NONE', #201479 ) ;
#60917 = CARTESIAN_POINT ( 'NONE',  ( -5.041653019435350380, 6.975290837464928728, -1.599625672291271394 ) ) ;
#60916 = CARTESIAN_POINT ( 'NONE',  ( -1.500000000000015099, 0.1604166673494879791, -0.8660254037844383745 ) ) ;
#60915 = CARTESIAN_POINT ( 'NONE',  ( 2.830216799141628492, -0.9462872844297947061, -1.661813493071498726 ) ) ;
#60918 = CARTESIAN_POINT ( 'NONE',  ( 3.598431038176507002, -2.204323482753521635, -0.1086902067785888437 ) ) ;
#60919 = EDGE_CURVE ( 'NONE', #41604, #21324, #170115, .T. ) ;
#60920 = CARTESIAN_POINT ( 'NONE',  ( 6.983263157960370116, 1.266851337794393961, 2.060309365732877485 ) ) ;
#60921 = CARTESIAN_POINT ( 'NONE',  ( 4.041739190205284160, 7.729463131965888856, 0.000000000000000000 ) ) ;
#60922 = AXIS2_PLACEMENT_3D ( 'NONE', #87947, #187569, #141011 ) ;
#60923 = CARTESIAN_POINT ( 'NONE',  ( -4.624739795592931912, 8.409630504918133909, -0.7216878364870338292 ) ) ;
#60924 = CARTESIAN_POINT ( 'NONE',  ( 1.651575284419577461, 0.5759676520707255332, -1.885319811257283096 ) ) ;
#60925 = CARTESIAN_POINT ( 'NONE',  ( 1.589377644589501148, -0.3404682245478432567, -2.282209529656929803 ) ) ;
#60926 = CARTESIAN_POINT ( 'NONE',  ( 2.857805160684105950, -0.6180756922911297968, 1.862011555624979886 ) ) ;
#60927 = CARTESIAN_POINT ( 'NONE',  ( 11.33772463945037146, 10.89999999999998259, 3.599999999999999201 ) ) ;
#60928 = CARTESIAN_POINT ( 'NONE',  ( 6.842638575262629530, -2.021612500624434539, -0.4081942145969327251 ) ) ;
#60929 = CARTESIAN_POINT ( 'NONE',  ( 5.043269954603547767, 4.986162489899998995, -0.7216878364870197293 ) ) ;
#60930 = CARTESIAN_POINT ( 'NONE',  ( 3.766814776335784209, -0.2024620155892907503, -2.006371719556559796 ) ) ;
#60931 = CARTESIAN_POINT ( 'NONE',  ( 6.066347387471824781, 6.042103138330730872, -0.7998128361456481317 ) ) ;
#60932 = ORIENTED_EDGE ( 'NONE', *, *, #196420, .F. ) ;
#60933 = CARTESIAN_POINT ( 'NONE',  ( -10.48453286206953727, 11.12637651536962125, 0.7998128361456462443 ) ) ;
#60934 = CARTESIAN_POINT ( 'NONE',  ( -1.499999999999963141, 7.750000000000000000, 10.99818166789402341 ) ) ;
#60935 = CARTESIAN_POINT ( 'NONE',  ( 8.387690588348714726, 12.93738945304888333, 1.040834085586084257E-14 ) ) ;
#60936 = CARTESIAN_POINT ( 'NONE',  ( 1.991327249661909882, 0.2097703728867078010, 2.160876515670279385 ) ) ;
#60937 = CARTESIAN_POINT ( 'NONE',  ( 5.448397627845284141, 7.449826213943242514, 1.599625672291268286 ) ) ;
#60938 = EDGE_CURVE ( 'NONE', #21699, #12172, #94074, .T. ) ;
#60939 = CARTESIAN_POINT ( 'NONE',  ( 11.33772465723203915, 11.00868300734825667, -3.600000000000076472 ) ) ;
#60940 = CARTESIAN_POINT ( 'NONE',  ( -6.042630808230841359E-15, -1.662500000000000533, 3.474999999999999645 ) ) ;
#60941 = CARTESIAN_POINT ( 'NONE',  ( 2.741296213614560440, -1.383352855433259698, -1.259238407996167153 ) ) ;
#60942 = CARTESIAN_POINT ( 'NONE',  ( 6.819591527820957566, -2.098570527662356522, 0.5178885164088961046 ) ) ;
#60944 = CARTESIAN_POINT ( 'NONE',  ( 6.727182134110186063, 1.310238205575515957, 1.828849833172506489 ) ) ;
#60943 = DIRECTION ( 'NONE',  ( 5.551115123125764829E-17, 0.000000000000000000, -1.000000000000000000 ) ) ;
#60945 = CARTESIAN_POINT ( 'NONE',  ( 1.364683531249986537, -0.6364583329919177856, 0.7879004041258500513 ) ) ;
#60946 = CARTESIAN_POINT ( 'NONE',  ( -1.493107181547909557, 3.264587186353522519, 0.1630395111544278020 ) ) ;
#60947 = CARTESIAN_POINT ( 'NONE',  ( 2.490748672031910083, -1.830495558572857728, -0.5533032672612181457 ) ) ;
#60948 = CARTESIAN_POINT ( 'NONE',  ( 4.715556530927702106, -1.735345248271908947, 0.3467660769565800161 ) ) ;
#60949 = CARTESIAN_POINT ( 'NONE',  ( 1.312987857083922627, 1.562780923097413677, -1.101767902142808175 ) ) ;
#60950 = CARTESIAN_POINT ( 'NONE',  ( -6.417086777969760902, 6.381022750586497594, 0.7998128361456341429 ) ) ;
#60952 = CARTESIAN_POINT ( 'NONE',  ( 6.362892188913578551, -0.09940890854263698118, -1.913169475778592865 ) ) ;
#60951 = FACE_OUTER_BOUND ( 'NONE', #7194, .T. ) ;
#60953 = CARTESIAN_POINT ( 'NONE',  ( 1.499999999999987566, -0.7249999999999825473, 0.000000000000000000 ) ) ;
#60954 = CARTESIAN_POINT ( 'NONE',  ( 0.8013346216862862192, -1.776568573310655985, 1.062853015585236482 ) ) ;
#60955 = CARTESIAN_POINT ( 'NONE',  ( -1.500000000000011324, 5.379166666666692187, -0.8660254037844313801 ) ) ;
#60956 = CARTESIAN_POINT ( 'NONE',  ( -1.772826578343126736, 4.000000000000003553, 0.4499999999999538813 ) ) ;
#60957 = CARTESIAN_POINT ( 'NONE',  ( 5.576977133510579776, -0.04717937999037385977, -1.870219006134994588 ) ) ;
#60958 = CARTESIAN_POINT ( 'NONE',  ( 1.734698295210383767, 0.1775668987445792879, 1.817036636966688823 ) ) ;
#60960 = CARTESIAN_POINT ( 'NONE',  ( 4.943016831304842817, 7.975319854387232787, 1.017975537214605319 ) ) ;
#60959 = CARTESIAN_POINT ( 'NONE',  ( 5.373716497573798101, 2.127666891504222058, -0.5857064233696291922 ) ) ;
#60961 = CARTESIAN_POINT ( 'NONE',  ( -1.364683531250000748, -0.4906249996585801409, 0.000000000000000000 ) ) ;
#60962 = CARTESIAN_POINT ( 'NONE',  ( 2.523947517756039982, 2.023366295090854194, -0.3999800566471324315 ) ) ;
#60963 = CARTESIAN_POINT ( 'NONE',  ( -7.690499447449645309, 9.995335326823163058, 1.599625672291295375 ) ) ;
#60964 = CARTESIAN_POINT ( 'NONE',  ( 6.610000000000028741, 4.695285100415147461, 2.562642482393460597 ) ) ;
#60965 = CARTESIAN_POINT ( 'NONE',  ( 1.392149563160024694, 3.364880846494863853, -0.1376214334732262790 ) ) ;
#60966 = ADVANCED_FACE ( 'NONE', ( #67210 ), #52065, .T. ) ;
#60967 = CARTESIAN_POINT ( 'NONE',  ( 7.042534447655770080, 7.180988041878682004, -0.7998128361456341429 ) ) ;
#60968 = ORIENTED_EDGE ( 'NONE', *, *, #86369, .F. ) ;
#60969 = CARTESIAN_POINT ( 'NONE',  ( 5.494608840674215955, 2.039112051642687717, 0.3575134270455831986 ) ) ;
#60970 = CARTESIAN_POINT ( 'NONE',  ( -1.402160292154681736E-14, 0.6343750003414162508, 1.575800808251672791 ) ) ;
#60971 = CARTESIAN_POINT ( 'NONE',  ( 2.390102426918311540, -0.9266024157483061519, 1.953076554623616401 ) ) ;
#60972 = CARTESIAN_POINT ( 'NONE',  ( -4.807049873888117553, 8.139959938814184781, 0.8294007104595437774 ) ) ;
#60973 = CARTESIAN_POINT ( 'NONE',  ( 2.877608074518396286, 0.2940240112025078179, -1.998017427383149913 ) ) ;
#60974 = CARTESIAN_POINT ( 'NONE',  ( 7.446209719563365859, -5.223431457505076203, 8.064677165291195493 ) ) ;
#60975 = PRODUCT ( 'isolation positive negative', 'isolation positive negative', '', ( #213993 ) ) ;
#60976 = ORIENTED_EDGE ( 'NONE', *, *, #122928, .F. ) ;
#60979 = CARTESIAN_POINT ( 'NONE',  ( 8.107412671292042461, 9.521364873671299023, 1.082531754730558626 ) ) ;
#60978 = CARTESIAN_POINT ( 'NONE',  ( -1.737499999999997824, -1.691666666666667762, 3.009438278150925683 ) ) ;
#60977 = CARTESIAN_POINT ( 'NONE',  ( -1.499999999999997780, 3.681250000682819046, 1.214306433183764966E-14 ) ) ;
#60980 = CARTESIAN_POINT ( 'NONE',  ( -4.950135482320939140, 4.947781948895412008, -0.7216878364870338292 ) ) ;
#60981 = CARTESIAN_POINT ( 'NONE',  ( 1.534389036647098692, 0.6371565916030231813, 1.913260934284975345 ) ) ;
#60983 = CARTESIAN_POINT ( 'NONE',  ( 6.128506746050899068, 0.2130254606748181456, 2.181202035047181020 ) ) ;
#60982 = CARTESIAN_POINT ( 'NONE',  ( -5.229694566569281555, 7.124396299129368337, 1.599625672291267398 ) ) ;
#60985 =( GEOMETRIC_REPRESENTATION_CONTEXT ( 3 ) GLOBAL_UNCERTAINTY_ASSIGNED_CONTEXT ( ( #127554 ) ) GLOBAL_UNIT_ASSIGNED_CONTEXT ( ( #74308, #157701, #205349 ) ) REPRESENTATION_CONTEXT ( 'NONE', 'WORKASPACE' ) );
#60984 = CARTESIAN_POINT ( 'NONE',  ( -1.201851678989727383E-14, 5.368750000682816825, -1.732050807568863648 ) ) ;
#60986 = CARTESIAN_POINT ( 'NONE',  ( 5.027564050633359649, -0.2746679736120913318, 1.892429487827557599 ) ) ;
#60987 = CARTESIAN_POINT ( 'NONE',  ( -4.253507506385335368, 5.985511395581417204, 1.599625672291267398 ) ) ;
#60988 = CARTESIAN_POINT ( 'NONE',  ( 5.951666246274792016, 8.927065806420504401, 1.082531754730558626 ) ) ;
#60990 = CARTESIAN_POINT ( 'NONE',  ( 2.987907820627898836, -2.013986125068282007, 0.1017690403029153645 ) ) ;
#60989 = CARTESIAN_POINT ( 'NONE',  ( -9.964879715919934711, 10.72804054476916313, 0.7216878364870438212 ) ) ;
#60991 = CARTESIAN_POINT ( 'NONE',  ( 1.364683531249997417, 13.79687500034139980, 2.602085213965210642E-15 ) ) ;
#60992 = CARTESIAN_POINT ( 'NONE',  ( -4.625266680917477835, 5.425174544939014964, -1.199719254218453823 ) ) ;
#60993 = CARTESIAN_POINT ( 'NONE',  ( 5.772382705887088683, -1.090832958316660273, 1.335977363661453809 ) ) ;
#60994 = CARTESIAN_POINT ( 'NONE',  ( 7.049313524462606395, 7.188896964819984525, 0.000000000000000000 ) ) ;
#60995 = CARTESIAN_POINT ( 'NONE',  ( 8.419250204406344196, 12.76628297187536809, 1.040834085586084257E-14 ) ) ;
#60996 = LINE ( 'NONE', #44770, #206068 ) ;
#60997 = CARTESIAN_POINT ( 'NONE',  ( 4.464026755505964950, 0.8799173153972823513, 1.650629236088823282 ) ) ;
#60998 = DIRECTION ( 'NONE',  ( -1.000000000000000000, 0.000000000000000000, 0.000000000000000000 ) ) ;
#60999 = CARTESIAN_POINT ( 'NONE',  ( 1.147426569842596722, 1.827566109494669577, -0.9725325914680116313 ) ) ;
#61000 = ORIENTED_EDGE ( 'NONE', *, *, #45759, .T. ) ;
#61001 = CARTESIAN_POINT ( 'NONE',  ( 5.883446949022190786, 0.1262479900229801499, -1.807133042791621458 ) ) ;
#61002 = CARTESIAN_POINT ( 'NONE',  ( 5.727393547130178675, 5.646656991265468939, 0.000000000000000000 ) ) ;
#61003 = CARTESIAN_POINT ( 'NONE',  ( -0.1407840215364779823, -1.400018645128609629, -1.149511601580233577 ) ) ;
#61004 = CARTESIAN_POINT ( 'NONE',  ( 4.217995187182915551, 7.935095128439824563, 0.7216878364870257245 ) ) ;
#61005 = CARTESIAN_POINT ( 'NONE',  ( 11.95247249465994166, 7.720304541436361134, -1.088600100142860017 ) ) ;
#61006 = CARTESIAN_POINT ( 'NONE',  ( 2.976726284633357533, -0.1618151936485581754, -2.185533650236513914 ) ) ;
#61007 = ORIENTED_EDGE ( 'NONE', *, *, #161592, .F. ) ;
#61008 = AXIS2_PLACEMENT_3D ( 'NONE', #41286, #75891, #106312 ) ;
#61010 = CARTESIAN_POINT ( 'NONE',  ( 9.077347539549325717, 10.54899253668443393, -1.199719254218446718 ) ) ;
#61009 = CARTESIAN_POINT ( 'NONE',  ( 0.4671467121175364445, 1.705069321186868159, 0.9702857188121425391 ) ) ;
#61011 = CARTESIAN_POINT ( 'NONE',  ( 4.903869178324737454, -1.028422014321051403, -1.615943446245589943 ) ) ;
#61012 = CARTESIAN_POINT ( 'NONE',  ( 10.50000000000000178, 10.19999999999999929, -3.600000000000000977 ) ) ;
#61013 = CARTESIAN_POINT ( 'NONE',  ( -5.679286501732877745, 7.334821546209805199, 1.225395024417414103 ) ) ;
#61014 = CARTESIAN_POINT ( 'NONE',  ( 0.6124999999999967137, 0.5833333333333314830, 1.060881119635929348 ) ) ;
#61015 = CARTESIAN_POINT ( 'NONE',  ( -0.6823417656250246877, 0.05104166700808931978, 1.181850606188755259 ) ) ;
#61017 = ORIENTED_EDGE ( 'NONE', *, *, #172073, .T. ) ;
#61016 = CARTESIAN_POINT ( 'NONE',  ( 6.005898861173831094, 6.109229547565340646, 1.040834085586084257E-14 ) ) ;
#61018 = CARTESIAN_POINT ( 'NONE',  ( -7.361714222540411967, 11.53249099303175385, 0.000000000000000000 ) ) ;
#61019 = CARTESIAN_POINT ( 'NONE',  ( 1.358524781292804517, 0.8764843271744371389, 1.976213614152767750 ) ) ;
#61020 = CARTESIAN_POINT ( 'NONE',  ( -5.147255595043616516, 6.034161611419515125, 1.199719254218452935 ) ) ;
#61021 = CARTESIAN_POINT ( 'NONE',  ( 6.482206841109512396, 9.616306177052839743, -1.082531754730548412 ) ) ;
#61022 = CARTESIAN_POINT ( 'NONE',  ( -4.613852347352193739, 4.277249248199312071, 1.214306433183764966E-14 ) ) ;
#61023 = CARTESIAN_POINT ( 'NONE',  ( 4.577060434696750946, -0.0006114206978560799951, -1.825762228460731551 ) ) ;
#61024 = CARTESIAN_POINT ( 'NONE',  ( 11.74001039742577923, 6.813547096158895755, 0.9622183096568183158 ) ) ;
#61025 = CARTESIAN_POINT ( 'NONE',  ( 1.563680990848853591, 1.942865793614118930, -0.3330471066002506642 ) ) ;
#61026 = CARTESIAN_POINT ( 'NONE',  ( 3.709155072767254868, 1.612916391665040416, -1.027221078234448859 ) ) ;
#61027 = ORIENTED_EDGE ( 'NONE', *, *, #166608, .F. ) ;
#61028 = CARTESIAN_POINT ( 'NONE',  ( 4.070725410728625704, 1.394476139410082638, -1.391156265790331581 ) ) ;
#61029 = EDGE_LOOP ( 'NONE', ( #181679, #7994, #48012, #110704 ) ) ;
#61030 = CARTESIAN_POINT ( 'NONE',  ( 5.724156413028869572, 1.872829174467111946, 0.5137480774947185136 ) ) ;
#61031 = ORIENTED_EDGE ( 'NONE', *, *, #108300, .F. ) ;
#61032 = CARTESIAN_POINT ( 'NONE',  ( -5.250750630242457362, 9.347902511916677426, 0.000000000000000000 ) ) ;
#61034 = CARTESIAN_POINT ( 'NONE',  ( 5.853796514643677007, -1.537196951383312804, -1.461068456062891041 ) ) ;
#61033 = CARTESIAN_POINT ( 'NONE',  ( -3.949167883330528372, 7.829389307186077396, 1.214306433183764966E-14 ) ) ;
#61035 = CARTESIAN_POINT ( 'NONE',  ( 7.336370518326124746, 7.731722824234849689, -0.7216878364870317197 ) ) ;
#61036 = CARTESIAN_POINT ( 'NONE',  ( 4.266199323752727146, 1.911794059647478949, -0.05023246155653331158 ) ) ;
#61037 = CARTESIAN_POINT ( 'NONE',  ( 4.628062896017484995, 7.124942365035781933, -1.349859865738218145 ) ) ;
#61038 = FACE_OUTER_BOUND ( 'NONE', #206890, .T. ) ;
#61039 = LINE ( 'NONE', #179071, #171447 ) ;
#61040 = LINE ( 'NONE', #197165, #27178 ) ;
#61041 = CARTESIAN_POINT ( 'NONE',  ( 5.514319586171100518, -2.013265972089046230, 0.002284521408187425995 ) ) ;
#61042 = CARTESIAN_POINT ( 'NONE',  ( -10.99943592164172834, -9.900000000000005684, 0.1113975120798846308 ) ) ;
#61043 = CARTESIAN_POINT ( 'NONE',  ( 5.830640656690653678, 1.760721658632548037, 0.4824517239352192344 ) ) ;
#61044 = CARTESIAN_POINT ( 'NONE',  ( 2.189971326302230903, -1.350648006375281929, -1.569233719104834890 ) ) ;
#61045 = CARTESIAN_POINT ( 'NONE',  ( -8.703971430293361067, 9.256980878204810637, 0.7216878364870438212 ) ) ;
#61046 = VECTOR ( 'NONE', #183267, 1000.000000000000000 ) ;
#61047 = CARTESIAN_POINT ( 'NONE',  ( -5.717536675473545493, 7.305230138711669596, -1.214019596050613492 ) ) ;
#61048 = CARTESIAN_POINT ( 'NONE',  ( -0.6125000000000053735, 2.020833334016133964, -1.060881119635941339 ) ) ;
#61049 = CARTESIAN_POINT ( 'NONE',  ( -3.285556943750000070, -2.909374999522040817, 0.000000000000000000 ) ) ;
#61050 = CARTESIAN_POINT ( 'NONE',  ( 5.666418135507635512, 8.698239360479199433, 1.199719254218462483 ) ) ;
#61052 = EDGE_CURVE ( 'NONE', #60728, #156131, #84555, .T. ) ;
#61051 = CIRCLE ( 'NONE', #88742, 0.08000000000000009881 ) ;
#61053 = CARTESIAN_POINT ( 'NONE',  ( 3.379006598303866848, 4.965260336153046516, -1.599625672291262513 ) ) ;
#61054 = CARTESIAN_POINT ( 'NONE',  ( 1.364683531250000303, 11.31770833367473550, -0.7879004041258355073 ) ) ;
#61055 = CARTESIAN_POINT ( 'NONE',  ( -4.569261463005423352, 5.289558780716470565, -1.199719254218446718 ) ) ;
#61057 = CARTESIAN_POINT ( 'NONE',  ( -8.120407659942227241, 8.438506789546210030, 0.7998128361456341429 ) ) ;
#61056 = CARTESIAN_POINT ( 'NONE',  ( 7.580882385732278905, -6.105993949506924423, -7.580882385732309103 ) ) ;
#61058 = CARTESIAN_POINT ( 'NONE',  ( 3.850049338483009009, 0.2070581644968480517, -1.721641829124469059 ) ) ;
#61059 = CARTESIAN_POINT ( 'NONE',  ( -3.418627288940168096, 7.140148937072163804, -0.7998128361456281477 ) ) ;
#61060 = CARTESIAN_POINT ( 'NONE',  ( 0.9540663221972445207, -0.7486024665571254788, 1.930331157511067097 ) ) ;
#61061 = CARTESIAN_POINT ( 'NONE',  ( 3.655961130333235776, 1.178038043211126817, 1.759042251235248600 ) ) ;
#61062 = CARTESIAN_POINT ( 'NONE',  ( 4.355193658487811703, 6.104145239700998538, -1.599625672291255185 ) ) ;
#61063 = CARTESIAN_POINT ( 'NONE',  ( 8.589254009457354400, 9.979550084910457031, -1.199719254218446718 ) ) ;
#61064 = CARTESIAN_POINT ( 'NONE',  ( 0.1851009548687417572, 6.360931694699415218, 3.114575592932423476 ) ) ;
#61065 = CARTESIAN_POINT ( 'NONE',  ( 0.3034763168169403169, -1.518637222489120919, -1.253724199518479354 ) ) ;
#61066 = CARTESIAN_POINT ( 'NONE',  ( 4.901917485988815493, 6.882077164048857831, 1.422854466155202502 ) ) ;
#61067 = CARTESIAN_POINT ( 'NONE',  ( 4.744990575102895569, 5.598539094783909320, -1.082531754730548412 ) ) ;
#61069 = CARTESIAN_POINT ( 'NONE',  ( 5.626270559546852290, 5.666329862333807199, 0.7216878364870122908 ) ) ;
#61068 = CARTESIAN_POINT ( 'NONE',  ( -3.474999999999998312, -2.070833333333331971, 2.006292185433951047 ) ) ;
#61070 = CARTESIAN_POINT ( 'NONE',  ( 3.697495799125404492, -0.6661743112182354487, 2.193330854740268343 ) ) ;
#61071 = CARTESIAN_POINT ( 'NONE',  ( 0.2932112110246976044, 1.350478442433366677, 1.228755397233910696 ) ) ;
#61072 = CARTESIAN_POINT ( 'NONE',  ( 3.621269620730773298, 1.642686141288721480, 0.9789267784374030557 ) ) ;
#61073 = CARTESIAN_POINT ( 'NONE',  ( 6.638652492546827766, 7.774124658506663010, 1.199719254218452047 ) ) ;
#61074 = CARTESIAN_POINT ( 'NONE',  ( 7.592202833528386208, 7.959917515312338487, 1.040834085586084257E-14 ) ) ;
#61075 = CARTESIAN_POINT ( 'NONE',  ( -9.820183334999905256, 10.35130206712171130, 1.040834085586084257E-14 ) ) ;
#61076 = CARTESIAN_POINT ( 'NONE',  ( 1.617441171277278711, 1.676116182522195519, 1.114898189108826543 ) ) ;
#61077 = CARTESIAN_POINT ( 'NONE',  ( 1.762477828903946442, -0.7011357286515782494, -1.832381215946830011 ) ) ;
#61078 = CARTESIAN_POINT ( 'NONE',  ( -8.839026081105473054, 12.39961529701003684, -1.199719254218446718 ) ) ;
#61079 = CARTESIAN_POINT ( 'NONE',  ( -5.554036483092550824, 9.631459663583308739, -0.7998128361456231517 ) ) ;
#61080 = CARTESIAN_POINT ( 'NONE',  ( -11.07651133989102554, 5.830166859442025284, -4.512497092989907976 ) ) ;
#61083 = B_SPLINE_CURVE_WITH_KNOTS ( 'NONE', 3,
 ( #121520, #7661, #55366, #38055 ),
 .UNSPECIFIED., .F., .F.,
 ( 4, 4 ),
 ( 0.003648968938405892752, 0.004840739682861143652 ),
 .UNSPECIFIED. ) ;
#61082 = CARTESIAN_POINT ( 'NONE',  ( 3.502600007508451352, 1.395586194379776712, -1.088321832170894288 ) ) ;
#61081 = CARTESIAN_POINT ( 'NONE',  ( 5.103505634659632584, -2.080644823048905412, 0.2041521072984452956 ) ) ;
#61084 = CARTESIAN_POINT ( 'NONE',  ( -0.6125000000000158096, 0.1041666673494701101, 1.060881119635906700 ) ) ;
#61086 = CARTESIAN_POINT ( 'NONE',  ( 5.964811824374402605, 0.1744345966951440507, -2.285673535861055594 ) ) ;
#61085 = CARTESIAN_POINT ( 'NONE',  ( -8.881784197001254049E-17, 4.400000000000001243, 1.600000000000005196 ) ) ;
#61087 = CARTESIAN_POINT ( 'NONE',  ( 5.367066450689647716, 1.675684007255513475, -0.4696764748959629809 ) ) ;
#61088 = CARTESIAN_POINT ( 'NONE',  ( 10.21336978979620191, 10.81001959771741205, 0.7998128361456462443 ) ) ;
#61089 = CARTESIAN_POINT ( 'NONE',  ( -0.1104750535120043037, 1.338503269012698116, -2.356272470560859755 ) ) ;
#61090 = CARTESIAN_POINT ( 'NONE',  ( 4.305767739847966347, -1.508829150093475180, 0.8539562774845139703 ) ) ;
#61091 = CARTESIAN_POINT ( 'NONE',  ( 5.916515574059204141, 0.8745146271147998807, 1.987442084954823773 ) ) ;
#61092 = CARTESIAN_POINT ( 'NONE',  ( 4.220665892555866883, 3.818531717603609987, -0.7998128361456211532 ) ) ;
#61093 = CARTESIAN_POINT ( 'NONE',  ( 0.4974488191052604535, -0.3042024069639309158, 2.095249342460514086 ) ) ;
#61094 = CARTESIAN_POINT ( 'NONE',  ( 5.843750000000004441, 1.895863743164205140, 0.7852924748296741253 ) ) ;
#61095 = CARTESIAN_POINT ( 'NONE',  ( 0.000000000000000000, 0.000000000000000000, -0.5000000000000004441 ) ) ;
#61096 = CARTESIAN_POINT ( 'NONE',  ( 3.416937173653651794, 1.740928992956072952, 0.8250102540389223638 ) ) ;
#61097 = CARTESIAN_POINT ( 'NONE',  ( -1.500000000000001110, 11.80208333401613352, 0.8660254037844419273 ) ) ;
#61098 = CARTESIAN_POINT ( 'NONE',  ( 0.6279475770487872310, -0.3202071342675495425, 2.197987568497254074 ) ) ;
#61099 = ORIENTED_EDGE ( 'NONE', *, *, #115015, .T. ) ;
#61100 = CARTESIAN_POINT ( 'NONE',  ( -0.2408018239684330541, 4.084923768815020395, -2.655285172934387372 ) ) ;
#61101 = CARTESIAN_POINT ( 'NONE',  ( 1.499999999999989120, 3.525000000000021227, 1.214306433183764966E-14 ) ) ;
#61102 = CARTESIAN_POINT ( 'NONE',  ( 6.647575389402066826, 6.649926130590872120, 1.040834085586084257E-14 ) ) ;
#61103 = CARTESIAN_POINT ( 'NONE',  ( 2.983289111093189394, -2.053184633062016484, -0.8481636011889515103 ) ) ;
#61104 = CARTESIAN_POINT ( 'NONE',  ( -0.02900071798683095947, 1.997299723774683455, -2.587491137808914488 ) ) ;
#61105 = CARTESIAN_POINT ( 'NONE',  ( 8.134528978519385944, 8.592631351135175066, -0.7216878364870267237 ) ) ;
#61106 = CARTESIAN_POINT ( 'NONE',  ( -10.27671724903424888, 11.09185100006920877, 1.040834085586084257E-14 ) ) ;
#61107 = CARTESIAN_POINT ( 'NONE',  ( 4.415115299905642665, 5.179997933758551554, -1.199719254218450271 ) ) ;
#61108 = CARTESIAN_POINT ( 'NONE',  ( 0.4576579978108759050, -1.899619568183811058, -0.6767110947205197125 ) ) ;
#61110 = CARTESIAN_POINT ( 'NONE',  ( 5.248506731170051509, -2.046683549694120252, -0.2560125357965719606 ) ) ;
#61109 = CARTESIAN_POINT ( 'NONE',  ( 9.053093885623066939, 11.58502883802551153, -1.599625672291262513 ) ) ;
#61111 = CARTESIAN_POINT ( 'NONE',  ( -4.627410500965859264, 4.293067094081919777, 0.7998128361456341429 ) ) ;
#61112 = PRESENTATION_STYLE_ASSIGNMENT (( #143474 ) ) ;
#61113 = CARTESIAN_POINT ( 'NONE',  ( 0.6823417656249899377, 0.5927083336747518416, 1.181850606188755259 ) ) ;
#61114 = CARTESIAN_POINT ( 'NONE',  ( 0.5261445748756715668, 1.690971295752751624, 0.5220769596525741685 ) ) ;
#61115 = CARTESIAN_POINT ( 'NONE',  ( 6.188101721744481587, 1.447254432076927166, 0.9550205611794166938 ) ) ;
#61116 = CARTESIAN_POINT ( 'NONE',  ( 5.214300491592821274, 1.611006010870178251, 0.6591642633846701571 ) ) ;
#61117 = CARTESIAN_POINT ( 'NONE',  ( 2.560454162224240271, -1.578354536769586591, 1.662689614829175211 ) ) ;
#61118 = CARTESIAN_POINT ( 'NONE',  ( -1.364683531250014514, -0.7197916663252461600, 0.7879004041258379498 ) ) ;
#61119 = CARTESIAN_POINT ( 'NONE',  ( 2.448939195788137013, 0.4911642875529352303, -1.774347143093172097 ) ) ;
#61120 = CARTESIAN_POINT ( 'NONE',  ( 9.856941372335116469, 11.45851867493453291, 1.199719254218450271 ) ) ;
#61121 = CARTESIAN_POINT ( 'NONE',  ( -10.71870444596734195, 5.124999999999999112, 5.395310463726811001 ) ) ;
#61122 = CARTESIAN_POINT ( 'NONE',  ( 1.746812667857342349, -1.544096848276183209, 0.9736100143667850704 ) ) ;
#61123 = CARTESIAN_POINT ( 'NONE',  ( 2.602185585689294367, -0.1948409242511044692, 2.006959980107574371 ) ) ;
#61124 = CARTESIAN_POINT ( 'NONE',  ( -3.212919216314315207, 5.731860938133201522, 1.082531754730560403 ) ) ;
#61125 = DIRECTION ( 'NONE',  ( -1.000000000000000000, 0.000000000000000000, 0.000000000000000000 ) ) ;
#61126 = CARTESIAN_POINT ( 'NONE',  ( 4.401466734191799901, 1.689890445582131084, 1.256493114684479329 ) ) ;
#61127 = CARTESIAN_POINT ( 'NONE',  ( -7.400052914960538963, 7.527816577075747695, 1.040834085586084257E-14 ) ) ;
#61128 = CARTESIAN_POINT ( 'NONE',  ( 8.806674072578211110, 13.38234123322611779, 7.683694639725048958 ) ) ;
#61129 = CARTESIAN_POINT ( 'NONE',  ( 2.629418614236479712, 0.1040367438073786233, -2.067886086930009970 ) ) ;
#61130 = CARTESIAN_POINT ( 'NONE',  ( 4.976006071415387311, 5.764094157194782575, 1.199719254218462483 ) ) ;
#61131 = CARTESIAN_POINT ( 'NONE',  ( -1.360316468750042862, 0.1510416670080827195, -0.7853790794159282163 ) ) ;
#61132 = CARTESIAN_POINT ( 'NONE',  ( 4.442108405842562391, -1.305342523080333272, -1.670987904322115636 ) ) ;
#61133 = CARTESIAN_POINT ( 'NONE',  ( 6.533835636172961259, -1.196796279342365210, -1.378804128639096849 ) ) ;
#61134 = ORIENTED_EDGE ( 'NONE', *, *, #161956, .F. ) ;
#61135 = CARTESIAN_POINT ( 'NONE',  ( -4.980641328173854632, 6.904110530993182948, 1.599625672291263179 ) ) ;
#61136 = CARTESIAN_POINT ( 'NONE',  ( 10.39640486358069360, 11.02356051713265650, 0.7998128361456462443 ) ) ;
#61137 = CARTESIAN_POINT ( 'NONE',  ( 4.516274566683592617, 8.283087737857252719, -0.7216878364870357165 ) ) ;
#61138 = CARTESIAN_POINT ( 'NONE',  ( 3.475000000000000533, -1.502083332377415870, -2.006292185433951047 ) ) ;
#61139 = CARTESIAN_POINT ( 'NONE',  ( -4.934277840369690971, 7.844075682818238526, -1.199719254218452047 ) ) ;
#61140 = CARTESIAN_POINT ( 'NONE',  ( 6.275647701495586261, 0.3610785225884837746, -2.089460823871174266 ) ) ;
#61141 = CARTESIAN_POINT ( 'NONE',  ( 1.044129769988952683, 0.8535497088724073311, -1.925424821390888663 ) ) ;
#61142 = CARTESIAN_POINT ( 'NONE',  ( -5.224688093219839402, 7.188831756880171397, -1.599625672291271394 ) ) ;
#61143 = CARTESIAN_POINT ( 'NONE',  ( 7.242026607993941489, 11.60078147596829901, 0.7998128361456462443 ) ) ;
#61144 = CARTESIAN_POINT ( 'NONE',  ( 6.069184012654499583, 1.640672622335254793, 0.8782983229575453965 ) ) ;
#61145 = CARTESIAN_POINT ( 'NONE',  ( 6.577677080924314801, 10.82570702772039262, 1.040834085586084257E-14 ) ) ;
#61146 = DIRECTION ( 'NONE',  ( 0.000000000000000000, 1.000000000000000000, 0.000000000000000000 ) ) ;
#61147 = CARTESIAN_POINT ( 'NONE',  ( -7.024532985656169792, 9.288650798055913427, 1.443375672974064550 ) ) ;
#61149 = ORIENTED_EDGE ( 'NONE', *, *, #159826, .F. ) ;
#61148 = CARTESIAN_POINT ( 'NONE',  ( -10.30383355670593737, 11.12348669235284504, -0.7216878364870267237 ) ) ;
#61150 = CARTESIAN_POINT ( 'NONE',  ( -1.833506991698480526, 2.501547993919093660, 2.496244204820596835 ) ) ;
#61151 = CARTESIAN_POINT ( 'NONE',  ( 1.063950011417321484, -4.204658361605590144, 0.1571845235116707262 ) ) ;
#61153 = CARTESIAN_POINT ( 'NONE',  ( 2.664445928352857429, -0.7481792696971515388, -1.813797970468238985 ) ) ;
#61152 = CARTESIAN_POINT ( 'NONE',  ( -5.994676475536691029, 10.14553965476814845, 0.7998128361456481317 ) ) ;
#61154 = CARTESIAN_POINT ( 'NONE',  ( 1.253037233087474611, -1.703760181015579134, 1.330383891403746688 ) ) ;
#61156 = CARTESIAN_POINT ( 'NONE',  ( -6.121777486219434294, 6.006025806897081765, -0.2357381234046468377 ) ) ;
#61155 = CARTESIAN_POINT ( 'NONE',  ( -4.261005416444848315, 8.193199762486115034, 0.7998128361456352531 ) ) ;
#61157 = CARTESIAN_POINT ( 'NONE',  ( 1.364683531249988535, 2.113541667008087099, 0.7879004041258500513 ) ) ;
#61158 = CARTESIAN_POINT ( 'NONE',  ( 2.706025971585944490, -1.282006620817040643, -1.167505586895122072 ) ) ;
#61159 = CARTESIAN_POINT ( 'NONE',  ( 2.694910210795556260, -0.5461130550479543766, 1.652493440627414323 ) ) ;
#61160 = CARTESIAN_POINT ( 'NONE',  ( 7.673551755654734130, 9.015193805427763607, -1.082531754730537976 ) ) ;
#61161 = CARTESIAN_POINT ( 'NONE',  ( -11.69243366784185945, 8.407932920124673970, 1.097391832464843286 ) ) ;
#61162 = CIRCLE ( 'NONE', #71489, 0.04999999999999883010 ) ;
#61163 = CARTESIAN_POINT ( 'NONE',  ( 2.372422516638694745, -0.4444355326964634090, 1.966343308868031103 ) ) ;
#61164 = CARTESIAN_POINT ( 'NONE',  ( 6.825078400183510752, 2.433016701115862102, 2.426111979085682879 ) ) ;
#61165 = CARTESIAN_POINT ( 'NONE',  ( -4.309512724297390740, 6.121127159803966933, 1.599625672291270506 ) ) ;
#61166 = CARTESIAN_POINT ( 'NONE',  ( 1.076956826339631856, -0.04624765943369788662, -1.971079714834519159 ) ) ;
#61167 = MECHANICAL_DESIGN_GEOMETRIC_PRESENTATION_REPRESENTATION (  '', ( #202924 ), #151150 ) ;
#61168 = EDGE_CURVE ( 'NONE', #104840, #133306, #180619, .T. ) ;
#61170 = CARTESIAN_POINT ( 'NONE',  ( -6.305950844131887223, 6.529566537674873494, 0.000000000000000000 ) ) ;
#61169 = CARTESIAN_POINT ( 'NONE',  ( 6.293217207623316156, -0.1008467329366956045, -1.909883259500498198 ) ) ;
#61171 = CARTESIAN_POINT ( 'NONE',  ( -6.116136693096208887, 6.308116694799912771, 0.7216878364870257245 ) ) ;
#61172 = CARTESIAN_POINT ( 'NONE',  ( 7.035755370848908896, 7.173079118937375931, 0.7998128361456352531 ) ) ;
#61173 = CARTESIAN_POINT ( 'NONE',  ( -5.420227550413282636, 9.545625585449309725, 0.7998128361456291469 ) ) ;
#61174 = CARTESIAN_POINT ( 'NONE',  ( 0.9440171659906453350, -1.283125807103436600, -1.559678575094858077 ) ) ;
#61175 = CARTESIAN_POINT ( 'NONE',  ( -15.75000000000000000, 10.90000000000000036, -0.7000000000000009548 ) ) ;
#61176 = CARTESIAN_POINT ( 'NONE',  ( 5.526528793889518454, 1.380124021263717804, -1.849252619965065847 ) ) ;
#61177 = CARTESIAN_POINT ( 'NONE',  ( 6.021922112293466967, 1.933069186966931863, -0.3339256516061983038 ) ) ;
#61178 = CARTESIAN_POINT ( 'NONE',  ( 3.098438489093110704, 1.946378968836332213, 0.2448508753878294586 ) ) ;
#61179 = CARTESIAN_POINT ( 'NONE',  ( 7.736899214892750010, 12.17813285068358020, 1.040834085586084257E-14 ) ) ;
#61180 = CARTESIAN_POINT ( 'NONE',  ( 1.527869225950146292, 1.291745156262789074, 1.495028600074751468 ) ) ;
#61181 = ORIENTED_EDGE ( 'NONE', *, *, #100659, .T. ) ;
#61182 = CARTESIAN_POINT ( 'NONE',  ( 0.6732554233833996093, 1.864234297354839143, -1.003953180072956419 ) ) ;
#61184 = CARTESIAN_POINT ( 'NONE',  ( -8.019811557683421910, 9.315200557840817908, 1.199719254218462483 ) ) ;
#61183 = CARTESIAN_POINT ( 'NONE',  ( -4.973143418114339021, 4.696422164088486895, 0.7998128361456341429 ) ) ;
#61185 = CARTESIAN_POINT ( 'NONE',  ( 1.974305314296275649, -0.08955604370030831318, -1.839086841257123073 ) ) ;
#61186 = ORIENTED_EDGE ( 'NONE', *, *, #64812, .F. ) ;
#61187 = CARTESIAN_POINT ( 'NONE',  ( 3.151577601795185757, 1.966304690962265234, -0.4465026806126579095 ) ) ;
#61188 = CARTESIAN_POINT ( 'NONE',  ( 11.97491505176683724, 7.682034517632803983, 0.8879925087013592622 ) ) ;
#61190 = EDGE_CURVE ( 'NONE', #106229, #7968, #53121, .T. ) ;
#61189 = CARTESIAN_POINT ( 'NONE',  ( 2.601940685209406467, 1.502730264585940168, 1.496503045097858919 ) ) ;
#61191 = CARTESIAN_POINT ( 'NONE',  ( -1.001543065824772872E-14, 4.743750000682822154, 1.732050807568877637 ) ) ;
#61192 = CARTESIAN_POINT ( 'NONE',  ( 6.740374924288304648, 11.01552117831172062, 1.040834085586084257E-14 ) ) ;
#61193 = CARTESIAN_POINT ( 'NONE',  ( 7.550965208168244125, 7.774157262476569130, -0.7998128361456341429 ) ) ;
#61194 = CARTESIAN_POINT ( 'NONE',  ( 3.427077464676528074, 0.04692547926744317088, 2.060408731095995094 ) ) ;
#61196 = CARTESIAN_POINT ( 'NONE',  ( 0.6965153189463432204, 1.505040478001760107, 1.060415605250275339 ) ) ;
#61195 = CARTESIAN_POINT ( 'NONE',  ( -6.828502922777144768, 11.11833717654868892, 0.7998128361456481317 ) ) ;
#61197 = CARTESIAN_POINT ( 'NONE',  ( -0.6823417656250003738, 2.717708333674753618, -1.181850606188749264 ) ) ;
#61198 = CARTESIAN_POINT ( 'NONE',  ( -0.02224634325202062834, 1.297472808610355521, -2.537530276547406149 ) ) ;
#61199 = CARTESIAN_POINT ( 'NONE',  ( 1.435188857121525441, 4.071834925727953802, 0.4528096192972438927 ) ) ;
#61200 = AXIS2_PLACEMENT_3D ( 'NONE', #54893, #72183, #118882 ) ;
#61201 = CARTESIAN_POINT ( 'NONE',  ( -7.285838599102589797E-14, 7.078193277237590841, -2.121339347286493648 ) ) ;
#61202 = CARTESIAN_POINT ( 'NONE',  ( 2.917521460708580872, -0.2248114924257374192, 2.251233801775154308 ) ) ;
#61203 = CARTESIAN_POINT ( 'NONE',  ( -9.815740026613960723, 11.51441345488021106, -1.082531754730539753 ) ) ;
#61204 = CARTESIAN_POINT ( 'NONE',  ( 2.232397805642115873, 1.180933449141470026, -1.373882015996011452 ) ) ;
#61205 = CARTESIAN_POINT ( 'NONE',  ( 2.958105166426743704, -1.137214127935105790, 1.541527475959689308 ) ) ;
#61206 = CARTESIAN_POINT ( 'NONE',  ( 4.088381982606685838, 1.110138344689771239, -1.747393465062855533 ) ) ;
#61207 = CARTESIAN_POINT ( 'NONE',  ( -0.6823417656250003738, 3.030208333674754062, -1.181850606188749264 ) ) ;
#61208 = AXIS2_PLACEMENT_3D ( 'NONE', #78769, #62526, #128688 ) ;
#61209 = CARTESIAN_POINT ( 'NONE',  ( 1.885558555406470660, 1.358073900086468333, 1.429321910850362753 ) ) ;
#61210 = CARTESIAN_POINT ( 'NONE',  ( 6.428350398238483088, 1.106843121268024976, -1.576624894639609309 ) ) ;
#61211 = CARTESIAN_POINT ( 'NONE',  ( 3.256579335763456040, -1.417408692332474462, 1.220890361658559575 ) ) ;
#61213 = CARTESIAN_POINT ( 'NONE',  ( 4.628438946891473726, 8.448539137754004003, 0.3726521946380862427 ) ) ;
#61212 = CARTESIAN_POINT ( 'NONE',  ( 2.456097291302907770, 0.6137686719557032822, -2.224517260854632639 ) ) ;
#61214 = CARTESIAN_POINT ( 'NONE',  ( 2.365471783816187834, -0.4113058309756181807, 1.814853103561973935 ) ) ;
#61215 = CARTESIAN_POINT ( 'NONE',  ( -0.6823417656250212460, 2.801041667008084879, 1.181850606188767472 ) ) ;
#61216 = CARTESIAN_POINT ( 'NONE',  ( 6.725054104113727504, -1.884248279909329638, -0.8396177084525523471 ) ) ;
#61217 = CARTESIAN_POINT ( 'NONE',  ( -3.764360206088648297, 7.543504007078730922, -0.7998128361456281477 ) ) ;
#61218 = CARTESIAN_POINT ( 'NONE',  ( 4.950698647284403009, 8.927565521807144577, 1.040834085586084257E-14 ) ) ;
#61219 = CARTESIAN_POINT ( 'NONE',  ( -1.491696246971095041, 3.267622381768281681, 0.1760465247046025805 ) ) ;
#61220 = ADVANCED_FACE ( 'NONE', ( #117119 ), #118191, .F. ) ;
#61221 = CARTESIAN_POINT ( 'NONE',  ( 6.809622064836790223, -0.4623527835773094119, 2.061910140347056331 ) ) ;
#61222 = CARTESIAN_POINT ( 'NONE',  ( -0.6823417656250212460, 4.613541667008086655, 1.181850606188767472 ) ) ;
#61223 = CARTESIAN_POINT ( 'NONE',  ( 5.536455037250767930, 2.128579029500421438, 0.3755436860354774420 ) ) ;
#61224 = CARTESIAN_POINT ( 'NONE',  ( -0.05247081622378191312, -1.844958069526716926, 0.8224554107575526851 ) ) ;
#61225 = CARTESIAN_POINT ( 'NONE',  ( -1.364683531250000748, -0.2406249996585799189, 0.000000000000000000 ) ) ;
#61226 = COLOUR_RGB ( '', 0.09019608, 0.27058824, 0.51372549) ;
#61227 = CARTESIAN_POINT ( 'NONE',  ( -5.422898255786209099, 5.429062174613087599, -0.7216878364870207285 ) ) ;
#61230 = CARTESIAN_POINT ( 'NONE',  ( 6.005898861173831094, 6.109229547565340646, 1.040834085586084257E-14 ) ) ;
#61229 = CARTESIAN_POINT ( 'NONE',  ( 6.825078400183544503, 2.075476428726834577, 2.163873318353096931 ) ) ;
#61228 = CARTESIAN_POINT ( 'NONE',  ( 6.550524494058025837, 7.671308660269694712, -1.199719254218452047 ) ) ;
#61231 = CARTESIAN_POINT ( 'NONE',  ( -5.178288325776719603, 5.006034233019745372, 0.000000000000000000 ) ) ;
#61232 = CARTESIAN_POINT ( 'NONE',  ( 5.085172837459294826, 1.651341431264556014, 1.157102043685846793 ) ) ;
#61233 = CARTESIAN_POINT ( 'NONE',  ( -9.013473194986783454, 9.410140237106395134, -0.7998128361456291469 ) ) ;
#61235 = CARTESIAN_POINT ( 'NONE',  ( -5.438229012412888252, 9.358701257874761481, -0.7216878364870338292 ) ) ;
#61234 = CARTESIAN_POINT ( 'NONE',  ( -8.514157279702027736, 10.95626946445095307, -1.443375672974059665 ) ) ;
#61236 = LINE ( 'NONE', #193364, #174382 ) ;
#61238 = CARTESIAN_POINT ( 'NONE',  ( -1.364683531250000748, 9.109375000341396245, 0.000000000000000000 ) ) ;
#61237 = CARTESIAN_POINT ( 'NONE',  ( 5.823154874416164084, -0.05760400987671504547, 2.161107263091876618 ) ) ;
#61239 = CARTESIAN_POINT ( 'NONE',  ( -10.91033920341459229, 4.885615726745597520, 4.996448585388895580 ) ) ;
#61241 = CARTESIAN_POINT ( 'NONE',  ( 0.1049102937123137097, -0.09321989032292328503, 1.913444960606479395 ) ) ;
#61240 = CARTESIAN_POINT ( 'NONE',  ( -7.524412065460066579, 7.880828285899290186, 0.7216878364870317197 ) ) ;
#61242 = CARTESIAN_POINT ( 'NONE',  ( -1.402160292154681736E-14, 0.2593750003414224681, -1.575800808251665908 ) ) ;
#61243 = DIRECTION ( 'NONE',  ( 1.016547956922408957E-15, 1.000000000000000000, -4.622230424712075819E-32 ) ) ;
#61244 = CARTESIAN_POINT ( 'NONE',  ( 1.804884324593715839, 1.432779585713826576, 0.9600471282974596399 ) ) ;
#61245 = CARTESIAN_POINT ( 'NONE',  ( 5.096939404094710468, 4.911127157724081371, 0.000000000000000000 ) ) ;
#61246 = CARTESIAN_POINT ( 'NONE',  ( 6.475954649182838807, 7.584310507915338562, 1.199719254218452047 ) ) ;
#61247 = CARTESIAN_POINT ( 'NONE',  ( -10.63109271062926275, 5.887865540153549127, -5.475652048317233955 ) ) ;
#61248 = CARTESIAN_POINT ( 'NONE',  ( 1.000807349803897628, 1.442299932730039869, 1.025250199436118503 ) ) ;
#61249 =( BOUNDED_CURVE ( )  B_SPLINE_CURVE ( 2, ( #112607, #128869, #78960, #208948, #146134, #94185, #80031, #176478, #113677 ),
 .UNSPECIFIED., .F., .T. ) 
 B_SPLINE_CURVE_WITH_KNOTS ( ( 3, 2, 2, 2, 3 ),
 ( 0.5803571428571429047, 0.5833333333333333703, 0.5892857142857143016, 0.5952380952380952328, 0.5982142857142856984 ),
 .UNSPECIFIED. ) 
 CURVE ( )  GEOMETRIC_REPRESENTATION_ITEM ( )  RATIONAL_B_SPLINE_CURVE ( ( 0.9330127018922194093, 0.9330127018922206306, 1.000000000000000000, 0.8660254037844387076, 1.000000000000000000, 0.8660254037844387076, 1.000000000000000000, 0.9330127018922194093, 0.9330127018922194093 ) ) 
 REPRESENTATION_ITEM ( '' )  );
#61250 = CARTESIAN_POINT ( 'NONE',  ( 2.455728839946738518, -1.493258543598206201, -1.350275873876593868 ) ) ;
#61251 = CARTESIAN_POINT ( 'NONE',  ( 4.506973327934083784, 1.708129512224244806, -1.397202154207459524 ) ) ;
#61252 = CARTESIAN_POINT ( 'NONE',  ( 5.102462520977921301, 2.164757797245045357, 0.1666947352320021780 ) ) ;
#61253 = ORIENTED_EDGE ( 'NONE', *, *, #183399, .F. ) ;
#61254 = CARTESIAN_POINT ( 'NONE',  ( -1.500000000000015099, -0.8291666666666407393, 0.8660254037844403729 ) ) ;
#61255 = CARTESIAN_POINT ( 'NONE',  ( 8.229436053370669413, 10.62409470039771442, 1.443375672974076540 ) ) ;
#61257 = CARTESIAN_POINT ( 'NONE',  ( 3.427361390312729572, -1.528753972193249933, -1.314983687342549556 ) ) ;
#61256 = CARTESIAN_POINT ( 'NONE',  ( 3.194099758881031814, 1.346771490053525033, 1.637864368873870990 ) ) ;
#61259 = ORIENTED_EDGE ( 'NONE', *, *, #208272, .T. ) ;
#61258 = CARTESIAN_POINT ( 'NONE',  ( 2.970771795020191064, -1.368765343908146415, 1.186782720094860855 ) ) ;
#61260 = CARTESIAN_POINT ( 'NONE',  ( 5.417364897112183719, 8.477953592343014932, 1.199719254218451159 ) ) ;
#61261 = ORIENTED_EDGE ( 'NONE', *, *, #172591, .T. ) ;
#61262 = CARTESIAN_POINT ( 'NONE',  ( 4.806723615010448736E-13, -7.868798029037617603, -9.500000000000001776 ) ) ;
#61263 = CARTESIAN_POINT ( 'NONE',  ( 6.094553744542824170, 7.069066442510145265, 1.199719254218462483 ) ) ;
#61264 = CARTESIAN_POINT ( 'NONE',  ( 5.918537399722813674, 1.222626809077583587, -1.356019982345892050 ) ) ;
#61266 = CARTESIAN_POINT ( 'NONE',  ( 1.499098398830187362, -0.2305585200724231121, 1.901688874922660588 ) ) ;
#61265 = CARTESIAN_POINT ( 'NONE',  ( -5.427341564172148303, 5.226320001155936090, 0.000000000000000000 ) ) ;
#61267 = CARTESIAN_POINT ( 'NONE',  ( 0.000000000000000000, -2.856854249492362996, 0.000000000000000000 ) ) ;
#61268 = CARTESIAN_POINT ( 'NONE',  ( -4.884430620531565737, 4.928167907039282980, -0.5181559072752897066 ) ) ;
#61269 = CARTESIAN_POINT ( 'NONE',  ( 1.364683531249986537, 1.176041667008082658, 0.7879004041258500513 ) ) ;
#61270 = DIRECTION ( 'NONE',  ( 0.000000000000000000, 1.000000000000000000, 0.000000000000000000 ) ) ;
#61271 = CARTESIAN_POINT ( 'NONE',  ( -7.808606406466886973, 11.19745900993164511, 1.199719254218453823 ) ) ;
#61272 = CARTESIAN_POINT ( 'NONE',  ( 5.014612968065254250, 1.493337269798940881, -1.563205770552501761 ) ) ;
#61273 = CARTESIAN_POINT ( 'NONE',  ( -4.909461021924285795, 6.821066840368686712, 1.443375672974058777 ) ) ;
#61274 = CARTESIAN_POINT ( 'NONE',  ( -7.370792787684826486, 8.628288336167626582, -1.199719254218452047 ) ) ;
#61275 = CARTESIAN_POINT ( 'NONE',  ( 3.305043459179863419, -0.4174351347619070784, -2.078937965663613774 ) ) ;
#61277 = CARTESIAN_POINT ( 'NONE',  ( -11.34338453707543515, 5.310936115193626961, -5.661293933977025183 ) ) ;
#61276 = DIRECTION ( 'NONE',  ( 0.000000000000000000, 0.000000000000000000, 1.000000000000000000 ) ) ;
#61278 = CARTESIAN_POINT ( 'NONE',  ( 4.024654096683129900, 1.870930367033913688, 0.6213144229534044438 ) ) ;
#61279 = CARTESIAN_POINT ( 'NONE',  ( 6.029550621839829816, -0.2273517531893587407, 1.898748578088353733 ) ) ;
#61280 = EDGE_LOOP ( 'NONE', ( #15850, #124326, #151645, #27339 ) ) ;
#61281 = VECTOR ( 'NONE', #7501, 1000.000000000000000 ) ;
#61282 = CARTESIAN_POINT ( 'NONE',  ( 5.805892041792804825, -1.178307743425134335, -1.758994673012766574 ) ) ;
#61283 = CARTESIAN_POINT ( 'NONE',  ( 6.197485614778206475, 6.403023770095559009, -0.7216878364870318308 ) ) ;
#61284 = CARTESIAN_POINT ( 'NONE',  ( 0.8013346216862862192, -1.776568573310655985, 1.062853015585236482 ) ) ;
#61285 = CARTESIAN_POINT ( 'NONE',  ( 2.220557385006210804, 0.0001418518128949025625, 1.942124712491780869 ) ) ;
#61286 = EDGE_LOOP ( 'NONE', ( #86923, #45849, #99932, #96170, #67074, #54357, #202881, #200163, #117822, #83923, #7709, #119452, #174808, #148625, #195022, #140453, #137494, #164137 ) ) ;
#61287 = CYLINDRICAL_SURFACE ( 'NONE', #182116, 0.08000000000000020983 ) ;
#61288 = CARTESIAN_POINT ( 'NONE',  ( 5.040599249230596435, 9.102725900736217568, 0.7998128361456341429 ) ) ;
#61290 = CARTESIAN_POINT ( 'NONE',  ( 5.795220594837462436, 8.848508896363995291, -1.199719254218440723 ) ) ;
#61289 = CARTESIAN_POINT ( 'NONE',  ( 3.099644000116580589, -2.088226275799191622, 0.1030096337034935861 ) ) ;
#61291 = CARTESIAN_POINT ( 'NONE',  ( 7.635176783151273128, 8.936736330878529699, 1.199719254218452935 ) ) ;
#61293 = ORIENTED_EDGE ( 'NONE', *, *, #171367, .F. ) ;
#61292 = CARTESIAN_POINT ( 'NONE',  ( 0.2053161149570548183, 1.340855080820763545, 1.218213988936674763 ) ) ;
#61294 = CARTESIAN_POINT ( 'NONE',  ( 5.197975494389605267, -0.7968864405506062010, 2.058166701804148957 ) ) ;
#61295 = CARTESIAN_POINT ( 'NONE',  ( 0.08058605610391310348, -6.304485801116100241, -10.99970480911016146 ) ) ;
#61296 = CARTESIAN_POINT ( 'NONE',  ( 3.505080564089088746, 1.740947047783932611, -1.355986173033681075 ) ) ;
#61297 = CARTESIAN_POINT ( 'NONE',  ( 9.284636267260101050, 9.726497154758602548, -0.7998128361456281477 ) ) ;
#61298 = DIRECTION ( 'NONE',  ( 0.000000000000000000, -1.000000000000000000, 0.000000000000000000 ) ) ;
#61299 = CARTESIAN_POINT ( 'NONE',  ( 2.016128127738999076, -1.911839501640894001, 0.04842977492004740814 ) ) ;
#61300 = CARTESIAN_POINT ( 'NONE',  ( 7.964525173024008531, 11.37936423758166526, 1.199719254218460707 ) ) ;
#61301 = CARTESIAN_POINT ( 'NONE',  ( 5.020015195830264787, 2.048331326439792210, -0.3003445753073652469 ) ) ;
#61303 = CARTESIAN_POINT ( 'NONE',  ( 3.168983506954273999, -1.996715753333128118, -0.8287754370841573515 ) ) ;
#61302 = CARTESIAN_POINT ( 'NONE',  ( 1.554911173149762016, 8.692115300649543741, -2.503913477513633357 ) ) ;
#61304 = CARTESIAN_POINT ( 'NONE',  ( 4.476244563333130699, -2.125884358948509689, -0.5320566845071761364 ) ) ;
#61305 = ORIENTED_EDGE ( 'NONE', *, *, #65262, .T. ) ;
#61306 = DIRECTION ( 'NONE',  ( -0.000000000000000000, -0.000000000000000000, -1.000000000000000000 ) ) ;
#61307 = B_SPLINE_CURVE_WITH_KNOTS ( 'NONE', 3,
 ( #112292, #14701, #196671, #95999, #145831 ),
 .UNSPECIFIED., .F., .F.,
 ( 4, 1, 4 ),
 ( 8.741117365843281861E-19, 5.162781510639185282E-05, 0.0001032556302127828247 ),
 .UNSPECIFIED. ) ;
#61308 = CARTESIAN_POINT ( 'NONE',  ( -6.042630808230841359E-15, -2.318749999044084298, 3.474999999999999645 ) ) ;
#61309 = CARTESIAN_POINT ( 'NONE',  ( -0.4998684179605343281, 7.978338306495868615, 1.936700108954719335 ) ) ;
#61310 = ADVANCED_FACE ( 'NONE', ( #202545 ), #120334, .T. ) ;
#61311 = CARTESIAN_POINT ( 'NONE',  ( 6.170896192875352959, 7.228408975556602556, 1.199719254218453823 ) ) ;
#61312 = CARTESIAN_POINT ( 'NONE',  ( -3.285556943749998737, -2.967708332855377051, 1.896917185911908721 ) ) ;
#61313 = CARTESIAN_POINT ( 'NONE',  ( -0.1102773484824129541, -0.006951161900758274365, -2.203378182130751206 ) ) ;
#61314 = CARTESIAN_POINT ( 'NONE',  ( -0.03452862918938356951, -1.956592590566148093, -0.4871966601913205186 ) ) ;
#61315 = CARTESIAN_POINT ( 'NONE',  ( -7.849807752632384172, 12.10193344480572897, 0.000000000000000000 ) ) ;
#61317 = CARTESIAN_POINT ( 'NONE',  ( 4.875038752565570732, 7.845239757038595663, -1.199719254218452047 ) ) ;
#61316 = AXIS2_PLACEMENT_3D ( 'NONE', #179619, #29102, #163372 ) ;
#61318 = CARTESIAN_POINT ( 'NONE',  ( 5.067269747081383890, 1.798595138155817841, 1.025117745595036878 ) ) ;
#61319 = CARTESIAN_POINT ( 'NONE',  ( 4.951747152513418904, 0.6024649636334912239, -1.829943702413504791 ) ) ;
#61320 = CARTESIAN_POINT ( 'NONE',  ( 0.4215001937674204280, -1.427952733550428288, -1.423947716221201976 ) ) ;
#61321 = CARTESIAN_POINT ( 'NONE',  ( -2.331034670843834533E-15, -7.357813805514510364, 9.695354081530208390 ) ) ;
#61322 = CARTESIAN_POINT ( 'NONE',  ( 3.974511587100456822, 7.788680618259193444, 1.040834085586084257E-14 ) ) ;
#61323 = CARTESIAN_POINT ( 'NONE',  ( -6.966220764712169000, 6.002124920821316323, -2.420000000000000373 ) ) ;
#61324 = CARTESIAN_POINT ( 'NONE',  ( 4.434397634191796556, -1.137439385922611290, 1.607554744723362017 ) ) ;
#61325 = CARTESIAN_POINT ( 'NONE',  ( 0.05887529153619439071, -1.959562692596405364, -0.9812908054248059564 ) ) ;
#61326 = CARTESIAN_POINT ( 'NONE',  ( 3.879382553896340013, 1.718498013671100777, -0.6167319420108534622 ) ) ;
#61327 = EDGE_CURVE ( 'NONE', #9317, #209619, #48947, .T. ) ;
#61328 = CARTESIAN_POINT ( 'NONE',  ( 6.156811154381533591, 9.236677875870187293, -1.082531754730548412 ) ) ;
#61329 = CARTESIAN_POINT ( 'NONE',  ( 3.158686601859607368, 6.628958768904106513, -0.7216878364870267237 ) ) ;
#61330 = CARTESIAN_POINT ( 'NONE',  ( -5.271087860662956537, 9.371629280740593870, 0.000000000000000000 ) ) ;
#61331 = CARTESIAN_POINT ( 'NONE',  ( 4.258142763143749399, 7.125527769379820242, 1.199719254218451159 ) ) ;
#61332 = ORIENTED_EDGE ( 'NONE', *, *, #49246, .T. ) ;
#61334 = CARTESIAN_POINT ( 'NONE',  ( 4.640889591357927557, 1.927823495868080439, 0.5801764560204000221 ) ) ;
#61333 = CARTESIAN_POINT ( 'NONE',  ( 1.259045258496578557, 1.813921241667546758, -0.3151448728593714277 ) ) ;
#61335 = CARTESIAN_POINT ( 'NONE',  ( 0.8964060800229460835, 0.1715710081350088068, 2.292006659179766537 ) ) ;
#61336 = CARTESIAN_POINT ( 'NONE',  ( 5.260583753728677259, -0.6573284944802314511, -1.848511375219172415 ) ) ;
#61337 = CARTESIAN_POINT ( 'NONE',  ( -5.856232286098998152, 8.919689202835742847, 1.199719254218452047 ) ) ;
#61338 = CARTESIAN_POINT ( 'NONE',  ( 4.800089777832203808, 5.120415418395356077, -0.7784788408505428636 ) ) ;
#61339 = CARTESIAN_POINT ( 'NONE',  ( -3.436101866059630527, 6.096203712789787232, 1.199719254218462483 ) ) ;
#61340 = CARTESIAN_POINT ( 'NONE',  ( -10.64229060209982514, 1.016282880930358568, -6.144329343916520081 ) ) ;
#61341 = CARTESIAN_POINT ( 'NONE',  ( -5.469788628470539926, 5.346117919495872783, -0.7998128361456362523 ) ) ;
#61343 = CARTESIAN_POINT ( 'NONE',  ( 6.508682224664005922, 1.308065493886721775, -1.192407281889706905 ) ) ;
#61342 = CARTESIAN_POINT ( 'NONE',  ( 0.9606207175340542026, -1.891748053602306578, -0.8905051939756128965 ) ) ;
#61344 = CARTESIAN_POINT ( 'NONE',  ( -0.005132432257077002187, 7.078226584369338603, 2.121329534126264349 ) ) ;
#61345 = CARTESIAN_POINT ( 'NONE',  ( -0.1104750535120025690, -0.004616138082884356161, -2.103378236956428893 ) ) ;
#61346 = CARTESIAN_POINT ( 'NONE',  ( 2.542201289624079319, -1.445942355291447434, 0.9683529963873671598 ) ) ;
#61347 = CARTESIAN_POINT ( 'NONE',  ( 5.606460214450851964, 6.499623990736163037, 1.199719254218462483 ) ) ;
#61349 = CARTESIAN_POINT ( 'NONE',  ( 4.161989969715248705, 4.726297878971393196, -2.420000000000000373 ) ) ;
#61348 = FACE_OUTER_BOUND ( 'NONE', #50260, .T. ) ;
#61350 = CARTESIAN_POINT ( 'NONE',  ( 1.558790235068749030, -1.477961618093760032, -0.8890178537931183733 ) ) ;
#61351 = CARTESIAN_POINT ( 'NONE',  ( 2.068174269828721101, -1.345378145056834063, 1.729934933326432445 ) ) ;
#61352 = CARTESIAN_POINT ( 'NONE',  ( 3.686314334879085663, -1.088174899301070253, 1.919869060924610293 ) ) ;
#61353 = CARTESIAN_POINT ( 'NONE',  ( -9.348596576284975868, 2.999985932080179829, -7.001940380475246251 ) ) ;
#61354 = AXIS2_PLACEMENT_3D ( 'NONE', #101677, #167747, #19347 ) ;
#61355 = CARTESIAN_POINT ( 'NONE',  ( 2.167058194802372828, 1.611091607626200961, -1.455523108145313937 ) ) ;
#61356 = CARTESIAN_POINT ( 'NONE',  ( 1.207329354700342305, -0.4456725867950651621, 1.770335049871730071 ) ) ;
#61357 = CARTESIAN_POINT ( 'NONE',  ( 3.485668972010677269, -0.6104075878305641467, 2.027481811383638810 ) ) ;
#61358 = CARTESIAN_POINT ( 'NONE',  ( 6.539320575229250920, 2.072231551265828475, 2.205269387046896679 ) ) ;
#61359 = ADVANCED_FACE ( 'NONE', ( #39014 ), #8631, .T. ) ;
#61360 = EDGE_LOOP ( 'NONE', ( #175217, #176093, #57799, #153828, #75425, #134572 ) ) ;
#61362 = CARTESIAN_POINT ( 'NONE',  ( -1.364683531250012516, 1.342708333674755616, 0.7879004041258379498 ) ) ;
#61361 = CARTESIAN_POINT ( 'NONE',  ( 3.175583430956610886, 1.455732557240730696, 1.770799584264992399 ) ) ;
#61363 = CARTESIAN_POINT ( 'NONE',  ( 0.07755575628181492209, 4.082361791518872352, -2.743585103993382734 ) ) ;
#61364 = CARTESIAN_POINT ( 'NONE',  ( 3.194917754314666514, 6.879154480009089134, 0.7998128361456321445 ) ) ;
#61365 = AXIS2_PLACEMENT_3D ( 'NONE', #86812, #69469, #106314 ) ;
#61366 = CARTESIAN_POINT ( 'NONE',  ( 5.795613637301100241, 2.053263797698097637, -0.8479724704701059323 ) ) ;
#61367 = CARTESIAN_POINT ( 'NONE',  ( -7.375272376154101472, 7.706831981708990753, -0.7216878364870278340 ) ) ;
#61368 = CARTESIAN_POINT ( 'NONE',  ( 4.026408433578586354, 7.641300905909586660, 1.040834085586084257E-14 ) ) ;
#61369 = CARTESIAN_POINT ( 'NONE',  ( -5.192409643909507544, 9.001635651295671892, 0.7216878364870458196 ) ) ;
#61370 = CARTESIAN_POINT ( 'NONE',  ( 4.014622883422321209, 5.777089012116397804, -1.443375672974068769 ) ) ;
#61371 = ORIENTED_EDGE ( 'NONE', *, *, #140986, .F. ) ;
#61372 = CARTESIAN_POINT ( 'NONE',  ( 3.779922787921150995, 1.701948043757589124, -1.081065327119046016 ) ) ;
#61374 = CARTESIAN_POINT ( 'NONE',  ( 2.588800687925230992, 1.999571085336487641, 0.5053362289856622169 ) ) ;
#61373 = CARTESIAN_POINT ( 'NONE',  ( 7.447506452608354088, 7.583179037664891098, 0.7998128361456341429 ) ) ;
#61375 = CARTESIAN_POINT ( 'NONE',  ( -2.964627556058684554, 6.451541201391447267, 0.3872157855231770918 ) ) ;
#61376 = EDGE_CURVE ( 'NONE', #160120, #138011, #24876, .T. ) ;
#61377 = CARTESIAN_POINT ( 'NONE',  ( 5.854088466050551887, 10.05179665369283981, 0.7998128361456341429 ) ) ;
#61378 = CARTESIAN_POINT ( 'NONE',  ( -3.285556943750000070, -2.909374999522040817, 0.000000000000000000 ) ) ;
#61379 = CARTESIAN_POINT ( 'NONE',  ( -1.201851678989727383E-14, 4.446875000341417916, -1.575800808251660134 ) ) ;
#61380 = CARTESIAN_POINT ( 'NONE',  ( 4.646525747415945595, -1.761044916313101671, 1.304081410864160739 ) ) ;
#61381 = CARTESIAN_POINT ( 'NONE',  ( 2.338517726396415863, 0.5350873343827439177, -1.944071628254496087 ) ) ;
#61382 = CARTESIAN_POINT ( 'NONE',  ( 2.085277916773973228, -0.7859315772556186852, 1.665205719185464561 ) ) ;
#61383 = CARTESIAN_POINT ( 'NONE',  ( 5.798083248138522272, 9.916180889470295412, 0.7998128361456462443 ) ) ;
#61384 = CARTESIAN_POINT ( 'NONE',  ( 6.756878055424797580, -1.408711550780303634, 1.160885376127060775 ) ) ;
#61385 = CARTESIAN_POINT ( 'NONE',  ( -6.581593504430098385, 9.765943957555402122, -1.199719254218440723 ) ) ;
#61387 = CARTESIAN_POINT ( 'NONE',  ( -6.168033539574333979, 6.160736982450306876, 0.7998128361456281477 ) ) ;
#61386 = CARTESIAN_POINT ( 'NONE',  ( 5.243177039506740300, -1.943355607328334678, 1.158386780943015504 ) ) ;
#61388 = CARTESIAN_POINT ( 'NONE',  ( 0.2937649352797070401, 1.562083697590540998, 1.412785709394439815 ) ) ;
#61389 = CARTESIAN_POINT ( 'NONE',  ( -8.072954122294394352, 8.383144328957069291, -0.7998128361456362523 ) ) ;
#61390 = CARTESIAN_POINT ( 'NONE',  ( 7.944187942603509356, 11.35563746875774882, 1.199719254218460707 ) ) ;
#61391 = CARTESIAN_POINT ( 'NONE',  ( 6.007671464186823407, 9.062681570643055906, 1.082531754730549967 ) ) ;
#61392 = CARTESIAN_POINT ( 'NONE',  ( -8.050844288416501016, 8.287073179441051707, 1.040834085586084257E-14 ) ) ;
#61393 = CARTESIAN_POINT ( 'NONE',  ( 6.766604819867146681, -7.256397064628574256, 6.766604819867123588 ) ) ;
#61394 = CARTESIAN_POINT ( 'NONE',  ( 8.256552360598020002, 8.734991963560254646, -0.7216878364870267237 ) ) ;
#61395 = CARTESIAN_POINT ( 'NONE',  ( 4.359152798643180837, 7.157646611464889119, -1.047953017514296370 ) ) ;
#61396 = CARTESIAN_POINT ( 'NONE',  ( -9.991996023591624976, 10.75967623705280296, 1.040834085586084257E-14 ) ) ;
#61397 = CARTESIAN_POINT ( 'NONE',  ( 3.094184762719538906, 1.412074837861827303, 1.714815191315356868 ) ) ;
#61398 = CARTESIAN_POINT ( 'NONE',  ( 3.231779075379137556, 6.036511184309971689, -2.420000000000002149 ) ) ;
#61399 = CARTESIAN_POINT ( 'NONE',  ( -4.274563570058511175, 8.209017608368725405, 0.000000000000000000 ) ) ;
#61400 = CARTESIAN_POINT ( 'NONE',  ( 6.145923705696426431, 6.064665832934283962, 0.7998128361456341429 ) ) ;
#61401 = CARTESIAN_POINT ( 'NONE',  ( 4.527759979645433752, 1.903474890065796732, -0.4746247275292309609 ) ) ;
#61402 = CARTESIAN_POINT ( 'NONE',  ( 8.269583629331492602, 11.73526576994040482, 1.199719254218450271 ) ) ;
#61403 = CARTESIAN_POINT ( 'NONE',  ( -5.250693970737303928, 6.428279158139240224, 1.158874695820178324 ) ) ;
#61404 = CARTESIAN_POINT ( 'NONE',  ( 2.900554798319789906, 5.471398800426671372, 1.199719254218452047 ) ) ;
#61405 = CARTESIAN_POINT ( 'NONE',  ( -1.364683531250000748, 0.5093750003414208027, 0.000000000000000000 ) ) ;
#61406 = CARTESIAN_POINT ( 'NONE',  ( -4.882344714696960075, 5.829061934302122161, 1.082531754730549078 ) ) ;
#61408 = ORIENTED_EDGE ( 'NONE', *, *, #207484, .F. ) ;
#61407 = CARTESIAN_POINT ( 'NONE',  ( -6.222829318992474157, 10.20379193889247382, 0.000000000000000000 ) ) ;
#61409 = CARTESIAN_POINT ( 'NONE',  ( 3.217144136595586179, 1.669276650691432495, -1.307696563879121365 ) ) ;
#61410 = CARTESIAN_POINT ( 'NONE',  ( -3.800028193580205382, 7.655393002477360653, -0.7998128361456481317 ) ) ;
#61411 = CARTESIAN_POINT ( 'NONE',  ( 4.469695567000064429, 2.097540297429688838, -0.5223010940857697459 ) ) ;
#61412 = CARTESIAN_POINT ( 'NONE',  ( 4.159580895514263688, 0.8717668643758098579, 1.621812032879976329 ) ) ;
#61413 = CARTESIAN_POINT ( 'NONE',  ( -4.327620591935813721, 7.230343590456815406, 0.9971501367836959062 ) ) ;
#61414 = CARTESIAN_POINT ( 'NONE',  ( -1.402160292154681736E-14, -0.3656249996585805295, 1.575800808251672791 ) ) ;
#61415 = CARTESIAN_POINT ( 'NONE',  ( 5.595574051893665413, -1.740516469239574704, 0.006108698158355239591 ) ) ;
#61416 = DIRECTION ( 'NONE',  ( 1.276756478318932585E-15, -1.000000000000000000, 1.665334536937738262E-16 ) ) ;
#61417 = CARTESIAN_POINT ( 'NONE',  ( 4.853455804012228647, 4.764712647543454693, 0.7216878364870317197 ) ) ;
#61418 = CARTESIAN_POINT ( 'NONE',  ( 3.239309987758617115, -1.907233169736745060, 1.017530501952010447 ) ) ;
#61419 = CARTESIAN_POINT ( 'NONE',  ( 5.940779784064256219, 1.198679029392090589, 1.620932600025201786 ) ) ;
#61420 = CARTESIAN_POINT ( 'NONE',  ( -8.120970824461345217, 12.41829036193951730, 0.7216878364870458196 ) ) ;
#61421 = CARTESIAN_POINT ( 'NONE',  ( 2.149508875876861236, -1.735919364271593768, -1.288018159417112729 ) ) ;
#61422 = CARTESIAN_POINT ( 'NONE',  ( 3.391827608253958015, -0.8021585586163967330, 1.800962559972321575 ) ) ;
#61423 = CARTESIAN_POINT ( 'NONE',  ( 4.229980187955574067, 1.905242447948073403, 0.3755566216582290617 ) ) ;
#61424 = B_SPLINE_CURVE_WITH_KNOTS ( 'NONE', 3,
 ( #4615, #103227, #1422, #102156 ),
 .UNSPECIFIED., .F., .F.,
 ( 4, 4 ),
 ( 0.000000000000000000, 0.0002909236271752678894 ),
 .UNSPECIFIED. ) ;
#61426 = VERTEX_POINT ( 'NONE', #205762 ) ;
#61425 = CARTESIAN_POINT ( 'NONE',  ( -9.314088342463968218, 9.968783942403868892, 0.7216878364870438212 ) ) ;
#61427 = CARTESIAN_POINT ( 'NONE',  ( -7.632314129850253259, 7.869064337772231355, 0.7998128361456341429 ) ) ;
#61428 = CARTESIAN_POINT ( 'NONE',  ( -6.385527162356468445, 10.39360608948380538, 1.040834085586084257E-14 ) ) ;
#61430 = ORIENTED_EDGE ( 'NONE', *, *, #190504, .T. ) ;
#61429 = CARTESIAN_POINT ( 'NONE',  ( -3.467853430045390706, 7.267855778353407459, 0.7998128361456352531 ) ) ;
#61431 = CARTESIAN_POINT ( 'NONE',  ( -7.171900071504729191, 11.31104115015678779, -0.7216878364870267237 ) ) ;
#61432 = CARTESIAN_POINT ( 'NONE',  ( 2.503190323335769740, 1.772782541628318720, -1.313999973512294472 ) ) ;
#61433 = CARTESIAN_POINT ( 'NONE',  ( -3.285556943750000514, -1.188541666188710044, -1.896917185911906500 ) ) ;
#61434 = CARTESIAN_POINT ( 'NONE',  ( 6.174655700867183405, 1.320063289540554408, -1.451312704123429498 ) ) ;
#61435 =( BOUNDED_SURFACE ( )  B_SPLINE_SURFACE ( 3, 2, ( 
 ( #158286, #78079, #178799 ),
 ( #160403, #144204, #210200 ),
 ( #30415, #159333, #45604 ),
 ( #58638, #111721, #177729 ),
 ( #124791, #190751, #97554 ),
 ( #132201, #49843, #196109 ) ),
 .UNSPECIFIED., .F., .F., .T. ) 
 B_SPLINE_SURFACE_WITH_KNOTS ( ( 4, 2, 4 ),
 ( 3, 3 ),
 ( 0.000000000000000000, 0.0003754689591423961527, 0.0007509379182847923054 ),
 ( 0.000000000000000000, 1.000000000000000000 ),
 .UNSPECIFIED. ) 
 GEOMETRIC_REPRESENTATION_ITEM ( )  RATIONAL_B_SPLINE_SURFACE ( (
 ( 1.000000000000000000, 0.7071067811865475727, 1.000000000000000000),
 ( 1.000000000000000000, 0.7018599272024182989, 1.000000000000000000),
 ( 1.000000000000000000, 0.6927733177260235742, 1.000000000000000000),
 ( 1.000000000000000000, 0.6772007068873748814, 1.000000000000000000),
 ( 1.000000000000000000, 0.6709974581637003777, 1.000000000000000000),
 ( 1.000000000000000000, 0.6711954675835484219, 1.000000000000000000) ) ) 
 REPRESENTATION_ITEM ( '' )  SURFACE ( )  );
#61436 = CARTESIAN_POINT ( 'NONE',  ( -1.001543065824772872E-14, 5.634375000341415252, 1.575800808251672791 ) ) ;
#61437 = CARTESIAN_POINT ( 'NONE',  ( -1.500000000000011324, 4.452083334016148086, 0.8660254037844403729 ) ) ;
#61438 = CARTESIAN_POINT ( 'NONE',  ( 5.603691946294323323, 6.350013490765915591, -1.172630952486140243 ) ) ;
#61439 = CARTESIAN_POINT ( 'NONE',  ( 6.287735281038357549, 1.518688880046001444, 1.601449620450722700 ) ) ;
#61440 = CARTESIAN_POINT ( 'NONE',  ( 5.507694354943953208, -0.8313836724207699369, -1.642813217252625524 ) ) ;
#61441 = VERTEX_POINT ( 'NONE', #93114 ) ;
#61442 = CARTESIAN_POINT ( 'NONE',  ( -1.360316468750030428, -0.6093749996585878792, -1.908195823574487804E-14 ) ) ;
#61443 = CARTESIAN_POINT ( 'NONE',  ( -8.518600588087975822, 8.832788862391110385, 1.040834085586084257E-14 ) ) ;
#61445 = EDGE_CURVE ( 'NONE', #123984, #106888, #137593, .T. ) ;
#61444 = CARTESIAN_POINT ( 'NONE',  ( 5.941668366282724101, -1.996146358238064522, 0.7160658055916299114 ) ) ;
#61446 = CARTESIAN_POINT ( 'NONE',  ( 10.36569475343129731, 9.168110967066926520, -6.000526395088528808 ) ) ;
#61447 = CARTESIAN_POINT ( 'NONE',  ( 6.335737856287750880, 6.286115675290828264, -0.7998128361456281477 ) ) ;
#61448 = CARTESIAN_POINT ( 'NONE',  ( 6.116494506269664733, 1.387434351230539598, -1.523912472565646770 ) ) ;
#61451 = CARTESIAN_POINT ( 'NONE',  ( 3.491602800004707241, -1.839307750763185645, -0.08696504193297231733 ) ) ;
#61450 = CARTESIAN_POINT ( 'NONE',  ( 1.925991809680915878, 0.9530580284189617002, 1.598336604343030931 ) ) ;
#61449 = PRESENTATION_STYLE_ASSIGNMENT (( #144880 ) ) ;
#61452 = CARTESIAN_POINT ( 'NONE',  ( 7.969495366734495434, 8.192166104145387706, 1.040834085586084257E-14 ) ) ;
#61453 = CARTESIAN_POINT ( 'NONE',  ( -7.138471902074302378, 15.51981486752699446, 9.655967197029408311 ) ) ;
#61454 = CARTESIAN_POINT ( 'NONE',  ( -7.144220599758281054, 7.299621885998258897, 0.7998128361456341429 ) ) ;
#61456 = ORIENTED_EDGE ( 'NONE', *, *, #122971, .F. ) ;
#61455 = LINE ( 'NONE', #62519, #29063 ) ;
#61457 = AXIS2_PLACEMENT_3D ( 'NONE', #133843, #70903, #118682 ) ;
#61458 = CARTESIAN_POINT ( 'NONE',  ( 3.317197348578094562, 1.995112415077514356, 0.9436014139095407760 ) ) ;
#61459 = CARTESIAN_POINT ( 'NONE',  ( 6.309908665641647652, -2.246456703917932618, 0.2676860584361096529 ) ) ;
#61460 = CARTESIAN_POINT ( 'NONE',  ( -5.748293942514186128, 6.769059690097084747, -1.082531754730544860 ) ) ;
#61461 = CARTESIAN_POINT ( 'NONE',  ( 5.519718948577209794, -0.4320008574366646648, 1.759211659423996155 ) ) ;
#61462 = CARTESIAN_POINT ( 'NONE',  ( 0.04025042243083893495, 0.7762349914572730381, 1.861342399428978389 ) ) ;
#61463 = CARTESIAN_POINT ( 'NONE',  ( -0.07933194154488912297, -7.473374494045017968, 9.499668754385634628 ) ) ;
#61464 = CARTESIAN_POINT ( 'NONE',  ( 6.332864056472936376, 0.1854757364097951722, 1.861418627818342664 ) ) ;
#61465 = CARTESIAN_POINT ( 'NONE',  ( 5.567032834676129305, -1.504811603839781631, 1.179860560037985895 ) ) ;
#61466 = CARTESIAN_POINT ( 'NONE',  ( 5.504247177468215568, 5.523969249908735613, 0.7216878364870122908 ) ) ;
#61467 = CARTESIAN_POINT ( 'NONE',  ( 0.6548940681232479077, -1.578012236938080015, -1.004313744925364071 ) ) ;
#61468 = AXIS2_PLACEMENT_3D ( 'NONE', #66839, #50630, #7196 ) ;
#61469 = CARTESIAN_POINT ( 'NONE',  ( 1.798064920797682653, -0.9548589541341389042, -1.776165177175797583 ) ) ;
#61471 = CARTESIAN_POINT ( 'NONE',  ( 3.651088154774425387, -1.721711045478736102, 1.212656735320973400 ) ) ;
#61470 = CARTESIAN_POINT ( 'NONE',  ( -7.655550293210764856, 12.08322577538792331, 0.000000000000000000 ) ) ;
#61472 = CARTESIAN_POINT ( 'NONE',  ( 8.127223016387999266, 11.56917838817298616, 1.199719254218460707 ) ) ;
#61474 = CARTESIAN_POINT ( 'NONE',  ( -9.450196763925152510, 10.98398329845622001, -1.199719254218441611 ) ) ;
#61473 = CARTESIAN_POINT ( 'NONE',  ( -0.7500000000000249800, -0.05833333333331303105, 1.299038105676659116 ) ) ;
#61475 = CARTESIAN_POINT ( 'NONE',  ( -10.39230484541323740, 3.499999999999989342, 6.000000000000048850 ) ) ;
#61476 = CARTESIAN_POINT ( 'NONE',  ( 3.498311158119755682, -0.9917195014866404534, 1.759444004082431068 ) ) ;
#61477 = CARTESIAN_POINT ( 'NONE',  ( -1.201851678989727383E-14, 3.071875000341420137, 1.575800808251672791 ) ) ;
#61478 = EDGE_CURVE ( 'NONE', #158010, #68875, #188452, .T. ) ;
#61479 = CARTESIAN_POINT ( 'NONE',  ( 3.708318708537623021, 4.285125567170706695, -1.199719254218446718 ) ) ;
#61480 = CARTESIAN_POINT ( 'NONE',  ( 2.724079341238437646, -1.242159841233332562, -1.768869243570107885 ) ) ;
#61481 = CARTESIAN_POINT ( 'NONE',  ( 8.174640274396848483, 8.501778173076651512, 0.7998128361456291469 ) ) ;
#61482 = CARTESIAN_POINT ( 'NONE',  ( 1.499999999999990896, 5.525000000000022560, 1.214306433183764966E-14 ) ) ;
#61484 = CARTESIAN_POINT ( 'NONE',  ( -9.483599735403307918, -9.201296717416616033, 0.5591315121169729840 ) ) ;
#61483 = CARTESIAN_POINT ( 'NONE',  ( 6.994027139803230320, 9.253060644560830994, -1.599625672291267398 ) ) ;
#61485 = CARTESIAN_POINT ( 'NONE',  ( 7.524412065460039933, 10.76193592880331984, -1.082531754730537976 ) ) ;
#61487 = CARTESIAN_POINT ( 'NONE',  ( 8.865490439548599610, 14.65774821460601274, -8.021509641190812445 ) ) ;
#61486 = CARTESIAN_POINT ( 'NONE',  ( 0.3972422249299937258, 0.3718246657071262451, 2.138946393809169511 ) ) ;
#61488 = CARTESIAN_POINT ( 'NONE',  ( -5.992340707560165569, 8.014150130285418783, 1.443375672974064550 ) ) ;
#61489 = CARTESIAN_POINT ( 'NONE',  ( 1.364683531249986537, 2.405208333674752286, -0.7879004041258239610 ) ) ;
#61490 = CARTESIAN_POINT ( 'NONE',  ( 2.472451708263478931, -2.098117355222902436, -0.6331711661175795092 ) ) ;
#61491 = CARTESIAN_POINT ( 'NONE',  ( 6.883263157960365142, -0.001323150302089473379, 1.953658984494692330 ) ) ;
#61492 = CARTESIAN_POINT ( 'NONE',  ( 2.096875702627752691, -0.6037365238656807742, -2.180425337281781673 ) ) ;
#61493 = CARTESIAN_POINT ( 'NONE',  ( -7.718669524881690336, 7.899535955317097624, 0.7998128361456462443 ) ) ;
#61494 = CARTESIAN_POINT ( 'NONE',  ( -0.6823417656250212460, 4.113541667008085767, 1.181850606188767472 ) ) ;
#61495 = CARTESIAN_POINT ( 'NONE',  ( 4.920187338115698417, 7.999083482620499730, 0.9937779052983791717 ) ) ;
#61496 = CARTESIAN_POINT ( 'NONE',  ( 1.499999999999993117, 12.10416666666666430, 0.8660254037844409281 ) ) ;
#61497 = CARTESIAN_POINT ( 'NONE',  ( 6.699137298928153683, 7.948653282571920720, 1.082531754730549967 ) ) ;
#61498 = CARTESIAN_POINT ( 'NONE',  ( 4.481574309046215454, 1.155277477370730832, 1.340746495013745543 ) ) ;
#61499 = MECHANICAL_DESIGN_GEOMETRIC_PRESENTATION_REPRESENTATION (  '', ( #154890 ), #40802 ) ;
#61500 = CARTESIAN_POINT ( 'NONE',  ( 7.425061681778431399, 11.81432239538354345, 0.7998128361456462443 ) ) ;
#61501 = CARTESIAN_POINT ( 'NONE',  ( 0.8507726699197988296, 0.6114878368043925594, 2.015236747771311343 ) ) ;
#61503 = CARTESIAN_POINT ( 'NONE',  ( -1.402160292154681736E-14, 0.5875000000000220046, -1.732050807568863648 ) ) ;
#61502 = CARTESIAN_POINT ( 'NONE',  ( -1.402160292154681736E-14, 8.671875000341403350, 1.575800808251682339 ) ) ;
#61504 = CARTESIAN_POINT ( 'NONE',  ( -5.472651281771599763, 6.413789912602166687, 1.199719254218452935 ) ) ;
#61505 = CARTESIAN_POINT ( 'NONE',  ( 6.603150281434943203, -0.1430492952050037847, 1.984088717376513822 ) ) ;
#61506 = ORIENTED_EDGE ( 'NONE', *, *, #53727, .F. ) ;
#61507 = AXIS2_PLACEMENT_3D ( 'NONE', #111697, #108499, #44516 ) ;
#61508 = EDGE_CURVE ( 'NONE', #75373, #210434, #125674, .T. ) ;
#61509 = CARTESIAN_POINT ( 'NONE',  ( 7.886038904643079661, 12.35212915539230139, -0.7998128361456352531 ) ) ;
#61510 = CARTESIAN_POINT ( 'NONE',  ( 4.223419137798128276, -1.790188510885984297, 0.5427707113358354318 ) ) ;
#61511 = CARTESIAN_POINT ( 'NONE',  ( 4.592674910654532816, 2.029287475768901228, 0.4089837765668055680 ) ) ;
#61512 = CARTESIAN_POINT ( 'NONE',  ( -5.099275172071237705, 8.963255110809500437, 0.000000000000000000 ) ) ;
#61513 = CARTESIAN_POINT ( 'NONE',  ( 0.000000000000000000, 11.37999999999998302, 0.000000000000000000 ) ) ;
#61514 = CARTESIAN_POINT ( 'NONE',  ( 9.576136569953906275, 10.06658084123472641, 0.000000000000000000 ) ) ;
#61515 = CARTESIAN_POINT ( 'NONE',  ( -9.561524646135538319, 12.17819805862340310, -1.599625672291263179 ) ) ;
#61516 = FILL_AREA_STYLE_COLOUR ( '', #169905 ) ;
#61517 = CARTESIAN_POINT ( 'NONE',  ( 6.315313271410192719, -0.2696487299426887363, 2.144762774094311375 ) ) ;
#61518 = CARTESIAN_POINT ( 'NONE',  ( -0.6823417656250003738, -0.7822916663252423852, -1.181850606188749264 ) ) ;
#61519 = CARTESIAN_POINT ( 'NONE',  ( 3.508209890309890167, 1.962046631884439174, 0.002529298861464468473 ) ) ;
#61520 = CARTESIAN_POINT ( 'NONE',  ( 0.5970295589228531430, 1.038836743281198238, -1.727736137786803461 ) ) ;
#61521 = CARTESIAN_POINT ( 'NONE',  ( -4.995253251992230581, 4.792493313604505367, 0.000000000000000000 ) ) ;
#61523 = DIRECTION ( 'NONE',  ( 0.2460297208025343518, 8.326672684688694761E-16, 0.9692622846690297500 ) ) ;
#61522 = CARTESIAN_POINT ( 'NONE',  ( 9.108380270282433244, 9.520865158284665952, 1.040834085586084257E-14 ) ) ;
#61524 = CARTESIAN_POINT ( 'NONE',  ( 0.8779421195594695471, -1.044212112285093585, 1.551753832453220294 ) ) ;
#61525 = CARTESIAN_POINT ( 'NONE',  ( -1.364683531250010295, 4.280208333674753618, 0.7879004041258379498 ) ) ;
#61526 = CARTESIAN_POINT ( 'NONE',  ( 3.181892525975566155, 1.963218260121324166, -0.4451317699624996460 ) ) ;
#61528 = CARTESIAN_POINT ( 'NONE',  ( 2.091562808734966250, -0.4604446976123123814, 2.066416142659666111 ) ) ;
#61527 = CARTESIAN_POINT ( 'NONE',  ( -6.236387472606153892, 8.298871356172400127, -1.443375672974059665 ) ) ;
#61529 = CARTESIAN_POINT ( 'NONE',  ( 8.432907547770344792, 13.95827226627088180, -8.537830883650524783 ) ) ;
#61530 = CARTESIAN_POINT ( 'NONE',  ( 3.912603064140641074, 0.7423916865902054907, 1.932869565047180549 ) ) ;
#61531 = CARTESIAN_POINT ( 'NONE',  ( 7.693325821111733021, 7.940244644243982464, -0.7998128361456341429 ) ) ;
#61533 = CARTESIAN_POINT ( 'NONE',  ( 11.91292854676725987, 13.61481529673029556, 1.446370920797347415 ) ) ;
#61532 = CARTESIAN_POINT ( 'NONE',  ( 0.5914941650546343688, -0.7489122546765265565, 1.952206342558031160 ) ) ;
#61535 = ORIENTED_EDGE ( 'NONE', *, *, #60818, .T. ) ;
#61534 = CARTESIAN_POINT ( 'NONE',  ( 5.491160184941096922, 1.609068807629027820, -0.8623064814072267659 ) ) ;
#61536 = CARTESIAN_POINT ( 'NONE',  ( 7.377608144130607393, 11.75895993479440982, -0.7998128361456291469 ) ) ;
#61537 = CARTESIAN_POINT ( 'NONE',  ( 2.493739017040997208, 8.265916556960590356, -2.456386464945223835 ) ) ;
#61538 = CARTESIAN_POINT ( 'NONE',  ( 10.15942246637696655, 13.50131128642754952, -7.248264454434499626 ) ) ;
#61539 = CARTESIAN_POINT ( 'NONE',  ( 6.264705869774118696, -1.564926740429407603, 1.556175991035801287 ) ) ;
#61540 = CARTESIAN_POINT ( 'NONE',  ( -1.364683531250014514, 12.40104166700806054, -0.7879004041258335089 ) ) ;
#61541 = CARTESIAN_POINT ( 'NONE',  ( 4.600206319907148789, -0.8982956317880007591, 1.688143452400918454 ) ) ;
#61542 = CARTESIAN_POINT ( 'NONE',  ( -9.345647958521597687, 9.797677461230342999, 0.7998128361456462443 ) ) ;
#61543 = CARTESIAN_POINT ( 'NONE',  ( 5.459129407796876166, 9.520734742405036144, 1.040834085586084257E-14 ) ) ;
#61544 = CARTESIAN_POINT ( 'NONE',  ( -0.6801582343750108839, 2.880208333674722176, -1.178068619123848526 ) ) ;
#61545 = CARTESIAN_POINT ( 'NONE',  ( 3.836594282542914236, 5.499112634431936542, 1.443375672974062551 ) ) ;
#61546 = CARTESIAN_POINT ( 'NONE',  ( 9.516020521606803229, -8.176244038172738371, -0.3909723190920387226 ) ) ;
#61547 = EDGE_CURVE ( 'NONE', #34023, #149597, #73640, .T. ) ;
#61548 = CARTESIAN_POINT ( 'NONE',  ( 5.169736645512481132, 4.925780929386339935, 0.7998128361456341429 ) ) ;
#61549 = EDGE_LOOP ( 'NONE', ( #111173, #153638, #147456 ) ) ;
#61550 = AXIS2_PLACEMENT_3D ( 'NONE', #157718, #74323, #109020 ) ;
#61551 = CARTESIAN_POINT ( 'NONE',  ( -7.923814432544069142, 8.209148024248356990, 0.000000000000000000 ) ) ;
#61552 = EDGE_CURVE ( 'NONE', #17896, #204026, #16940, .T. ) ;
#61553 = CARTESIAN_POINT ( 'NONE',  ( -3.824766175154623582, 7.348582304423016964, -0.7466790275774716212 ) ) ;
#61554 = CARTESIAN_POINT ( 'NONE',  ( 5.936491157937257235, 8.019268665717216749, 1.599625672291268286 ) ) ;
#61555 = FILL_AREA_STYLE ('',( #77801 ) ) ;
#61556 = CARTESIAN_POINT ( 'NONE',  ( -5.333877144031607287, 7.620261487198364492, 1.234409035313356107 ) ) ;
#61557 = CARTESIAN_POINT ( 'NONE',  ( -5.097502569058210753, 7.930541516334467467, -1.082531754730549967 ) ) ;
#61558 = CARTESIAN_POINT ( 'NONE',  ( 3.161022370280501814, 6.839609865302569425, 0.000000000000000000 ) ) ;
#61559 = CARTESIAN_POINT ( 'NONE',  ( 2.500782807205007341, 0.4266943614082556180, 1.922505800989605218 ) ) ;
#61561 = CARTESIAN_POINT ( 'NONE',  ( 2.952750085323506024, -1.864176452196796507, -0.7691048347045483791 ) ) ;
#61560 = B_SPLINE_CURVE_WITH_KNOTS ( 'NONE', 3,
 ( #76829, #45425, #29158, #95249, #161298, #145082, #211085, #135995 ),
 .UNSPECIFIED., .F., .F.,
 ( 4, 2, 2, 4 ),
 ( 0.0001232303426307903009, 0.0004276537133814902261, 0.0005798653987568402023, 0.0007320770841321901784 ),
 .UNSPECIFIED. ) ;
#61562 = CARTESIAN_POINT ( 'NONE',  ( -6.496328159242330536, 10.73079995242472862, 0.000000000000000000 ) ) ;
#61563 = CARTESIAN_POINT ( 'NONE',  ( 5.367048706163317640, 7.354919138647580290, -1.599625672291281386 ) ) ;
#61564 = CARTESIAN_POINT ( 'NONE',  ( 6.827182134110199030, 6.034458849223407029, 2.683941674059683979 ) ) ;
#61565 = CARTESIAN_POINT ( 'NONE',  ( 3.644632398932126094, -1.791719913761843364, 1.261548167004488130 ) ) ;
#61566 = CARTESIAN_POINT ( 'NONE',  ( -5.561826481650498977, 5.891466595178788346, -0.7788020862528137744 ) ) ;
#61567 = CARTESIAN_POINT ( 'NONE',  ( 2.538006180297863068, 0.9099634639774205613, -1.697936525022441190 ) ) ;
#61568 = CARTESIAN_POINT ( 'NONE',  ( -8.136864746495904299, 12.64475930422059768, -0.7998128361456281477 ) ) ;
#61569 = CARTESIAN_POINT ( 'NONE',  ( 0.1331565106231571705, 2.881392620029461504, -2.434650611646618223 ) ) ;
#61570 = EDGE_CURVE ( 'NONE', #39641, #121817, #116123, .T. ) ;
#61571 = CARTESIAN_POINT ( 'NONE',  ( 3.119784744920330422, 6.653849612466795627, 0.7216878364870257245 ) ) ;
#61572 = CARTESIAN_POINT ( 'NONE',  ( 8.620286740190458374, 8.951422706510690830, 1.040834085586084257E-14 ) ) ;
#61573 = CARTESIAN_POINT ( 'NONE',  ( -6.825099317097829577, -8.105676417795773858, 6.608557002163587768 ) ) ;
#61574 = CARTESIAN_POINT ( 'NONE',  ( 5.478903473698239601, 7.485416367438324059, -1.443375672974078761 ) ) ;
#61575 = ORIENTED_EDGE ( 'NONE', *, *, #13673, .F. ) ;
#61577 = CARTESIAN_POINT ( 'NONE',  ( 1.805339258485965992, 1.750370858315702272, -0.9942575048343755828 ) ) ;
#61576 = CARTESIAN_POINT ( 'NONE',  ( 5.126429434416579056, 0.1410513515392505246, 1.835921608166577013 ) ) ;
#61578 = CARTESIAN_POINT ( 'NONE',  ( 3.884340333706528092, -0.1737987063687232436, 2.291882653078499477 ) ) ;
#61580 = CARTESIAN_POINT ( 'NONE',  ( 2.096333906143353243, 1.839810448830980105, 0.2789567515945317600 ) ) ;
#61579 = CARTESIAN_POINT ( 'NONE',  ( -0.1290005225502675879, 2.860092606084875033, -2.662085506130333457 ) ) ;
#61581 = CARTESIAN_POINT ( 'NONE',  ( 3.285556943749998737, -1.305208332855376296, -1.896917185911906500 ) ) ;
#61582 = DIRECTION ( 'NONE',  ( 0.6507913734559640506, -0.7592566023653003482, 0.000000000000000000 ) ) ;
#61583 = CARTESIAN_POINT ( 'NONE',  ( 6.011958326525193463, -0.6379227081053112647, 1.803018720113582773 ) ) ;
#61584 = CARTESIAN_POINT ( 'NONE',  ( -8.830438121202295321, 9.196599317691152464, -0.7998128361456291469 ) ) ;
#61585 = CARTESIAN_POINT ( 'NONE',  ( -5.966997003790232235, 7.094489604910957148, -1.082531754730549967 ) ) ;
#61587 = CARTESIAN_POINT ( 'NONE',  ( 3.168673215318769110, -1.727878594304608217, -0.7172629358194044791 ) ) ;
#61586 = CARTESIAN_POINT ( 'NONE',  ( 4.792568760853118448, 1.737405308921141645, -1.162709912544395152 ) ) ;
#61588 = CARTESIAN_POINT ( 'NONE',  ( 6.561783159334121152, 8.678499657355050800, -1.443375672974057666 ) ) ;
#61589 = VERTEX_POINT ( 'NONE', #159156 ) ;
#61590 = LINE ( 'NONE', #193716, #202155 ) ;
#61591 = CARTESIAN_POINT ( 'NONE',  ( 6.586556832619708146, -1.693200007625778492, -0.3281344310326217428 ) ) ;
#61592 = CARTESIAN_POINT ( 'NONE',  ( -7.223796917982883592, 7.322184580601816428, -0.7998128361456291469 ) ) ;
#61593 = CARTESIAN_POINT ( 'NONE',  ( 1.072469862579095379, -0.7803941858975007584, 1.548669665330544953 ) ) ;
#61594 = PRESENTATION_STYLE_ASSIGNMENT (( #13890 ) ) ;
#61595 = CARTESIAN_POINT ( 'NONE',  ( -1.284279953904128524, 10.64264068711930733, -0.7749999999999892530 ) ) ;
#61596 = AXIS2_PLACEMENT_3D ( 'NONE', #205964, #42436, #22928 ) ;
#61597 = FILL_AREA_STYLE_COLOUR ( '', #138096 ) ;
#61598 = CARTESIAN_POINT ( 'NONE',  ( 5.524361701572801486, 1.063745579927848794, 1.892525341434271091 ) ) ;
#61599 = CARTESIAN_POINT ( 'NONE',  ( 5.004447790439923160, -0.6182884515001166870, -1.717943145347331502 ) ) ;
#61600 = CARTESIAN_POINT ( 'NONE',  ( 1.903102209365503894, -1.660057620245494636, 1.045011325395063251 ) ) ;
#61601 = CARTESIAN_POINT ( 'NONE',  ( 0.2986504545328653726, 1.456477371935499088, -1.536899124724122601 ) ) ;
#61602 = CARTESIAN_POINT ( 'NONE',  ( 4.370663978927085580, 5.060324124126027279, 7.500000000000000000 ) ) ;
#61603 = CARTESIAN_POINT ( 'NONE',  ( -9.022061154889962964, 12.61315621642528129, -1.199719254218446718 ) ) ;
#61604 = CARTESIAN_POINT ( 'NONE',  ( 7.052212457402625922, 11.37933163361175382, -0.7998128361456291469 ) ) ;
#61605 = CARTESIAN_POINT ( 'NONE',  ( 2.631617588254760776, -0.2053842346896698201, 2.110501108333342035 ) ) ;
#61606 = CARTESIAN_POINT ( 'NONE',  ( -2.968872451712654126, 6.407508927065978632, 1.040834085586084257E-14 ) ) ;
#61607 = CARTESIAN_POINT ( 'NONE',  ( -4.595871994550918771, 6.958256438637705266, -1.193191807407071536 ) ) ;
#61609 = TOROIDAL_SURFACE ( 'NONE', #134169, 7.750000000000000888, 0.7500000000000000000 ) ;
#61608 = TOROIDAL_SURFACE ( 'NONE', #179297, 11.92000000000000171, 0.08000000000000000167 ) ;
#61610 = CARTESIAN_POINT ( 'NONE',  ( 6.930535145478218695, -1.343193056793217988, 1.706537673033242664 ) ) ;
#61612 = CARTESIAN_POINT ( 'NONE',  ( -1.500000000000015099, 14.01041666734946212, -0.8660254037844309360 ) ) ;
#61611 = DIRECTION ( 'NONE',  ( -1.084202172485362439E-14, -1.000000000000000000, -3.260636891504970529E-14 ) ) ;
#61614 = ORIENTED_EDGE ( 'NONE', *, *, #169387, .T. ) ;
#61613 = CARTESIAN_POINT ( 'NONE',  ( 2.948112417477159575, -1.493347798232132373, -1.644555409524293577 ) ) ;
#61615 = CARTESIAN_POINT ( 'NONE',  ( 0.3703313985920617668, -0.2899475993979240274, -2.280306813078219363 ) ) ;
#61617 = CARTESIAN_POINT ( 'NONE',  ( 6.051645708474242547, 1.558200330177769377, 1.351431136778310726 ) ) ;
#61616 = CARTESIAN_POINT ( 'NONE',  ( 2.198393463710220264, 5.716542807637226886, 0.7998128361456462443 ) ) ;
#61619 = CARTESIAN_POINT ( 'NONE',  ( 3.475000000000000533, -2.245833333333331350, -2.006292185433951047 ) ) ;
#61618 = CARTESIAN_POINT ( 'NONE',  ( 5.285699784481295183, 7.260012063351913625, 1.599625672291268286 ) ) ;
#61620 = EDGE_CURVE ( 'NONE', #143294, #125996, #105738, .T. ) ;
#61621 = CARTESIAN_POINT ( 'NONE',  ( 0.1329588055935213564, 1.397696041676167678, -2.105440929937075989 ) ) ;
#61622 = CARTESIAN_POINT ( 'NONE',  ( 5.601068772352080671, -0.4412860211496574814, 1.787476196608045464 ) ) ;
#61623 = CARTESIAN_POINT ( 'NONE',  ( -5.249999999999987566, 0.000000000000000000, 1.599999999999997202 ) ) ;
#61624 = ADVANCED_FACE ( 'NONE', ( #190574 ), #108346, .F. ) ;
#61625 = CARTESIAN_POINT ( 'NONE',  ( 5.352771719296971042, 5.139321848801576387, 0.7998128361456341429 ) ) ;
#61626 = CARTESIAN_POINT ( 'NONE',  ( -4.911285141672522059, 4.693790260148114513, 0.3511878651327460243 ) ) ;
#61627 = CARTESIAN_POINT ( 'NONE',  ( 3.434305118180380756, 1.682496158873967529, 0.3786907865064632062 ) ) ;
#61628 = CARTESIAN_POINT ( 'NONE',  ( 0.8488426437929346147, -1.825078332268307513, -0.8578388575243289793 ) ) ;
#61629 = CARTESIAN_POINT ( 'NONE',  ( 2.655266180633470086, 1.232652804806773528, 1.940110688254999438 ) ) ;
#61630 = CARTESIAN_POINT ( 'NONE',  ( -0.6823417656249969321, 3.530208333674754506, -1.181850606188749264 ) ) ;
#61631 = CARTESIAN_POINT ( 'NONE',  ( 2.812116484403729633, -2.238188867732244791, 0.3292703641907517298 ) ) ;
#61632 = CARTESIAN_POINT ( 'NONE',  ( 4.881522348829672175, 1.965384978258335247, -0.7572991678025364770 ) ) ;
#61633 = CARTESIAN_POINT ( 'NONE',  ( -6.292392690518202159, 9.394856334696294553, -1.082531754730549967 ) ) ;
#61634 = CARTESIAN_POINT ( 'NONE',  ( 4.059615542810626643, 1.756569389245852042, -0.2146349482602862846 ) ) ;
#61635 = CARTESIAN_POINT ( 'NONE',  ( 4.690231075323689325, 7.559354456931247412, 1.199719254218462483 ) ) ;
#61637 = CARTESIAN_POINT ( 'NONE',  ( 6.198803536200695241, 1.903451089567553822, 1.277169966706873883 ) ) ;
#61636 = CARTESIAN_POINT ( 'NONE',  ( 4.895902867866261055, 4.884510565364971413, -0.7216878364870458196 ) ) ;
#61638 = CARTESIAN_POINT ( 'NONE',  ( 4.804558796598876746, 1.603369264058150279, 0.9048477820690554729 ) ) ;
#61639 = CARTESIAN_POINT ( 'NONE',  ( -4.249591082879585535, 7.045274465746411252, 1.199719254218464037 ) ) ;
#61640 = CARTESIAN_POINT ( 'NONE',  ( 4.311129659021211147, 7.973475668925984472, 1.040834085586084257E-14 ) ) ;
#61641 = CARTESIAN_POINT ( 'NONE',  ( -1.201851678989727383E-14, 3.212500000000018119, 1.732050807568877637 ) ) ;
#61642 = CARTESIAN_POINT ( 'NONE',  ( 4.259861650310483583, 1.032037387010206198, 1.933225914978464299 ) ) ;
#61643 = CARTESIAN_POINT ( 'NONE',  ( -4.192495815123836955, 5.914331089109674089, -1.599625672291256295 ) ) ;
#61644 = CARTESIAN_POINT ( 'NONE',  ( 0.2652791711382319617, 7.171141847836379313, -2.094821536884158508 ) ) ;
#61645 = CARTESIAN_POINT ( 'NONE',  ( 0.000000000000000000, 3.499999999999989342, 12.00000000000000178 ) ) ;
#61646 = STYLED_ITEM ( 'NONE', ( #193556 ), #106360 ) ;
#61647 = CARTESIAN_POINT ( 'NONE',  ( 1.364683531249988535, 4.113541667008088432, 0.7879004041258500513 ) ) ;
#61648 = CARTESIAN_POINT ( 'NONE',  ( 3.738824155997504395, 0.2837420414000761393, 1.905379044178076686 ) ) ;
#61649 = CARTESIAN_POINT ( 'NONE',  ( 1.364683531250000303, 9.505208333674735499, -0.7879004041258355073 ) ) ;
#61650 = CARTESIAN_POINT ( 'NONE',  ( -4.202664430556263930, 5.926194473780837413, 1.443375672974064550 ) ) ;
#61651 = CARTESIAN_POINT ( 'NONE',  ( 6.310795917644286490, -0.5669512758468171487, -2.043305014803979525 ) ) ;
#61652 = ORIENTED_EDGE ( 'NONE', *, *, #171517, .T. ) ;
#61654 =( NAMED_UNIT ( * ) PLANE_ANGLE_UNIT ( ) SI_UNIT ( $, .RADIAN. ) );
#61653 = CARTESIAN_POINT ( 'NONE',  ( 1.299038105676669330, 6.499999999999999112, -0.7500000000000006661 ) ) ;
#61655 = CARTESIAN_POINT ( 'NONE',  ( 5.190073875932979419, 4.949507698210251938, 0.7998128361456341429 ) ) ;
#61656 = CARTESIAN_POINT ( 'NONE',  ( 7.787098537122153274, -5.543994141378499663, -7.698131257602417676 ) ) ;
#61657 = DIRECTION ( 'NONE',  ( 0.000000000000000000, 0.000000000000000000, 1.000000000000000000 ) ) ;
#61658 = CARTESIAN_POINT ( 'NONE',  ( 4.911177513620411439, 4.783069230954930084, 0.3872126393177600101 ) ) ;
#61659 = CARTESIAN_POINT ( 'NONE',  ( 2.665247472508886606, 0.9327722559238416089, 1.469172323213832065 ) ) ;
#61660 = CARTESIAN_POINT ( 'NONE',  ( 3.553238514845298734, 7.337208092372121904, -0.2327671511505452484 ) ) ;
#61662 = CARTESIAN_POINT ( 'NONE',  ( 11.81905481421901705, 12.34264344382731871, 1.592167362352177262 ) ) ;
#61661 = CIRCLE ( 'NONE', #141333, 4.022469383779238683 ) ;
#61663 = CARTESIAN_POINT ( 'NONE',  ( 0.6823417656249882723, 0.7385416670080829915, -1.181850606188749264 ) ) ;
#61664 = CARTESIAN_POINT ( 'NONE',  ( 6.280167721515548251, -1.160692707240444710, 1.823489969145650313 ) ) ;
#61665 = CARTESIAN_POINT ( 'NONE',  ( -8.272446282632566650, 12.80293776304669962, 0.7998128361456481317 ) ) ;
#61666 = CARTESIAN_POINT ( 'NONE',  ( -5.219525951136845698, 8.072902128759544382, -1.082531754730543971 ) ) ;
#61667 = CARTESIAN_POINT ( 'NONE',  ( 6.280167721515548251, -1.160692707240444710, 1.823489969145650313 ) ) ;
#61669 = ORIENTED_EDGE ( 'NONE', *, *, #76744, .F. ) ;
#61668 = DIRECTION ( 'NONE',  ( 1.000000000000000000, 0.000000000000000000, -1.665334536937734811E-16 ) ) ;
#61670 = CARTESIAN_POINT ( 'NONE',  ( 1.364683531249990311, 4.384375000341417028, 1.214306433183764966E-14 ) ) ;
#61671 = CARTESIAN_POINT ( 'NONE',  ( 0.2275331484566482099, -1.145445245298154946, -1.479381579510357980 ) ) ;
#61672 = CARTESIAN_POINT ( 'NONE',  ( 5.905553417332951582, 0.3413034225961882884, 1.699694455674398919 ) ) ;
#61674 = CARTESIAN_POINT ( 'NONE',  ( 3.632539538618652752, 0.3231117836275976818, 2.167502126216628522 ) ) ;
#61673 = CARTESIAN_POINT ( 'NONE',  ( 1.360316468749963592, 0.03645833367470611985, -0.7853790794159122290 ) ) ;
#61675 = CARTESIAN_POINT ( 'NONE',  ( 3.856711057068095805, 0.8274802039119494301, 2.154294293310366371 ) ) ;
#61676 = CARTESIAN_POINT ( 'NONE',  ( 5.659468487958158711, 0.4062720387869744876, -2.020156115232510707 ) ) ;
#61677 = CARTESIAN_POINT ( 'NONE',  ( 1.429522090333503304, 0.9575595492820774268, -1.689375863068052430 ) ) ;
#61678 = CARTESIAN_POINT ( 'NONE',  ( -6.412643469139482910, 7.544134137826577380, 1.082531754730549967 ) ) ;
#61679 = DIRECTION ( 'NONE',  ( -0.000000000000000000, -1.000000000000000000, -0.000000000000000000 ) ) ;
#61680 = CARTESIAN_POINT ( 'NONE',  ( 11.84100621633422179, 11.11041574223334649, 1.444132586618105174 ) ) ;
#61681 = CARTESIAN_POINT ( 'NONE',  ( 4.447591161967184625, -1.937652164471121763, 0.8620916771790232414 ) ) ;
#61682 =( NAMED_UNIT ( * ) SI_UNIT ( $, .STERADIAN. ) SOLID_ANGLE_UNIT ( ) );
#61683 = CARTESIAN_POINT ( 'NONE',  ( 1.881482635453747720, -0.5404922439061732309, -1.942541187959702764 ) ) ;
#61684 = CARTESIAN_POINT ( 'NONE',  ( -5.788968402910818156, 7.776882441527838807, 1.443375672974064550 ) ) ;
#61685 = CARTESIAN_POINT ( 'NONE',  ( 5.227635310461984375, -2.096914331502324647, 0.6878394029543041244 ) ) ;
#61686 = FACE_OUTER_BOUND ( 'NONE', #185159, .T. ) ;
#61687 = CARTESIAN_POINT ( 'NONE',  ( 0.008622056077349157799, 14.55305231409391808, 11.95585894185517084 ) ) ;
#61688 = EDGE_CURVE ( 'NONE', #154255, #149077, #17815, .T. ) ;
#61689 = CARTESIAN_POINT ( 'NONE',  ( -10.91944002402978775, -9.999999999999994671, 0.1105873483556694958 ) ) ;
#61691 = CARTESIAN_POINT ( 'NONE',  ( 3.877268743828242936, 7.467304601200888570, 0.7216878364870187301 ) ) ;
#61690 = CARTESIAN_POINT ( 'NONE',  ( -5.586845290032572464, 7.502486493224762576, 1.347716017753825879 ) ) ;
#61692 = DIRECTION ( 'NONE',  ( -1.000000000000000000, 0.000000000000000000, -8.638326563840826660E-31 ) ) ;
#61693 = ORIENTED_EDGE ( 'NONE', *, *, #40364, .T. ) ;
#61694 = CARTESIAN_POINT ( 'NONE',  ( 4.733308493599470701, -1.885100903509504544, 0.8332785242166717010 ) ) ;
#61695 = FACE_OUTER_BOUND ( 'NONE', #7848, .T. ) ;
#61696 = CARTESIAN_POINT ( 'NONE',  ( 0.4734109229373711925, 6.656475628599715755, -3.353491478376180890 ) ) ;
#61697 = CARTESIAN_POINT ( 'NONE',  ( -5.037017762676898158, 5.835274463666530131, -1.199719254218446718 ) ) ;
#61698 = CARTESIAN_POINT ( 'NONE',  ( -3.709037541790315640, 6.484905011134099340, -1.199719254218450271 ) ) ;
#61699 = CARTESIAN_POINT ( 'NONE',  ( 5.057288377774205479, -1.731171949422895651, 1.040023186547271328 ) ) ;
#61700 = CARTESIAN_POINT ( 'NONE',  ( -0.7500000000000215383, 0.9416666666666878571, 1.299038105676659116 ) ) ;
#61701 = AXIS2_PLACEMENT_3D ( 'NONE', #103577, #169635, #21218 ) ;
#61703 = CARTESIAN_POINT ( 'NONE',  ( 8.839552966430002101, 11.33589776563360019, -1.443375672974052559 ) ) ;
#61702 = CARTESIAN_POINT ( 'NONE',  ( -3.806807270387036368, 7.663301925418665839, 0.000000000000000000 ) ) ;
#61704 = CARTESIAN_POINT ( 'NONE',  ( 7.039708073993665494, 9.236078724457858158, 1.599625672291281386 ) ) ;
#61705 = CARTESIAN_POINT ( 'NONE',  ( 2.887629844759795450, 1.456389637235107948, 1.458414562493230759 ) ) ;
#61706 = CARTESIAN_POINT ( 'NONE',  ( 2.883435573726996548, -0.5880205015329244000, -1.928751729079546173 ) ) ;
#61707 = EDGE_LOOP ( 'NONE', ( #109469, #90878, #70491, #174290 ) ) ;
#61708 = CARTESIAN_POINT ( 'NONE',  ( 1.250000000000037526, 8.500000000000000000, 10.85702537530423406 ) ) ;
#61709 = CARTESIAN_POINT ( 'NONE',  ( 3.018661757337009810, 6.673522483535157868, 0.000000000000000000 ) ) ;
#61711 = EDGE_LOOP ( 'NONE', ( #185570, #164276, #139244, #77497 ) ) ;
#61710 = CARTESIAN_POINT ( 'NONE',  ( -0.4636475088197898886, 7.942422027498800219, -1.946104516853415678 ) ) ;
#61712 = CARTESIAN_POINT ( 'NONE',  ( 2.706407486732204770, -1.492025830231600070, -1.356093404896424826 ) ) ;
#61713 = CARTESIAN_POINT ( 'NONE',  ( 2.343484645521694887, 1.840739972059933560, 0.04548452486473342216 ) ) ;
#61714 = CARTESIAN_POINT ( 'NONE',  ( 0.5402173299829955422, -1.636151841282366126, -1.627667753820499330 ) ) ;
#61715 = CARTESIAN_POINT ( 'NONE',  ( 3.711900195091365262, 7.552577004240394132, -0.7998128361456362523 ) ) ;
#61716 = CARTESIAN_POINT ( 'NONE',  ( 3.005316911853897821, 1.824354345256746557, 1.159134172154026032 ) ) ;
#61717 = CIRCLE ( 'NONE', #137950, 11.49999999999998934 ) ;
#61718 = CARTESIAN_POINT ( 'NONE',  ( -6.738566041191992539, 7.820414121934134322, 1.199719254218450271 ) ) ;
#61719 = CARTESIAN_POINT ( 'NONE',  ( 2.794613785990595733, -2.145299970026095071, 0.8252070097543462435 ) ) ;
#61720 = EDGE_LOOP ( 'NONE', ( #152806, #144072, #89534, #145480, #137481, #49975, #107044, #86703, #98395, #122164, #23423, #82378, #145777, #10814, #5844, #115042 ) ) ;
#61721 = CARTESIAN_POINT ( 'NONE',  ( 2.168404344971008868E-16, -7.246166700193014343, -9.579665964947887247 ) ) ;
#61722 = CARTESIAN_POINT ( 'NONE',  ( 1.463515404423965105, 1.843522461416190250, -0.3164952454337774390 ) ) ;
#61723 = CARTESIAN_POINT ( 'NONE',  ( 5.963742398600946792, 1.942370021616221409, -0.3365726279523760800 ) ) ;
#61725 = CARTESIAN_POINT ( 'NONE',  ( 8.554831740098654436, 11.00372300158037042, 1.443375672974076540 ) ) ;
#61724 = CARTESIAN_POINT ( 'NONE',  ( -1.201851678989727383E-14, 3.321875000341421025, 1.575800808251672791 ) ) ;
#61727 = CARTESIAN_POINT ( 'NONE',  ( 1.014635385311330795, -0.9952708415592588231, -1.969785480804244315 ) ) ;
#61726 = CARTESIAN_POINT ( 'NONE',  ( -6.388916700537716764, 8.476822122092563916, 1.599625672291283607 ) ) ;
#61728 = CARTESIAN_POINT ( 'NONE',  ( 6.232888004217203459, -1.964670499678453197, -0.6532144590316590893 ) ) ;
#61729 = CARTESIAN_POINT ( 'NONE',  ( 4.659198344590585350, 8.587481835331020719, 0.7998128361456462443 ) ) ;
#61730 = CARTESIAN_POINT ( 'NONE',  ( -4.740547266272593596, 8.682388910626682943, -0.7998128361456281477 ) ) ;
#61731 = CARTESIAN_POINT ( 'NONE',  ( 6.639320575229281651, 0.5623622132289189945, 2.255000583061476771 ) ) ;
#61732 = CARTESIAN_POINT ( 'NONE',  ( 4.539890248181537302, 0.8439850759212139675, -1.781816264247655157 ) ) ;
#61733 = CARTESIAN_POINT ( 'NONE',  ( 0.07077104593807002908, 0.8175350930016941353, 1.956879683024402183 ) ) ;
#61734 = CARTESIAN_POINT ( 'NONE',  ( -1.500000000000001332, 0.6812500006828161592, 0.000000000000000000 ) ) ;
#61735 = CARTESIAN_POINT ( 'NONE',  ( 4.530063604893081575, -1.417328398590127714, -1.821081770091488083 ) ) ;
#61736 = ADVANCED_FACE ( 'NONE', ( #109418 ), #9699, .T. ) ;
#61737 = CARTESIAN_POINT ( 'NONE',  ( 2.008709601793839283, 0.6428708581102732245, 1.959923294053036669 ) ) ;
#61738 = CARTESIAN_POINT ( 'NONE',  ( 7.795575138177731844, 8.197185204069915798, 1.040834085586084257E-14 ) ) ;
#61739 = CARTESIAN_POINT ( 'NONE',  ( 4.505052181490820651, 8.477920988373101707, -0.7998128361456381397 ) ) ;
#61740 = CARTESIAN_POINT ( 'NONE',  ( 4.706615602599436343, 5.520081620234675412, 1.199719254218452935 ) ) ;
#61741 = CARTESIAN_POINT ( 'NONE',  ( 1.364683531249986537, 2.217708333674751398, -0.7879004041258239610 ) ) ;
#61742 = CARTESIAN_POINT ( 'NONE',  ( -1.673882606082500946, 14.48013547004651436, 11.91749650979550701 ) ) ;
#61743 = CARTESIAN_POINT ( 'NONE',  ( 5.707619481228810798, 7.681975366232176583, -1.443375672974057666 ) ) ;
#61744 = CARTESIAN_POINT ( 'NONE',  ( 4.229095133649480864, -2.024433085375398900, -0.7850780064641171840 ) ) ;
#61746 = CARTESIAN_POINT ( 'NONE',  ( 3.860763913883006992, 0.2215400755124704024, -1.827792592973469743 ) ) ;
#61745 = CARTESIAN_POINT ( 'NONE',  ( -2.819732761962335577, 5.273143408055916304, -1.082531754730543971 ) ) ;
#61748 = CARTESIAN_POINT ( 'NONE',  ( 6.720655732516666703, 0.5845450044974825898, 1.978693153076715783 ) ) ;
#61747 = FACE_OUTER_BOUND ( 'NONE', #170195, .T. ) ;
#61749 = CARTESIAN_POINT ( 'NONE',  ( 5.021103811603734535, -2.081066139062941023, 0.6872292908843835590 ) ) ;
#61750 = CARTESIAN_POINT ( 'NONE',  ( -3.609978820808566802, 4.211641957610042120, -2.420000000000000373 ) ) ;
#61751 = CARTESIAN_POINT ( 'NONE',  ( 5.911039803662155201, 1.992093809783651803, 1.072660102914186897 ) ) ;
#61752 = VERTEX_POINT ( 'NONE', #56331 ) ;
#61753 = CARTESIAN_POINT ( 'NONE',  ( -4.432925279414208219, 7.308574008990986748, -1.253226476263115341 ) ) ;
#61754 = CYLINDRICAL_SURFACE ( 'NONE', #72044, 0.08000000000000041800 ) ;
#61755 = CARTESIAN_POINT ( 'NONE',  ( 5.017113787211129328, 8.018716392533608683, 1.139262206072016559 ) ) ;
#61756 = CARTESIAN_POINT ( 'NONE',  ( -4.543390873910949423, 6.393985001019784953, 1.443375672974058777 ) ) ;
#61757 = CARTESIAN_POINT ( 'NONE',  ( 4.773879485787624333, 4.742149952939897162, -0.7216878364870357165 ) ) ;
#61758 = CARTESIAN_POINT ( 'NONE',  ( 1.287592460671227457, -0.8000790430911768336, 1.578758917787604021 ) ) ;
#61760 = CARTESIAN_POINT ( 'NONE',  ( 5.197907085625908863, 1.353584514550598472, 1.490229472901122065 ) ) ;
#61759 = AXIS2_PLACEMENT_3D ( 'NONE', #59457, #22668, #122428 ) ;
#61761 = CARTESIAN_POINT ( 'NONE',  ( 7.467843683028853263, 7.606905806488803101, 0.7998128361456341429 ) ) ;
#61762 = CARTESIAN_POINT ( 'NONE',  ( 4.401466734191799901, 1.689890445582131084, 1.256493114684479329 ) ) ;
#61763 = CARTESIAN_POINT ( 'NONE',  ( 2.337376834759529398, 0.5087095155123841916, -1.846764813590465515 ) ) ;
#61764 = DIRECTION ( 'NONE',  ( 0.000000000000000000, 0.000000000000000000, -1.000000000000000000 ) ) ;
#61765 = CARTESIAN_POINT ( 'NONE',  ( 3.367590298639517421, -0.3867537717311599343, 1.931019599036578160 ) ) ;
#61767 = EDGE_CURVE ( 'NONE', #758, #103686, #23810, .T. ) ;
#61766 = CARTESIAN_POINT ( 'NONE',  ( 5.801037524829370184, -0.3003419868748377630, -1.997221587554024458 ) ) ;
#61768 = CARTESIAN_POINT ( 'NONE',  ( 1.744777856283234785, -1.581906188472384400, 0.9981555316627908070 ) ) ;
#61771 = VERTEX_POINT ( 'NONE', #55264 ) ;
#61770 = CARTESIAN_POINT ( 'NONE',  ( 1.002048865836258518, -0.8573748960705518396, 1.709468765625526521 ) ) ;
#61769 = CARTESIAN_POINT ( 'NONE',  ( 5.004412211769132313, -0.5859011197271257743, -1.622467267129880097 ) ) ;
#61773 = CARTESIAN_POINT ( 'NONE',  ( 3.877268743828266029, 6.506935386899531437, 1.082531754730558626 ) ) ;
#61772 = CARTESIAN_POINT ( 'NONE',  ( 0.9970219447392356660, -0.5395372827587068265, -2.139793933917451874 ) ) ;
#61774 = CARTESIAN_POINT ( 'NONE',  ( 1.364683531249986537, 2.467708333674753174, -0.7879004041258239610 ) ) ;
#61776 = EDGE_CURVE ( 'NONE', #23582, #73840, #166722, .T. ) ;
#61775 = CARTESIAN_POINT ( 'NONE',  ( 7.781490099239519509, 11.16582331816642260, 1.199719254218460707 ) ) ;
#61777 = CARTESIAN_POINT ( 'NONE',  ( 11.55950211276791428, 12.22000000000000064, -3.221476510067115662 ) ) ;
#61778 =( LENGTH_UNIT ( ) NAMED_UNIT ( * ) SI_UNIT ( .MILLI., .METRE. ) );
#61779 = CARTESIAN_POINT ( 'NONE',  ( -4.229253852459088137, 7.021547696922494808, 1.199719254218464037 ) ) ;
#61780 = CARTESIAN_POINT ( 'NONE',  ( 0.000000000000000000, 3.499999999999989342, 0.000000000000000000 ) ) ;
#61781 = CIRCLE ( 'NONE', #179449, 0.07999999999999969635 ) ;
#61782 = CARTESIAN_POINT ( 'NONE',  ( 1.469279758060073160, 1.824989553406907383, 0.9776941847434923449 ) ) ;
#61783 = CARTESIAN_POINT ( 'NONE',  ( -1.500000000000013101, 2.170833333333357373, 0.8660254037844403729 ) ) ;
#61784 = CARTESIAN_POINT ( 'NONE',  ( 5.961834861707224320, 7.978559976790334574, -1.599625672291262513 ) ) ;
#61785 = CARTESIAN_POINT ( 'NONE',  ( -8.050844288416501016, 8.287073179441051707, 1.040834085586084257E-14 ) ) ;
#61786 = CARTESIAN_POINT ( 'NONE',  ( 5.065906673361608270, 5.939254536123854677, -1.199719254218450271 ) ) ;
#61787 = CARTESIAN_POINT ( 'NONE',  ( 0.2760433103432077262, 1.997375541027920587, -0.2984889601853820129 ) ) ;
#61788 = CARTESIAN_POINT ( 'NONE',  ( 0.6823417656249882723, 2.926041667008084879, -1.181850606188754593 ) ) ;
#61789 = VERTEX_POINT ( 'NONE', #177550 ) ;
#61791 = CARTESIAN_POINT ( 'NONE',  ( 10.54788032175191326, 11.40820791823982994, 0.7216878364870317197 ) ) ;
#61790 = CARTESIAN_POINT ( 'NONE',  ( 6.865691018405424728, -0.4312029709039078007, 1.920920986087648163 ) ) ;
#61792 = CARTESIAN_POINT ( 'NONE',  ( 4.516953773913958692, 2.015725170860783066, -0.04666989112152990227 ) ) ;
#61793 = CARTESIAN_POINT ( 'NONE',  ( 4.223789564141206654, 0.8136391335250325874, -1.734469729061314913 ) ) ;
#61794 = CARTESIAN_POINT ( 'NONE',  ( 3.122796855005858241, 0.05607861761174406934, 2.191015320347329709 ) ) ;
#61795 = CARTESIAN_POINT ( 'NONE',  ( -11.84668730067608600, 10.19999999999998153, 1.399999999999998579 ) ) ;
#61796 = CARTESIAN_POINT ( 'NONE',  ( -1.500000000000015099, 0.6604166673494823447, -0.8660254037844313801 ) ) ;
#61797 = CARTESIAN_POINT ( 'NONE',  ( 4.992444313356595664, -1.114831962662912845, 1.676160436541684229 ) ) ;
#61798 = CARTESIAN_POINT ( 'NONE',  ( -6.531277313481209212, 8.642909503859968368, 1.599625672291283607 ) ) ;
#61800 = CARTESIAN_POINT ( 'NONE',  ( 5.782842150838196638, 1.730585719646136056, -1.219460781990765463 ) ) ;
#61799 = CARTESIAN_POINT ( 'NONE',  ( -3.145128448690317935, 5.652771709238564313, -1.082531754730549967 ) ) ;
#61801 = CARTESIAN_POINT ( 'NONE',  ( -8.012344526598182026E-15, 9.609375000341399797, -1.575800808251669460 ) ) ;
#61803 = CARTESIAN_POINT ( 'NONE',  ( -5.596483547390937119, 9.751257581923240991, 0.000000000000000000 ) ) ;
#61802 = CARTESIAN_POINT ( 'NONE',  ( 3.526972370393847811, -1.930915134098612373, 0.8022322841883463562 ) ) ;
#61805 = ORIENTED_EDGE ( 'NONE', *, *, #69350, .F. ) ;
#61804 = CARTESIAN_POINT ( 'NONE',  ( 1.641173577361688896, -1.245895879902914727, -1.192971367628747448 ) ) ;
#61806 = CARTESIAN_POINT ( 'NONE',  ( 4.851869265964163347, -1.501451181749386743, -1.497782127133556296 ) ) ;
#61807 = CARTESIAN_POINT ( 'NONE',  ( 6.986529229743720926, 7.045372277656132276, -0.7998128361456281477 ) ) ;
#61808 = CARTESIAN_POINT ( 'NONE',  ( 7.710100441483561440, -6.699703214240864568, 7.845789747616994880 ) ) ;
#61809 = STYLED_ITEM ( 'NONE', ( #22521 ), #22111 ) ;
#61810 = CARTESIAN_POINT ( 'NONE',  ( 0.000000000000000000, 0.5000000000000004441, 0.000000000000000000 ) ) ;
#61811 = CARTESIAN_POINT ( 'NONE',  ( 7.156006149914539982, 7.243095351188763686, 1.040834085586084257E-14 ) ) ;
#61812 = ORIENTED_EDGE ( 'NONE', *, *, #41018, .T. ) ;
#61813 = CARTESIAN_POINT ( 'NONE',  ( 0.000000000000000000, 11.37999999999999901, 0.000000000000000000 ) ) ;
#61815 = CARTESIAN_POINT ( 'NONE',  ( 1.453448513857479973, -1.311971142947904401, -1.249319819763055950 ) ) ;
#61814 = CARTESIAN_POINT ( 'NONE',  ( 5.879395890181562834, 6.888325289080478697, -1.199719254218452047 ) ) ;
#61816 = CARTESIAN_POINT ( 'NONE',  ( -4.882907879216086933, 8.848476292394087395, -0.7998128361456281477 ) ) ;
#61817 = ORIENTED_EDGE ( 'NONE', *, *, #195348, .F. ) ;
#61818 = CARTESIAN_POINT ( 'NONE',  ( 4.390142812726693045, 4.016254791136236513, 1.214306433183764966E-14 ) ) ;
#61819 = ORIENTED_EDGE ( 'NONE', *, *, #66399, .F. ) ;
#61820 = CARTESIAN_POINT ( 'NONE',  ( 5.631432701629774051, 7.663367133358481631, 1.599625672291269396 ) ) ;
#61821 = CARTESIAN_POINT ( 'NONE',  ( 3.105918186854994989, -0.7317858000257486673, 1.657260211903899938 ) ) ;
#61822 = CARTESIAN_POINT ( 'NONE',  ( 6.539320575229279342, 6.038407674219216759, 2.491644695858772796 ) ) ;
#61823 =( NAMED_UNIT ( * ) SI_UNIT ( $, .STERADIAN. ) SOLID_ANGLE_UNIT ( ) );
#61824 = CARTESIAN_POINT ( 'NONE',  ( 4.546345379095670047, 6.970243970676179401, 1.177900817425497904 ) ) ;
#61825 = CARTESIAN_POINT ( 'NONE',  ( 3.842128478764065047, -0.9187925100661897826, 1.618370328034287597 ) ) ;
#61826 = CARTESIAN_POINT ( 'NONE',  ( 1.792461972651203439, 1.418048008323580911, -1.288064678409290398 ) ) ;
#61827 = CARTESIAN_POINT ( 'NONE',  ( 6.317406038308035043, -0.2352959436980571473, 1.911917130847824886 ) ) ;
#61828 = CARTESIAN_POINT ( 'NONE',  ( -11.94105721237523099, 13.40000000000000036, 1.187919463087248273 ) ) ;
#61829 = CARTESIAN_POINT ( 'NONE',  ( -3.449547071718257030, 5.499999999999998224, 2.025000000000002576 ) ) ;
#61830 = CARTESIAN_POINT ( 'NONE',  ( 4.631618433768171172, 8.327536854573105884, -0.3785340233409782984 ) ) ;
#61831 = DIRECTION ( 'NONE',  ( 0.000000000000000000, 0.000000000000000000, 1.000000000000000000 ) ) ;
#61832 = DIRECTION ( 'NONE',  ( 0.000000000000000000, -1.000000000000000000, 0.000000000000000000 ) ) ;
#61833 = CARTESIAN_POINT ( 'NONE',  ( 7.402388683381404988, 10.61957531637824204, -1.082531754730537976 ) ) ;
#61834 = CARTESIAN_POINT ( 'NONE',  ( 6.192246204073627247, 0.9737480728593052026, -1.711826031884769339 ) ) ;
#61835 = CARTESIAN_POINT ( 'NONE',  ( -5.066996723205291708, 6.934582148538044777, 1.599625672291267398 ) ) ;
#61836 = CARTESIAN_POINT ( 'NONE',  ( -0.5100041365948099203, 6.733978373159967390, 3.471634244333542618 ) ) ;
#61837 = CARTESIAN_POINT ( 'NONE',  ( -0.01160896700787457207, -0.4585933848370716270, -2.046879979534850236 ) ) ;
#61838 = CARTESIAN_POINT ( 'NONE',  ( 4.970485548933691433, 6.521808019254549116, 1.328095809470300814 ) ) ;
#61839 = CARTESIAN_POINT ( 'NONE',  ( 5.807627864512785898, -0.4676060548664852101, 1.868651349408587681 ) ) ;
#61840 = CARTESIAN_POINT ( 'NONE',  ( -5.392392409933270514, 7.314210449720692786, 1.599625672291269396 ) ) ;
#61841 = CARTESIAN_POINT ( 'NONE',  ( 0.7799652524137988818, -1.018268764971082430, 1.515009401286564694 ) ) ;
#61842 = CARTESIAN_POINT ( 'NONE',  ( 2.227434312139275896, 0.001603268854937638837, 2.207063162490217056 ) ) ;
#61843 = EDGE_CURVE ( 'NONE', #47264, #211508, #14560, .T. ) ;
#61844 = CARTESIAN_POINT ( 'NONE',  ( -0.006158830626153827259, 7.078243236992583398, 2.121324627965421872 ) ) ;
#61845 = CARTESIAN_POINT ( 'NONE',  ( 0.1055216070770526038, 1.418477292093557329, 1.282857148695019989 ) ) ;
#61846 = CARTESIAN_POINT ( 'NONE',  ( 0.4320049508096295288, 1.131045402950446199, 1.612214446364314213 ) ) ;
#61847 = CARTESIAN_POINT ( 'NONE',  ( 2.683070245604711523, 1.375115853580029635, 1.371619177916082011 ) ) ;
#61848 = CARTESIAN_POINT ( 'NONE',  ( 1.264999722075825561, -2.016288307338756525, -0.002813990012486000669 ) ) ;
#61850 = CARTESIAN_POINT ( 'NONE',  ( 5.365987026107917224, -1.852166562183876986, 0.1801111341232768115 ) ) ;
#61849 = CARTESIAN_POINT ( 'NONE',  ( -5.631432701629818460, 7.663367133358481631, 1.599625672291263179 ) ) ;
#61851 = CARTESIAN_POINT ( 'NONE',  ( 6.235824307642648279, 6.239826211863360506, 0.000000000000000000 ) ) ;
#61852 = CARTESIAN_POINT ( 'NONE',  ( 0.000000000000000000, 4.000007913748540922, 0.000000000000000000 ) ) ;
#61853 = CARTESIAN_POINT ( 'NONE',  ( 1.474248253919626883, 7.378028154546084849, -4.279201940601814691 ) ) ;
#61854 = CARTESIAN_POINT ( 'NONE',  ( -4.042302355168801320, 7.867769847672247074, 0.7998128361456341429 ) ) ;
#61855 = CARTESIAN_POINT ( 'NONE',  ( -7.533490631048818109, 8.818102486758951031, -1.199719254218452047 ) ) ;
#61856 = CARTESIAN_POINT ( 'NONE',  ( 1.224469250947546328, 2.113408192816915943, 0.5798510048089372537 ) ) ;
#61857 = CARTESIAN_POINT ( 'NONE',  ( 4.039966587192259873, 5.736380323189513852, 1.443375672974062551 ) ) ;
#61858 = CIRCLE ( 'NONE', #106903, 4.022469383779238683 ) ;
#61859 = DIRECTION ( 'NONE',  ( 0.000000000000000000, 0.000000000000000000, -1.000000000000000000 ) ) ;
#61861 =( BOUNDED_SURFACE ( )  B_SPLINE_SURFACE ( 3, 2, ( 
 ( #10395, #76470, #60221 ),
 ( #61295, #176128, #142579 ),
 ( #124254, #208586, #126380 ),
 ( #192339, #11465, #27727 ),
 ( #207536, #74351, #42938 ),
 ( #93821, #58093, #12531 ),
 ( #78603, #159862, #127456 ),
 ( #177184, #45071, #9342 ) ),
 .UNSPECIFIED., .F., .F., .F. ) 
 B_SPLINE_SURFACE_WITH_KNOTS ( ( 4, 2, 2, 4 ),
 ( 3, 3 ),
 ( 0.000000000000000000, 0.0005109843281227174992, 0.0007664764921840762487, 0.001021968656245434998 ),
 ( 0.000000000000000000, 1.000000000000000000 ),
 .UNSPECIFIED. ) 
 GEOMETRIC_REPRESENTATION_ITEM ( )  RATIONAL_B_SPLINE_SURFACE ( (
 ( 1.000000000000000000, 0.7045118851637612867, 1.000000000000000000),
 ( 1.000000000000000000, 0.6478559580219772629, 1.000000000000000000),
 ( 1.000000000000000000, 0.5832506164449779984, 1.000000000000000000),
 ( 1.000000000000000000, 0.4879709628488522188, 1.000000000000000000),
 ( 1.000000000000000000, 0.4561823831824661224, 1.000000000000000000),
 ( 1.000000000000000000, 0.4039565156457392558, 1.000000000000000000),
 ( 1.000000000000000000, 0.3848936348729107282, 1.000000000000000000),
 ( 1.000000000000000000, 0.3826834323650832315, 1.000000000000000000) ) ) 
 REPRESENTATION_ITEM ( '' )  SURFACE ( )  );
#61860 = CARTESIAN_POINT ( 'NONE',  ( 2.743825832610055748, 3.021665646862250920, -2.500000000000000444 ) ) ;
#61863 = ADVANCED_FACE ( 'NONE', ( #179680 ), #128762, .T. ) ;
#61862 = CARTESIAN_POINT ( 'NONE',  ( 2.209345402013741300, -0.4006574107652469130, 1.781019818369505847 ) ) ;
#61864 = CARTESIAN_POINT ( 'NONE',  ( -3.066115294984855133, 6.728884944124295053, 0.7998128361456341429 ) ) ;
#61865 = CARTESIAN_POINT ( 'NONE',  ( -5.526470424545159688, 7.552361116859303891, -1.349762019914104272 ) ) ;
#61866 = CARTESIAN_POINT ( 'NONE',  ( 6.608999999999983999, 4.692729314731947099, 2.662616042240486536 ) ) ;
#61867 = CARTESIAN_POINT ( 'NONE',  ( 10.21336978979620191, 10.81001959771741205, 0.7998128361456462443 ) ) ;
#61868 = CARTESIAN_POINT ( 'NONE',  ( 0.8207749864527034145, 1.779613767027238502, 0.7382806748287008558 ) ) ;
#61869 = CARTESIAN_POINT ( 'NONE',  ( 5.418788444413384475, -1.423528547644649755, 1.350099487149841071 ) ) ;
#61870 = CARTESIAN_POINT ( 'NONE',  ( -7.226659571283968297, 8.389856573708110332, 1.199719254218450271 ) ) ;
#61871 = CARTESIAN_POINT ( 'NONE',  ( 4.123651276850781144, 7.962676922967908411, -0.7998128361456221525 ) ) ;
#61872 = CARTESIAN_POINT ( 'NONE',  ( 4.722331747100577459, 2.097238624054961864, 0.6360808509995665716 ) ) ;
#61873 = CARTESIAN_POINT ( 'NONE',  ( 3.876741858503734761, 6.610283703974623393, 1.199719254218462483 ) ) ;
#61874 = CARTESIAN_POINT ( 'NONE',  ( 4.469627305733424372, -0.3590069766891256231, 2.038746214588673666 ) ) ;
#61876 = CARTESIAN_POINT ( 'NONE',  ( 0.6823417656249882723, 0.7385416670080829915, -1.181850606188749264 ) ) ;
#61875 = DIRECTION ( 'NONE',  ( -0.6483454320283799088, 0.000000000000000000, 0.7613463080411786432 ) ) ;
#61877 = VERTEX_POINT ( 'NONE', #47566 ) ;
#61878 = CARTESIAN_POINT ( 'NONE',  ( 4.448018067569548428, -2.052855444095956550, -1.034378808386252624 ) ) ;
#61880 = ORIENTED_EDGE ( 'NONE', *, *, #48997, .F. ) ;
#61879 = CARTESIAN_POINT ( 'NONE',  ( 6.141480397310468575, 10.10888486359680982, 1.040834085586084257E-14 ) ) ;
#61882 = CARTESIAN_POINT ( 'NONE',  ( -5.436456409399874623, 5.444880020495701523, 0.000000000000000000 ) ) ;
#61881 = CARTESIAN_POINT ( 'NONE',  ( 4.556949027968946631, 8.330541276023501140, -0.7216878364870357165 ) ) ;
#61884 = EDGE_CURVE ( 'NONE', #29314, #105686, #39112, .T. ) ;
#61883 = CARTESIAN_POINT ( 'NONE',  ( 6.620655732516649294, 0.5971256128398574337, 1.879834161342401666 ) ) ;
#61885 = B_SPLINE_CURVE_WITH_KNOTS ( 'NONE', 3,
 ( #172632, #110885, #42645, #209357 ),
 .UNSPECIFIED., .F., .F.,
 ( 4, 4 ),
 ( 0.002911097519902588939, 0.003691190409735757919 ),
 .UNSPECIFIED. ) ;
#61886 = CARTESIAN_POINT ( 'NONE',  ( -10.49167095263963034, 5.343775707538782171, -5.730694126968528757 ) ) ;
#61887 = CARTESIAN_POINT ( 'NONE',  ( 3.837779778221518168, 1.932683437559437500, 0.1894486881511766863 ) ) ;
#61888 = EDGE_LOOP ( 'NONE', ( #209065, #212444, #163689, #165072 ) ) ;
#61889 = CARTESIAN_POINT ( 'NONE',  ( 10.52076401408022299, 11.37657222595619189, 0.000000000000000000 ) ) ;
#61890 = EDGE_CURVE ( 'NONE', #116561, #11879, #61249, .T. ) ;
#61891 = ORIENTED_EDGE ( 'NONE', *, *, #173375, .T. ) ;
#61892 = CARTESIAN_POINT ( 'NONE',  ( 5.695548698317931091, 1.764485844685494742, -0.7379451211212140205 ) ) ;
#61893 = DIRECTION ( 'NONE',  ( 0.7592566023653005702, -0.6507913734559639396, 0.000000000000000000 ) ) ;
#61894 = CARTESIAN_POINT ( 'NONE',  ( 6.370102249521607973, 0.8915232854993185851, 1.476320845237573787 ) ) ;
#61895 = CARTESIAN_POINT ( 'NONE',  ( 4.382046175016578005, -2.016188710442788246, -0.04465648322755921829 ) ) ;
#61896 = CARTESIAN_POINT ( 'NONE',  ( -3.332168893502611251, 7.719402352560151392, 2.450693629706233168 ) ) ;
#61897 = CARTESIAN_POINT ( 'NONE',  ( 1.875870136999336246, 2.111227540014638304, -0.6426800678154330759 ) ) ;
#61899 = CARTESIAN_POINT ( 'NONE',  ( -3.011319516011047082, 6.527306845405913549, 0.7216878364870328300 ) ) ;
#61898 = CARTESIAN_POINT ( 'NONE',  ( -10.47775378526269918, 11.11846759242831872, -0.7998128361456221525 ) ) ;
#61901 = CARTESIAN_POINT ( 'NONE',  ( 0.5843626980001519478, -0.2102794380555508547, -1.757238120818458649 ) ) ;
#61900 = CARTESIAN_POINT ( 'NONE',  ( 2.044979492446592939, -1.679722130475280961, -1.244493991799436650 ) ) ;
#61902 = CARTESIAN_POINT ( 'NONE',  ( 6.152970239395502361, 1.038990588714868490, 1.728003889287746286 ) ) ;
#61904 = CARTESIAN_POINT ( 'NONE',  ( 2.642860430951101680, -1.905069302404806875, 1.274549645703947132 ) ) ;
#61903 = CARTESIAN_POINT ( 'NONE',  ( 3.725458348705031231, 7.568394850123006279, -1.734723475976807094E-15 ) ) ;
#61905 = CARTESIAN_POINT ( 'NONE',  ( 1.024908375165583863, -1.101351337790077212, -1.347483777630980040 ) ) ;
#61906 = FACE_OUTER_BOUND ( 'NONE', #57586, .T. ) ;
#61907 = CARTESIAN_POINT ( 'NONE',  ( 1.598581759805017155, 0.8596790983186454183, -1.505624278722474951 ) ) ;
#61908 = CARTESIAN_POINT ( 'NONE',  ( 1.360316468749955598, 0.5260416670081085044, 0.7853790794158820310 ) ) ;
#61909 = CARTESIAN_POINT ( 'NONE',  ( -11.89197816957260478, 13.79999999999999893, -0.8055420615339585755 ) ) ;
#61910 = CARTESIAN_POINT ( 'NONE',  ( 1.399139394074319753, 0.4229888639164773867, 2.129416274499373429 ) ) ;
#61911 = CARTESIAN_POINT ( 'NONE',  ( 2.395720570290179374, -1.993893129684479293, 0.3006499569925198956 ) ) ;
#61912 = CARTESIAN_POINT ( 'NONE',  ( 3.625000000000002665, -2.052068128417946280, 2.068584262981140017E-13 ) ) ;
#61913 =( BOUNDED_SURFACE ( )  B_SPLINE_SURFACE ( 3, 2, ( 
 ( #212345, #96518, #181978 ),
 ( #65029, #49863, #195050 ),
 ( #14139, #61853, #193974 ),
 ( #80232, #146330, #45622 ) ),
 .UNSPECIFIED., .F., .F., .T. ) 
 B_SPLINE_SURFACE_WITH_KNOTS ( ( 4, 4 ),
 ( 3, 3 ),
 ( 0.000000000000000000, 0.0001288481725889855669 ),
 ( 0.000000000000000000, 1.000000000000000000 ),
 .UNSPECIFIED. ) 
 GEOMETRIC_REPRESENTATION_ITEM ( )  RATIONAL_B_SPLINE_SURFACE ( (
 ( 1.000000000000000000, 0.7779734834199504290, 1.000000000000000000),
 ( 1.000000000000000000, 0.8164436902898472015, 1.000000000000000000),
 ( 1.000000000000000000, 0.8496999780352315623, 1.000000000000000000),
 ( 1.000000000000000000, 0.8739472344198672138, 1.000000000000000000) ) ) 
 REPRESENTATION_ITEM ( '' )  SURFACE ( )  );
#61914 = CIRCLE ( 'NONE', #155301, 0.07999999999999998779 ) ;
#61915 = CARTESIAN_POINT ( 'NONE',  ( 1.499999999999989120, 1.556250000682817047, 0.000000000000000000 ) ) ;
#61916 = CARTESIAN_POINT ( 'NONE',  ( 6.182248986134903035, -1.028413017182037370, 1.628868941788450764 ) ) ;
#61917 = CARTESIAN_POINT ( 'NONE',  ( -0.6823417656250003738, 13.65104166700806232, 1.181850606188754593 ) ) ;
#61918 = CARTESIAN_POINT ( 'NONE',  ( 2.900855728284880808, -2.189247779298031826, -0.3757519495388698672 ) ) ;
#61919 = ORIENTED_EDGE ( 'NONE', *, *, #207872, .F. ) ;
#61920 = CARTESIAN_POINT ( 'NONE',  ( 6.588752024304575627, -8.074889850123490476, 6.844216539294094126 ) ) ;
#61921 = DIRECTION ( 'NONE',  ( 5.578564026256490882E-16, 1.000000000000000000, 9.066213480720158442E-32 ) ) ;
#61922 = CARTESIAN_POINT ( 'NONE',  ( 7.564559641420864899, 10.91273778404466199, -1.199719254218446718 ) ) ;
#61923 = DIRECTION ( 'NONE',  ( 1.000000000000000000, -0.000000000000000000, -0.000000000000000000 ) ) ;
#61924 = CARTESIAN_POINT ( 'NONE',  ( 4.968161617874263136, -1.641142972212021656, -0.5799033918824270106 ) ) ;
#61925 = CARTESIAN_POINT ( 'NONE',  ( 4.088298575758734898, 1.051444423028622399, -1.656135347060924135 ) ) ;
#61927 = CARTESIAN_POINT ( 'NONE',  ( -4.758548728716557541, 8.495464583570553785, 1.040834085586084257E-14 ) ) ;
#61926 = CARTESIAN_POINT ( 'NONE',  ( 2.737856954955798727, 5.281584649835344258, 1.199719254218452047 ) ) ;
#61928 = CARTESIAN_POINT ( 'NONE',  ( 5.747730777550676073, 5.670383760089384495, 0.000000000000000000 ) ) ;
#61929 = CARTESIAN_POINT ( 'NONE',  ( 4.991644252507740021, 1.671830779756987573, 1.524457814443666903 ) ) ;
#61930 = AXIS2_PLACEMENT_3D ( 'NONE', #158597, #74145, #58957 ) ;
#61931 = CARTESIAN_POINT ( 'NONE',  ( 1.908709741418318062, 0.6448079515158434694, 1.959386160279535494 ) ) ;
#61932 = CARTESIAN_POINT ( 'NONE',  ( -5.856232286098998152, 8.919689202835742847, 1.199719254218452047 ) ) ;
#61933 = VERTEX_POINT ( 'NONE', #196981 ) ;
#61934 = CARTESIAN_POINT ( 'NONE',  ( 0.7499999999999885647, 1.097916667349485564, -1.299038105676652899 ) ) ;
#61935 = CARTESIAN_POINT ( 'NONE',  ( 3.128041797164154758, 1.042111378005972311, -1.553157497896196393 ) ) ;
#61936 = CARTESIAN_POINT ( 'NONE',  ( 2.637049607583162203, 0.5866705090989009497, 1.632017879250416525 ) ) ;
#61937 = CARTESIAN_POINT ( 'NONE',  ( 0.06458782335966220534, -1.490751515076127465, 1.741559778653593238 ) ) ;
#61938 = CARTESIAN_POINT ( 'NONE',  ( 0.1654306582001447423, -1.972458130798220077, -0.9897840116655574061 ) ) ;
#61939 = CARTESIAN_POINT ( 'NONE',  ( 3.467792127863758456, 2.109446376165153847, -0.4717452660116944196 ) ) ;
#61940 = CARTESIAN_POINT ( 'NONE',  ( 4.681548850490841573, -0.9142078566968904196, 1.713296222823880166 ) ) ;
#61941 = CARTESIAN_POINT ( 'NONE',  ( -4.731432421044888592, 4.622352034081546712, -0.7216878364870207285 ) ) ;
#61942 = CARTESIAN_POINT ( 'NONE',  ( 6.731728662460410462, -1.222180481402233898, -1.416172877279207931 ) ) ;
#61943 = CARTESIAN_POINT ( 'NONE',  ( 4.196871964084724738, 7.339766560697110975, 0.8424661700066529146 ) ) ;
#61944 = CARTESIAN_POINT ( 'NONE',  ( 0.5773502691896192918, -4.295408888568413630, 1.000000000000004441 ) ) ;
#61945 = CARTESIAN_POINT ( 'NONE',  ( 0.03560581989598374242, -0.09759080014098624190, 2.118463022953632091 ) ) ;
#61946 = CARTESIAN_POINT ( 'NONE',  ( -4.957638175832625493E-14, 2.078125000341435769, -1.570758158831802254 ) ) ;
#61947 = CARTESIAN_POINT ( 'NONE',  ( 5.449842333688053486, -1.824117940560719298, -0.8596331684956670660 ) ) ;
#61948 = CARTESIAN_POINT ( 'NONE',  ( -9.667127221743832877, 11.23706883257798772, 1.199719254218462483 ) ) ;
#61949 = CARTESIAN_POINT ( 'NONE',  ( 8.782984583554449998, 9.141236857102018831, 1.040834085586084257E-14 ) ) ;
#61950 = CARTESIAN_POINT ( 'NONE',  ( 2.642331537210453440, -0.3998488639457564719, -0.1525862845480549512 ) ) ;
#61951 = CARTESIAN_POINT ( 'NONE',  ( 3.017977635683791071, -0.9002817137206723386, -1.588204215665294461 ) ) ;
#61952 = CARTESIAN_POINT ( 'NONE',  ( 2.520803682403276902, 1.441976459853638204, -1.670562425240495363 ) ) ;
#61953 = ORIENTED_EDGE ( 'NONE', *, *, #89270, .T. ) ;
#61954 = CARTESIAN_POINT ( 'NONE',  ( -5.939880696118548187, 6.102484698325975288, 0.000000000000000000 ) ) ;
#61955 = UNCERTAINTY_MEASURE_WITH_UNIT (LENGTH_MEASURE( 1.000000000000000082E-05 ), #41497, 'distance_accuracy_value', 'NONE');
#61956 = CARTESIAN_POINT ( 'NONE',  ( -3.285556943749998737, -3.667708332855377673, 1.896917185911908499 ) ) ;
#61957 = CARTESIAN_POINT ( 'NONE',  ( -8.128276786592724790, 9.441743324901704426, -1.199719254218446718 ) ) ;
#61958 = CARTESIAN_POINT ( 'NONE',  ( 0.5100284451979911760, -0.7230318888242005526, 1.886137889315203875 ) ) ;
#61959 = CARTESIAN_POINT ( 'NONE',  ( 0.7332529803791461021, 1.960763319057107879, 0.8078710241638600298 ) ) ;
#61960 = ORIENTED_EDGE ( 'NONE', *, *, #91370, .F. ) ;
#61961 = CARTESIAN_POINT ( 'NONE',  ( -4.437261413422502798, 8.398831758960053406, 0.000000000000000000 ) ) ;
#61962 = CARTESIAN_POINT ( 'NONE',  ( 1.516205985490867381, 0.7479433349990645130, 1.704208623783896259 ) ) ;
#61963 = CARTESIAN_POINT ( 'NONE',  ( 3.246287715468270108, 5.874753870433235825, 1.199719254218450271 ) ) ;
#61964 = CIRCLE ( 'NONE', #134650, 11.09999999999999964 ) ;
#61965 = CARTESIAN_POINT ( 'NONE',  ( 5.946181061342999286, 2.058424064105804696, 0.1035008386942332104 ) ) ;
#61966 = CARTESIAN_POINT ( 'NONE',  ( 6.258435431136967431, 1.928752767684217106, -0.5880170417187426946 ) ) ;
#61967 = ORIENTED_EDGE ( 'NONE', *, *, #170552, .T. ) ;
#61968 = ORIENTED_EDGE ( 'NONE', *, *, #64072, .F. ) ;
#61969 = ORIENTED_EDGE ( 'NONE', *, *, #98928, .F. ) ;
#61970 = CARTESIAN_POINT ( 'NONE',  ( -9.110189153378817295, 12.71597221466224603, 1.199719254218462483 ) ) ;
#61971 = CARTESIAN_POINT ( 'NONE',  ( 3.457459740917231628, 0.4424662778084071935, -1.771134634090239190 ) ) ;
#61974 = ORIENTED_EDGE ( 'NONE', *, *, #88712, .F. ) ;
#61973 = CARTESIAN_POINT ( 'NONE',  ( -5.562564655730993124, 6.373022183664215135, -1.235959600235781330 ) ) ;
#61972 = CARTESIAN_POINT ( 'NONE',  ( -5.492988512192097161, 6.437516681426083132, 1.199719254218452935 ) ) ;
#61975 = CARTESIAN_POINT ( 'NONE',  ( 5.307274686206796765, 7.744096871513173497, 1.304404211447189876 ) ) ;
#61976 = CARTESIAN_POINT ( 'NONE',  ( 5.940779784064256219, 1.198679029392090589, 1.620932600025201786 ) ) ;
#61977 = CARTESIAN_POINT ( 'NONE',  ( 5.683513393433289096, -0.8240744568873883402, 1.646495476055845231 ) ) ;
#61978 = CARTESIAN_POINT ( 'NONE',  ( 0.07680821025391608436, 0.2560392329899116026, -1.846278364303982178 ) ) ;
#61979 = CARTESIAN_POINT ( 'NONE',  ( 4.073124928733475869, -2.152535440544633971, -0.8323431910086924734 ) ) ;
#61980 = CARTESIAN_POINT ( 'NONE',  ( 5.529746549527311039, 7.544733289238903851, -1.599625672291281386 ) ) ;
#61981 = CARTESIAN_POINT ( 'NONE',  ( 6.362596528949501895, -1.533591692085239266, 1.523617273982772247 ) ) ;
#61982 = CARTESIAN_POINT ( 'NONE',  ( 5.282873410819217241, 9.315102745931094219, -0.7998128361456281477 ) ) ;
#61983 = CARTESIAN_POINT ( 'NONE',  ( 1.505311199525250831, -1.927169978453403321, 0.2396651170105366657 ) ) ;
#61984 = VERTEX_POINT ( 'NONE', #212147 ) ;
#61985 = CIRCLE ( 'NONE', #189835, 6.961139734775127152 ) ;
#61986 = CARTESIAN_POINT ( 'NONE',  ( 5.079617024973425821, 1.589842341716392493, -1.660015637060639371 ) ) ;
#61987 = DIRECTION ( 'NONE',  ( -5.551115123125765446E-17, 0.000000000000000000, 1.000000000000000000 ) ) ;
#61988 = CARTESIAN_POINT ( 'NONE',  ( -4.085803189671902480, 5.860132702740892263, -1.599625672291271394 ) ) ;
#61989 = CARTESIAN_POINT ( 'NONE',  ( 4.451927283622527654, 1.870250842541102410, -0.04591718433973044494 ) ) ;
#61990 = ORIENTED_EDGE ( 'NONE', *, *, #168278, .F. ) ;
#61993 = CARTESIAN_POINT ( 'NONE',  ( -4.936050443827081580, 7.916420063510339666, 1.199719254218452935 ) ) ;
#61992 = CARTESIAN_POINT ( 'NONE',  ( -1.500000000000013101, 0.7020833340161545255, 0.8660254037844403729 ) ) ;
#61991 = CARTESIAN_POINT ( 'NONE',  ( 2.935702856749936362, -1.841876368404654629, 0.5141854427313449216 ) ) ;
#61994 = CARTESIAN_POINT ( 'NONE',  ( 3.563272299071856164, -1.946135509614330239, -1.040604674307284316 ) ) ;
#61995 = CARTESIAN_POINT ( 'NONE',  ( 6.883263157960393563, 1.268976584491373183, 2.060807272249213451 ) ) ;
#61996 = CARTESIAN_POINT ( 'NONE',  ( 4.376584659113025744, 4.000436945253625254, 0.7998128361456341429 ) ) ;
#61997 = CARTESIAN_POINT ( 'NONE',  ( 6.834718834620487016, 7.146462526578263308, 0.000000000000000000 ) ) ;
#61998 = CARTESIAN_POINT ( 'NONE',  ( -8.109748439268576803, 12.61312361245537517, 0.7998128361456481317 ) ) ;
#61999 = CARTESIAN_POINT ( 'NONE',  ( -5.112833325684904118, 8.979072956692109031, -0.7216878364870338292 ) ) ;
#62000 = CARTESIAN_POINT ( 'NONE',  ( 1.686731049638652502, -0.2853660037422758866, -1.950466449893713428 ) ) ;
#62001 = CARTESIAN_POINT ( 'NONE',  ( 1.483892314354786857, 2.131289638308156320, -0.8850757863276045301 ) ) ;
#62002 = CARTESIAN_POINT ( 'NONE',  ( 2.383191274269541360, -0.003000794896521400724, 1.962046632024143866 ) ) ;
#62003 = DIRECTION ( 'NONE',  ( 0.9782075119096202975, 0.1245777785630026030, 0.1661037047506698505 ) ) ;
#62004 = CARTESIAN_POINT ( 'NONE',  ( 4.821169966264648998, -1.840000718094082943, -0.9321929973984711681 ) ) ;
#62005 = CARTESIAN_POINT ( 'NONE',  ( 4.284013352238246419, 6.021101549076499637, -1.443375672974051449 ) ) ;
#62006 = CARTESIAN_POINT ( 'NONE',  ( 5.879395890181562834, 6.888325289080478697, -1.199719254218452047 ) ) ;
#62007 = ORIENTED_EDGE ( 'NONE', *, *, #63875, .T. ) ;
#62008 = CARTESIAN_POINT ( 'NONE',  ( -4.903732577545095950, 4.837283930932079201, 0.1501914610188368471 ) ) ;
#62009 = CARTESIAN_POINT ( 'NONE',  ( -11.55950211276791428, 13.87999999999998302, 3.221476510067114329 ) ) ;
#62010 = CARTESIAN_POINT ( 'NONE',  ( 4.175548122884573665, 3.973820352894515295, 1.214306433183764966E-14 ) ) ;
#62011 = CARTESIAN_POINT ( 'NONE',  ( 0.8312205373445592516, -2.043673001365586384, -0.7330250775806450569 ) ) ;
#62012 = CARTESIAN_POINT ( 'NONE',  ( 0.000000000000000000, 5.999999999999998224, 0.000000000000000000 ) ) ;
#62013 = CARTESIAN_POINT ( 'NONE',  ( 4.318600669050584706, 4.999583595936801572, 2.419999999999999485 ) ) ;
#62014 = DIRECTION ( 'NONE',  ( 0.9989735196462988798, 0.000000000000000000, -0.04529798058948708572 ) ) ;
#62015 = CARTESIAN_POINT ( 'NONE',  ( 2.600682448077856090, 1.504852936121018558, -1.110837741034584436 ) ) ;
#62016 = CIRCLE ( 'NONE', #3215, 4.000000000000000000 ) ;
#62017 = CARTESIAN_POINT ( 'NONE',  ( 6.731704548537910782, -1.406307105171537009, -1.641701734229366716 ) ) ;
#62018 = ADVANCED_FACE ( 'NONE', ( #48621 ), #170268, .F. ) ;
#62020 = SURFACE_SIDE_STYLE ('',( #194136 ) ) ;
#62019 = CARTESIAN_POINT ( 'NONE',  ( 0.07755575628181145265, 0.2276780653837663093, -2.222404768597834757 ) ) ;
#62021 = CARTESIAN_POINT ( 'NONE',  ( 0.6823417656249882723, -0.4072916663252490466, 1.181850606188755259 ) ) ;
#62022 = CARTESIAN_POINT ( 'NONE',  ( 2.051281676579026492, -1.707476168062868060, 0.8611843332394365502 ) ) ;
#62023 = CARTESIAN_POINT ( 'NONE',  ( 4.311239457809501907, -0.3017279273445966914, 1.743759454612598070 ) ) ;
#62024 = CARTESIAN_POINT ( 'NONE',  ( 2.297387027313551044, 1.747684631587187454, -0.7765785915121098393 ) ) ;
#62025 = CARTESIAN_POINT ( 'NONE',  ( -5.473741331615264549, 7.409117525016355010, -1.599625672291256295 ) ) ;
#62027 = CARTESIAN_POINT ( 'NONE',  ( 6.046487378053778450, -1.350936885689631772, 1.358403761460762471 ) ) ;
#62026 =( NAMED_UNIT ( * ) PLANE_ANGLE_UNIT ( ) SI_UNIT ( $, .RADIAN. ) );
#62028 = AXIS2_PLACEMENT_3D ( 'NONE', #84477, #53038, #151630 ) ;
#62029 = CARTESIAN_POINT ( 'NONE',  ( 1.499999999999985123, 0.04583333333335545129, -0.8660254037844323793 ) ) ;
#62030 = CARTESIAN_POINT ( 'NONE',  ( 6.584429662329396749, 1.135205087083859476, -1.609268749140836618 ) ) ;
#62031 = CARTESIAN_POINT ( 'NONE',  ( 1.499999999999989120, 5.295833333333356485, -0.8660254037844323793 ) ) ;
#62032 = ADVANCED_FACE ( 'NONE', ( #11824 ), #163433, .T. ) ;
#62033 = CARTESIAN_POINT ( 'NONE',  ( 3.147653791585803162, 8.919999999999939533, -2.500000000000000444 ) ) ;
#62034 = CARTESIAN_POINT ( 'NONE',  ( 5.313307075269409374, -0.2735208697075517947, 1.850433306854900817 ) ) ;
#62036 = VERTEX_POINT ( 'NONE', #98424 ) ;
#62035 = CARTESIAN_POINT ( 'NONE',  ( 2.086296903703276140, -1.790263230197926436, -0.3570169370194844483 ) ) ;
#62038 = CARTESIAN_POINT ( 'NONE',  ( 5.054560120293923653, 7.862967615930308796, 1.113740650586869219 ) ) ;
#62037 = CARTESIAN_POINT ( 'NONE',  ( 4.987059637548557411, -0.2676712469649074055, -2.190530366034774801 ) ) ;
#62039 = AXIS2_PLACEMENT_3D ( 'NONE', #176425, #46427, #125622 ) ;
#62040 = CARTESIAN_POINT ( 'NONE',  ( -1.364683531250000748, -1.240624999658580752, 0.000000000000000000 ) ) ;
#62041 = CARTESIAN_POINT ( 'NONE',  ( 2.805193546069509214, -1.716336894061726737, 1.143758443631032407 ) ) ;
#62042 = EDGE_CURVE ( 'NONE', #122458, #47720, #61560, .T. ) ;
#62043 = CARTESIAN_POINT ( 'NONE',  ( -9.027031348600448979, 9.425958082989001952, 1.040834085586084257E-14 ) ) ;
#62044 =( NAMED_UNIT ( * ) PLANE_ANGLE_UNIT ( ) SI_UNIT ( $, .RADIAN. ) );
#62045 = CARTESIAN_POINT ( 'NONE',  ( 1.436299488671524571, 3.619978527027484905, 0.4486666144298699366 ) ) ;
#62046 = CARTESIAN_POINT ( 'NONE',  ( 5.671053392266061977, 9.838255734277600695, 0.7998128361456331437 ) ) ;
#62047 = ORIENTED_EDGE ( 'NONE', *, *, #146436, .T. ) ;
#62048 = CARTESIAN_POINT ( 'NONE',  ( 5.564915762860970894, 1.570151797963925455, -1.349580972669261580 ) ) ;
#62049 = CARTESIAN_POINT ( 'NONE',  ( -0.6823417656250246877, -1.136458332991911790, 1.181850606188755259 ) ) ;
#62050 = CARTESIAN_POINT ( 'NONE',  ( 3.181113218772323226, -0.1555236193923059951, -2.156033859764289407 ) ) ;
#62051 = CARTESIAN_POINT ( 'NONE',  ( -4.712247760717829692, 8.249883430950177399, 0.6303846594760522670 ) ) ;
#62052 = CARTESIAN_POINT ( 'NONE',  ( 3.158857784513937617, 0.4929582698031101939, 1.958447305144744410 ) ) ;
#62053 = CARTESIAN_POINT ( 'NONE',  ( 6.620655732516652847, 0.5779860733656561056, 2.127054332187257923 ) ) ;
#62054 = ORIENTED_EDGE ( 'NONE', *, *, #56512, .T. ) ;
#62055 = ORIENTED_EDGE ( 'NONE', *, *, #23354, .T. ) ;
#62057 = CARTESIAN_POINT ( 'NONE',  ( 6.588899466561449536, 9.670504563421618016, -1.082531754730537088 ) ) ;
#62056 = CARTESIAN_POINT ( 'NONE',  ( 3.475000000000000533, -0.8458333333333335480, -2.006292185433951047 ) ) ;
#62058 = CARTESIAN_POINT ( 'NONE',  ( -3.146901051703345331, 6.685485303713597283, 0.000000000000000000 ) ) ;
#62059 = CARTESIAN_POINT ( 'NONE',  ( 1.516814941429758701, 0.2024661778830244008, 2.006371303556075958 ) ) ;
#62060 = CARTESIAN_POINT ( 'NONE',  ( 6.532779862045914321, -1.958661757936002612, 0.9833580883553474372 ) ) ;
#62061 = CARTESIAN_POINT ( 'NONE',  ( -1.499999999999997780, 4.181250000682819490, 1.214306433183764966E-14 ) ) ;
#62062 = CARTESIAN_POINT ( 'NONE',  ( 5.168181644781757456, 1.909928461159452251, -0.09994665148223277895 ) ) ;
#62063 = CARTESIAN_POINT ( 'NONE',  ( -2.767835915484202047, 6.380892334706859792, -0.7998128361456281477 ) ) ;
#62064 = CARTESIAN_POINT ( 'NONE',  ( 4.961921032477176752, 8.732732271291288484, 1.040834085586084257E-14 ) ) ;
#62066 = CARTESIAN_POINT ( 'NONE',  ( 2.847279977023515318, 0.2930488483154705670, -1.994874153863256172 ) ) ;
#62065 = CARTESIAN_POINT ( 'NONE',  ( -8.283668667825340393, 12.60810451253083997, 0.7216878364870458196 ) ) ;
#62067 = CARTESIAN_POINT ( 'NONE',  ( -0.6823417656250003738, 13.21354166700806942, 1.181850606188754593 ) ) ;
#62068 = CARTESIAN_POINT ( 'NONE',  ( -5.327428015527048366, 5.180030537728460338, -0.7998128361456362523 ) ) ;
#62069 = CARTESIAN_POINT ( 'NONE',  ( 5.614166379062860202, -0.7790257685919326214, -1.538869111107727505 ) ) ;
#62070 = CARTESIAN_POINT ( 'NONE',  ( 6.003228155800906407, 10.22579295840155744, 0.000000000000000000 ) ) ;
#62071 = CARTESIAN_POINT ( 'NONE',  ( 3.440018289565364817, 5.036440642624797626, 1.599625672291267398 ) ) ;
#62072 = LINE ( 'NONE', #13308, #202886 ) ;
#62073 = CARTESIAN_POINT ( 'NONE',  ( 1.006788857090525013, 0.5974033793386055446, 1.982218910981221827 ) ) ;
#62074 = LINE ( 'NONE', #10104, #126241 ) ;
#62075 = ORIENTED_EDGE ( 'NONE', *, *, #191014, .F. ) ;
#62076 = CARTESIAN_POINT ( 'NONE',  ( 5.162699569786796339, 0.5314807639728249544, 1.731738579618222973 ) ) ;
#62077 = CARTESIAN_POINT ( 'NONE',  ( 5.499767588998890844, 6.445425604367387429, 1.199719254218451159 ) ) ;
#62078 = CYLINDRICAL_SURFACE ( 'NONE', #146576, 0.07999999999999993228 ) ;
#62079 = CARTESIAN_POINT ( 'NONE',  ( 6.006502151196043471, -1.803439199047681907, -0.1703578026433834602 ) ) ;
#62080 = CARTESIAN_POINT ( 'NONE',  ( 5.139949632912227173, 8.050339434155988627, -1.082531754730548412 ) ) ;
#62081 = CARTESIAN_POINT ( 'NONE',  ( 3.556733441538503016, -1.932615445784117369, -1.033156731641969195 ) ) ;
#62082 = ORIENTED_EDGE ( 'NONE', *, *, #41738, .F. ) ;
#62084 = CARTESIAN_POINT ( 'NONE',  ( 7.404724451357931336, 11.79059562655963056, 0.7998128361456462443 ) ) ;
#62083 = CARTESIAN_POINT ( 'NONE',  ( 0.2737812321212430566, -1.924752420120953822, 0.3788971555385572954 ) ) ;
#62085 = CARTESIAN_POINT ( 'NONE',  ( 4.921452907191903314, -1.357786409588169096, -1.351554235494869749 ) ) ;
#62086 = DIRECTION ( 'NONE',  ( -0.6507913734559641616, -0.7592566023653004592, 0.000000000000000000 ) ) ;
#62087 = CARTESIAN_POINT ( 'NONE',  ( -6.344338864096334518, 6.859745832460597548, 0.6559349933493059392 ) ) ;
#62088 =( NAMED_UNIT ( * ) PLANE_ANGLE_UNIT ( ) SI_UNIT ( $, .RADIAN. ) );
#62089 = CARTESIAN_POINT ( 'NONE',  ( -1.402160292154681736E-14, 0.1968750003414221628, -1.575800808251665908 ) ) ;
#62091 = ORIENTED_EDGE ( 'NONE', *, *, #13231, .T. ) ;
#62090 = CARTESIAN_POINT ( 'NONE',  ( 4.853455804012216213, 6.685451076146141425, 1.443375672974062551 ) ) ;
#62092 = CARTESIAN_POINT ( 'NONE',  ( -8.026063749610047537, 11.34719622697832264, -1.082531754730543971 ) ) ;
#62093 = CARTESIAN_POINT ( 'NONE',  ( 1.639762333045853726, -1.565812861550972324, -1.490595759849027813 ) ) ;
#62094 = CARTESIAN_POINT ( 'NONE',  ( -4.472210567661380587, 6.310941310395290493, 1.599625672291270506 ) ) ;
#62095 = CARTESIAN_POINT ( 'NONE',  ( 5.011674058906918638, 5.875983152593414971, 1.199719254218452047 ) ) ;
#62096 = CARTESIAN_POINT ( 'NONE',  ( 1.535882326342351334, 0.9031702520058831896, -1.586444745400449108 ) ) ;
#62097 = CARTESIAN_POINT ( 'NONE',  ( -2.279742385392243165, 5.811449882932888222, -0.7998128361456281477 ) ) ;
#62098 = CARTESIAN_POINT ( 'NONE',  ( 4.963791182761823961, 1.805510465697376610, -0.2690417022049585438 ) ) ;
#62099 = EDGE_CURVE ( 'NONE', #85030, #84121, #198505, .T. ) ;
#62100 = CARTESIAN_POINT ( 'NONE',  ( 9.639237905258834616, 11.95699723271644466, -8.657004797785544881 ) ) ;
#62101 = CARTESIAN_POINT ( 'NONE',  ( 2.847809051801777791, -1.287500320553297994, -1.414207669007704116 ) ) ;
#62102 = ORIENTED_EDGE ( 'NONE', *, *, #191462, .T. ) ;
#62103 = CARTESIAN_POINT ( 'NONE',  ( 3.508217419976053630, 1.969739563948954331, 0.002549893942540777322 ) ) ;
#62104 = ORIENTED_EDGE ( 'NONE', *, *, #136759, .F. ) ;
#62105 = CARTESIAN_POINT ( 'NONE',  ( 6.146037779257278011, 0.6132840560482490933, 1.842739892034722882 ) ) ;
#62106 = VERTEX_POINT ( 'NONE', #202009 ) ;
#62107 = CARTESIAN_POINT ( 'NONE',  ( -7.273023059088104425, 7.449891421883056530, 0.000000000000000000 ) ) ;
#62109 = CARTESIAN_POINT ( 'NONE',  ( 5.625269520628737752, 1.871107552910089122, 0.9978724776121964402 ) ) ;
#62108 = CARTESIAN_POINT ( 'NONE',  ( 4.844006021832467646, 8.873367135438366304, 0.000000000000000000 ) ) ;
#62110 = CARTESIAN_POINT ( 'NONE',  ( 6.495764994278797388, 8.671754808115688107, 1.443375672974063439 ) ) ;
#62112 = VERTEX_POINT ( 'NONE', #73098 ) ;
#62111 = CARTESIAN_POINT ( 'NONE',  ( 4.195896582043898704, 1.251535281948525036, 1.445917311372606262 ) ) ;
#62113 = CARTESIAN_POINT ( 'NONE',  ( 4.612443543746578278, 7.139628114692022187, -1.342220757880496995 ) ) ;
#62114 = CARTESIAN_POINT ( 'NONE',  ( -9.586610838029429260, -7.161464053357567749, 0.003376046620574604893 ) ) ;
#62115 = CARTESIAN_POINT ( 'NONE',  ( 0.2357703454196959370, -2.016519153289020760, 0.8967723332334791575 ) ) ;
#62116 = CARTESIAN_POINT ( 'NONE',  ( 4.916656812733911863, -0.6802563888389367985, -1.894789199515679146 ) ) ;
#62117 = DIRECTION ( 'NONE',  ( -1.000000000000000000, 5.578564026256504688E-16, 0.000000000000000000 ) ) ;
#62118 = CARTESIAN_POINT ( 'NONE',  ( 6.041596546049881944, -1.325759876995153075, -1.255439798616593716 ) ) ;
#62119 = CARTESIAN_POINT ( 'NONE',  ( 0.3267351109269464593, -1.353470794461093751, 1.566751113397255590 ) ) ;
#62120 = CARTESIAN_POINT ( 'NONE',  ( -7.863365906246068349, 9.236643647784308797, -1.082531754730543971 ) ) ;
#62121 = CARTESIAN_POINT ( 'NONE',  ( -5.206707715320216145, 7.734635641480951840, -1.194516140545264227 ) ) ;
#62122 = DIRECTION ( 'NONE',  ( -0.6507913734559640506, -0.7592566023653003482, 0.000000000000000000 ) ) ;
#62123 = CARTESIAN_POINT ( 'NONE',  ( 6.561405567229332547, 0.3174558530528898692, -1.843364171016811603 ) ) ;
#62124 = CARTESIAN_POINT ( 'NONE',  ( 7.935599982700328958, 8.152621489438862667, 0.7998128361456481317 ) ) ;
#62125 = CARTESIAN_POINT ( 'NONE',  ( -3.113568832632681360, 6.784247404713426910, -0.7998128361456282587 ) ) ;
#62126 = CARTESIAN_POINT ( 'NONE',  ( 1.364683531250000303, 11.56770833367472839, -0.7879004041258355073 ) ) ;
#62127 = CARTESIAN_POINT ( 'NONE',  ( -3.601662362724658895, 7.353689856487406473, -0.7998128361456281477 ) ) ;
#62129 = CARTESIAN_POINT ( 'NONE',  ( -2.984203208339354152, 6.495671153122273722, 0.000000000000000000 ) ) ;
#62128 = DIRECTION ( 'NONE',  ( -6.314299915563594049E-62, -8.546850786086437571E-32, -1.000000000000000000 ) ) ;
#62130 = AXIS2_PLACEMENT_3D ( 'NONE', #33804, #199486, #68418 ) ;
#62131 = CARTESIAN_POINT ( 'NONE',  ( 4.183993884235046146, 1.395953275470160682, 1.028640563475995640 ) ) ;
#62132 = CARTESIAN_POINT ( 'NONE',  ( -6.078132937628113908, 5.985576603521232109, 1.040834085586084257E-14 ) ) ;
#62133 = CARTESIAN_POINT ( 'NONE',  ( 1.868117093089691760, -2.055091939184821026, 0.2493290443424806546 ) ) ;
#62134 = CARTESIAN_POINT ( 'NONE',  ( 2.038805038046047624, -1.634495437704911458, 1.345740563223641217 ) ) ;
#62135 = CARTESIAN_POINT ( 'NONE',  ( 3.655894977179307226, 7.416961240017848844, -0.7998128361456291469 ) ) ;
#62136 = CARTESIAN_POINT ( 'NONE',  ( 7.832860060393120882, 10.16142270859057462, 1.599625672291281386 ) ) ;
#62137 = DIRECTION ( 'NONE',  ( -2.168462536859579677E-14, -1.000000000000000000, -9.418999208338882750E-28 ) ) ;
#62138 = CARTESIAN_POINT ( 'NONE',  ( 0.6374758831957715310, 1.839649526063956042, -0.7036667969960698210 ) ) ;
#62139 = CARTESIAN_POINT ( 'NONE',  ( 4.666586266758273815, 7.089143983547513628, 1.366926838653566012 ) ) ;
#62140 = CARTESIAN_POINT ( 'NONE',  ( 4.934804725694211136, 6.780358151441803649, -1.443375672974051449 ) ) ;
#62142 = DIRECTION ( 'NONE',  ( 0.000000000000000000, 0.000000000000000000, 1.000000000000000000 ) ) ;
#62141 = CARTESIAN_POINT ( 'NONE',  ( 3.475000000000000533, -1.954166666666666163, 2.006292185433948827 ) ) ;
#62143 = CARTESIAN_POINT ( 'NONE',  ( 2.045279198001882737, -1.842668879747776156, -1.363283251902024817 ) ) ;
#62145 = EDGE_CURVE ( 'NONE', #146253, #107037, #208293, .T. ) ;
#62144 = CARTESIAN_POINT ( 'NONE',  ( 1.154616158753757338, -1.440623569337009968, 1.121372061650728558 ) ) ;
#62146 = CARTESIAN_POINT ( 'NONE',  ( 3.304848191199673213, -0.3775801424153284458, -1.874573493127674961 ) ) ;
#62147 = CARTESIAN_POINT ( 'NONE',  ( 5.342795052237045539, 8.390955439988655229, -1.199719254218450271 ) ) ;
#62148 = CARTESIAN_POINT ( 'NONE',  ( 7.632877294369377452, 8.967740267261513409, -1.082531754730537976 ) ) ;
#62149 = CARTESIAN_POINT ( 'NONE',  ( -6.970863535720637216, 11.28442455831609337, 0.7998128361456481317 ) ) ;
#62150 = CARTESIAN_POINT ( 'NONE',  ( 1.547136693356679249, 0.2016598947911317496, 2.003107868921078616 ) ) ;
#62151 = CARTESIAN_POINT ( 'NONE',  ( 2.430452978529148655, -1.210835280720125917, 1.543375930141199115 ) ) ;
#62152 = CARTESIAN_POINT ( 'NONE',  ( -9.671043645249580933, 10.17730576241299900, 0.7998128361456462443 ) ) ;
#62153 = CARTESIAN_POINT ( 'NONE',  ( -7.985916173649233230, 9.275655943134292869, -1.199719254218446718 ) ) ;
#62155 = EDGE_CURVE ( 'NONE', #18633, #169050, #83369, .T. ) ;
#62154 = CARTESIAN_POINT ( 'NONE',  ( 0.000000000000000000, 0.08000000000000020983, 11.92000000000000171 ) ) ;
#62157 = CARTESIAN_POINT ( 'NONE',  ( 3.748697311245871688, -1.446992627045262214, 1.018796548582428185 ) ) ;
#62156 = CARTESIAN_POINT ( 'NONE',  ( 5.367163668781920194, 2.014996964747676422, -0.5569773519958736152 ) ) ;
#62158 = CARTESIAN_POINT ( 'NONE',  ( -1.878313713278110919, 15.99999999999692335, 12.68000002627077905 ) ) ;
#62160 = CARTESIAN_POINT ( 'NONE',  ( 6.720655732516684466, -0.007268404184076341853, 2.273772995263834140 ) ) ;
#62159 = CARTESIAN_POINT ( 'NONE',  ( 0.000000000000000000, 0.08000000000000020983, 0.000000000000000000 ) ) ;
#62161 = CARTESIAN_POINT ( 'NONE',  ( 4.593551391122507432, -1.740074876368927104, -0.03866795590094784102 ) ) ;
#62162 = CARTESIAN_POINT ( 'NONE',  ( 7.865701674222579598, 12.32840238656838139, -0.7998128361456352531 ) ) ;
#62163 = CARTESIAN_POINT ( 'NONE',  ( -1.499999999999997780, 4.150000000000021672, 1.214306433183764966E-14 ) ) ;
#62164 = CARTESIAN_POINT ( 'NONE',  ( 4.077271355118361029, 1.226738060269889408, -1.225556752838660168 ) ) ;
#62165 = CARTESIAN_POINT ( 'NONE',  ( 5.072805357664615045, 1.500764584350265718, -1.569201701505947844 ) ) ;
#62166 = CARTESIAN_POINT ( 'NONE',  ( 3.816783937446950770, 4.411668334231586996, 1.199719254218464037 ) ) ;
#62167 = CARTESIAN_POINT ( 'NONE',  ( -0.1529269513586241080, -1.894431756695889923, -0.9458152384202949126 ) ) ;
#62168 = CARTESIAN_POINT ( 'NONE',  ( 5.250000000000002665, 2.988487650205320908E-13, 2.052068128417942283 ) ) ;
#62169 = CARTESIAN_POINT ( 'NONE',  ( -3.360966176420824070, 6.372552851524760698, 0.8599059493307342761 ) ) ;
#62170 = CARTESIAN_POINT ( 'NONE',  ( 3.504829168241951898, 1.519505285488613744, -1.184012928881588822 ) ) ;
#62171 = CARTESIAN_POINT ( 'NONE',  ( -1.402160292154681736E-14, 10.34375000068279782, 1.732050807568881190 ) ) ;
#62172 = CARTESIAN_POINT ( 'NONE',  ( 6.398696371038459674, -2.178289998122169280, -0.4347530419120289036 ) ) ;
#62173 = ORIENTED_EDGE ( 'NONE', *, *, #79643, .T. ) ;
#62174 = CARTESIAN_POINT ( 'NONE',  ( 6.983263157960371004, 2.969675876345272858, 2.399270433241917466 ) ) ;
#62175 = CARTESIAN_POINT ( 'NONE',  ( -0.7499999999999972244, 3.108333333333358706, -1.299038105676652011 ) ) ;
#62176 = CARTESIAN_POINT ( 'NONE',  ( 4.690231075323689325, 7.559354456931247412, 1.199719254218462483 ) ) ;
#62177 = CARTESIAN_POINT ( 'NONE',  ( 2.174768466102798836, 0.9529365794415098900, 2.006655600372597714 ) ) ;
#62179 =( NAMED_UNIT ( * ) SI_UNIT ( $, .STERADIAN. ) SOLID_ANGLE_UNIT ( ) );
#62178 = CIRCLE ( 'NONE', #110643, 0.08000000000000001554 ) ;
#62180 = CARTESIAN_POINT ( 'NONE',  ( 6.792271770766432404, 10.86814146596211472, 1.040834085586084257E-14 ) ) ;
#62181 = CARTESIAN_POINT ( 'NONE',  ( -9.449669878600616357, 12.04770082983265844, -1.443375672974058777 ) ) ;
#62182 = EDGE_CURVE ( 'NONE', #54188, #182367, #154375, .T. ) ;
#62183 = CARTESIAN_POINT ( 'NONE',  ( 7.404161286838808920, 8.771181268467660885, -1.082531754730548412 ) ) ;
#62184 = CARTESIAN_POINT ( 'NONE',  ( 0.3521856818783953846, 0.1948384997633167970, -2.006960225185448810 ) ) ;
#62186 = CARTESIAN_POINT ( 'NONE',  ( 5.740703853076708718, -2.011634581743710903, -0.4553567745326501104 ) ) ;
#62185 = CARTESIAN_POINT ( 'NONE',  ( 8.727698198895078363, 11.20540053684285553, -1.599625672291257406 ) ) ;
#62187 = DIRECTION ( 'NONE',  ( 0.000000000000000000, 0.000000000000000000, -1.000000000000000000 ) ) ;
#62188 = CARTESIAN_POINT ( 'NONE',  ( -3.391510981712833939, 7.108513245306943062, 0.7998128361456341429 ) ) ;
#62189 = CARTESIAN_POINT ( 'NONE',  ( -1.499999999999997780, 5.181250000682820378, 1.214306433183764966E-14 ) ) ;
#62190 = CARTESIAN_POINT ( 'NONE',  ( 1.364683531249986537, 1.155208333674754728, -0.7879004041258239610 ) ) ;
#62191 = CARTESIAN_POINT ( 'NONE',  ( 6.802024559211160337, -1.870114703409443857, 0.04643648283486622591 ) ) ;
#62192 = CARTESIAN_POINT ( 'NONE',  ( 6.293613488329289574, 1.277945636399902440, -1.172455961997687535 ) ) ;
#62193 = CARTESIAN_POINT ( 'NONE',  ( 5.144012499716256848, 0.5123920008897012712, 1.663301317158589754 ) ) ;
#62194 = CARTESIAN_POINT ( 'NONE',  ( 2.876852093609012950, -0.1713799144957695864, -2.286037302510893099 ) ) ;
#62195 = CARTESIAN_POINT ( 'NONE',  ( 1.364683531249988757, -0.3656249996585800299, 0.000000000000000000 ) ) ;
#62196 = CARTESIAN_POINT ( 'NONE',  ( 1.499689682683522207, -0.6613356838569836027, -1.718437284301529422 ) ) ;
#62197 = DIRECTION ( 'NONE',  ( 0.000000000000000000, 1.000000000000000000, 0.000000000000000000 ) ) ;
#62198 = CARTESIAN_POINT ( 'NONE',  ( 1.922601709848625440, 1.702220721529534853, 0.6601445126475160574 ) ) ;
#62199 = CARTESIAN_POINT ( 'NONE',  ( 2.848279904836711118, 0.2930702634792031747, -1.994869876753922799 ) ) ;
#62200 = CARTESIAN_POINT ( 'NONE',  ( 1.218978173989828884, -0.05078841826402365894, 2.191026318449231791 ) ) ;
#62201 = CARTESIAN_POINT ( 'NONE',  ( 8.800298414079730236, 13.41797088714002761, -7.691148693810730741 ) ) ;
#62202 = CARTESIAN_POINT ( 'NONE',  ( 4.436618261691759102, 2.064837277596673903, 0.4132364508900014943 ) ) ;
#62203 = CARTESIAN_POINT ( 'NONE',  ( -5.391338639728555648, 9.441645512991978961, -0.7998128361456231517 ) ) ;
#62204 = CARTESIAN_POINT ( 'NONE',  ( 8.342299507848510487, 13.15171158923614669, 8.537531030106581653 ) ) ;
#62205 = CARTESIAN_POINT ( 'NONE',  ( 1.680221237283368696, -1.148429780529091948, -1.722445320287042447 ) ) ;
#62206 = CARTESIAN_POINT ( 'NONE',  ( 4.493637847925535667, 7.329995691633395261, -1.199719254218452047 ) ) ;
#62207 = CARTESIAN_POINT ( 'NONE',  ( 1.360316468749971364, -0.7031249996586053097, -3.469446951953614189E-14 ) ) ;
#62208 = CARTESIAN_POINT ( 'NONE',  ( 4.248766647586673884, 2.079802475202694900, 0.4125236972643344102 ) ) ;
#62209 = CARTESIAN_POINT ( 'NONE',  ( 6.217409598193539999, -0.2183660865492654257, 1.812524795094340835 ) ) ;
#62210 = EDGE_LOOP ( 'NONE', ( #179478, #52217, #163043, #16766 ) ) ;
#62211 = CARTESIAN_POINT ( 'NONE',  ( -5.926849427829407269, 6.943687749669614995, -1.199719254218453823 ) ) ;
#62212 = CARTESIAN_POINT ( 'NONE',  ( 8.550388431712704573, 13.12720360364021133, 0.000000000000000000 ) ) ;
#62213 = CARTESIAN_POINT ( 'NONE',  ( 6.983858524370782028, 8.280828045588322084, 1.082531754730549967 ) ) ;
#62214 = CARTESIAN_POINT ( 'NONE',  ( 1.001543065824772753E-15, -1.618749999044086119, 4.012584370867899430 ) ) ;
#62215 = CARTESIAN_POINT ( 'NONE',  ( -4.530395885260773525, 8.437212299446219532, 0.7998128361456481317 ) ) ;
#62216 = CARTESIAN_POINT ( 'NONE',  ( -0.1927127643980519056, -0.4999767001874329542, -2.172835435166208473 ) ) ;
#62217 = CARTESIAN_POINT ( 'NONE',  ( 0.7628874492277806230, -1.525271245827728661, 1.452362197770618923 ) ) ;
#62218 = CARTESIAN_POINT ( 'NONE',  ( -5.601453741101424022, 6.564059448486966986, -1.199719254218453823 ) ) ;
#62219 = CARTESIAN_POINT ( 'NONE',  ( 7.879259827836241570, 12.34422023245099176, 1.040834085586084257E-14 ) ) ;
#62220 = CARTESIAN_POINT ( 'NONE',  ( 5.084723738625635647, 1.780007044882421008, 0.5427147737909858716 ) ) ;
#62221 = CARTESIAN_POINT ( 'NONE',  ( 8.762647353133951711, 9.117510088278095282, 1.040834085586084257E-14 ) ) ;
#62222 = DIRECTION ( 'NONE',  ( -0.000000000000000000, -1.000000000000000000, -0.000000000000000000 ) ) ;
#62223 = CARTESIAN_POINT ( 'NONE',  ( -3.135678666510573365, 6.880318554229450712, 0.000000000000000000 ) ) ;
#62224 = CARTESIAN_POINT ( 'NONE',  ( -8.514157279702020631, 11.91663867875229776, -1.082531754730543971 ) ) ;
#62225 = DIRECTION ( 'NONE',  ( 0.000000000000000000, -1.000000000000000000, -0.000000000000000000 ) ) ;
#62227 = CARTESIAN_POINT ( 'NONE',  ( 2.137090596337941406, -0.09316805448006218460, -1.959763546484971197 ) ) ;
#62226 = CARTESIAN_POINT ( 'NONE',  ( -6.938021921891187382, 9.117444880338284818, -1.599625672291263179 ) ) ;
#62228 = CARTESIAN_POINT ( 'NONE',  ( 0.7081719773709761467, -2.151164098719647200, 0.2130325561137471624 ) ) ;
#62230 = CARTESIAN_POINT ( 'NONE',  ( -5.702738293170157569, 6.277038442308466415, 1.111922112425635989 ) ) ;
#62229 = CARTESIAN_POINT ( 'NONE',  ( -6.283277845290492714, 6.295188672452495915, -0.7998128361456362523 ) ) ;
#62231 = CARTESIAN_POINT ( 'NONE',  ( -1.364683531250014514, 0.2802083336747505649, 0.7879004041258379498 ) ) ;
#62232 = CARTESIAN_POINT ( 'NONE',  ( 2.917049273830461864, 0.5812832248327322038, 1.633648419047509792 ) ) ;
#62233 = CARTESIAN_POINT ( 'NONE',  ( 1.851089384485626210, 1.735827849189163663, -0.1260499613615853887 ) ) ;
#62234 = CARTESIAN_POINT ( 'NONE',  ( 6.263503779833467178, 9.290876262238963790, -1.082531754730537088 ) ) ;
#62235 = CARTESIAN_POINT ( 'NONE',  ( -10.78227258717170578, 6.269840026405313793, 4.500979083849748541 ) ) ;
#62236 = CARTESIAN_POINT ( 'NONE',  ( 1.458361007166041334, 1.524808354686446821, 1.319028796778199730 ) ) ;
#62237 = CARTESIAN_POINT ( 'NONE',  ( 6.925078400183582339, 6.034855204486058611, 2.639235227498262670 ) ) ;
#62238 = CARTESIAN_POINT ( 'NONE',  ( -3.610214042988883598, 7.433943160120816351, 0.7998128361456352531 ) ) ;
#62239 = CARTESIAN_POINT ( 'NONE',  ( 1.164844247922683707, -1.781316891034259164, -0.8450378345598685836 ) ) ;
#62241 = CARTESIAN_POINT ( 'NONE',  ( -6.617788377246204945, 6.893376992974917350, -0.7216878364870338292 ) ) ;
#62240 = CARTESIAN_POINT ( 'NONE',  ( 5.607647405131535479, 1.452367144367059826, 1.244281684088064166 ) ) ;
#62242 = CARTESIAN_POINT ( 'NONE',  ( -5.248414861821563804, 9.137251415518218067, 0.7216878364870267237 ) ) ;
#62243 = CARTESIAN_POINT ( 'NONE',  ( 7.361151057576892143, 7.552707420120024828, 0.7998128361456291469 ) ) ;
#62244 = CARTESIAN_POINT ( 'NONE',  ( -6.095272577795516789, 9.268845886473535245, 1.199719254218452047 ) ) ;
#62245 = CARTESIAN_POINT ( 'NONE',  ( 1.594405160661801490, -1.078473704070359140, 1.707419690039575499 ) ) ;
#62246 = CARTESIAN_POINT ( 'NONE',  ( 4.594930786881223916, -0.5007672277346334466, -2.252456893713528530 ) ) ;
#62247 = CARTESIAN_POINT ( 'NONE',  ( 5.969191311310417802, 1.729517061547349632, 0.9261464158661563140 ) ) ;
#62248 = CARTESIAN_POINT ( 'NONE',  ( 2.131626046773547500, 1.878804184644796926, -0.5645400877590660560 ) ) ;
#62249 = CARTESIAN_POINT ( 'NONE',  ( 8.615316546479974136, 12.13862083994696839, 1.199719254218450271 ) ) ;
#62250 = CARTESIAN_POINT ( 'NONE',  ( -9.494322903035145700, 14.66521395919849624, 7.339005329529387112 ) ) ;
#62251 = VERTEX_POINT ( 'NONE', #37413 ) ;
#62252 = CARTESIAN_POINT ( 'NONE',  ( 1.604857428818485587, 1.977717902320776266, 0.7566523057890365278 ) ) ;
#62254 = CARTESIAN_POINT ( 'NONE',  ( -8.030507057996002729, 8.263346410617135263, 1.040834085586084257E-14 ) ) ;
#62253 = CARTESIAN_POINT ( 'NONE',  ( -5.284980951228653190, 5.060232619388524533, 0.000000000000000000 ) ) ;
#62255 = CARTESIAN_POINT ( 'NONE',  ( 0.9723034553027897209, -0.04304006056080752346, -1.840805954149108636 ) ) ;
#62256 = VERTEX_POINT ( 'NONE', #105652 ) ;
#62257 = CARTESIAN_POINT ( 'NONE',  ( 11.13873122529103554, 9.084116728910979432, 4.468116630735651462 ) ) ;
#62258 = CARTESIAN_POINT ( 'NONE',  ( 2.391022662813433453, -2.030629854096975606, -0.6112283555373964061 ) ) ;
#62259 = CARTESIAN_POINT ( 'NONE',  ( -1.500000000000011324, 4.452083334016148086, 0.8660254037844403729 ) ) ;
#62260 = CARTESIAN_POINT ( 'NONE',  ( 6.916630921265960019, 11.22115317478565188, 0.7998128361456462443 ) ) ;
#62261 = SURFACE_STYLE_USAGE ( .BOTH. , #47100 ) ;
#62262 = CARTESIAN_POINT ( 'NONE',  ( 3.550122082181893290, 2.060967561582152108, 0.003633429623469893420 ) ) ;
#62263 = VECTOR ( 'NONE', #161126, 1000.000000000000000 ) ;
#62265 = CARTESIAN_POINT ( 'NONE',  ( -0.02423404108400224743, -1.785672699080865788, -0.4486397487279417118 ) ) ;
#62264 = CARTESIAN_POINT ( 'NONE',  ( -8.015895134177625891, 10.37496362800581018, 1.599625672291295375 ) ) ;
#62266 = CARTESIAN_POINT ( 'NONE',  ( -1.364683531250012516, 3.738541667008087099, -0.7879004041258300672 ) ) ;
#62267 = CARTESIAN_POINT ( 'NONE',  ( -0.02244404828160087226, 4.081832076214893412, -2.743766916979750281 ) ) ;
#62268 = CARTESIAN_POINT ( 'NONE',  ( 1.362971619486228025, 4.002954933304044616, 0.6272962186313684185 ) ) ;
#62269 = LINE ( 'NONE', #147798, #51152 ) ;
#62270 = CARTESIAN_POINT ( 'NONE',  ( 2.724197551734920175, -1.300482880258296836, -1.851114353284079472 ) ) ;
#62271 = CARTESIAN_POINT ( 'NONE',  ( -8.026063749610043985, 12.30756544127966912, -0.7216878364870267237 ) ) ;
#62272 = CARTESIAN_POINT ( 'NONE',  ( 2.109342631017618874, 1.402271653390272377, 1.146968571259598058 ) ) ;
#62273 = CARTESIAN_POINT ( 'NONE',  ( 3.151485257178482158, 1.867856130240726387, -0.4247363484005464151 ) ) ;
#62274 = CARTESIAN_POINT ( 'NONE',  ( 4.439934286204096914, 1.349936692791346093, 1.569845735447549906 ) ) ;
#62275 = CARTESIAN_POINT ( 'NONE',  ( -1.364683531250012516, 2.342708333674752286, 0.7879004041258379498 ) ) ;
#62276 = EDGE_CURVE ( 'NONE', #11879, #114519, #15676, .T. ) ;
#62277 = CARTESIAN_POINT ( 'NONE',  ( 1.604304721248978494, -0.7076282383621353977, -1.840268529672415498 ) ) ;
#62278 = CARTESIAN_POINT ( 'NONE',  ( 6.217406027492617504, -0.2333201818524588411, 1.912260165615098595 ) ) ;
#62279 = CARTESIAN_POINT ( 'NONE',  ( 2.606148294764852213, -0.7140300644919925777, -1.729217693616967644 ) ) ;
#62280 = CIRCLE ( 'NONE', #38009, 1.600000000000005196 ) ;
#62282 = CARTESIAN_POINT ( 'NONE',  ( 4.827426732796687325, 8.217478009653898852, -0.9130428269800896501 ) ) ;
#62281 = CARTESIAN_POINT ( 'NONE',  ( 1.067484182866541564, -2.088262569869667740, -0.9824423588734966239 ) ) ;
#62283 = CARTESIAN_POINT ( 'NONE',  ( 2.523689441098162511, 1.825779920793478839, -0.3596660026494375995 ) ) ;
#62284 = CARTESIAN_POINT ( 'NONE',  ( 1.364683531249988535, 2.613541667008089764, 0.7879004041258500513 ) ) ;
#62285 = CARTESIAN_POINT ( 'NONE',  ( 6.162562474744170515, -0.7388518307863629619, -1.925989236560563977 ) ) ;
#62286 = CARTESIAN_POINT ( 'NONE',  ( -4.954615070790188369, 7.867802451642154082, -1.199719254218452047 ) ) ;
#62287 = CARTESIAN_POINT ( 'NONE',  ( -1.317902950743175872, 3.538712461327640391, -0.3966175983076866696 ) ) ;
#62288 = CARTESIAN_POINT ( 'NONE',  ( 5.983450976520548359, 1.947180606154915727, -0.8027177699698545554 ) ) ;
#62289 = CARTESIAN_POINT ( 'NONE',  ( 1.364683531249988535, 4.717708333674756283, -0.7879004041258300672 ) ) ;
#62290 = CARTESIAN_POINT ( 'NONE',  ( 6.239563118392394969, -1.560868990211834895, -1.495623836407403484 ) ) ;
#62291 = CARTESIAN_POINT ( 'NONE',  ( 6.006511931541290927, -2.010153113457528118, -0.1956843118748711474 ) ) ;
#62292 = B_SPLINE_CURVE_WITH_KNOTS ( 'NONE', 3,
 ( #133701, #115348, #82772, #66490, #182392, #97990, #134756, #147795, #67557, #148846, #100095, #198636, #116403 ),
 .UNSPECIFIED., .F., .F.,
 ( 4, 3, 3, 3, 4 ),
 ( 2.035183503902616585E-17, 6.251625766521519618E-05, 0.0001877438076102492463, 0.0003155212742595949371, 0.0004444121044040558622 ),
 .UNSPECIFIED. ) ;
#62293 = CARTESIAN_POINT ( 'NONE',  ( 0.6823417656249882723, -1.157291666325249713, 1.181850606188755259 ) ) ;
#62294 = CARTESIAN_POINT ( 'NONE',  ( -3.294268138440636928, 6.787137228248626641, 1.040834085586084257E-14 ) ) ;
#62295 = EDGE_CURVE ( 'NONE', #73749, #146898, #4750, .T. ) ;
#62298 = CARTESIAN_POINT ( 'NONE',  ( 3.985733972737593778, 6.633478153960411738, -1.082531754730548412 ) ) ;
#62297 = CARTESIAN_POINT ( 'NONE',  ( 6.825078400183556049, 7.053092130845653784, 2.453807127456457238 ) ) ;
#62296 = CARTESIAN_POINT ( 'NONE',  ( 5.631432701629774051, 7.663367133358481631, 1.599625672291269396 ) ) ;
#62299 = CARTESIAN_POINT ( 'NONE',  ( -3.983063267364693960, 7.868933921892603323, -0.7998128361456481317 ) ) ;
#62300 = CARTESIAN_POINT ( 'NONE',  ( 4.680875185974167074, 1.673856063443099895, -1.124242729735332347 ) ) ;
#62301 = CARTESIAN_POINT ( 'NONE',  ( -8.376239975144482486, 8.666701480623698828, 1.040834085586084257E-14 ) ) ;
#62303 = CARTESIAN_POINT ( 'NONE',  ( -6.658462837642833421, 8.861568958707010779, 1.443375672974064550 ) ) ;
#62302 = CARTESIAN_POINT ( 'NONE',  ( -8.175203439360366531, 12.48156174598837787, 1.040834085586084257E-14 ) ) ;
#62304 = CARTESIAN_POINT ( 'NONE',  ( 1.364683531249988535, 4.655208333674755394, -0.7879004041258300672 ) ) ;
#62306 = CARTESIAN_POINT ( 'NONE',  ( -1.402160292154681736E-14, 8.921875000341405126, 1.575800808251682339 ) ) ;
#62305 = CARTESIAN_POINT ( 'NONE',  ( 5.893488898593548520, 1.633865717575968324, 1.415524914074948404 ) ) ;
#62307 = CARTESIAN_POINT ( 'NONE',  ( 10.53927507717300216, 2.018041202054248195, -6.084853302869510649 ) ) ;
#62308 = CARTESIAN_POINT ( 'NONE',  ( -11.57163011835881328, 7.018793155873597200, 3.185446920310014640 ) ) ;
#62310 = CARTESIAN_POINT ( 'NONE',  ( 6.362907676916636390, -0.1017654035869921675, -2.013986322929907757 ) ) ;
#62309 = CARTESIAN_POINT ( 'NONE',  ( -5.382223794500835545, 8.262716279350872384, -1.082531754730543971 ) ) ;
#62311 = CARTESIAN_POINT ( 'NONE',  ( 1.364683531249986537, -0.3239583329919163424, 0.7879004041258500513 ) ) ;
#62312 = CARTESIAN_POINT ( 'NONE',  ( 6.639320575229232801, 7.629137130509035636, 2.803262396134009737 ) ) ;
#62313 = CARTESIAN_POINT ( 'NONE',  ( 2.244387868473923575, 0.3767020243423558901, 1.683057829810198136 ) ) ;
#62314 = CARTESIAN_POINT ( 'NONE',  ( 5.657495238652423097, 9.822437888394988548, 0.000000000000000000 ) ) ;
#62315 = CARTESIAN_POINT ( 'NONE',  ( 6.017840079619279692, 8.114175741012878973, -1.599625672291281386 ) ) ;
#62316 = CARTESIAN_POINT ( 'NONE',  ( -11.04678362031243388, 7.051902476693844513, -4.575054176827851649 ) ) ;
#62317 = CARTESIAN_POINT ( 'NONE',  ( 6.116445839754358182, 1.256427234498383561, -1.385894902050835542 ) ) ;
#62318 = CARTESIAN_POINT ( 'NONE',  ( 1.260403266252381416, 2.010875322206317151, 0.09671919503399273310 ) ) ;
#62319 = CARTESIAN_POINT ( 'NONE',  ( -4.793291032674840579, 4.846031192413886579, -0.3973851993939380156 ) ) ;
#62320 = CARTESIAN_POINT ( 'NONE',  ( 2.960231987352707428, 2.196266598062237563, -0.2149427413448631863 ) ) ;
#62321 = CARTESIAN_POINT ( 'NONE',  ( 5.049771808528761952, 1.604214368398539925, 1.463040072455735974 ) ) ;
#62322 = ORIENTED_EDGE ( 'NONE', *, *, #165017, .T. ) ;
#62323 = CARTESIAN_POINT ( 'NONE',  ( 4.085803189671889157, 5.860132702740892263, -1.599625672291273171 ) ) ;
#62324 = CARTESIAN_POINT ( 'NONE',  ( 8.663296969007976855, 12.09063498294259809, -1.082531754730543083 ) ) ;
#62325 = B_SPLINE_CURVE_WITH_KNOTS ( 'NONE', 3,
 ( #86140, #197749, #33129, #181501, #149007, #183633, #152211, #201981, #16851, #151154 ),
 .UNSPECIFIED., .F., .F.,
 ( 4, 2, 2, 2, 4 ),
 ( 0.000000000000000000, 0.1250610353511166506, 0.2501220707022333012, 0.3751831060533499240, 0.5002441414044666024 ),
 .UNSPECIFIED. ) ;
#62327 = CARTESIAN_POINT ( 'NONE',  ( 2.952750085323506468, -1.864176452196796507, -0.7691048347045483791 ) ) ;
#62326 = CARTESIAN_POINT ( 'NONE',  ( 3.405043383231837417, -0.4154483767263848493, -2.079220720149973278 ) ) ;
#62329 = ORIENTED_EDGE ( 'NONE', *, *, #161282, .F. ) ;
#62328 = CARTESIAN_POINT ( 'NONE',  ( 3.603588835282888869, 1.315886683649561295, 1.245372468285299128 ) ) ;
#62330 = CARTESIAN_POINT ( 'NONE',  ( 5.189738938980948291, 9.276722205444929870, 0.000000000000000000 ) ) ;
#62331 = ORIENTED_EDGE ( 'NONE', *, *, #82621, .T. ) ;
#62332 = CARTESIAN_POINT ( 'NONE',  ( 0.8131078318618142342, -0.2785150557334699073, 1.849687307983488571 ) ) ;
#62333 = CARTESIAN_POINT ( 'NONE',  ( 6.972971076130050072, 7.029554431773520129, 1.040834085586084257E-14 ) ) ;
#62335 = CARTESIAN_POINT ( 'NONE',  ( 1.288148359701014600, -0.6930021182445024186, -1.786147582385696486 ) ) ;
#62334 = CARTESIAN_POINT ( 'NONE',  ( -3.228813138348844536, 6.918699094715619502, 0.7998128361456341429 ) ) ;
#62336 = CARTESIAN_POINT ( 'NONE',  ( 3.719872605471109761, 6.605953636083950364, -2.420000000000002149 ) ) ;
#62337 = DIRECTION ( 'NONE',  ( 0.000000000000000000, 0.000000000000000000, 1.000000000000000000 ) ) ;
#62338 = CARTESIAN_POINT ( 'NONE',  ( -1.364683531250012516, 1.842708333674749843, 0.7879004041258379498 ) ) ;
#62339 = CARTESIAN_POINT ( 'NONE',  ( -8.283668668269720925, 8.766627655843896250, 1.056142170575426150E-14 ) ) ;
#62340 = CARTESIAN_POINT ( 'NONE',  ( -9.541187415715041809, 12.15447128979948310, -1.599625672291263179 ) ) ;
#62341 = CARTESIAN_POINT ( 'NONE',  ( 5.471600609837615536, 2.084441204114939161, -0.5725544205837928002 ) ) ;
#62342 = CARTESIAN_POINT ( 'NONE',  ( -5.370438244788932280, 6.398504386076097283, 1.082531754730549078 ) ) ;
#62343 = CARTESIAN_POINT ( 'NONE',  ( -5.901542003698421190, 10.10715911428198055, 0.000000000000000000 ) ) ;
#62344 = CARTESIAN_POINT ( 'NONE',  ( 3.199588043238619672, 1.915454767000431602, -0.9102714984489733707 ) ) ;
#62346 = CARTESIAN_POINT ( 'NONE',  ( -11.79409034920973021, 4.782243044590097192, -4.941202808084400822 ) ) ;
#62345 = DIRECTION ( 'NONE',  ( -3.451266460341926649E-31, -5.200010849845536803E-32, 1.000000000000000000 ) ) ;
#62347 = CARTESIAN_POINT ( 'NONE',  ( 4.358636338273668365, -1.462950666040288006, 1.321578431016472654 ) ) ;
#62348 = CARTESIAN_POINT ( 'NONE',  ( 6.135011676971934058, 1.786887936952135991, 0.6819008164158719687 ) ) ;
#62349 = ORIENTED_EDGE ( 'NONE', *, *, #16160, .F. ) ;
#62350 = CARTESIAN_POINT ( 'NONE',  ( 0.3267351109269465148, -1.353470794461093973, 1.566751113397255812 ) ) ;
#62351 = CARTESIAN_POINT ( 'NONE',  ( 2.923698373526161465, 1.078347508963822587, -1.614843327186490374 ) ) ;
#62352 = ORIENTED_EDGE ( 'NONE', *, *, #68459, .T. ) ;
#62353 = CARTESIAN_POINT ( 'NONE',  ( -4.065465959251405081, 5.836405933916976707, -1.599625672291271394 ) ) ;
#62354 = CARTESIAN_POINT ( 'NONE',  ( 5.363132282657546490, 8.414682208812571673, -1.199719254218452047 ) ) ;
#62356 = CARTESIAN_POINT ( 'NONE',  ( 4.808338034340912337, 8.761478140039733020, 1.040834085586084257E-14 ) ) ;
#62355 = CARTESIAN_POINT ( 'NONE',  ( 2.730511870197129820, 0.2565026084431647480, 2.074771742164283950 ) ) ;
#62357 = CARTESIAN_POINT ( 'NONE',  ( 5.207740400980577888, 5.248321020665011716, 0.000000000000000000 ) ) ;
#62359 = ORIENTED_EDGE ( 'NONE', *, *, #157678, .T. ) ;
#62358 = CARTESIAN_POINT ( 'NONE',  ( 0.5920784091685951100, -1.007499442088593211, 1.505216462368397234 ) ) ;
#62360 = CARTESIAN_POINT ( 'NONE',  ( 4.406973378220558679, 1.706932345810768359, -1.398813476408675260 ) ) ;
#62361 = CARTESIAN_POINT ( 'NONE',  ( 2.977765718515756888, 2.095881712254169305, -0.6909776239150815513 ) ) ;
#62362 = CARTESIAN_POINT ( 'NONE',  ( 1.189939518123926510, 1.139724415472416652, 1.535358521287055300 ) ) ;
#62363 = PRESENTATION_LAYER_ASSIGNMENT (  '', '', ( #114243 ) ) ;
#62364 = CARTESIAN_POINT ( 'NONE',  ( 11.55950211276791428, 13.88000000000000078, -3.221476510067115662 ) ) ;
#62365 = CARTESIAN_POINT ( 'NONE',  ( 4.510256325466165173, 2.069976601481211542, -0.04757507122059301263 ) ) ;
#62367 = CARTESIAN_POINT ( 'NONE',  ( 3.151412294154242844, -1.766339975446712174, -1.245920677233211871 ) ) ;
#62366 = CARTESIAN_POINT ( 'NONE',  ( -3.735435015764967837, 4.316761258935923884, -1.199719254218452047 ) ) ;
#62368 = CARTESIAN_POINT ( 'NONE',  ( 4.810206850810132551, 1.511280187219691928, -1.587364365194674498 ) ) ;
#62369 = DIRECTION ( 'NONE',  ( -0.000000000000000000, -1.000000000000000000, -0.000000000000000000 ) ) ;
#62370 = CARTESIAN_POINT ( 'NONE',  ( -0.4000000000000243916, 3.000000000000566214, -2.023857702507757317 ) ) ;
#62371 = CARTESIAN_POINT ( 'NONE',  ( -0.3520457843950398069, 7.165311474886403076, 1.969365997876477037 ) ) ;
#62372 = CARTESIAN_POINT ( 'NONE',  ( 4.525389411911321602, 8.501647757197021704, -0.7998128361456381397 ) ) ;
#62373 = CARTESIAN_POINT ( 'NONE',  ( -1.642778471874998480, -2.588541666188707957, 2.845375778867863303 ) ) ;
#62374 = CARTESIAN_POINT ( 'NONE',  ( -3.709037541790315640, 6.484905011134099340, -1.199719254218450271 ) ) ;
#62375 = CARTESIAN_POINT ( 'NONE',  ( 0.4049229342097167006, -1.081068455937021611, -1.701946057285643743 ) ) ;
#62376 = CARTESIAN_POINT ( 'NONE',  ( -8.731087737520713432, 10.24898578427137963, 1.082531754730558626 ) ) ;
#62377 = CARTESIAN_POINT ( 'NONE',  ( 4.188381925097388603, 1.111774711627441681, -1.746232563387891679 ) ) ;
#62378 = CARTESIAN_POINT ( 'NONE',  ( 3.791558849520747287, 1.396117892292214613, 1.327735796816224223 ) ) ;
#62379 = CARTESIAN_POINT ( 'NONE',  ( -0.03552856956758054796, -1.956598898622825766, -0.4871759670460884539 ) ) ;
#62380 = CARTESIAN_POINT ( 'NONE',  ( 4.635998460869027227, 7.496083073400806818, -1.199719254218452047 ) ) ;
#62381 = CARTESIAN_POINT ( 'NONE',  ( -1.364683531250010740, 5.738541667008088432, -0.7879004041258300672 ) ) ;
#62382 = CARTESIAN_POINT ( 'NONE',  ( 3.502752968683011225, 0.4741538486671539876, 1.911403532405174133 ) ) ;
#62383 = CARTESIAN_POINT ( 'NONE',  ( 0.8147124124333324779, 2.026155960571228043, 0.8354305900151803854 ) ) ;
#62384 = CARTESIAN_POINT ( 'NONE',  ( 4.266095019097836172, 0.8626762044917112293, 1.609013669381313294 ) ) ;
#62385 = CARTESIAN_POINT ( 'NONE',  ( 6.021229618244865023, 10.03886863134542828, -0.7216878364870458196 ) ) ;
#62386 = CARTESIAN_POINT ( 'NONE',  ( 4.338245966248566177, 4.163634503485842409, 1.214306433183764966E-14 ) ) ;
#62387 = CARTESIAN_POINT ( 'NONE',  ( -6.770317605177755382, 8.992066187497757213, 1.599625672291269396 ) ) ;
#62388 = CARTESIAN_POINT ( 'NONE',  ( 4.908934136599710563, 7.884784371745123366, 1.199719254218451159 ) ) ;
#62389 = ORIENTED_EDGE ( 'NONE', *, *, #88437, .F. ) ;
#62391 = CARTESIAN_POINT ( 'NONE',  ( 5.273694575261410833, 0.3885250917745143862, -1.975199337908732256 ) ) ;
#62390 = CARTESIAN_POINT ( 'NONE',  ( 1.628196140939692338, 0.1813696128579282696, 1.832309401408799276 ) ) ;
#62392 = CARTESIAN_POINT ( 'NONE',  ( 0.3691051123158794467, -0.6094954538576388137, 2.216020297015007134 ) ) ;
#62393 = CARTESIAN_POINT ( 'NONE',  ( 5.225427317040848507, 0.1961275920050585819, -1.951957996302315257 ) ) ;
#62394 = CARTESIAN_POINT ( 'NONE',  ( -6.043183783389232566, 8.073467052085995022, 1.599625672291269396 ) ) ;
#62395 = DIRECTION ( 'NONE',  ( -1.000000000000000000, 0.000000000000000000, 0.000000000000000000 ) ) ;
#62397 = CARTESIAN_POINT ( 'NONE',  ( -4.086893239515592136, 6.855460315155083251, 1.199719254218464037 ) ) ;
#62396 = B_SPLINE_CURVE_WITH_KNOTS ( 'NONE', 3,
 ( #186986, #1811, #134016, #87368, #734, #51675, #132940 ),
 .UNSPECIFIED., .F., .F.,
 ( 4, 3, 4 ),
 ( 0.0001135037246152888473, 0.0006245292469112881514, 0.002007692286193847424 ),
 .UNSPECIFIED. ) ;
#62399 = ADVANCED_FACE ( 'NONE', ( #138135 ), #54733, .F. ) ;
#62398 = CARTESIAN_POINT ( 'NONE',  ( 0.000000000000000000, -5.223431457505076203, 0.000000000000000000 ) ) ;
#62400 = CARTESIAN_POINT ( 'NONE',  ( -4.634908411025374875, 6.500755460986618495, 1.599625672291263179 ) ) ;
#62402 = CARTESIAN_POINT ( 'NONE',  ( 0.4263524580605422276, 1.788790299270696993, 0.5473224044415525569 ) ) ;
#62401 = CARTESIAN_POINT ( 'NONE',  ( 1.734041596967655252, 2.068474147835582144, 0.3034153833333247396 ) ) ;
#62403 = CARTESIAN_POINT ( 'NONE',  ( 0.2981862293453664825, 7.114787932596398079, -1.978802099905859535 ) ) ;
#62404 = CARTESIAN_POINT ( 'NONE',  ( -0.1106727585415836906, 0.7252806920327293794, -2.087287528096515299 ) ) ;
#62405 = CARTESIAN_POINT ( 'NONE',  ( 0.3975144409600079309, -0.5839149016878465437, -1.639678601710597983 ) ) ;
#62406 = CARTESIAN_POINT ( 'NONE',  ( 7.637320603199683866, 7.804628880021436288, -0.7998128361456281477 ) ) ;
#62408 = DIRECTION ( 'NONE',  ( 3.219646771412963434E-15, 1.665334536937739741E-16, 1.000000000000000000 ) ) ;
#62407 = CARTESIAN_POINT ( 'NONE',  ( -11.55950211276791428, 13.88000000000000078, -3.221476510067114329 ) ) ;
#62409 = CARTESIAN_POINT ( 'NONE',  ( 1.980655567072008072, -0.08268669962357808045, -1.723028944404185303 ) ) ;
#62410 = CARTESIAN_POINT ( 'NONE',  ( 1.294752383181968503, 1.788903229852260246, -1.265732775075766092 ) ) ;
#62411 = CARTESIAN_POINT ( 'NONE',  ( 4.635508124736155366, -2.018492079602551392, 0.8926152185086615454 ) ) ;
#62412 = CARTESIAN_POINT ( 'NONE',  ( -9.470156251935129887, 4.005132839944305800, -6.837168546664702085 ) ) ;
#62413 = CARTESIAN_POINT ( 'NONE',  ( 0.8839112305873472186, -2.062193702853211352, 0.6791930824729536242 ) ) ;
#62414 = CARTESIAN_POINT ( 'NONE',  ( 0.1701549220758866166, -1.195335944658926230, 1.380069390326914336 ) ) ;
#62415 = CARTESIAN_POINT ( 'NONE',  ( 2.852857698155007782, -1.958159313504294730, -0.8059144277542380497 ) ) ;
#62416 = CARTESIAN_POINT ( 'NONE',  ( 6.539320575229268684, 7.629137130509104026, 2.396737603865983779 ) ) ;
#62417 = VERTEX_POINT ( 'NONE', #86169 ) ;
#62419 = CARTESIAN_POINT ( 'NONE',  ( 0.6823417656249882723, 0.1552083336747514530, 1.181850606188755259 ) ) ;
#62418 = CARTESIAN_POINT ( 'NONE',  ( 3.386539700769741312, -0.4487184517108309123, -2.247870937536749381 ) ) ;
#62420 = CARTESIAN_POINT ( 'NONE',  ( 0.07755575628183573877, 1.996246338214379801, -2.602582295553407032 ) ) ;
#62421 = CARTESIAN_POINT ( 'NONE',  ( 4.680589345215795838, 6.483773540883647435, -1.599625672291256295 ) ) ;
#62422 = CARTESIAN_POINT ( 'NONE',  ( 5.813180279319686505, 1.817354232980341378, -1.277000798603223464 ) ) ;
#62423 = CARTESIAN_POINT ( 'NONE',  ( -7.049876689426113785, 8.287572894827684777, -1.082531754730544860 ) ) ;
#62424 = CARTESIAN_POINT ( 'NONE',  ( 4.853455804012222430, 5.725081861844796727, 1.082531754730560403 ) ) ;
#62425 = CARTESIAN_POINT ( 'NONE',  ( -6.466876083594135238, 9.528143949959703818, 1.082531754730548412 ) ) ;
#62427 = EDGE_CURVE ( 'NONE', #201330, #86850, #766, .T. ) ;
#62426 = SHAPE_REPRESENTATION ( 'rubber for drip tip', ( #200407 ), #124768 ) ;
#62428 = CARTESIAN_POINT ( 'NONE',  ( 4.041739190649647817, 6.769093918182960579, -1.082531754730548412 ) ) ;
#62429 = EDGE_LOOP ( 'NONE', ( #118493, #200815, #194477, #141120 ) ) ;
#62430 = CARTESIAN_POINT ( 'NONE',  ( 3.656875104409584853, 1.122498086849915921, 1.674887873639265390 ) ) ;
#62432 = CARTESIAN_POINT ( 'NONE',  ( 2.254800304804779110, -0.5458148477457210879, -1.989007103235032048 ) ) ;
#62431 = CARTESIAN_POINT ( 'NONE',  ( 5.717788096661236885, 7.693838750903348789, 1.599625672291267398 ) ) ;
#62433 = CARTESIAN_POINT ( 'NONE',  ( 0.000000000000000000, 19.00000000000000000, 0.000000000000000000 ) ) ;
#62434 = CARTESIAN_POINT ( 'NONE',  ( 4.055297343818923039, 7.745280977848496562, 0.7216878364870257245 ) ) ;
#62435 = DIRECTION ( 'NONE',  ( 0.000000000000000000, 1.000000000000000000, 0.000000000000000000 ) ) ;
#62436 = CARTESIAN_POINT ( 'NONE',  ( 1.364683531249988535, 4.655208333674755394, -0.7879004041258300672 ) ) ;
#62437 = CARTESIAN_POINT ( 'NONE',  ( 5.314472526525434226, 2.023830839259177949, 0.8410439265160507549 ) ) ;
#62438 = CARTESIAN_POINT ( 'NONE',  ( 2.268204128460939550, 1.842446992372799963, -0.8197738674571022344 ) ) ;
#62439 = CARTESIAN_POINT ( 'NONE',  ( 1.891909123491273492, -0.4922293657834125313, -1.774144672653771293 ) ) ;
#62440 = CARTESIAN_POINT ( 'NONE',  ( 5.608269097547198712, 9.694731047113750222, -0.7998128361456281477 ) ) ;
#62441 = FILL_AREA_STYLE_COLOUR ( '', #124461 ) ;
#62442 = CARTESIAN_POINT ( 'NONE',  ( 5.209893869493905427, -1.816617279468687229, 0.1804919988709560719 ) ) ;
#62443 = CARTESIAN_POINT ( 'NONE',  ( 6.557263107265463020, -1.238491779027944162, 1.591905563659588907 ) ) ;
#62444 = CARTESIAN_POINT ( 'NONE',  ( -8.688077508258798431, 9.030511935923748013, -0.7998128361456291469 ) ) ;
#62446 = CARTESIAN_POINT ( 'NONE',  ( -4.959250327548641479, 9.007818825440551791, -0.7998128361456362523 ) ) ;
#62445 = CARTESIAN_POINT ( 'NONE',  ( 5.418922386936855240, 2.088194672119690676, 0.8713435986696310698 ) ) ;
#62447 = CARTESIAN_POINT ( 'NONE',  ( 1.225372267635124635, -0.04993704651819717150, 2.105648344105083947 ) ) ;
#62448 = CARTESIAN_POINT ( 'NONE',  ( -7.937372586157736443, 8.224965870130965584, 0.7998128361456341429 ) ) ;
#62449 = CARTESIAN_POINT ( 'NONE',  ( 8.076906825439115423, 10.44614393447756129, -1.599625672291262513 ) ) ;
#62450 = CARTESIAN_POINT ( 'NONE',  ( 0.6801582343749831283, 2.755208333674742605, 1.178068619123796568 ) ) ;
#62451 = DIRECTION ( 'NONE',  ( 0.7293754827041812883, 0.4452152234102623729, -0.5194177606453139751 ) ) ;
#62452 = CARTESIAN_POINT ( 'NONE',  ( -7.039708073993679704, 9.236078724457858158, 1.599625672291283607 ) ) ;
#62453 = UNCERTAINTY_MEASURE_WITH_UNIT (LENGTH_MEASURE( 1.000000000000000082E-05 ), #7370, 'distance_accuracy_value', 'NONE');
#62454 = CARTESIAN_POINT ( 'NONE',  ( 3.542963271983512463, 7.334866628692126689, -0.05839583369298829985 ) ) ;
#62455 = CARTESIAN_POINT ( 'NONE',  ( 6.502017186205484300, 9.743381262951846367, -1.199719254218452047 ) ) ;
#62456 = CARTESIAN_POINT ( 'NONE',  ( 5.048403365090235795, 6.545034038527520082, -1.227034678662905609 ) ) ;
#62457 = CARTESIAN_POINT ( 'NONE',  ( -9.707274797704657843, 11.38787068781932987, 1.082531754730558626 ) ) ;
#62459 = CARTESIAN_POINT ( 'NONE',  ( 2.830584216690882116, -1.098655552678593716, -1.930667878645520474 ) ) ;
#62458 = CARTESIAN_POINT ( 'NONE',  ( 1.986737319265439394, -1.300789755646198476, 1.674730562594067829 ) ) ;
#62460 = LINE ( 'NONE', #111284, #85573 ) ;
#62462 = CARTESIAN_POINT ( 'NONE',  ( -5.855142236255304944, 7.924361590421551860, -1.599625672291271394 ) ) ;
#62461 = CIRCLE ( 'NONE', #41771, 0.07999999999999998779 ) ;
#62463 = CARTESIAN_POINT ( 'NONE',  ( 5.341022448779654930, 8.318611059296550536, 1.199719254218462483 ) ) ;
#62464 = CARTESIAN_POINT ( 'NONE',  ( 2.980854556682940526, 1.846358069237159949, 0.6635599008937702603 ) ) ;
#62465 = CARTESIAN_POINT ( 'NONE',  ( 4.798696304233017074, 7.685897223992134819, -1.199719254218452047 ) ) ;
#62466 = CARTESIAN_POINT ( 'NONE',  ( -4.026842413655439046, 7.608452276161581374, 0.2328349793435397497 ) ) ;
#62467 = CARTESIAN_POINT ( 'NONE',  ( 5.196852952739813070, 4.957416621151553571, -0.7998128361456221525 ) ) ;
#62468 = CARTESIAN_POINT ( 'NONE',  ( -3.499413046103020175, 7.096749297179887783, 0.7216878364870338292 ) ) ;
#62470 = EDGE_LOOP ( 'NONE', ( #110779, #120571, #122925, #157467, #66735, #4333 ) ) ;
#62469 = CARTESIAN_POINT ( 'NONE',  ( -7.876924059859742755, 8.292092279365579799, 1.040834085586084257E-14 ) ) ;
#62471 = CARTESIAN_POINT ( 'NONE',  ( 2.900754761704402274, -2.089926006748676457, -0.3584049868644647585 ) ) ;
#62472 = CARTESIAN_POINT ( 'NONE',  ( -4.827585214917754719, 7.789877296449459365, -1.199719254218453823 ) ) ;
#62473 = CARTESIAN_POINT ( 'NONE',  ( 4.416967121957662279, 1.975198431823081302, 0.8787980929093119897 ) ) ;
#62474 = CARTESIAN_POINT ( 'NONE',  ( 3.210337823311388394, 1.665856106666419034, 0.7845605768846477535 ) ) ;
#62475 = CARTESIAN_POINT ( 'NONE',  ( -5.171837412746745244, 6.485142596490002909, 1.193510785747232905 ) ) ;
#62476 = CARTESIAN_POINT ( 'NONE',  ( 1.364683531249986537, 0.2177083336747502595, -0.7879004041258309554 ) ) ;
#62477 = CARTESIAN_POINT ( 'NONE',  ( 5.630708778567339756, -1.570753007681056079, 0.7496256940079452091 ) ) ;
#62478 = CARTESIAN_POINT ( 'NONE',  ( 10.94245301910277668, 3.162178953954597471, -3.962121973755224680 ) ) ;
#62479 = CARTESIAN_POINT ( 'NONE',  ( 5.016153647376212277, 5.914896012436124728, 1.082531754730558626 ) ) ;
#62480 = AXIS2_PLACEMENT_3D ( 'NONE', #103712, #19234, #170833 ) ;
#62481 = CARTESIAN_POINT ( 'NONE',  ( 3.028364643526501698, 1.202066397148596977, -1.796461956351296019 ) ) ;
#62482 = CARTESIAN_POINT ( 'NONE',  ( 4.481795959180916888, 1.842165523724150544, 0.8196470798618460396 ) ) ;
#62483 = CARTESIAN_POINT ( 'NONE',  ( -8.148087131688683371, 11.48955683940339867, -1.082531754730543083 ) ) ;
#62484 = CARTESIAN_POINT ( 'NONE',  ( 2.905317003618158367, 1.825515667692039878, 1.157497049167732550 ) ) ;
#62485 = CARTESIAN_POINT ( 'NONE',  ( 2.899638734157696796, -0.6216841358992927224, 1.870808799549168233 ) ) ;
#62486 = DIRECTION ( 'NONE',  ( 0.7592566023653004592, 0.6507913734559639396, 0.000000000000000000 ) ) ;
#62487 = CARTESIAN_POINT ( 'NONE',  ( 4.563973399113295137, -1.265747467430546225, 1.473022616845516053 ) ) ;
#62490 = ORIENTED_EDGE ( 'NONE', *, *, #106413, .F. ) ;
#62489 = DIRECTION ( 'NONE',  ( -0.000000000000000000, -1.000000000000000000, -0.000000000000000000 ) ) ;
#62488 = CARTESIAN_POINT ( 'NONE',  ( -9.639484029191951464, 10.34841224358651601, 0.7216878364870438212 ) ) ;
#62491 = CARTESIAN_POINT ( 'NONE',  ( -7.767895665986912057, 8.027242796598338614, -0.7998128361456362523 ) ) ;
#62493 = VERTEX_POINT ( 'NONE', #120884 ) ;
#62492 = CARTESIAN_POINT ( 'NONE',  ( -5.666381855868691808, 5.575476684793721383, 0.000000000000000000 ) ) ;
#62494 = CARTESIAN_POINT ( 'NONE',  ( -8.825994812371996900, 9.399341490629888440, 0.7216878364870438212 ) ) ;
#62495 = CARTESIAN_POINT ( 'NONE',  ( 0.6048602812970468312, -0.7454967350204610987, -2.077179305122120123 ) ) ;
#62496 = CARTESIAN_POINT ( 'NONE',  ( 3.285556943750000070, -0.9843749995220412163, 0.000000000000000000 ) ) ;
#62497 = CARTESIAN_POINT ( 'NONE',  ( 5.910985094894211755, -1.548708053515185812, 1.204094020389692155 ) ) ;
#62498 = CARTESIAN_POINT ( 'NONE',  ( 0.6823417656249899377, 5.238541667008086655, -1.181850606188754593 ) ) ;
#62499 = CARTESIAN_POINT ( 'NONE',  ( -1.500000000000011324, 3.952083334016153415, 0.8660254037844403729 ) ) ;
#62500 = CARTESIAN_POINT ( 'NONE',  ( 5.693912546396379781, 6.288398852508453096, -1.088204328156989087 ) ) ;
#62501 = CARTESIAN_POINT ( 'NONE',  ( 0.07499057489264347731, 2.883324855518037300, -2.444194386608829372 ) ) ;
#62502 = CARTESIAN_POINT ( 'NONE',  ( 4.927609005033061429, 0.9437523325564222132, -1.580719041474540010 ) ) ;
#62503 = ORIENTED_EDGE ( 'NONE', *, *, #61376, .F. ) ;
#62504 = CARTESIAN_POINT ( 'NONE',  ( -5.558564015327489343E-14, -0.4218749996585599571, -1.570758158831802254 ) ) ;
#62505 = CARTESIAN_POINT ( 'NONE',  ( -6.496328159242330536, 10.73079995242472862, 0.000000000000000000 ) ) ;
#62506 = DIRECTION ( 'NONE',  ( 0.000000000000000000, 9.023263958591316185E-17, -1.000000000000000000 ) ) ;
#62507 = LINE ( 'NONE', #25735, #209912 ) ;
#62508 = FILL_AREA_STYLE ('',( #210883 ) ) ;
#62509 = CARTESIAN_POINT ( 'NONE',  ( 4.476163270806094552, 8.373940915915776273, 0.7998128361456462443 ) ) ;
#62510 = CARTESIAN_POINT ( 'NONE',  ( 6.696563014664697278, -0.5452183415704283664, -1.987298092995327226 ) ) ;
#62513 = CARTESIAN_POINT ( 'NONE',  ( 3.720104550828434942, 1.749555917645674530, 0.5740644926693627692 ) ) ;
#62512 = CARTESIAN_POINT ( 'NONE',  ( 1.715070751487054013, -1.593955780799067412, -0.9604075334226671590 ) ) ;
#62511 = CARTESIAN_POINT ( 'NONE',  ( -10.50060100873255031, 5.377693802073530982, 5.808388628131299747 ) ) ;
#62514 = CARTESIAN_POINT ( 'NONE',  ( 8.284195553149872993, 9.623648552551724578, -1.199719254218445830 ) ) ;
#62515 = SURFACE_STYLE_FILL_AREA ( #179485 ) ;
#62516 =( BOUNDED_SURFACE ( )  B_SPLINE_SURFACE ( 3, 3, ( 
 ( #78065, #58619, #61822, #195019, #76990, #145245, #43460, #210182, #161470, #192867, #46651 ),
 ( #109581, #91143, #157199, #27175, #8796, #74875, #190734, #42397, #108507, #60746, #126908 ),
 ( #176642, #11989, #45590, #175585, #193943, #95418, #93279, #159317, #111706, #44523, #28254 ),
 ( #144190, #177715, #29324, #47727, #67107, #214408, #64993, #183017, #97537, #196094, #179839 ),
 ( #31460, #30399, #15177, #146298, #181942, #96485, #66039, #32511, #163594, #130100, #162532 ),
 ( #180889, #81264, #132186, #113843, #147343, #213371, #212310, #112774, #50895, #117021, #99644 ),
 ( #198192, #33572, #178785, #131147, #197136, #14104, #148409, #165711, #17300, #48775, #80194 ) ),
 .UNSPECIFIED., .T., .F., .T. ) 
 B_SPLINE_SURFACE_WITH_KNOTS ( ( 4, 3, 4 ),
 ( 4, 1, 1, 1, 1, 1, 1, 1, 4 ),
 ( 0.000000000000000000, 0.5000000000000000000, 1.000000000000000000 ),
 ( 0.000000000000000000, 0.2255234228546724728, 0.3973271701647976828, 0.5245128843546777997, 0.6161923999872991331, 0.6815320185768301009, 0.7298552812456317040, 0.7704940248801678271, 1.000000000000000000 ),
 .UNSPECIFIED. ) 
 GEOMETRIC_REPRESENTATION_ITEM ( )  RATIONAL_B_SPLINE_SURFACE ( (
 ( 1.000000000000000222, 1.000000000000000222, 1.000000000000000666, 0.9999999999999996669, 1.000000000000000222, 0.9999999999999997780, 1.000000000000000000, 1.000000000000000222, 1.000000000000000000, 1.000000000000000000, 1.000000000000000000),
 ( 0.3333333333333334259, 0.3333333333333334259, 0.3333333333333335369, 0.3333333333333333148, 0.3333333333333333148, 0.3333333333333333703, 0.3333333333333333703, 0.3333333333333334814, 0.3333333333333333148, 0.3333333333333334259, 0.3333333333333333703),
 ( 0.3333333333333334259, 0.3333333333333334259, 0.3333333333333335369, 0.3333333333333333148, 0.3333333333333333148, 0.3333333333333333703, 0.3333333333333333703, 0.3333333333333334814, 0.3333333333333333148, 0.3333333333333334259, 0.3333333333333333703),
 ( 1.000000000000000222, 1.000000000000000222, 1.000000000000000666, 0.9999999999999996669, 1.000000000000000222, 0.9999999999999997780, 1.000000000000000000, 1.000000000000000222, 1.000000000000000000, 1.000000000000000000, 1.000000000000000000),
 ( 0.3333333333333334259, 0.3333333333333334259, 0.3333333333333335369, 0.3333333333333333148, 0.3333333333333333148, 0.3333333333333333703, 0.3333333333333333703, 0.3333333333333334814, 0.3333333333333333148, 0.3333333333333334259, 0.3333333333333333703),
 ( 0.3333333333333334259, 0.3333333333333334259, 0.3333333333333335369, 0.3333333333333333148, 0.3333333333333333148, 0.3333333333333333703, 0.3333333333333333703, 0.3333333333333334814, 0.3333333333333333148, 0.3333333333333334259, 0.3333333333333333703),
 ( 1.000000000000000222, 1.000000000000000222, 1.000000000000000666, 0.9999999999999996669, 1.000000000000000222, 0.9999999999999997780, 1.000000000000000000, 1.000000000000000222, 1.000000000000000000, 1.000000000000000000, 1.000000000000000000) ) ) 
 REPRESENTATION_ITEM ( '' )  SURFACE ( )  );
#62517 = AXIS2_PLACEMENT_3D ( 'NONE', #76563, #121146, #210826 ) ;
#62518 = CARTESIAN_POINT ( 'NONE',  ( -6.740338644649361832, 7.892758502626242567, -1.199719254218452047 ) ) ;
#62520 = ORIENTED_EDGE ( 'NONE', *, *, #132876, .F. ) ;
#62519 = CARTESIAN_POINT ( 'NONE',  ( 1.284279953904126748, 10.64264068711930733, -0.7749999999999874767 ) ) ;
#62521 = CARTESIAN_POINT ( 'NONE',  ( 3.369938178094655346, 2.153121441420174698, -0.4834393813165636100 ) ) ;
#62522 = CARTESIAN_POINT ( 'NONE',  ( 6.221994747346401233, -1.249160343739505352, -1.886125069868335613 ) ) ;
#62523 = CARTESIAN_POINT ( 'NONE',  ( -6.941411460516810017, 8.161030127766803588, 1.082531754730549967 ) ) ;
#62524 = CARTESIAN_POINT ( 'NONE',  ( 5.871335974614770414, -1.558408318232169298, -0.9234296637983196998 ) ) ;
#62525 = CARTESIAN_POINT ( 'NONE',  ( 5.999236059146234368, -0.2270968913323672123, 1.902120139356741069 ) ) ;
#62526 = DIRECTION ( 'NONE',  ( -5.578564026256491869E-16, -1.000000000000000000, -9.066213480720160632E-32 ) ) ;
#62527 = ADVANCED_FACE ( 'NONE', ( #186858 ), #87246, .T. ) ;
#62528 = CARTESIAN_POINT ( 'NONE',  ( 6.016445890116215445, 1.255022122864515310, -1.387330985440645037 ) ) ;
#62529 = DIRECTION ( 'NONE',  ( 1.000000000000000000, -5.578564026256504688E-16, 1.972152263052529514E-31 ) ) ;
#62530 = CARTESIAN_POINT ( 'NONE',  ( 6.473528777534793832, 1.692185636751794897, -0.5185713626470798143 ) ) ;
#62531 = CARTESIAN_POINT ( 'NONE',  ( 1.182827746461931229, 1.645757370610765102, -1.164989914844760444 ) ) ;
#62533 = CARTESIAN_POINT ( 'NONE',  ( 3.334694542603059642, 2.054772597177223936, 0.4612437286577449891 ) ) ;
#62532 = CARTESIAN_POINT ( 'NONE',  ( -10.17947440576205054, 10.77047498301088346, 0.7998128361456462443 ) ) ;
#62534 = CARTESIAN_POINT ( 'NONE',  ( 7.801827329660018684, 11.18955008699033726, 1.199719254218460707 ) ) ;
#62536 = CARTESIAN_POINT ( 'NONE',  ( -9.124801077197171040, 10.60435499727357289, -1.199719254218441611 ) ) ;
#62535 = CARTESIAN_POINT ( 'NONE',  ( 1.499999999999987121, -0.9958333333333134751, 0.8660254037844524744 ) ) ;
#62537 = DIRECTION ( 'NONE',  ( 0.000000000000000000, 0.000000000000000000, 1.000000000000000000 ) ) ;
#62538 = CARTESIAN_POINT ( 'NONE',  ( 2.496358458697241378, -1.034576831241553307, 1.734530517449877740 ) ) ;
#62539 = CARTESIAN_POINT ( 'NONE',  ( -1.364683531249997417, 4.009375000341424133, 1.214306433183764966E-14 ) ) ;
#62540 = CARTESIAN_POINT ( 'NONE',  ( 10.56143847536557878, 11.42402576412244386, 0.000000000000000000 ) ) ;
#62541 = CARTESIAN_POINT ( 'NONE',  ( 3.497504216883956296, 1.701635573755799324, 1.332874705691905248 ) ) ;
#62542 = CARTESIAN_POINT ( 'NONE',  ( 7.364013710877980401, 8.620379413226322285, -1.199719254218452047 ) ) ;
#62543 = CARTESIAN_POINT ( 'NONE',  ( 6.481679955784983349, 9.719654494127929922, -1.199719254218452047 ) ) ;
#62544 = CARTESIAN_POINT ( 'NONE',  ( 8.717529583462646059, 11.19353715217169309, 1.443375672974076540 ) ) ;
#62546 = CARTESIAN_POINT ( 'NONE',  ( 6.902720183911292828, 15.44694763437295570, -9.761920501353822388 ) ) ;
#62545 = CARTESIAN_POINT ( 'NONE',  ( 0.7663804396884700276, -2.160669279729439562, 0.2131170157090022665 ) ) ;
#62547 = CARTESIAN_POINT ( 'NONE',  ( -6.019457014787517046, 9.006155036351978893, 1.082531754730548412 ) ) ;
#62548 = CARTESIAN_POINT ( 'NONE',  ( 1.364683531249988757, 0.3843750003414206362, 0.000000000000000000 ) ) ;
#62549 = CARTESIAN_POINT ( 'NONE',  ( 2.560326853991791829, -1.509077608345666066, 1.589458984681046516 ) ) ;
#62550 = CARTESIAN_POINT ( 'NONE',  ( 6.983263157960368339, 1.271300847835453940, 2.069154070428773196 ) ) ;
#62551 = CARTESIAN_POINT ( 'NONE',  ( 3.046068780686244981, 0.8155736813739141722, -2.110571434806473690 ) ) ;
#62552 = CARTESIAN_POINT ( 'NONE',  ( -8.505042434474312074, 8.816971016508505343, -0.7998128361456291469 ) ) ;
#62553 = CARTESIAN_POINT ( 'NONE',  ( -4.270455198180246548, 4.084545274072787890, 0.7216878364870317197 ) ) ;
#62554 = CARTESIAN_POINT ( 'NONE',  ( -0.6823417656250003738, 2.780208333674753618, -1.181850606188749264 ) ) ;
#62555 = CARTESIAN_POINT ( 'NONE',  ( 5.510920874727778696, 7.454463421478725316, 1.249874847645112697 ) ) ;
#62556 = CARTESIAN_POINT ( 'NONE',  ( -1.500000000000015099, 12.22916666666666607, -0.8660254037844309360 ) ) ;
#62557 = CARTESIAN_POINT ( 'NONE',  ( 7.363486825997814123, 7.763358516518489516, 0.000000000000000000 ) ) ;
#62558 = CARTESIAN_POINT ( 'NONE',  ( 3.848697245170757508, -1.448060206101034808, 1.017097547381773159 ) ) ;
#62559 = CARTESIAN_POINT ( 'NONE',  ( 8.048736748007069508, 12.54194330598362406, -0.7998128361456352531 ) ) ;
#62560 = CARTESIAN_POINT ( 'NONE',  ( 6.704147062870869256, -2.206433763861126884, 0.04732420095975712476 ) ) ;
#62562 = EDGE_CURVE ( 'NONE', #116082, #148658, #15141, .T. ) ;
#62561 = CARTESIAN_POINT ( 'NONE',  ( -1.364683531250014514, 9.838541667008064096, -0.7879004041258335089 ) ) ;
#62563 = CARTESIAN_POINT ( 'NONE',  ( -5.255720823952942489, 6.160704378480398979, -1.199719254218453823 ) ) ;
#62564 = CARTESIAN_POINT ( 'NONE',  ( -7.285838599102589797E-14, 7.078193277237590841, -2.121339347286493648 ) ) ;
#62565 = ORIENTED_EDGE ( 'NONE', *, *, #48830, .F. ) ;
#62566 = CARTESIAN_POINT ( 'NONE',  ( 4.012460596634464416, 1.323225596166040186, -1.322536486416128199 ) ) ;
#62567 = CARTESIAN_POINT ( 'NONE',  ( 3.731357587288411715, 0.05568397596692270524, -2.069689236595618542 ) ) ;
#62568 = AXIS2_PLACEMENT_3D ( 'NONE', #133331, #97621, #99727 ) ;
#62569 = CARTESIAN_POINT ( 'NONE',  ( -5.763624699140882157, 7.817591130454727200, -1.443375672974066548 ) ) ;
#62570 = CARTESIAN_POINT ( 'NONE',  ( -10.39336823037077195, 4.932734307774878424, -5.330979603150785451 ) ) ;
#62571 = CARTESIAN_POINT ( 'NONE',  ( -4.108375792757257727, 7.564741050373271491, 0.6295801075443598904 ) ) ;
#62572 = ADVANCED_FACE ( 'NONE', ( #127300 ), #58708, .T. ) ;
#62573 = CARTESIAN_POINT ( 'NONE',  ( 6.139563164240942506, -1.562336469324271837, -1.494251390645913835 ) ) ;
#62574 = CARTESIAN_POINT ( 'NONE',  ( -1.402160292154681736E-14, -0.8031249996585825279, -1.575800808251665908 ) ) ;
#62575 = CARTESIAN_POINT ( 'NONE',  ( 3.262109210011232108, -1.959739898415867154, 0.09363895518171151677 ) ) ;
#62576 = CARTESIAN_POINT ( 'NONE',  ( 1.106795812180675798, 0.8196504822069600182, -1.842164015508622521 ) ) ;
#62577 = CARTESIAN_POINT ( 'NONE',  ( -4.146814880933400005, 5.931313009212638931, 1.599625672291270506 ) ) ;
#62579 = CARTESIAN_POINT ( 'NONE',  ( 6.385527162356455122, 10.39360608948380538, 1.056142170575426150E-14 ) ) ;
#62578 = CARTESIAN_POINT ( 'NONE',  ( 7.801827329660018684, 11.18955008699033726, 1.199719254218460707 ) ) ;
#62580 = CARTESIAN_POINT ( 'NONE',  ( 0.5615140978009087736, 1.851110617189118734, -0.2680550677405246773 ) ) ;
#62581 = CARTESIAN_POINT ( 'NONE',  ( 0.6823417656249917140, 4.092708333674755394, 1.181850606188765695 ) ) ;
#62582 = CARTESIAN_POINT ( 'NONE',  ( 2.672137747239998529, 2.003105221038860684, -0.2016864653290161569 ) ) ;
#62584 = CARTESIAN_POINT ( 'NONE',  ( 1.792722901331974761, 1.566437577840825712, -1.424566180320179010 ) ) ;
#62583 = CARTESIAN_POINT ( 'NONE',  ( -6.561783159334130922, 9.638868871656395498, -1.082531754730538864 ) ) ;
#62585 = CARTESIAN_POINT ( 'NONE',  ( 9.984004359900959358, 9.817747272193987129, -6.683988694658842711 ) ) ;
#62586 = CARTESIAN_POINT ( 'NONE',  ( 4.246580143467587831, -2.047389768388275577, -0.3068500204662719666 ) ) ;
#62587 = CARTESIAN_POINT ( 'NONE',  ( 6.318982112420993502, 9.529840343536603697, -1.199719254218452047 ) ) ;
#62589 = CARTESIAN_POINT ( 'NONE',  ( 4.227444969362701421, 3.826440640544909400, 1.214306433183764966E-14 ) ) ;
#62588 = CARTESIAN_POINT ( 'NONE',  ( 5.419903170966573924, 1.246048553727102659, -1.678571210107776324 ) ) ;
#62591 = ORIENTED_EDGE ( 'NONE', *, *, #184771, .T. ) ;
#62590 = CARTESIAN_POINT ( 'NONE',  ( 5.332948099851452461, 0.1360325894329272867, 1.820554394434070744 ) ) ;
#62592 = CARTESIAN_POINT ( 'NONE',  ( 8.041957671200231417, 12.53403438304231976, 1.040834085586084257E-14 ) ) ;
#62593 = CARTESIAN_POINT ( 'NONE',  ( 1.598423149420349354, 8.713846000021359117, -2.499999999999995115 ) ) ;
#62594 = CARTESIAN_POINT ( 'NONE',  ( 12.12244102266335233, 8.055895858565015999, 3.199560920820632148 ) ) ;
#62595 = TOROIDAL_SURFACE ( 'NONE', #17592, 10.89999999999920632, 0.2000000000000000111 ) ;
#62596 = CARTESIAN_POINT ( 'NONE',  ( 6.458075443588827014, 2.201329523236052577, -0.1558686762383256486 ) ) ;
#62597 = CARTESIAN_POINT ( 'NONE',  ( 0.6823417656249934904, 11.25520833367473017, 1.181850606188764807 ) ) ;
#62598 = CARTESIAN_POINT ( 'NONE',  ( 5.180287844241702189, 0.9460499258955605839, 1.661804969971327761 ) ) ;
#62599 = CARTESIAN_POINT ( 'NONE',  ( -8.947491310014823895, 12.52615806407091803, 1.199719254218462483 ) ) ;
#62600 = CARTESIAN_POINT ( 'NONE',  ( 7.142447996300871793, 7.227277505306155092, 0.7998128361456341429 ) ) ;
#62601 = CARTESIAN_POINT ( 'NONE',  ( -1.360316468750032870, 0.9427083336747505982, 0.7853790794158641564 ) ) ;
#62602 = CARTESIAN_POINT ( 'NONE',  ( 4.039439701867726384, 6.800097854565950506, 1.199719254218462483 ) ) ;
#62603 = ORIENTED_EDGE ( 'NONE', *, *, #97745, .T. ) ;
#62604 = AXIS2_PLACEMENT_3D ( 'NONE', #192868, #206991, #95419 ) ;
#62605 = CARTESIAN_POINT ( 'NONE',  ( -7.208094944320834863, 8.438474185576302133, -1.199719254218452047 ) ) ;
#62606 = CARTESIAN_POINT ( 'NONE',  ( 5.096879011283717453, 1.555924861325823416, -1.037969726935553005 ) ) ;
#62607 = CARTESIAN_POINT ( 'NONE',  ( -0.02319159430949970999, 0.003959926571647092407, -1.810968101872318714 ) ) ;
#62608 = CARTESIAN_POINT ( 'NONE',  ( 7.503511670520385479, 7.718794801887437274, 0.7998128361456281477 ) ) ;
#62609 = CARTESIAN_POINT ( 'NONE',  ( 0.06970548857354719186, 14.49233334675339080, 11.99964040467434145 ) ) ;
#62610 = B_SPLINE_CURVE_WITH_KNOTS ( 'NONE', 3,
 ( #60870, #177836, #146421, #145375 ),
 .UNSPECIFIED., .F., .F.,
 ( 4, 4 ),
 ( 1.084337306069862702E-15, 8.505390839925406612E-05 ),
 .UNSPECIFIED. ) ;
#62611 = CARTESIAN_POINT ( 'NONE',  ( -5.679286501732877745, 7.334821546209805199, 1.225395024417414103 ) ) ;
#62612 = CARTESIAN_POINT ( 'NONE',  ( -7.226132686403777150, 7.532835677000276675, 1.040834085586084257E-14 ) ) ;
#62613 = CARTESIAN_POINT ( 'NONE',  ( 5.332434488876471868, 5.115595079977664383, 0.7998128361456341429 ) ) ;
#62614 = CARTESIAN_POINT ( 'NONE',  ( 0.8835773814684219074, -1.871821877138898582, 0.6126781507047509567 ) ) ;
#62615 = CARTESIAN_POINT ( 'NONE',  ( 3.304314702139679039, 1.277028363417181289, -1.560513873864778578 ) ) ;
#62616 = CARTESIAN_POINT ( 'NONE',  ( -8.016948904382338981, 8.247528564734524892, -0.7998128361456291469 ) ) ;
#62617 = CARTESIAN_POINT ( 'NONE',  ( 4.960304097753311936, 6.880383762169266504, 1.599625672291268286 ) ) ;
#62618 = DIRECTION ( 'NONE',  ( 3.451266460341927524E-31, -0.6000000000000035305, -0.7999999999999974909 ) ) ;
#62619 = CARTESIAN_POINT ( 'NONE',  ( 3.152458698460915532, -1.659165413833121550, 1.431739491984926671 ) ) ;
#62620 = CARTESIAN_POINT ( 'NONE',  ( -10.08065090696061716, 11.71951313199760136, -1.199719254218441611 ) ) ;
#62621 = CARTESIAN_POINT ( 'NONE',  ( 6.825078400183572036, 4.699117039843025090, 2.418333817060664526 ) ) ;
#62622 = CARTESIAN_POINT ( 'NONE',  ( -5.204170427930421283E-14, 3.949999999999960654, -4.683753385137379155E-14 ) ) ;
#62623 = CARTESIAN_POINT ( 'NONE',  ( -9.470156251935129887, 4.005132839944305800, -6.837168546664702085 ) ) ;
#62624 = CARTESIAN_POINT ( 'NONE',  ( 8.457588896826466751, 8.761608555919362828, 1.040834085586084257E-14 ) ) ;
#62625 = CARTESIAN_POINT ( 'NONE',  ( 4.403700966340357681, 4.032072637018845107, -0.7998128361456211532 ) ) ;
#62626 = CARTESIAN_POINT ( 'NONE',  ( 5.641601317062233001, 7.675230518029648508, -1.443375672974078761 ) ) ;
#62627 = ORIENTED_EDGE ( 'NONE', *, *, #189117, .T. ) ;
#62629 = CARTESIAN_POINT ( 'NONE',  ( 1.436190773529995468, -1.120142249841639348, -1.672479584328613988 ) ) ;
#62628 = CARTESIAN_POINT ( 'NONE',  ( 5.003375819710620398, -1.831856422778654681, 0.1858995714831001289 ) ) ;
#62630 = CARTESIAN_POINT ( 'NONE',  ( 3.814061661026487915, -1.881531058455442329, 1.319806432912509209 ) ) ;
#62632 = CARTESIAN_POINT ( 'NONE',  ( 2.131498006616658891, 1.782543213153169548, -0.5345681993311669489 ) ) ;
#62631 = CARTESIAN_POINT ( 'NONE',  ( -0.02880301295724378360, 1.300294777490899056, -2.522425657339548266 ) ) ;
#62633 = CARTESIAN_POINT ( 'NONE',  ( 1.642778471875000035, -1.276041666188710400, -2.845375778867859751 ) ) ;
#62634 = FACE_OUTER_BOUND ( 'NONE', #105617, .T. ) ;
#62635 = CARTESIAN_POINT ( 'NONE',  ( 5.431871263539022721, -1.864374737420209760, 0.4251265778823994368 ) ) ;
#62636 = CARTESIAN_POINT ( 'NONE',  ( -8.355902744723985975, 8.642974711799791265, 1.040834085586084257E-14 ) ) ;
#62637 = EDGE_CURVE ( 'NONE', #71330, #212186, #76880, .T. ) ;
#62638 = CARTESIAN_POINT ( 'NONE',  ( -6.780486220610195680, 7.083191143566240910, -0.7216878364870338292 ) ) ;
#62640 = CARTESIAN_POINT ( 'NONE',  ( 2.887410755087606695, 1.321643875934110479, 1.324118206929347563 ) ) ;
#62639 = CARTESIAN_POINT ( 'NONE',  ( 4.335544241866786663, 0.8922555979511301860, -1.890918108395107211 ) ) ;
#62641 = CARTESIAN_POINT ( 'NONE',  ( 5.178851490740187913, 8.985817805931475277, 0.7216878364870438212 ) ) ;
#62642 = CARTESIAN_POINT ( 'NONE',  ( 6.216338285296751920, 1.720575329815833943, 0.6561210673821931127 ) ) ;
#62643 = CARTESIAN_POINT ( 'NONE',  ( 4.356247428692526569, 3.976710176429713250, 0.7998128361456341429 ) ) ;
#62644 = CARTESIAN_POINT ( 'NONE',  ( 0.1826339422288050240, -7.841768514962160097, -10.96557956857097160 ) ) ;
#62645 = CARTESIAN_POINT ( 'NONE',  ( 5.373588365490253871, 1.660756567380991866, -0.4657003604296525157 ) ) ;
#62646 = CARTESIAN_POINT ( 'NONE',  ( -6.144869935491728441, 8.192100896205577243, -1.599625672291263179 ) ) ;
#62647 = CARTESIAN_POINT ( 'NONE',  ( -11.71730914997697326, 8.541829549342406125, -2.386335717864155104 ) ) ;
#62648 = SURFACE_SIDE_STYLE ('',( #131967 ) ) ;
#62649 = CARTESIAN_POINT ( 'NONE',  ( -10.38819714233668456, 3.487142912321096855, -5.997628416522944761 ) ) ;
#62650 = VECTOR ( 'NONE', #41214, 1000.000000000000000 ) ;
#62651 = CARTESIAN_POINT ( 'NONE',  ( 5.014598762909163732, 0.8246402433861481640, 2.008555861535677778 ) ) ;
#62652 = CARTESIAN_POINT ( 'NONE',  ( 4.564971734551386717, -1.632036996880025903, -0.8184370388232551363 ) ) ;
#62653 = CARTESIAN_POINT ( 'NONE',  ( 1.586688997538304058, 1.889165970957426444, 0.5283831072378853966 ) ) ;
#62654 = CARTESIAN_POINT ( 'NONE',  ( -0.1056256405159265443, -0.9088113327815927622, -1.910082645617340757 ) ) ;
#62655 = VECTOR ( 'NONE', #5232, 1000.000000000000000 ) ;
#62656 = CARTESIAN_POINT ( 'NONE',  ( 1.364683531249990311, 3.946875000341417028, 1.214306433183764966E-14 ) ) ;
#62657 = CARTESIAN_POINT ( 'NONE',  ( 3.998178221199472748, 7.810824081292446763, -0.04219917931748625589 ) ) ;
#62658 = CARTESIAN_POINT ( 'NONE',  ( 8.101160479365381306, 9.410107633136481908, -1.199719254218446718 ) ) ;
#62659 = CARTESIAN_POINT ( 'NONE',  ( 3.071057173463411338, -1.604308532545582366, 1.386676294644908713 ) ) ;
#62660 = CARTESIAN_POINT ( 'NONE',  ( -4.338245966692955591, 5.124003718305597310, 1.082531754730560403 ) ) ;
#62661 = CARTESIAN_POINT ( 'NONE',  ( 6.034787771414189095, 6.213209619504255876, -0.7216878364870512597 ) ) ;
#62662 = CARTESIAN_POINT ( 'NONE',  ( -5.544921637864841379, 5.571422787038166291, -0.7216878364870197293 ) ) ;
#62663 = CARTESIAN_POINT ( 'NONE',  ( 0.4794554595633391814, -0.1051018081165492196, 2.067734805981166435 ) ) ;
#62665 = CARTESIAN_POINT ( 'NONE',  ( -0.7500000000000006661, 13.73958333401613352, -1.299038105676657340 ) ) ;
#62664 = CARTESIAN_POINT ( 'NONE',  ( 6.883263157960371359, 1.234153227268469877, 2.265917448979277271 ) ) ;
#62667 = EDGE_LOOP ( 'NONE', ( #5630, #37582, #14338, #131946 ) ) ;
#62666 = CARTESIAN_POINT ( 'NONE',  ( 2.737233380259511684, 2.092449130469396401, 0.7459289674271016857 ) ) ;
#62668 = CARTESIAN_POINT ( 'NONE',  ( 0.2296305240335142495, 2.293118238291039113, 0.1608910274224564507 ) ) ;
#62670 = CARTESIAN_POINT ( 'NONE',  ( 5.278211761479340680, -1.098870959053561469, -1.745292714083917174 ) ) ;
#62669 = CARTESIAN_POINT ( 'NONE',  ( 4.695201269034174452, 4.372156323494968966, 1.214306433183764966E-14 ) ) ;
#62672 = CARTESIAN_POINT ( 'NONE',  ( 3.475000000000000533, -1.545833333333334503, -2.006292185433951047 ) ) ;
#62671 = CARTESIAN_POINT ( 'NONE',  ( 4.532168488718122390, 8.509556680138327778, 0.7998128361456271485 ) ) ;
#62673 = CARTESIAN_POINT ( 'NONE',  ( 7.035755370848908896, 7.173079118937375931, 0.7998128361456352531 ) ) ;
#62674 = CARTESIAN_POINT ( 'NONE',  ( 0.2333540202161792088, 6.948072531064760859, -2.640811564931430766 ) ) ;
#62675 = CARTESIAN_POINT ( 'NONE',  ( 5.319803798718575116, 1.092037692397327620, -1.482314076171886708 ) ) ;
#62676 = CARTESIAN_POINT ( 'NONE',  ( 4.192495815123822744, 5.914331089109666983, -1.599625672291255185 ) ) ;
#62677 = CARTESIAN_POINT ( 'NONE',  ( 1.482971688208828187, 1.595641881047437538, -0.6553127101004208033 ) ) ;
#62678 = CARTESIAN_POINT ( 'NONE',  ( 0.6906390985809904848, 1.523792322931913468, -1.320830384837400118 ) ) ;
#62679 =( BOUNDED_CURVE ( )  B_SPLINE_CURVE ( 2, ( #51962, #21544, #171028, #19432, #201371, #53011, #203501, #56220, #153724, #118084, #202435, #5293, #4233, #72447, #167833, #71371, #70303, #119146, #155858, #85512, #151598, #137487, #39979, #86583, #55154, #152648, #136419, #121301, #6377, #106087, #187275, #38903, #104987, #22623, #88734, #208840, #111428, #125566, #8522, #160112, #57287, #124505, #95133, #205650, #75667, #173188, #156933, #61540, #76717, #161182, #141775, #93004, #9591, #191526, #174260, #108236, #60470, #190464, #193667, #159049, #41054, #123450, #107163, #59409, #175313, #139627, #143909, #207782, #176371, #42123, #43191, #189412, #25832, #94071, #24768, #91941, #29050, #73525, #158002, #110366, #177433, #11714, #109304, #58349, #126627, #45310, #26900, #10641, #142834, #192590, #140707, #206721, #77788, #90871, #74603, #27978, #127706, #44245, #209902, #31186, #48505, #212032, #62597, #63674, #79913, #762, #132972, #96201, #131912, #78843, #46371, #34362, #165433, #100435, #196867, #164375, #82043, #194733, #128759, #99380, #162250, #66829, #144963, #114625, #49549, #112490, #13837, #146020, #148137, #17029, #180615, #12768, #80989, #147078, #97259, #83106, #210969, #213099, #163313, #129828, #116744, #113562, #198974, #32240, #149187, #50619, #98311, #195810, #178500, #64729, #33296, #182744, #30110, #15960, #47446, #179565, #214138, #65766, #14895, #130872, #197921, #115674, #181669, #2906, #188083, #84185, #168635, #51704, #35427, #154535, #169704, #37573, #101505, #134045, #72185, #187016, #21294, #5038, #6115, #200055, #184871, #102575, #70041, #52751, #201111, #87399, #68978, #138293, #185938, #117827, #135097, #67901, #167575, #71114, #136157, #202174, #119963, #103653, #183817, #122118, #38649, #118885, #104727, #19174, #36497, #39712, #166506, #20238, #203252, #55966, #86323, #152395, #85248, #18097, #150273, #151337, #1842, #3974, #204309, #53832, #153465, #170775, #137231, #54895, #121049, #22364, #88476, #41875, #124257, #141530, #74353, #90620, #24509, #8270, #205395, #171847, #139364, #206469, #156677 ),
 .UNSPECIFIED., .F., .T. ) 
 B_SPLINE_CURVE_WITH_KNOTS ( ( 3, 2, 2, 2, 2, 2, 2, 2, 2, 2, 2, 2, 2, 2, 2, 2, 2, 2, 2, 2, 2, 2, 2, 2, 2, 2, 2, 2, 2, 2, 2, 2, 2, 2, 2, 2, 2, 2, 2, 2, 2, 2, 2, 2, 2, 2, 2, 2, 2, 2, 2, 2, 2, 2, 2, 2, 2, 2, 2, 2, 2, 2, 2, 2, 2, 2, 2, 2, 2, 2, 2, 2, 2, 2, 2, 2, 2, 2, 2, 2, 2, 2, 2, 2, 2, 2, 2, 2, 2, 2, 2, 2, 2, 2, 2, 2, 2, 2, 2, 2, 2, 2, 2, 2, 2, 2, 2, 2, 2, 2, 2, 2, 2, 2, 2, 2, 2, 2, 2, 3 ),
 ( 0.2923662209080201690, 0.2976190476190476164, 0.3035714285714285476, 0.3095238095238095344, 0.3154761904761904656, 0.3214285714285714524, 0.3273809523809523836, 0.3333333333333333148, 0.3392857142857143016, 0.3452380952380952328, 0.3511904761904761640, 0.3571428571428571508, 0.3630952380952380820, 0.3690476190476190688, 0.3750000000000000000, 0.3809523809523809312, 0.3869047619047619180, 0.3928571428571428492, 0.3988095238095238360, 0.4047619047619047672, 0.4107142857142856984, 0.4166666666666666852, 0.4226190476190476164, 0.4285714285714285476, 0.4345238095238095344, 0.4404761904761904656, 0.4464285714285714524, 0.4523809523809523836, 0.4583333333333333148, 0.4642857142857143016, 0.4702380952380952328, 0.4761904761904761640, 0.4821428571428571508, 0.4880952380952380820, 0.4940476190476190688, 0.5000000000000000000, 0.5059523809523809312, 0.5119047619047618625, 0.5178571428571429047, 0.5238095238095238360, 0.5297619047619047672, 0.5357142857142856984, 0.5416666666666666297, 0.5476190476190476719, 0.5535714285714286031, 0.5595238095238095344, 0.5654761904761904656, 0.5714285714285713969, 0.5773809523809523281, 0.5833333333333333703, 0.5892857142857143016, 0.5952380952380952328, 0.6011904761904761640, 0.6071428571428570953, 0.6130952380952381375, 0.6190476190476190688, 0.6250000000000000000, 0.6309523809523809312, 0.6369047619047618625, 0.6428571428571429047, 0.6488095238095238360, 0.6547619047619047672, 0.6607142857142856984, 0.6666666666666666297, 0.6726190476190476719, 0.6785714285714286031, 0.6845238095238095344, 0.6904761904761904656, 0.6964285714285713969, 0.7023809523809523281, 0.7083333333333333703, 0.7142857142857143016, 0.7202380952380953438, 0.7261904761904761640, 0.7321428571428570953, 0.7380952380952381375, 0.7440476190476190688, 0.7500000000000000000, 0.7559523809523809312, 0.7619047619047618625, 0.7678571428571430157, 0.7738095238095238360, 0.7797619047619047672, 0.7857142857142856984, 0.7916666666666666297, 0.7976190476190476719, 0.8035714285714286031, 0.8095238095238095344, 0.8154761904761904656, 0.8214285714285713969, 0.8273809523809523281, 0.8333333333333334814, 0.8392857142857144126, 0.8452380952380953438, 0.8511904761904762751, 0.8571428571428572063, 0.8630952380952381375, 0.8690476190476190688, 0.8750000000000000000, 0.8809523809523809312, 0.8869047619047618625, 0.8928571428571430157, 0.8988095238095239470, 0.9047619047619048782, 0.9107142857142858094, 0.9166666666666667407, 0.9226190476190476719, 0.9285714285714286031, 0.9345238095238095344, 0.9404761904761904656, 0.9464285714285713969, 0.9523809523809523281, 0.9583333333333334814, 0.9642857142857144126, 0.9702380952380953438, 0.9761904761904762751, 0.9821428571428572063, 0.9880952380952381375, 0.9940476190476190688, 1.000000000000000000 ),
 .UNSPECIFIED. ) 
 CURVE ( )  GEOMETRIC_REPRESENTATION_ITEM ( )  RATIONAL_B_SPLINE_CURVE ( ( 0.9722101959979289054, 0.8817707832831631620, 1.000000000000000000, 0.8660254037844387076, 1.000000000000000000, 0.8660254037844387076, 1.000000000000000000, 0.8660254037844387076, 1.000000000000000000, 0.8660254037844387076, 1.000000000000000000, 0.8660254037844387076, 1.000000000000000000, 0.8660254037844387076, 1.000000000000000000, 0.8660254037844387076, 1.000000000000000000, 0.8660254037844387076, 1.000000000000000000, 0.8660254037844387076, 1.000000000000000000, 0.8660254037844387076, 1.000000000000000000, 0.8660254037844387076, 1.000000000000000000, 0.8660254037844387076, 1.000000000000000000, 0.8660254037844387076, 1.000000000000000000, 0.8660254037844387076, 1.000000000000000000, 0.8660254037844387076, 1.000000000000000000, 0.8660254037844387076, 1.000000000000000000, 0.8660254037844387076, 1.000000000000000000, 0.8660254037844387076, 1.000000000000000000, 0.8660254037844387076, 1.000000000000000000, 0.8660254037844387076, 1.000000000000000000, 0.8660254037844387076, 1.000000000000000000, 0.8660254037844387076, 1.000000000000000000, 0.8660254037844387076, 1.000000000000000000, 0.8660254037844387076, 1.000000000000000000, 0.8660254037844387076, 1.000000000000000000, 0.8660254037844387076, 1.000000000000000000, 0.8660254037844387076, 1.000000000000000000, 0.8660254037844387076, 1.000000000000000000, 0.8660254037844387076, 1.000000000000000000, 0.8660254037844387076, 1.000000000000000000, 0.8660254037844387076, 1.000000000000000000, 0.8660254037844387076, 1.000000000000000000, 0.8660254037844387076, 1.000000000000000000, 0.8660254037844387076, 1.000000000000000000, 0.8660254037844387076, 1.000000000000000000, 0.8660254037844387076, 1.000000000000000000, 0.8660254037844387076, 1.000000000000000000, 0.8660254037844387076, 1.000000000000000000, 0.8660254037844387076, 1.000000000000000000, 0.8660254037844387076, 1.000000000000000000, 0.8660254037844387076, 1.000000000000000000, 0.8660254037844387076, 1.000000000000000000, 0.8660254037844387076, 1.000000000000000000, 0.8660254037844387076, 1.000000000000000000, 0.8660254037844387076, 1.000000000000000000, 0.8660254037844387076, 1.000000000000000000, 0.8660254037844387076, 1.000000000000000000, 0.8660254037844387076, 1.000000000000000000, 0.8660254037844387076, 1.000000000000000000, 0.8660254037844387076, 1.000000000000000000, 0.8660254037844387076, 1.000000000000000000, 0.8660254037844387076, 1.000000000000000000, 0.8660254037844387076, 1.000000000000000000, 0.8660254037844387076, 1.000000000000000000, 0.8660254037844387076, 1.000000000000000000, 0.8660254037844387076, 1.000000000000000000, 0.8660254037844387076, 1.000000000000000000, 0.8660254037844387076, 1.000000000000000000, 0.8660254037844387076, 1.000000000000000000, 0.8660254037844387076, 1.000000000000000000, 0.8660254037844387076, 1.000000000000000000, 0.8660254037844387076, 1.000000000000000000, 0.8660254037844387076, 1.000000000000000000, 0.8660254037844387076, 1.000000000000000000, 0.8660254037844387076, 1.000000000000000000, 0.8660254037844387076, 1.000000000000000000, 0.8660254037844387076, 1.000000000000000000, 0.8660254037844387076, 1.000000000000000000, 0.8660254037844387076, 1.000000000000000000, 0.8660254037844387076, 1.000000000000000000, 0.8660254037844387076, 1.000000000000000000, 0.8660254037844387076, 1.000000000000000000, 0.8660254037844387076, 1.000000000000000000, 0.8660254037844387076, 1.000000000000000000, 0.8660254037844387076, 1.000000000000000000, 0.8660254037844387076, 1.000000000000000000, 0.8660254037844387076, 1.000000000000000000, 0.8660254037844387076, 1.000000000000000000, 0.8660254037844387076, 1.000000000000000000, 0.8660254037844387076, 1.000000000000000000, 0.8660254037844387076, 1.000000000000000000, 0.8660254037844387076, 1.000000000000000000, 0.8660254037844387076, 1.000000000000000000, 0.8660254037844387076, 1.000000000000000000, 0.8660254037844387076, 1.000000000000000000, 0.8660254037844387076, 1.000000000000000000, 0.8660254037844387076, 1.000000000000000000, 0.8660254037844387076, 1.000000000000000000, 0.8660254037844387076, 1.000000000000000000, 0.8660254037844387076, 1.000000000000000000, 0.8660254037844387076, 1.000000000000000000, 0.8660254037844387076, 1.000000000000000000, 0.8660254037844387076, 1.000000000000000000, 0.8660254037844387076, 1.000000000000000000, 0.8660254037844387076, 1.000000000000000000, 0.8660254037844387076, 1.000000000000000000, 0.8660254037844387076, 1.000000000000000000, 0.8660254037844387076, 1.000000000000000000, 0.8660254037844387076, 1.000000000000000000, 0.8660254037844387076, 1.000000000000000000, 0.8660254037844387076, 1.000000000000000000, 0.8660254037844387076, 1.000000000000000000, 0.8660254037844387076, 1.000000000000000000, 0.8660254037844387076, 1.000000000000000000, 0.8660254037844387076, 1.000000000000000000, 0.8660254037844387076, 1.000000000000000000, 0.8660254037844387076, 1.000000000000000000, 0.8660254037844387076, 1.000000000000000000, 0.8660254037844387076, 1.000000000000000000, 0.8660254037844387076, 1.000000000000000000, 0.8660254037844387076, 1.000000000000000000, 0.8660254037844387076, 1.000000000000000000, 0.8660254037844387076, 1.000000000000000000, 0.8660254037844387076, 1.000000000000000000, 0.8660254037844387076, 1.000000000000000000, 0.8660254037844387076, 1.000000000000000000, 0.8660254037844387076, 1.000000000000000000, 0.8660254037844387076, 1.000000000000000000 ) ) 
 REPRESENTATION_ITEM ( '' )  );
#62680 = CARTESIAN_POINT ( 'NONE',  ( 2.303761666418477461, 1.498124540730429333, -1.743551778261544838 ) ) ;
#62681 = CARTESIAN_POINT ( 'NONE',  ( -1.364683531249997417, 4.571875000341417028, 1.214306433183764966E-14 ) ) ;
#62682 = CARTESIAN_POINT ( 'NONE',  ( 2.161739655719534081, 0.3883039046224411317, -2.228698702525088393 ) ) ;
#62683 = CARTESIAN_POINT ( 'NONE',  ( 3.633512520595981066, -1.945918672469678867, 0.8060524589711003385 ) ) ;
#62684 = CARTESIAN_POINT ( 'NONE',  ( -4.995253251992230581, 4.792493313604505367, 0.000000000000000000 ) ) ;
#62685 = CARTESIAN_POINT ( 'NONE',  ( 2.952157954411178675, 0.5926004979403748374, 1.667723606733088060 ) ) ;
#62686 = CARTESIAN_POINT ( 'NONE',  ( 5.066996723205273057, 6.934582148538044777, 1.599625672291267398 ) ) ;
#62688 = CARTESIAN_POINT ( 'NONE',  ( 5.706620831843001618, 2.020032061211772589, 1.083668233456626551 ) ) ;
#62687 = CARTESIAN_POINT ( 'NONE',  ( 5.989670002187236442, 10.20997511251894529, -0.7998128361456481317 ) ) ;
#62689 = CARTESIAN_POINT ( 'NONE',  ( 4.945164379994194448, 0.5744887182440976403, -1.749284230371531024 ) ) ;
#62690 = CARTESIAN_POINT ( 'NONE',  ( -5.274285450916075035, 6.112086766612214284, 1.199719254218450271 ) ) ;
#62691 = CARTESIAN_POINT ( 'NONE',  ( 4.622967192135525316, 8.337286124226029216, -0.7216878364870207285 ) ) ;
#62692 = CARTESIAN_POINT ( 'NONE',  ( -1.500000000000011324, 2.920833333333352932, 0.8660254037844403729 ) ) ;
#62693 = CARTESIAN_POINT ( 'NONE',  ( 4.119203469048302146, -2.097337170177868693, 0.6352863671069891582 ) ) ;
#62694 = CARTESIAN_POINT ( 'NONE',  ( -4.086893239515592136, 6.855460315155083251, 1.199719254218464037 ) ) ;
#62695 = CARTESIAN_POINT ( 'NONE',  ( 0.1081551476993989624, 7.159877756659379422, -1.998460492244654274 ) ) ;
#62696 = CARTESIAN_POINT ( 'NONE',  ( -11.86239285000045918, 9.719999999999998863, -1.812080536912752837 ) ) ;
#62697 = CARTESIAN_POINT ( 'NONE',  ( -0.6823417656250212460, 4.801041667008086655, 1.181850606188767472 ) ) ;
#62698 = CARTESIAN_POINT ( 'NONE',  ( 3.264201069286599477, 0.8669165009558920110, 1.720499056138290683 ) ) ;
#62699 = CARTESIAN_POINT ( 'NONE',  ( -1.364683531250000748, 8.609375000341396245, 0.000000000000000000 ) ) ;
#62700 = CARTESIAN_POINT ( 'NONE',  ( -4.446711195602252253, 6.210915699667823198, -1.443375672974053447 ) ) ;
#62701 = CARTESIAN_POINT ( 'NONE',  ( 5.660427296577901224, 2.118236611397010805, 0.1021076702828054988 ) ) ;
#62702 = CARTESIAN_POINT ( 'NONE',  ( -6.780486220610195680, 7.083191143566240910, -0.7216878364870338292 ) ) ;
#62703 = EDGE_LOOP ( 'NONE', ( #56254, #70105, #185472, #36987 ) ) ;
#62705 = DIRECTION ( 'NONE',  ( 3.491481338843133355E-15, 0.000000000000000000, 1.000000000000000000 ) ) ;
#62704 = CARTESIAN_POINT ( 'NONE',  ( -5.831415467653581430, 5.975941931783510519, 0.7216878364870257245 ) ) ;
#62706 = CARTESIAN_POINT ( 'NONE',  ( 4.487912541323413329, 5.194651705420806564, 1.199719254218462483 ) ) ;
#62707 = DIRECTION ( 'NONE',  ( 1.000000000000000000, -0.000000000000000000, -0.000000000000000000 ) ) ;
#62708 = DIRECTION ( 'NONE',  ( 0.000000000000000000, 1.000000000000000000, 0.000000000000000000 ) ) ;
#62709 = CARTESIAN_POINT ( 'NONE',  ( 0.3387147352624392815, 6.550290604319550347, -3.193285863367457900 ) ) ;
#62710 = CARTESIAN_POINT ( 'NONE',  ( 0.6823417656249899377, 4.238541667008085767, -1.181850606188754593 ) ) ;
#62711 = CARTESIAN_POINT ( 'NONE',  ( 2.208218529973245303, 1.555207145793806811, 0.7814158636046761863 ) ) ;
#62712 = CARTESIAN_POINT ( 'NONE',  ( -2.494940289813118994, 3.447199233515649386, 11.73777120880565583 ) ) ;
#62713 = CARTESIAN_POINT ( 'NONE',  ( 0.3968290921660848625, 0.3316028935436679537, 1.933473477243151439 ) ) ;
#62714 = CARTESIAN_POINT ( 'NONE',  ( 1.364683531249986537, -0.2822916663252520997, -0.7879004041258309554 ) ) ;
#62715 = CARTESIAN_POINT ( 'NONE',  ( 1.579999999999989413, 6.280000000000042881, 2.580000000000000515 ) ) ;
#62716 = CARTESIAN_POINT ( 'NONE',  ( 6.139563164240942506, -1.562336469324271837, -1.494251390645913613 ) ) ;
#62717 = CARTESIAN_POINT ( 'NONE',  ( -9.429859533504656000, 10.96025652963230534, -1.199719254218441611 ) ) ;
#62718 = CIRCLE ( 'NONE', #142250, 2.000000000000000000 ) ;
#62719 = CARTESIAN_POINT ( 'NONE',  ( -6.873620692004104527, 7.121571683533994168, 0.7216878364870317197 ) ) ;
#62720 = CARTESIAN_POINT ( 'NONE',  ( 5.454052192070485638, 2.159419290912270029, -0.1019294599445344784 ) ) ;
#62722 = VERTEX_POINT ( 'NONE', #195159 ) ;
#62721 = CARTESIAN_POINT ( 'NONE',  ( -9.029845422049838533, 1.720726420432414638, -7.609771484012884279 ) ) ;
#62723 = CARTESIAN_POINT ( 'NONE',  ( 1.364683531249988535, 4.155208333674753618, -0.7879004041258239610 ) ) ;
#62724 = CARTESIAN_POINT ( 'NONE',  ( 6.555938671473301227, 1.966215360770405818, -0.1428278144062731236 ) ) ;
#62725 = CARTESIAN_POINT ( 'NONE',  ( 6.397740202767369766, 0.1737558121157663782, 1.725068634017632885 ) ) ;
#62727 = CARTESIAN_POINT ( 'NONE',  ( 2.788834510562918645, 1.878274557074947948, -1.128960604485473862 ) ) ;
#62726 = CARTESIAN_POINT ( 'NONE',  ( -1.360316468750042862, -0.08854166632527044056, 0.7853790794158801436 ) ) ;
#62728 = CARTESIAN_POINT ( 'NONE',  ( 3.821538862543779391, -0.1730032229720068482, 2.301163704417693356 ) ) ;
#62729 = CARTESIAN_POINT ( 'NONE',  ( 5.940714679333914283, 0.3976391751681263576, 2.021873298595587176 ) ) ;
#62730 = CARTESIAN_POINT ( 'NONE',  ( 1.060374178334378303, -1.755330386401842802, -0.8309217204432550741 ) ) ;
#62731 = CARTESIAN_POINT ( 'NONE',  ( -7.361714222096077620, 7.691014135307965738, 0.7216878364870317197 ) ) ;
#62732 = PRODUCT_DEFINITION_SHAPE ( 'NONE', 'NONE',  #214430 ) ;
#62733 = CARTESIAN_POINT ( 'NONE',  ( -0.3080734816351294314, -8.169755926620753783, -9.495223711095173158 ) ) ;
#62734 = CARTESIAN_POINT ( 'NONE',  ( -1.214306433183764966E-14, 3.299999999999969624, -3.122502256758252770E-14 ) ) ;
#62735 = CARTESIAN_POINT ( 'NONE',  ( 3.990573222356631256, -1.218298518170106925, 1.735533685479621502 ) ) ;
#62736 = CARTESIAN_POINT ( 'NONE',  ( 2.408827471728996361, -1.163269702728772392, -1.646838680093346996 ) ) ;
#62737 = CARTESIAN_POINT ( 'NONE',  ( -5.165293336682207581, 8.009630745229104676, 1.082531754730548412 ) ) ;
#62738 = CARTESIAN_POINT ( 'NONE',  ( 4.120313900606538127, -1.131812998600056241, -1.894281110011143632 ) ) ;
#62739 = CARTESIAN_POINT ( 'NONE',  ( -4.650083499807267984, 5.295740330745369207, 1.164732466530402855 ) ) ;
#62740 = CARTESIAN_POINT ( 'NONE',  ( 0.3788956605885723250, 3.049042541176466337, -0.4283520265746156852 ) ) ;
#62741 = CARTESIAN_POINT ( 'NONE',  ( 0.3986991128735201673, 1.519733473351183362, -1.011397189243423700 ) ) ;
#62742 = CARTESIAN_POINT ( 'NONE',  ( -6.936931872047518155, 8.122117267924091166, 1.199719254218452047 ) ) ;
#62744 = CARTESIAN_POINT ( 'NONE',  ( 6.825078400183572036, 2.942104585519232263, 2.696255528691358982 ) ) ;
#62743 = CARTESIAN_POINT ( 'NONE',  ( -5.689102680971802606, 7.419971068449684459, 1.333831099742349480 ) ) ;
#62745 = DIRECTION ( 'NONE',  ( 0.000000000000000000, 0.000000000000000000, -1.000000000000000000 ) ) ;
#62746 = VERTEX_POINT ( 'NONE', #148542 ) ;
#62747 = CARTESIAN_POINT ( 'NONE',  ( 4.416905344109374632, 1.883477791879540231, 0.8369615876049685266 ) ) ;
#62748 = CARTESIAN_POINT ( 'NONE',  ( -0.6801582343750282034, 2.682291667008049441, 1.178068619123805227 ) ) ;
#62749 = FACE_OUTER_BOUND ( 'NONE', #208758, .T. ) ;
#62750 = CARTESIAN_POINT ( 'NONE',  ( -5.739179097286464248, 5.590130456455974617, -0.7998128361456221525 ) ) ;
#62751 = CARTESIAN_POINT ( 'NONE',  ( -3.305155586681401303, 7.078041627762083898, 0.7998128361456352531 ) ) ;
#62752 = CARTESIAN_POINT ( 'NONE',  ( 2.930336769707508893, -0.9972767022783147750, -1.756213584645490267 ) ) ;
#62753 = CARTESIAN_POINT ( 'NONE',  ( -0.7500000000000006661, 0.3583333333333563187, -1.299038105676652011 ) ) ;
#62755 = CARTESIAN_POINT ( 'NONE',  ( 7.429504990608736037, 11.61158022244479682, -0.7216878364870267237 ) ) ;
#62754 = CARTESIAN_POINT ( 'NONE',  ( -4.492547798081878874, 6.334668079219206049, 1.599625672291263179 ) ) ;
#62756 = CARTESIAN_POINT ( 'NONE',  ( 6.928380191783277908, 8.041863964290678624, 1.199719254218462483 ) ) ;
#62757 = CARTESIAN_POINT ( 'NONE',  ( 2.536071046656536598, 0.9725223524452746293, -1.817000187329747884 ) ) ;
#62758 = CARTESIAN_POINT ( 'NONE',  ( 2.901017702322743919, -0.9963018188003970321, -1.753030416019534021 ) ) ;
#62759 = CARTESIAN_POINT ( 'NONE',  ( -6.396834479292370368, -8.176568542494905500, -7.055228938194266775 ) ) ;
#62760 = CARTESIAN_POINT ( 'NONE',  ( 4.330940004561544043, 7.140181541042074365, -1.199719254218452047 ) ) ;
#62762 = ORIENTED_EDGE ( 'NONE', *, *, #175809, .F. ) ;
#62761 = CARTESIAN_POINT ( 'NONE',  ( -0.04711431077965874681, 7.150937050891459812, -2.000088718515178776 ) ) ;
#62763 = CARTESIAN_POINT ( 'NONE',  ( 3.181017370561005198, -0.9912469002804729090, -1.755500664876320727 ) ) ;
#62764 = CARTESIAN_POINT ( 'NONE',  ( 1.868857239601273923, 1.762127240619456803, -0.5335365013287919345 ) ) ;
#62765 = CARTESIAN_POINT ( 'NONE',  ( 6.656857027519620829, -1.708965229049699053, 1.396003577074665714 ) ) ;
#62766 = CARTESIAN_POINT ( 'NONE',  ( 5.306037014901791693, 7.283738832175834510, 1.599625672291269396 ) ) ;
#62767 = CARTESIAN_POINT ( 'NONE',  ( 2.214359598146302677, -1.016813397907929239, -1.907474440234189217 ) ) ;
#62768 = CARTESIAN_POINT ( 'NONE',  ( -4.785665035943912571, 4.685623418130398399, 1.214306433183764966E-14 ) ) ;
#62769 = CARTESIAN_POINT ( 'NONE',  ( 5.102788515576859751, 1.957488760995762300, 0.8075332785216599030 ) ) ;
#62770 = VECTOR ( 'NONE', #66041, 1000.000000000000000 ) ;
#62771 = ADVANCED_FACE ( 'NONE', ( #115030, #14237 ), #31596, .F. ) ;
#62772 = CARTESIAN_POINT ( 'NONE',  ( 4.232369794311310053E-13, -9.350066838357705024, 9.500000000000001776 ) ) ;
#62773 = CARTESIAN_POINT ( 'NONE',  ( 0.8834254411415434216, 1.253375741028007084, 1.388844808110502038 ) ) ;
#62774 =( BOUNDED_SURFACE ( )  B_SPLINE_SURFACE ( 3, 2, ( 
 ( #110397, #172140, #28007 ),
 ( #208869, #126659, #209935 ),
 ( #188367, #40007, #106117 ),
 ( #89838, #7475, #139659 ),
 ( #129859, #15990, #146050 ),
 ( #97291, #95165, #78874 ),
 ( #131944, #45342, #177467 ),
 ( #99410, #96231, #164406 ) ),
 .UNSPECIFIED., .F., .F., .T. ) 
 B_SPLINE_SURFACE_WITH_KNOTS ( ( 4, 2, 2, 4 ),
 ( 3, 3 ),
 ( -2.253405795293872416E-15, 0.003001918495467197773, 0.004502877743201923362, 0.006003836990936648951 ),
 ( 0.000000000000000000, 1.000000000000000000 ),
 .UNSPECIFIED. ) 
 GEOMETRIC_REPRESENTATION_ITEM ( )  RATIONAL_B_SPLINE_SURFACE ( (
 ( 1.000000000000000000, 0.7835651598521441441, 1.000000000000000000),
 ( 1.000000000000000000, 0.7913519369914218116, 1.000000000000000000),
 ( 1.000000000000000000, 0.8009496234832708117, 1.000000000000000000),
 ( 1.000000000000000000, 0.8230981486289181692, 1.000000000000000000),
 ( 1.000000000000000000, 0.8318333311020545962, 1.000000000000000000),
 ( 1.000000000000000000, 0.8529518727571846481, 1.000000000000000000),
 ( 1.000000000000000000, 0.8654984584228418987, 1.000000000000000000),
 ( 1.000000000000000000, 0.8789000212895415887, 1.000000000000000000) ) ) 
 REPRESENTATION_ITEM ( '' )  SURFACE ( )  );
#62775 = CARTESIAN_POINT ( 'NONE',  ( 5.489129097700779170, 1.738912991666073715, -0.9288780838571459864 ) ) ;
#62777 = CARTESIAN_POINT ( 'NONE',  ( 7.565086526301031178, 11.76975868075249387, 1.040834085586084257E-14 ) ) ;
#62776 = CARTESIAN_POINT ( 'NONE',  ( -1.364683531250012516, 3.238541667008084879, -0.7879004041258289570 ) ) ;
#62779 = CARTESIAN_POINT ( 'NONE',  ( 6.498663405296385420, -0.5599463640075187376, -2.030188946737851108 ) ) ;
#62778 = CARTESIAN_POINT ( 'NONE',  ( -7.223796917982883592, 7.322184580601816428, -0.7998128361456291469 ) ) ;
#62780 = CARTESIAN_POINT ( 'NONE',  ( 5.934052368846653991, 1.230181698326970885, 1.665117723180092213 ) ) ;
#62781 = CARTESIAN_POINT ( 'NONE',  ( 4.469384193999260901, 8.366031992974468423, -0.7998128361456231517 ) ) ;
#62782 = CARTESIAN_POINT ( 'NONE',  ( -6.226218857173722476, 8.287007971501239467, 1.599625672291283607 ) ) ;
#62783 = CARTESIAN_POINT ( 'NONE',  ( 6.639320575229281651, -0.0007625845807879281287, 2.103388539994067497 ) ) ;
#62784 = CARTESIAN_POINT ( 'NONE',  ( 4.821144081919094049, -0.09777198692111942202, 1.969167557456591666 ) ) ;
#62785 = CARTESIAN_POINT ( 'NONE',  ( 6.117445925308827803, 1.681535965833020230, 1.118592408852390641 ) ) ;
#62786 = CARTESIAN_POINT ( 'NONE',  ( -0.7500000000000006661, 0.6395833340161540814, -1.299038105676652011 ) ) ;
#62787 = CARTESIAN_POINT ( 'NONE',  ( 4.688248866636615553, -1.090845489383242883, 2.033590232148785759 ) ) ;
#62788 = EDGE_CURVE ( 'NONE', #166237, #87955, #104577, .T. ) ;
#62789 = CARTESIAN_POINT ( 'NONE',  ( 1.938405323705337135, -1.106995438288145950, 1.740174596247965555 ) ) ;
#62790 = CARTESIAN_POINT ( 'NONE',  ( 6.588899466561449536, 9.670504563421618016, -1.082531754730537088 ) ) ;
#62791 = CARTESIAN_POINT ( 'NONE',  ( 6.066347387471824781, 6.042103138330730872, -0.7998128361456481317 ) ) ;
#62792 = CARTESIAN_POINT ( 'NONE',  ( 4.115782150200256950, 6.959440387612411349, 1.199719254218452047 ) ) ;
#62793 = CARTESIAN_POINT ( 'NONE',  ( -1.364683531250000748, 2.321875000341422357, 1.214306433183764966E-14 ) ) ;
#62794 = CARTESIAN_POINT ( 'NONE',  ( 3.932747076415766596, 6.745899468197171345, 1.199719254218451159 ) ) ;
#62795 = CARTESIAN_POINT ( 'NONE',  ( 4.297571505407542958, 7.957657823043374989, -0.7216878364870197293 ) ) ;
#62796 = CARTESIAN_POINT ( 'NONE',  ( 4.176368576274028577, -1.112882343535037677, -1.864130199707826785 ) ) ;
#62797 = CARTESIAN_POINT ( 'NONE',  ( -2.880977623208980098, -0.8887487162373146621, -1.594386611912667284 ) ) ;
#62799 = CARTESIAN_POINT ( 'NONE',  ( 3.597050949361340511, -0.5310884314010614338, 1.763007376093472800 ) ) ;
#62798 = CARTESIAN_POINT ( 'NONE',  ( -4.338245966692955591, 5.124003718305597310, 1.082531754730560403 ) ) ;
#62800 = B_SPLINE_CURVE_WITH_KNOTS ( 'NONE', 3,
 ( #143885, #44221, #90844, #175291, #107138, #110344, #42098, #207759, #156908, #140682 ),
 .UNSPECIFIED., .F., .F.,
 ( 4, 3, 3, 4 ),
 ( 5.423634105407616645E-16, 3.125291908127631347E-05, 6.323748278266503285E-05, 9.524284239289069348E-05 ),
 .UNSPECIFIED. ) ;
#62802 = CARTESIAN_POINT ( 'NONE',  ( 6.620655732516647518, 7.053381450551401421, 2.424417106520880161 ) ) ;
#62801 = CARTESIAN_POINT ( 'NONE',  ( -0.6823417656250212460, 4.551041667008086655, 1.181850606188767472 ) ) ;
#62803 = CARTESIAN_POINT ( 'NONE',  ( 5.513277522340928272, -2.138352208816508782, 0.4792397250529822905 ) ) ;
#62804 = CARTESIAN_POINT ( 'NONE',  ( 4.067155351693835485E-15, 0.2500000006828133059, -1.225000000000014300 ) ) ;
#62805 = CARTESIAN_POINT ( 'NONE',  ( 5.647450836711301214, -1.779752484188871886, -1.396855495411459147 ) ) ;
#62806 = VERTEX_POINT ( 'NONE', #132320 ) ;
#62807 = CARTESIAN_POINT ( 'NONE',  ( -4.398207409718558836, 7.344456035913847103, -1.221965942340837552 ) ) ;
#62808 = CARTESIAN_POINT ( 'NONE',  ( 4.672271667806711548, 8.395315985019093930, 0.5582388282892002396 ) ) ;
#62809 = CARTESIAN_POINT ( 'NONE',  ( -4.462041952228942954, 8.219816354326809460, -0.7216878364870338292 ) ) ;
#62810 = CARTESIAN_POINT ( 'NONE',  ( -6.605500049835229426, -8.049367966558005349, -6.875062624577632064 ) ) ;
#62811 = CARTESIAN_POINT ( 'NONE',  ( 0.6722625022101048620, -1.664400848580146919, -0.6021564899992714048 ) ) ;
#62812 = VECTOR ( 'NONE', #35170, 1000.000000000000000 ) ;
#62813 = CARTESIAN_POINT ( 'NONE',  ( 4.811194018343159406, 1.672433887399711994, -1.120210643937557871 ) ) ;
#62814 = CARTESIAN_POINT ( 'NONE',  ( 6.602984505055297326, 7.662235663108029726, 1.199719254218462483 ) ) ;
#62815 = CARTESIAN_POINT ( 'NONE',  ( 4.489357033980984291, 1.882333632172785487, -0.9445240646021864084 ) ) ;
#62816 = CARTESIAN_POINT ( 'NONE',  ( 2.495587842290597713, -1.894396863028270594, 0.2834604161582406356 ) ) ;
#62818 = EDGE_CURVE ( 'NONE', #50089, #126346, #116085, .T. ) ;
#62817 = CARTESIAN_POINT ( 'NONE',  ( 4.142179624174931796, 4.791296635414242111, 1.199719254218464037 ) ) ;
#62819 = CARTESIAN_POINT ( 'NONE',  ( 2.910559396907284047, 0.6610699718948702674, 1.855445417178583911 ) ) ;
#62820 = CARTESIAN_POINT ( 'NONE',  ( 5.273696820376614802, 0.3899264243738297941, -1.981607871481812833 ) ) ;
#62821 = CARTESIAN_POINT ( 'NONE',  ( 1.463515404423965105, 1.843522461416190250, -0.3164952454337774390 ) ) ;
#62822 = CARTESIAN_POINT ( 'NONE',  ( 2.049198471137442912, 1.708465938063120637, -0.9642302061752603404 ) ) ;
#62825 = VERTEX_POINT ( 'NONE', #33707 ) ;
#62824 = CARTESIAN_POINT ( 'NONE',  ( 1.037202349414727109, -0.04413313863061394532, 1.912034500058952036 ) ) ;
#62823 = CARTESIAN_POINT ( 'NONE',  ( 3.457353000975535551, 0.4177302890290990889, -1.673392258113172382 ) ) ;
#62827 = CARTESIAN_POINT ( 'NONE',  ( 4.934804725694211136, 6.780358151441803649, -1.443375672974051449 ) ) ;
#62826 = CARTESIAN_POINT ( 'NONE',  ( 1.278255639411193245, 1.316999024263129092, 1.770685722221450709 ) ) ;
#62828 = CARTESIAN_POINT ( 'NONE',  ( -1.201851678989727383E-14, 1.884375000341422135, 1.575800808251672791 ) ) ;
#62829 = CARTESIAN_POINT ( 'NONE',  ( 8.751951852821344247, 10.16936423550178503, -1.199719254218446718 ) ) ;
#62830 = CARTESIAN_POINT ( 'NONE',  ( 11.35573736746281348, 12.48729585586717761, -3.554362808847921773 ) ) ;
#62831 = CARTESIAN_POINT ( 'NONE',  ( -6.471393748265563239, 5.229711127717889596, 2.419999999999998597 ) ) ;
#62832 = CARTESIAN_POINT ( 'NONE',  ( 1.250000000000037526, 8.500000000000000000, -12.00100000000000122 ) ) ;
#62833 = CARTESIAN_POINT ( 'NONE',  ( 6.965700764728601335, -0.4599482372066622249, 2.025938098699997525 ) ) ;
#62834 = CARTESIAN_POINT ( 'NONE',  ( 1.258353326579707776, -2.070544811992577561, -0.001879966208345739808 ) ) ;
#62835 = CARTESIAN_POINT ( 'NONE',  ( -1.402160292154681736E-14, 1.587500000000018785, -1.732050807568863648 ) ) ;
#62836 = CARTESIAN_POINT ( 'NONE',  ( 5.124091990960999432, 8.065525525174782828, -1.199719254218452047 ) ) ;
#62837 = CARTESIAN_POINT ( 'NONE',  ( -7.771848369131641121, 10.09024240211882351, -1.599625672291263179 ) ) ;
#62838 = CARTESIAN_POINT ( 'NONE',  ( 6.540882763950133238, 6.595727744222092959, 0.000000000000000000 ) ) ;
#62840 = EDGE_CURVE ( 'NONE', #166319, #36647, #142637, .T. ) ;
#62839 = CARTESIAN_POINT ( 'NONE',  ( 5.742871283745087041, 2.043606947765171267, 0.5656136300068030920 ) ) ;
#62841 = CARTESIAN_POINT ( 'NONE',  ( 3.400062661977048428, 7.188766548940353829, -1.734723475976807094E-15 ) ) ;
#62842 = CARTESIAN_POINT ( 'NONE',  ( -1.364683531250014514, 1.988541667008086655, -0.7879004041258289570 ) ) ;
#62843 = EDGE_CURVE ( 'NONE', #162782, #192662, #22799, .T. ) ;
#62844 = CARTESIAN_POINT ( 'NONE',  ( 0.7499999999999902300, 3.233333333333352044, 1.299038105676669330 ) ) ;
#62846 = CARTESIAN_POINT ( 'NONE',  ( 8.595506201383999567, 12.97191496834930113, 0.7216878364870438212 ) ) ;
#62845 = CARTESIAN_POINT ( 'NONE',  ( 6.144970055084349347, -0.2864424343173576082, -1.940704187532462210 ) ) ;
#62847 = CARTESIAN_POINT ( 'NONE',  ( 4.569685373303983944, 1.560260980002409870, -1.276848140101802365 ) ) ;
#62848 = CARTESIAN_POINT ( 'NONE',  ( 3.344859342474030939, -1.692025585574646662, -0.8982749641134063490 ) ) ;
#62849 = CARTESIAN_POINT ( 'NONE',  ( 1.611130907606239004, -0.2639259086049255965, 2.175532687872412829 ) ) ;
#62850 = CARTESIAN_POINT ( 'NONE',  ( -11.07124251632621537, 11.29999999999999716, -0.8054525327832626758 ) ) ;
#62851 = CARTESIAN_POINT ( 'NONE',  ( -0.7500000000000006661, 0.6395833340161540814, -1.299038105676652011 ) ) ;
#62852 = CARTESIAN_POINT ( 'NONE',  ( 4.799092303436800933, -0.2508153390233992530, -1.997484173059483892 ) ) ;
#62853 = CARTESIAN_POINT ( 'NONE',  ( -7.867809214632013770, 8.073532260025807261, 1.040834085586084257E-14 ) ) ;
#62854 = CARTESIAN_POINT ( 'NONE',  ( 5.958642064211575828, -2.010625215935774257, -0.6636248059145292144 ) ) ;
#62856 = CARTESIAN_POINT ( 'NONE',  ( -6.851666526859749418, 9.086973262793417661, -1.599625672291271394 ) ) ;
#62855 = CARTESIAN_POINT ( 'NONE',  ( 3.263305109790759939, 2.039240668410980284, -0.4604351538632973639 ) ) ;
#62858 = EDGE_LOOP ( 'NONE', ( #139635, #210844, #88485, #170784, #112955, #173895, #43996 ) ) ;
#62857 = CARTESIAN_POINT ( 'NONE',  ( 1.693959787788183347, -1.716010565565774915, -0.1736237626131422462 ) ) ;
#62859 = CARTESIAN_POINT ( 'NONE',  ( 4.939744792934912532, -2.012803497507459127, 0.6676120485993168874 ) ) ;
#62860 = CARTESIAN_POINT ( 'NONE',  ( 5.015626762051672571, 7.938982758113895422, 1.199719254218462483 ) ) ;
#62861 = CYLINDRICAL_SURFACE ( 'NONE', #2101, 0.3999999999999997446 ) ;
#62862 = CARTESIAN_POINT ( 'NONE',  ( 7.806953216197655365, -6.479141885268318468, 7.749822179018618584 ) ) ;
#62863 = FILL_AREA_STYLE ('',( #212300 ) ) ;
#62864 = CARTESIAN_POINT ( 'NONE',  ( 5.469824908109481854, 8.468880595181346393, -1.199719254218446718 ) ) ;
#62865 = ORIENTED_EDGE ( 'NONE', *, *, #98111, .T. ) ;
#62866 = DIRECTION ( 'NONE',  ( -0.000000000000000000, -1.000000000000000000, -0.000000000000000000 ) ) ;
#62868 = CARTESIAN_POINT ( 'NONE',  ( 1.312835156398382885, 1.481033882128342194, -1.042734985588577468 ) ) ;
#62867 = CARTESIAN_POINT ( 'NONE',  ( 4.854701522145073334, 7.821512988214679218, -1.199719254218450271 ) ) ;
#62869 = CARTESIAN_POINT ( 'NONE',  ( -6.073162743917628781, 9.172774736957510555, -1.199719254218440723 ) ) ;
#62870 = ORIENTED_EDGE ( 'NONE', *, *, #90474, .T. ) ;
#62871 = CARTESIAN_POINT ( 'NONE',  ( 4.487912541323413329, 5.194651705420806564, 1.199719254218462483 ) ) ;
#62872 = ORIENTED_EDGE ( 'NONE', *, *, #124338, .F. ) ;
#62873 = CARTESIAN_POINT ( 'NONE',  ( 6.574778147984297938, 6.635272358928617997, -0.7998128361456481317 ) ) ;
#62874 = CARTESIAN_POINT ( 'NONE',  ( 2.332397652471474903, 1.182373381703984094, -1.372477691862858729 ) ) ;
#62875 = CARTESIAN_POINT ( 'NONE',  ( 0.4340096093344653627, 3.713252088577059684, -0.4851708347456812898 ) ) ;
#62876 = CARTESIAN_POINT ( 'NONE',  ( 1.499999999999993117, 9.135416667349462116, 0.8660254037844408170 ) ) ;
#62877 = CARTESIAN_POINT ( 'NONE',  ( 4.113906668039927439, 7.442175195026684342, 0.6721147198667943856 ) ) ;
#62878 = EDGE_LOOP ( 'NONE', ( #172630, #24222, #185088, #198284, #84076 ) ) ;
#62879 = CARTESIAN_POINT ( 'NONE',  ( 3.455356687279837136, 1.465577529964179115, 1.146850193174092203 ) ) ;
#62880 = CARTESIAN_POINT ( 'NONE',  ( 1.036581048048822673, -1.509151586612084373, 1.179680973199858318 ) ) ;
#62881 = CARTESIAN_POINT ( 'NONE',  ( 0.2174332111963481196, -1.791455004416471430, 0.3504355335035569396 ) ) ;
#62882 = CARTESIAN_POINT ( 'NONE',  ( 1.492698588115513703, 4.434522803406307112, -0.1666886929329614297 ) ) ;
#62883 = FACE_OUTER_BOUND ( 'NONE', #6336, .T. ) ;
#62884 = CARTESIAN_POINT ( 'NONE',  ( 4.666668778386947380, 8.284408874816399759, 0.5204741841226891985 ) ) ;
#62885 = DIRECTION ( 'NONE',  ( -0.000000000000000000, 1.000000000000000000, -0.000000000000000000 ) ) ;
#62886 = CARTESIAN_POINT ( 'NONE',  ( -4.446711195602264688, 4.290177271065136466, -0.7216878364870207285 ) ) ;
#62887 = CARTESIAN_POINT ( 'NONE',  ( 6.914295153289432783, 10.05013286460426691, -1.082531754730537976 ) ) ;
#62888 = CARTESIAN_POINT ( 'NONE',  ( 4.293777937636614972, -1.355062202172536034, -1.429424366026492033 ) ) ;
#62889 = B_SPLINE_CURVE_WITH_KNOTS ( 'NONE', 3,
 ( #147949, #65583, #78662, #211856, #97084, #48329 ),
 .UNSPECIFIED., .F., .F.,
 ( 4, 2, 4 ),
 ( 0.000000000000000000, 0.0003168911866439334075, 0.0006337823732878668150 ),
 .UNSPECIFIED. ) ;
#62890 = CARTESIAN_POINT ( 'NONE',  ( -5.590039407536138150, 5.416134151747256986, 0.000000000000000000 ) ) ;
#62891 = DIRECTION ( 'NONE',  ( 0.000000000000000000, 1.000000000000000000, 0.000000000000000000 ) ) ;
#62892 = CARTESIAN_POINT ( 'NONE',  ( 0.6211766780156646739, -1.984520161701831986, 0.6578015034230285663 ) ) ;
#62893 = CARTESIAN_POINT ( 'NONE',  ( -2.788906526875773208E-15, 9.968750000682797818, -1.499999999999998446 ) ) ;
#62894 = CARTESIAN_POINT ( 'NONE',  ( 5.491212607897098863, 1.698784202212012762, -0.9083314536618128932 ) ) ;
#62895 = CARTESIAN_POINT ( 'NONE',  ( -7.019370843573183194, 9.212351955633947043, 1.599625672291283607 ) ) ;
#62896 = CARTESIAN_POINT ( 'NONE',  ( 1.500715674837904468, 1.494693011815557693, -1.047886037138339166 ) ) ;
#62897 = CARTESIAN_POINT ( 'NONE',  ( 2.438337523484556790, 1.039148161723329578, -1.946916322307743252 ) ) ;
#62898 = CARTESIAN_POINT ( 'NONE',  ( -6.249896535389937391, 6.922618705386589077, 0.8105719012266124901 ) ) ;
#62899 = CARTESIAN_POINT ( 'NONE',  ( 0.4043728756845180183, -1.898191424145349471, -0.2318213773434482650 ) ) ;
#62900 = EDGE_LOOP ( 'NONE', ( #184608, #74311, #47718, #142983 ) ) ;
#62901 = ORIENTED_EDGE ( 'NONE', *, *, #50156, .T. ) ;
#62902 = CARTESIAN_POINT ( 'NONE',  ( 0.1683113222354900018, -0.8393015767643360325, -1.780324559216818425 ) ) ;
#62903 = CARTESIAN_POINT ( 'NONE',  ( 1.399837892970667630, -0.7005499098489911258, -1.811468074468420841 ) ) ;
#62904 = CARTESIAN_POINT ( 'NONE',  ( 1.194685229111978497, -1.276845315561925931, -1.560263297373874813 ) ) ;
#62906 = CARTESIAN_POINT ( 'NONE',  ( 5.664867498354182018, 1.410286671683948168, -1.214315750818369510 ) ) ;
#62905 = CARTESIAN_POINT ( 'NONE',  ( -5.794130544993808307, 7.853181283949808744, 1.599625672291263179 ) ) ;
#62907 = CARTESIAN_POINT ( 'NONE',  ( 5.091969210384201361, 8.098325291160362482, 1.199719254218452047 ) ) ;
#62908 = DIRECTION ( 'NONE',  ( 1.000000000000000000, -0.000000000000000000, -0.000000000000000000 ) ) ;
#62909 = CARTESIAN_POINT ( 'NONE',  ( 2.021340551328831836, -3.221904128336454264E-15, -0.2879360613984097150 ) ) ;
#62910 = CARTESIAN_POINT ( 'NONE',  ( -5.739179097286464248, 5.590130456455974617, -0.7998128361456221525 ) ) ;
#62911 = ADVANCED_FACE ( 'NONE', ( #113978 ), #28498, .T. ) ;
#62912 = CARTESIAN_POINT ( 'NONE',  ( -6.343235766347277149, 8.493804042195527870, -1.599625672291271394 ) ) ;
#62913 = CARTESIAN_POINT ( 'NONE',  ( 1.382659466718983543, -0.3261178763579902218, -2.167053615394160637 ) ) ;
#62914 = CARTESIAN_POINT ( 'NONE',  ( 3.660338286009610975, 6.253849852777763729, -1.082531754730543083 ) ) ;
#62915 = AXIS2_PLACEMENT_3D ( 'NONE', #160490, #78165, #46764 ) ;
#62916 = CYLINDRICAL_SURFACE ( 'NONE', #70747, 0.08000000000000020983 ) ;
#62917 = CARTESIAN_POINT ( 'NONE',  ( -5.265089941164633594E-14, 3.949999999999961542, 1.829047314007895997 ) ) ;
#62918 = CARTESIAN_POINT ( 'NONE',  ( 1.400715809426569702, 1.493624456287694358, -1.049586478250638999 ) ) ;
#62919 = CARTESIAN_POINT ( 'NONE',  ( -4.647747731386360215, 4.316793862905830892, 0.7998128361456341429 ) ) ;
#62920 = CARTESIAN_POINT ( 'NONE',  ( -2.578021764892882040, 6.159442492350315490, 0.7998128361456341429 ) ) ;
#62921 = CARTESIAN_POINT ( 'NONE',  ( -6.489832820117282353, 6.840411167308092288, -0.6218019135817691723 ) ) ;
#62922 = CARTESIAN_POINT ( 'NONE',  ( 6.609000000000038177, 0.002801690667396730672, 2.000160786441218530 ) ) ;
#62923 = CARTESIAN_POINT ( 'NONE',  ( 10.40318394038753702, 11.03146944007395724, -0.7998128361456281477 ) ) ;
#62924 = CARTESIAN_POINT ( 'NONE',  ( 1.049297559255836010, -1.518254527582623359, -1.185787014772927916 ) ) ;
#62925 = CARTESIAN_POINT ( 'NONE',  ( 6.034033239799157400, 1.165729394902741189, 1.577711426528668692 ) ) ;
#62926 = VECTOR ( 'NONE', #36774, 1000.000000000000000 ) ;
#62927 = CARTESIAN_POINT ( 'NONE',  ( -7.934546212495630968, 10.28005655271014795, -1.599625672291263179 ) ) ;
#62928 = CARTESIAN_POINT ( 'NONE',  ( 6.010342169559767633, 5.906487374108181143, -0.7998128361456281477 ) ) ;
#62929 = CARTESIAN_POINT ( 'NONE',  ( 4.827760788416924242, 1.126602223531171898, -1.879657820484957664 ) ) ;
#62930 = EDGE_CURVE ( 'NONE', #95923, #61752, #173862, .T. ) ;
#62931 = CARTESIAN_POINT ( 'NONE',  ( 4.847203612085560387, 5.613824621309978724, -1.199719254218452047 ) ) ;
#62932 = CARTESIAN_POINT ( 'NONE',  ( 3.748938768049938197, -0.3990674421511587466, -2.031259957477090428 ) ) ;
#62934 = CARTESIAN_POINT ( 'NONE',  ( 0.6823417656249882723, 1.738541667008083991, -1.181850606188749264 ) ) ;
#62933 = DIRECTION ( 'NONE',  ( 0.000000000000000000, 0.000000000000000000, -1.000000000000000000 ) ) ;
#62935 = EDGE_LOOP ( 'NONE', ( #112309, #92282, #102310 ) ) ;
#62936 = CARTESIAN_POINT ( 'NONE',  ( 3.955939753277417648, -2.145046849925678956, -0.8267234532119535073 ) ) ;
#62938 = ORIENTED_EDGE ( 'NONE', *, *, #58624, .T. ) ;
#62937 = CARTESIAN_POINT ( 'NONE',  ( 8.107412671292042461, 9.521364873671299023, 1.082531754730558626 ) ) ;
#62940 = CARTESIAN_POINT ( 'NONE',  ( 3.285556943749998737, -0.2552083328553768071, -1.896917185911906500 ) ) ;
#62939 = CARTESIAN_POINT ( 'NONE',  ( 5.045042558060919724, 8.899983727797476263, -0.7216878364870458196 ) ) ;
#62941 = CARTESIAN_POINT ( 'NONE',  ( 6.620655732516668834, 7.629137130509086262, 2.526260288887293814 ) ) ;
#62942 = CARTESIAN_POINT ( 'NONE',  ( 3.872937777176552299, 1.828215432968218535, -0.6551730591081408317 ) ) ;
#62943 = VERTEX_POINT ( 'NONE', #185279 ) ;
#62944 = CARTESIAN_POINT ( 'NONE',  ( -11.37385970535894231, 1.000000000000000888, 3.825613075418397457 ) ) ;
#62945 = CARTESIAN_POINT ( 'NONE',  ( 5.326388512780113160, -0.8654452107222168067, -1.705464787417856787 ) ) ;
#62946 = DIRECTION ( 'NONE',  ( -0.6507913734559641616, -0.7592566023653004592, 0.000000000000000000 ) ) ;
#62947 = CARTESIAN_POINT ( 'NONE',  ( 6.809587843971872445, -0.3681478646948634914, 1.690922663601742038 ) ) ;
#62948 = CARTESIAN_POINT ( 'NONE',  ( 4.171111447311355747, 1.799123655847803205, -0.9110083886025857058 ) ) ;
#62949 = CARTESIAN_POINT ( 'NONE',  ( 0.4019237886466778820, 11.07366454968463110, 1.500000000000001554 ) ) ;
#62950 = CARTESIAN_POINT ( 'NONE',  ( 0.6630615684519860498, -1.595754342771567025, 1.524677653706180802 ) ) ;
#62952 = CARTESIAN_POINT ( 'NONE',  ( -4.285785955695645910, 7.053815144069948140, 1.082531754730549967 ) ) ;
#62951 = CARTESIAN_POINT ( 'NONE',  ( -8.455481356417053007, 13.01647868246193518, 0.7998128361456341429 ) ) ;
#62954 = CARTESIAN_POINT ( 'NONE',  ( 6.591055360535956531, 1.538344802651976373, -0.8746889052434738687 ) ) ;
#62953 = CARTESIAN_POINT ( 'NONE',  ( 0.07627643479381736313, -2.028408900457449704, -0.5058713263092640133 ) ) ;
#62955 = CARTESIAN_POINT ( 'NONE',  ( 5.432267593368638181, -1.591316862017605471, -1.238322901282742805 ) ) ;
#62957 = CARTESIAN_POINT ( 'NONE',  ( 3.574455624386526420, -2.209025962754256334, -0.6118928016028857275 ) ) ;
#62956 = CARTESIAN_POINT ( 'NONE',  ( 5.224688093219824303, 7.188831756880171397, -1.599625672291283607 ) ) ;
#62958 = CARTESIAN_POINT ( 'NONE',  ( 0.9193797689642355664, 1.039780534333001771, -1.395406566618085709 ) ) ;
#62959 = DIRECTION ( 'NONE',  ( 1.039099362110107450E-15, 1.000000000000000000, -4.583713267641621330E-32 ) ) ;
#62960 = CARTESIAN_POINT ( 'NONE',  ( 1.369977976685434751, -0.4280273037657927881, 1.680018549819038531 ) ) ;
#62961 = CARTESIAN_POINT ( 'NONE',  ( -0.6801582343750177673, 0.9635416670080582113, 1.178068619123796568 ) ) ;
#62962 = CARTESIAN_POINT ( 'NONE',  ( -1.833030277982346634, 9.001999999999998892, -2.499999999999998668 ) ) ;
#62963 = CARTESIAN_POINT ( 'NONE',  ( 1.733130889747940495, -2.061367544037566280, -0.6818780404978814769 ) ) ;
#62964 = CARTESIAN_POINT ( 'NONE',  ( 2.044158018538293042, 0.8666093899718421145, 1.820985203412978093 ) ) ;
#62965 = CARTESIAN_POINT ( 'NONE',  ( 4.406250000000002665, 1.895863743163984649, -0.7852924748302168023 ) ) ;
#62966 = MECHANICAL_DESIGN_GEOMETRIC_PRESENTATION_REPRESENTATION (  '', ( #146024 ), #187434 ) ;
#62967 = CARTESIAN_POINT ( 'NONE',  ( -0.7500000000000215383, 0.9729166673494854534, 1.299038105676659116 ) ) ;
#62968 = CARTESIAN_POINT ( 'NONE',  ( 6.076777883369302913, -1.830186849185039044, -0.6017253874085000120 ) ) ;
#62969 = CARTESIAN_POINT ( 'NONE',  ( 0.6823417656249934904, 12.94270833367473017, 1.181850606188764807 ) ) ;
#62970 = CARTESIAN_POINT ( 'NONE',  ( 3.463320643641348173, -1.814240386431978713, 1.281607931980492054 ) ) ;
#62971 = VERTEX_POINT ( 'NONE', #105137 ) ;
#62972 = CARTESIAN_POINT ( 'NONE',  ( 7.664830294503436114, -9.999999999999994671, -7.777967379493309075 ) ) ;
#62973 = CARTESIAN_POINT ( 'NONE',  ( 1.438959988998140160E-15, 4.000000000000003553, 11.50000000000000000 ) ) ;
#62974 = CARTESIAN_POINT ( 'NONE',  ( 7.404724451357931336, 11.79059562655963056, 0.7998128361456462443 ) ) ;
#62975 = CARTESIAN_POINT ( 'NONE',  ( 6.983858524370782028, 8.280828045588322084, 1.082531754730549967 ) ) ;
#62976 = DIRECTION ( 'NONE',  ( 1.000000000000000000, -0.000000000000000000, -0.000000000000000000 ) ) ;
#62977 = CARTESIAN_POINT ( 'NONE',  ( 5.267066465580821699, 1.675244640197434798, -0.4716337365339871579 ) ) ;
#62978 = CARTESIAN_POINT ( 'NONE',  ( 3.719154087244529894, -1.729071306366702476, -0.9269775827704658244 ) ) ;
#62980 = CARTESIAN_POINT ( 'NONE',  ( -6.738039156311804945, 6.963393225226301553, 1.040834085586084257E-14 ) ) ;
#62979 = CARTESIAN_POINT ( 'NONE',  ( 3.708318708537623021, 4.285125567170706695, -1.199719254218446718 ) ) ;
#62981 = EDGE_CURVE ( 'NONE', #19391, #208229, #105319, .T. ) ;
#62982 = CARTESIAN_POINT ( 'NONE',  ( -1.300105796840246519, 4.107110749520949788, 0.4336863642760122040 ) ) ;
#62983 = CARTESIAN_POINT ( 'NONE',  ( 4.077597889297270406, 2.132052650593726728, -0.7572755323067262845 ) ) ;
#62984 = CARTESIAN_POINT ( 'NONE',  ( 1.662626038903247228, -0.7403543059694576156, -1.925410787417888958 ) ) ;
#62985 = CARTESIAN_POINT ( 'NONE',  ( -6.856673000209188906, 9.022537805042615489, 1.599625672291283607 ) ) ;
#62986 = CARTESIAN_POINT ( 'NONE',  ( 2.870297354751516039, 1.209492683862042339, 1.911920897162355582 ) ) ;
#62987 = ORIENTED_EDGE ( 'NONE', *, *, #180163, .F. ) ;
#62988 = CARTESIAN_POINT ( 'NONE',  ( 1.499999999999987121, 0.7854166673494828999, 0.8660254037844524744 ) ) ;
#62989 = CARTESIAN_POINT ( 'NONE',  ( 3.725732288501612199, -1.111853074318921664, -1.504101509696729400 ) ) ;
#62990 = CARTESIAN_POINT ( 'NONE',  ( 2.232704217388951751, 1.733830997258398066, 0.04099941454244887540 ) ) ;
#62991 = CARTESIAN_POINT ( 'NONE',  ( 6.075747529084263299, -1.173811750163206158, 1.850510016281024850 ) ) ;
#62992 = CARTESIAN_POINT ( 'NONE',  ( 6.791963826450252206, -0.9943653912195188349, 2.080009744879149913 ) ) ;
#62993 = CARTESIAN_POINT ( 'NONE',  ( 4.399409362686744096, 1.734418756986338295, 1.290045131933370781 ) ) ;
#62994 = CARTESIAN_POINT ( 'NONE',  ( 4.751864635371732426, 0.7446896046985322926, 1.793680106537680174 ) ) ;
#62995 = CARTESIAN_POINT ( 'NONE',  ( -4.406036734316906234, 4.242723732898890709, -0.7216878364870207285 ) ) ;
#62997 = UNCERTAINTY_MEASURE_WITH_UNIT (LENGTH_MEASURE( 1.000000000000000082E-05 ), #177344, 'distance_accuracy_value', 'NONE');
#62996 = CARTESIAN_POINT ( 'NONE',  ( 6.919227945209173392, -0.1346273106918663420, 1.840389347376285345 ) ) ;
#62998 = CARTESIAN_POINT ( 'NONE',  ( 4.052428274714076295, 7.522979123003127988, 0.4826459875755910733 ) ) ;
#62999 = DIRECTION ( 'NONE',  ( -1.276756478318932191E-15, 1.000000000000000000, -3.330669073875483426E-16 ) ) ;
#63000 = CARTESIAN_POINT ( 'NONE',  ( 4.014622883422321209, 5.777089012116397804, -1.443375672974068769 ) ) ;
#63001 = CARTESIAN_POINT ( 'NONE',  ( -2.353626204688216217E-14, 2.453125000341405570, 1.570758158831792262 ) ) ;
#63002 = CARTESIAN_POINT ( 'NONE',  ( 6.082657761774013849, -0.6767167302549759178, 1.899617564980569995 ) ) ;
#63003 = CARTESIAN_POINT ( 'NONE',  ( -10.47775378526269918, 11.11846759242831872, -0.7998128361456221525 ) ) ;
#63004 = CARTESIAN_POINT ( 'NONE',  ( 7.934546212495622086, 10.28005655271014795, -1.599625672291262513 ) ) ;
#63005 = APPLICATION_CONTEXT ( 'automotive_design' ) ;
#63006 = DIRECTION ( 'NONE',  ( 0.3162277660168376636, 0.9486832980505138790, 0.000000000000000000 ) ) ;
#63007 = CARTESIAN_POINT ( 'NONE',  ( 3.492628380820805400, -0.3572889717703279788, -1.790209119249221548 ) ) ;
#63008 = CARTESIAN_POINT ( 'NONE',  ( -0.1296875068447916890, 6.948706544289747988, -2.421546651465163347 ) ) ;
#63009 = ORIENTED_EDGE ( 'NONE', *, *, #84492, .F. ) ;
#63010 = CARTESIAN_POINT ( 'NONE',  ( -5.438229012412903352, 6.477593614970734492, -1.082531754730549967 ) ) ;
#63011 = DIRECTION ( 'NONE',  ( 0.000000000000000000, 0.000000000000000000, 1.000000000000000000 ) ) ;
#63012 = CARTESIAN_POINT ( 'NONE',  ( -7.751511138711140170, 10.06651563329490529, -1.599625672291263179 ) ) ;
#63013 = CARTESIAN_POINT ( 'NONE',  ( 0.2815179179852530522, 0.1935487615560542163, -2.010460980806235920 ) ) ;
#63014 = CARTESIAN_POINT ( 'NONE',  ( 1.612141420133822223, -0.7113448269009944314, 1.997755531611951962 ) ) ;
#63015 = EDGE_CURVE ( 'NONE', #158170, #206605, #134452, .T. ) ;
#63016 = ORIENTED_EDGE ( 'NONE', *, *, #153420, .F. ) ;
#63017 = CARTESIAN_POINT ( 'NONE',  ( -6.635789839245807897, 6.706452665400368218, 0.7998128361456341429 ) ) ;
#63018 = CARTESIAN_POINT ( 'NONE',  ( 1.692022144237431469, 0.9228297918665344657, -1.615966242530289199 ) ) ;
#63019 = CIRCLE ( 'NONE', #18001, 2.080000000000000071 ) ;
#63020 = CARTESIAN_POINT ( 'NONE',  ( 5.217190183160311356, 4.981143389975473568, -0.7998128361456211532 ) ) ;
#63021 = CARTESIAN_POINT ( 'NONE',  ( 0.07536363704235826688, -0.001874865094115066300, -2.144269471569634877 ) ) ;
#63022 = CARTESIAN_POINT ( 'NONE',  ( 5.977185442992979603, -2.006959616289708315, -0.1948445219252663840 ) ) ;
#63023 = ORIENTED_EDGE ( 'NONE', *, *, #50862, .F. ) ;
#63024 = ORIENTED_EDGE ( 'NONE', *, *, #120212, .F. ) ;
#63025 = ORIENTED_EDGE ( 'NONE', *, *, #136902, .F. ) ;
#63026 = CARTESIAN_POINT ( 'NONE',  ( -5.579343907223557331, 6.467988298970945849, 1.199719254218450271 ) ) ;
#63027 = CARTESIAN_POINT ( 'NONE',  ( -7.974166903131914452, 12.45494515362926435, -0.7998128361456281477 ) ) ;
#63028 = CARTESIAN_POINT ( 'NONE',  ( 4.389149243953620605, 1.629682310347341456, -0.8231139397327084106 ) ) ;
#63031 = ORIENTED_EDGE ( 'NONE', *, *, #200985, .T. ) ;
#63030 = CARTESIAN_POINT ( 'NONE',  ( 1.737499999999999378, -2.916666666666668295, -3.009438278150925683 ) ) ;
#63029 = CARTESIAN_POINT ( 'NONE',  ( -3.983063267364693960, 7.868933921892603323, -0.7998128361456481317 ) ) ;
#63032 = CARTESIAN_POINT ( 'NONE',  ( 6.218145995260431214, 7.027935176161393294, 1.016989286988238206 ) ) ;
#63033 = CARTESIAN_POINT ( 'NONE',  ( 6.204453847213379447, -1.458334814074750740, -1.392330997281837623 ) ) ;
#63034 = CARTESIAN_POINT ( 'NONE',  ( 5.982333729491328356, -0.2747192703472668418, -1.820405398140816589 ) ) ;
#63035 = CARTESIAN_POINT ( 'NONE',  ( 2.984786552656538472, 6.457129931797648048, 0.3969071495571047103 ) ) ;
#63036 = CARTESIAN_POINT ( 'NONE',  ( 3.211855371912860413, -0.4501829054360923510, 2.263203710529379187 ) ) ;
#63037 = CARTESIAN_POINT ( 'NONE',  ( 6.367489420273535039, 7.457767740854454708, -1.199719254218452047 ) ) ;
#63038 = CARTESIAN_POINT ( 'NONE',  ( 5.641917277892137150, 0.8817427965214555963, -1.973778517010720490 ) ) ;
#63039 = CARTESIAN_POINT ( 'NONE',  ( 7.202405917357655341, 9.425892875049191488, 1.599625672291281386 ) ) ;
#63040 = CARTESIAN_POINT ( 'NONE',  ( 1.628360684195095054, 0.1923838640373880249, 1.932526033267305765 ) ) ;
#63041 = VERTEX_POINT ( 'NONE', #183161 ) ;
#63042 = CARTESIAN_POINT ( 'NONE',  ( 5.044420649243852139, 2.147057653193120252, -0.8206418397275447862 ) ) ;
#63043 = DIRECTION ( 'NONE',  ( -0.000000000000000000, -0.000000000000000000, 1.000000000000000000 ) ) ;
#63044 = CARTESIAN_POINT ( 'NONE',  ( -3.169574050544739841, 6.919863168935977527, -0.7998128361456481317 ) ) ;
#63045 =( GEOMETRIC_REPRESENTATION_CONTEXT ( 3 ) GLOBAL_UNCERTAINTY_ASSIGNED_CONTEXT ( ( #110460 ) ) GLOBAL_UNIT_ASSIGNED_CONTEXT ( ( #176010, #27602, #128405 ) ) REPRESENTATION_CONTEXT ( 'NONE', 'WORKASPACE' ) );
#63046 = CARTESIAN_POINT ( 'NONE',  ( 4.188257260935820625, -1.850246793840780279, -0.2747695030091561463 ) ) ;
#63047 =( GEOMETRIC_REPRESENTATION_CONTEXT ( 3 ) GLOBAL_UNCERTAINTY_ASSIGNED_CONTEXT ( ( #27045 ) ) GLOBAL_UNIT_ASSIGNED_CONTEXT ( ( #109827, #93527, #11166 ) ) REPRESENTATION_CONTEXT ( 'NONE', 'WORKASPACE' ) );
#63048 = B_SPLINE_CURVE_WITH_KNOTS ( 'NONE', 3,
 ( #126796, #192751, #76878, #127876, #208997, #44408, #110528, #163479, #176528, #31351, #28140 ),
 .UNSPECIFIED., .F., .F.,
 ( 4, 1, 1, 1, 1, 1, 1, 1, 4 ),
 ( 0.000000000000000000, 0.2256926809922864541, 0.3979886288388991278, 0.5260859906349554249, 0.6192013483571605637, 0.6864504996671639825, 0.7364865548622955282, 0.7772638159577213157, 1.000000000000000000 ),
 .UNSPECIFIED. ) ;
#63051 = CARTESIAN_POINT ( 'NONE',  ( -5.971440312176176768, 5.931378217152456500, 0.000000000000000000 ) ) ;
#63050 = CARTESIAN_POINT ( 'NONE',  ( -1.500000000000001332, -0.06874999931718445145, 0.000000000000000000 ) ) ;
#63049 = CARTESIAN_POINT ( 'NONE',  ( 1.037202349414727109, -0.04413313863061394532, 1.912034500058952036 ) ) ;
#63052 = CARTESIAN_POINT ( 'NONE',  ( 4.442132104469964204, 0.9450947508268662256, -1.994404356956205326 ) ) ;
#63053 = CARTESIAN_POINT ( 'NONE',  ( 6.983263157960327483, 4.697935251208478213, 2.408834092705824936 ) ) ;
#63054 = CARTESIAN_POINT ( 'NONE',  ( 7.309254211098767051, 7.700087132469628948, 0.7216878364870267237 ) ) ;
#63055 = CARTESIAN_POINT ( 'NONE',  ( -4.783329267523015460, 4.474972321731942593, -0.7998128361456221525 ) ) ;
#63056 = CARTESIAN_POINT ( 'NONE',  ( -5.248414861821563804, 9.137251415518218067, 0.7216878364870267237 ) ) ;
#63057 = CARTESIAN_POINT ( 'NONE',  ( 1.493369529629706705, 1.490176471889271603, 1.290657618255620864 ) ) ;
#63058 = CARTESIAN_POINT ( 'NONE',  ( 1.519075522400476830, 1.548194965108589782, -1.711296875134951545 ) ) ;
#63060 = EDGE_CURVE ( 'NONE', #52075, #116404, #20638, .T. ) ;
#63059 = CARTESIAN_POINT ( 'NONE',  ( 2.682025323810240280, -1.127217178123595565, -1.605522638798158264 ) ) ;
#63061 = CARTESIAN_POINT ( 'NONE',  ( 5.717653809678179044, 0.4078037869292486239, -2.021697613586806774 ) ) ;
#63062 = CARTESIAN_POINT ( 'NONE',  ( 5.205967797967541166, 5.175976640491323444, -0.7216878364870197293 ) ) ;
#63063 = CARTESIAN_POINT ( 'NONE',  ( 4.342354338126830804, 8.288106837781779035, -0.7998128361456381397 ) ) ;
#63064 = VERTEX_POINT ( 'NONE', #100838 ) ;
#63065 = CARTESIAN_POINT ( 'NONE',  ( -1.364683531249997417, 5.571875000341417916, 1.214306433183764966E-14 ) ) ;
#63066 = CARTESIAN_POINT ( 'NONE',  ( 1.579999999999991189, 8.758163473637745611, -2.499999999999989342 ) ) ;
#63067 = CARTESIAN_POINT ( 'NONE',  ( 10.58621901417202515, 11.24501035948919991, -0.7998128361456281477 ) ) ;
#63068 = CARTESIAN_POINT ( 'NONE',  ( 1.182764167570474534, 1.294921473658101840, -1.742447618606123960 ) ) ;
#63070 = CARTESIAN_POINT ( 'NONE',  ( -1.500000000000008216, 12.24999999999999645, 3.469446951953614189E-15 ) ) ;
#63069 = CARTESIAN_POINT ( 'NONE',  ( -1.123270288254055060, 3.033552654332631437, 0.7749999999939940487 ) ) ;
#63071 = FACE_OUTER_BOUND ( 'NONE', #14497, .T. ) ;
#63072 = DIRECTION ( 'NONE',  ( -0.7592566023652994600, 0.6507913734559651608, 0.000000000000000000 ) ) ;
#63073 = CARTESIAN_POINT ( 'NONE',  ( 2.143623209005097507, 0.7202431893391960660, -1.726524797105493336 ) ) ;
#63074 = CARTESIAN_POINT ( 'NONE',  ( 6.450466699499744827, 0.6713059571747861387, 2.054807225473152865 ) ) ;
#63075 = AXIS2_PLACEMENT_3D ( 'NONE', #66135, #83480, #163693 ) ;
#63076 = CARTESIAN_POINT ( 'NONE',  ( 6.827182134110207024, 2.985003573113382824, 2.264833014350222662 ) ) ;
#63077 = CARTESIAN_POINT ( 'NONE',  ( -1.364683531250014514, -0.9697916663252473812, 0.7879004041258379498 ) ) ;
#63078 = EDGE_CURVE ( 'NONE', #116100, #140668, #197925, .T. ) ;
#63079 = CARTESIAN_POINT ( 'NONE',  ( 2.525908831824146716, -1.891188341833285103, 0.2824699455093656053 ) ) ;
#63080 = CARTESIAN_POINT ( 'NONE',  ( 4.223360090310752213, -1.693420319160190646, 0.5144795390387302270 ) ) ;
#63081 = CARTESIAN_POINT ( 'NONE',  ( 1.752457306817490457, 1.891635876823925200, 0.2793096714826873161 ) ) ;
#63082 = CARTESIAN_POINT ( 'NONE',  ( -5.555090253297260361, 7.504024600312024340, 1.599625672291269396 ) ) ;
#63084 = CARTESIAN_POINT ( 'NONE',  ( 5.800374965758359203, 1.282846238547242557, -1.422814914302351852 ) ) ;
#63083 = CARTESIAN_POINT ( 'NONE',  ( 7.869907033621586834, -7.024005807131050716, -7.214015686748633804 ) ) ;
#63085 = CARTESIAN_POINT ( 'NONE',  ( 0.1685321339487330372, -0.8835925182541467526, -1.870455940253319183 ) ) ;
#63086 = CARTESIAN_POINT ( 'NONE',  ( -0.7499999999999972244, 4.608333333333352932, -1.299038105676652011 ) ) ;
#63087 = CARTESIAN_POINT ( 'NONE',  ( 2.267978396857213585, 0.5610993688725562922, -2.044979925899123252 ) ) ;
#63088 =( NAMED_UNIT ( * ) PLANE_ANGLE_UNIT ( ) SI_UNIT ( $, .RADIAN. ) );
#63089 = CARTESIAN_POINT ( 'NONE',  ( 5.278141497218024725, -1.038406966791558528, 1.555765341417144842 ) ) ;
#63091 = VERTEX_POINT ( 'NONE', #3316 ) ;
#63090 = CARTESIAN_POINT ( 'NONE',  ( 1.857752496991037061, 1.820901040755190214, -0.1330985588276211995 ) ) ;
#63093 = CARTESIAN_POINT ( 'NONE',  ( 5.220047253295719614, 7.706380104734268599, 1.202949228536150938 ) ) ;
#63092 = CARTESIAN_POINT ( 'NONE',  ( 4.108205984530819421, -2.201057848371779535, 0.1611738814469021175 ) ) ;
#63094 = CARTESIAN_POINT ( 'NONE',  ( -1.364683531250014514, -0.5114583329919092369, -0.7879004041258359514 ) ) ;
#63095 = CARTESIAN_POINT ( 'NONE',  ( 1.943872066224684669, 1.420748078972498440, 1.495595626624636409 ) ) ;
#63096 = CARTESIAN_POINT ( 'NONE',  ( 6.287230548435207567, 8.358188277972981695, -1.599625672291262513 ) ) ;
#63097 = CARTESIAN_POINT ( 'NONE',  ( -8.715193815486133033, 9.062147627688959872, 0.7998128361456462443 ) ) ;
#63098 = PRESENTATION_STYLE_ASSIGNMENT (( #194158 ) ) ;
#63099 = CARTESIAN_POINT ( 'NONE',  ( 1.430949710260811969, 3.674736480791923388, 0.4689103363401325164 ) ) ;
#63100 =( LENGTH_UNIT ( ) NAMED_UNIT ( * ) SI_UNIT ( .MILLI., .METRE. ) );
#63101 = CARTESIAN_POINT ( 'NONE',  ( 6.318982112420993502, 9.529840343536603697, -1.199719254218452047 ) ) ;
#63102 = ORIENTED_EDGE ( 'NONE', *, *, #88807, .T. ) ;
#63103 = CARTESIAN_POINT ( 'NONE',  ( 4.246580143467587831, -2.047389768388275577, -0.3068500204662719666 ) ) ;
#63104 = CARTESIAN_POINT ( 'NONE',  ( -1.364683531250014514, -0.6989583329919100141, -0.7879004041258359514 ) ) ;
#63105 = CARTESIAN_POINT ( 'NONE',  ( 2.091316376603330252, 1.881825464268515269, -1.063406855978922039 ) ) ;
#63106 = CARTESIAN_POINT ( 'NONE',  ( -5.206707715320216145, 7.734635641480951840, -1.194516140545264227 ) ) ;
#63108 = EDGE_CURVE ( 'NONE', #176917, #81409, #58880, .T. ) ;
#63107 = CARTESIAN_POINT ( 'NONE',  ( 2.297526485177129540, 1.845687725436034432, -0.8205148536439119678 ) ) ;
#63109 = CARTESIAN_POINT ( 'NONE',  ( 6.620655732516611103, 6.035157181942712334, 2.668628960472289702 ) ) ;
#63110 = B_SPLINE_CURVE_WITH_KNOTS ( 'NONE', 3,
 ( #94741, #80601, #112109, #147745, #129444, #29728, #127308, #179176, #30800, #180239, #63281, #130500, #195426, #12380, #96879, #109972, #78460, #175983 ),
 .UNSPECIFIED., .F., .F.,
 ( 4, 2, 2, 2, 2, 2, 2, 2, 4 ),
 ( 0.001640627021451598498, 0.001845642838648688241, 0.002050658655845778201, 0.002255674473042867945, 0.002460690290239957688, 0.002665706107437047431, 0.002870721924634137175, 0.003075737741831227352, 0.003280753559028317095 ),
 .UNSPECIFIED. ) ;
#63111 = VERTEX_POINT ( 'NONE', #201516 ) ;
#63112 = ADVANCED_FACE ( 'NONE', ( #187422 ), #87811, .T. ) ;
#63114 = CARTESIAN_POINT ( 'NONE',  ( 6.968527767744093993, 10.11340424813470662, 1.082531754730558626 ) ) ;
#63113 = CARTESIAN_POINT ( 'NONE',  ( 0.000000000000000000, -1.837499999999999911, -4.012584370867899430 ) ) ;
#63115 = CARTESIAN_POINT ( 'NONE',  ( -3.323157048681004699, 6.891117300187535655, -0.7216878364870458196 ) ) ;
#63116 = CARTESIAN_POINT ( 'NONE',  ( 1.499232818411553536, -0.2420282084563407654, 2.001858358113464575 ) ) ;
#63117 = CARTESIAN_POINT ( 'NONE',  ( 5.653911837654605144, 0.8871495062587383407, 2.004161502255866090 ) ) ;
#63118 = CARTESIAN_POINT ( 'NONE',  ( -1.500000000000013101, 4.160416667349482900, -0.8660254037844313801 ) ) ;
#63119 = CARTESIAN_POINT ( 'NONE',  ( 5.220932206144772714, 1.444093599275039885, -1.253800916539760113 ) ) ;
#63120 = CARTESIAN_POINT ( 'NONE',  ( -2.605138072120212200, 6.191078184115536232, -0.7998128361456281477 ) ) ;
#63122 = CARTESIAN_POINT ( 'NONE',  ( 5.897433631820129918, 8.863794422890064695, -1.082531754730537976 ) ) ;
#63121 = CARTESIAN_POINT ( 'NONE',  ( 4.259000112335223243, -0.004834882008357410665, -2.016708403958865414 ) ) ;
#63124 = CARTESIAN_POINT ( 'NONE',  ( 1.845327587665198443, 0.3419125196015109225, -1.987051676161588620 ) ) ;
#63123 = CARTESIAN_POINT ( 'NONE',  ( -9.802181872555943087, 10.53822639417784046, 0.7216878364870438212 ) ) ;
#63125 = CARTESIAN_POINT ( 'NONE',  ( -1.364683531250000748, 12.17187500034139980, 0.000000000000000000 ) ) ;
#63126 = CARTESIAN_POINT ( 'NONE',  ( -4.679499295372141709, 5.488445928469455559, 1.199719254218452935 ) ) ;
#63127 = CARTESIAN_POINT ( 'NONE',  ( 5.473588350598873831, 1.661195908839340873, -0.4637430927098630806 ) ) ;
#63128 = CARTESIAN_POINT ( 'NONE',  ( -0.1394461523061326647, 2.860155921427895542, -2.768185420354400073 ) ) ;
#63129 = CARTESIAN_POINT ( 'NONE',  ( 8.568389894156670294, 12.94027927658408217, -0.7216878364870257245 ) ) ;
#63130 = CARTESIAN_POINT ( 'NONE',  ( 1.499999999999990896, 4.775000000000022560, 1.214306433183764966E-14 ) ) ;
#63131 =( BOUNDED_SURFACE ( )  B_SPLINE_SURFACE ( 3, 3, ( 
 ( #93254, #31434, #114864, #28227, #97512, #96457, #163569, #15152, #213347, #81238 ),
 ( #30370, #94320, #146274, #27150, #159288, #10887, #44498, #209081, #126881, #192839 ),
 ( #110615, #160361, #18352, #165686, #49801, #20480, #119129, #33547, #151582, #1018 ),
 ( #100678, #135338, #136401, #70285, #17275, #201352, #150519, #67083, #84430, #83351 ),
 ( #2080, #185109, #36735, #180865, #202417, #52993, #102821, #132162, #34609, #16206 ),
 ( #68153, #182992, #166756, #69219, #134287, #4216, #167817, #149436, #164621, #99620 ),
 ( #101750, #50870, #35672, #184053, #168876, #116992, #200292, #19417, #133217, #54072 ) ),
 .UNSPECIFIED., .T., .F., .F. ) 
 B_SPLINE_SURFACE_WITH_KNOTS ( ( 4, 3, 4 ),
 ( 4, 1, 1, 1, 1, 1, 1, 4 ),
 ( 0.000000000000000000, 0.5000000000000000000, 1.000000000000000000 ),
 ( 0.000000000000000000, 0.09373397616858752945, 0.1863105892815605236, 0.2574079725677296260, 0.3612190813870841954, 0.5208938042821120717, 0.7336009914826546741, 1.000000000000000000 ),
 .UNSPECIFIED. ) 
 GEOMETRIC_REPRESENTATION_ITEM ( )  RATIONAL_B_SPLINE_SURFACE ( (
 ( 1.000000000000000000, 1.000000000000000000, 0.9999999999999997780, 1.000000000000000000, 1.000000000000000000, 1.000000000000000222, 1.000000000000000444, 1.000000000000000222, 1.000000000000000000, 1.000000000000000000),
 ( 0.3333333333333333703, 0.3333333333333333703, 0.3333333333333332593, 0.3333333333333333703, 0.3333333333333333703, 0.3333333333333334259, 0.3333333333333334814, 0.3333333333333334259, 0.3333333333333333703, 0.3333333333333333703),
 ( 0.3333333333333333703, 0.3333333333333333703, 0.3333333333333332593, 0.3333333333333333703, 0.3333333333333333703, 0.3333333333333334259, 0.3333333333333334814, 0.3333333333333334259, 0.3333333333333333703, 0.3333333333333333703),
 ( 1.000000000000000000, 1.000000000000000000, 0.9999999999999997780, 1.000000000000000000, 1.000000000000000000, 1.000000000000000222, 1.000000000000000444, 1.000000000000000222, 1.000000000000000000, 1.000000000000000000),
 ( 0.3333333333333333703, 0.3333333333333333703, 0.3333333333333332593, 0.3333333333333333703, 0.3333333333333333703, 0.3333333333333334259, 0.3333333333333334814, 0.3333333333333334259, 0.3333333333333333703, 0.3333333333333333703),
 ( 0.3333333333333333703, 0.3333333333333333703, 0.3333333333333332593, 0.3333333333333333703, 0.3333333333333333703, 0.3333333333333334259, 0.3333333333333334814, 0.3333333333333334259, 0.3333333333333333703, 0.3333333333333333703),
 ( 1.000000000000000000, 1.000000000000000000, 0.9999999999999997780, 1.000000000000000000, 1.000000000000000000, 1.000000000000000222, 1.000000000000000444, 1.000000000000000222, 1.000000000000000000, 1.000000000000000000) ) ) 
 REPRESENTATION_ITEM ( '' )  SURFACE ( )  );
#63132 = CARTESIAN_POINT ( 'NONE',  ( 4.216749469050096621, 4.878294787768598262, -1.199719254218452047 ) ) ;
#63133 = DIRECTION ( 'NONE',  ( -0.000000000000000000, -1.000000000000000000, -0.000000000000000000 ) ) ;
#63135 = AXIS2_PLACEMENT_3D ( 'NONE', #23661, #24726, #186159 ) ;
#63134 = CARTESIAN_POINT ( 'NONE',  ( 0.9364849611055334755, -1.153160888946737961, 1.719151461320179042 ) ) ;
#63136 = EDGE_LOOP ( 'NONE', ( #97153, #184030, #97293, #166927 ) ) ;
#63137 = CARTESIAN_POINT ( 'NONE',  ( 4.600164522386200439, -0.8494929878282222457, 1.599918020626096782 ) ) ;
#63139 = CARTESIAN_POINT ( 'NONE',  ( 4.258142763143749399, 7.125527769379820242, 1.199719254218451159 ) ) ;
#63138 = VECTOR ( 'NONE', #90265, 1000.000000000000000 ) ;
#63140 = CARTESIAN_POINT ( 'NONE',  ( 6.610000000000006537, 0.002781820520842553934, 2.000159646111852929 ) ) ;
#63141 = CARTESIAN_POINT ( 'NONE',  ( 6.076794983551159213, -1.275939312151072258, 1.286130553019491307 ) ) ;
#63142 = CARTESIAN_POINT ( 'NONE',  ( 6.346625304528514810, 6.577020074804287297, 0.000000000000000000 ) ) ;
#63143 = CARTESIAN_POINT ( 'NONE',  ( 11.63470271956841806, 8.257786514500919495, -2.967717102421748798 ) ) ;
#63144 = CARTESIAN_POINT ( 'NONE',  ( 3.082162360440068749, -2.159116730143955998, -0.3741398933536920768 ) ) ;
#63145 = ORIENTED_EDGE ( 'NONE', *, *, #80091, .F. ) ;
#63147 = CARTESIAN_POINT ( 'NONE',  ( 8.565000355531088516, 11.01558638625153286, -1.599625672291257406 ) ) ;
#63146 = CARTESIAN_POINT ( 'NONE',  ( 0.1390251588108057101, -0.1389306544097475005, -1.930426113910483688 ) ) ;
#63148 = CARTESIAN_POINT ( 'NONE',  ( 5.132410944242819184, 0.5605724621733051416, 1.831730044279370029 ) ) ;
#63149 = CARTESIAN_POINT ( 'NONE',  ( -4.083708824282378913, 7.596498746673441715, 0.5977277219625460880 ) ) ;
#63150 = CARTESIAN_POINT ( 'NONE',  ( -15.75000000000000000, 12.69999999999999929, 0.6999999999999992895 ) ) ;
#63151 = CARTESIAN_POINT ( 'NONE',  ( 1.364683531249986537, -0.3447916663252443836, -0.7879004041258309554 ) ) ;
#63152 = CARTESIAN_POINT ( 'NONE',  ( 5.341549334104188418, 7.254893527920112994, 1.443375672974062551 ) ) ;
#63153 = CARTESIAN_POINT ( 'NONE',  ( -8.297226821883391779, 11.66355314463053006, 1.082531754730549967 ) ) ;
#63154 = CARTESIAN_POINT ( 'NONE',  ( 1.411231610350563992, 1.906656261001705488, 1.018656936289302539 ) ) ;
#63155 = CARTESIAN_POINT ( 'NONE',  ( -4.716257332707368910, 6.595662536282280719, -1.599625672291271394 ) ) ;
#63156 = CARTESIAN_POINT ( 'NONE',  ( 5.551137550152489553, 5.441024994791534120, 0.7998128361456352531 ) ) ;
#63157 = CARTESIAN_POINT ( 'NONE',  ( 1.711645973048509850, -1.812212506298327197, 0.2199163931802459171 ) ) ;
#63158 = CARTESIAN_POINT ( 'NONE',  ( -3.415764635639130020, 6.072476943965863683, 1.199719254218462483 ) ) ;
#63159 = CARTESIAN_POINT ( 'NONE',  ( 4.190329584092522097, -1.805708503706305423, -0.2678305112727846771 ) ) ;
#63160 = CARTESIAN_POINT ( 'NONE',  ( 9.245776177298674625, 13.11974810171090056, -9.005675837709214093 ) ) ;
#63161 = ORIENTED_EDGE ( 'NONE', *, *, #62637, .F. ) ;
#63162 = CARTESIAN_POINT ( 'NONE',  ( 4.088306882321583124, 1.055547913133596749, -1.662622193200061771 ) ) ;
#63163 = ORIENTED_EDGE ( 'NONE', *, *, #68346, .T. ) ;
#63164 = CARTESIAN_POINT ( 'NONE',  ( 5.179219622276672652, 1.307079648806110050, 1.436513822289321674 ) ) ;
#63165 = ORIENTED_EDGE ( 'NONE', *, *, #64003, .T. ) ;
#63166 = CARTESIAN_POINT ( 'NONE',  ( -6.099189001301292379, 8.209082816308541197, 1.599625672291263179 ) ) ;
#63168 = CARTESIAN_POINT ( 'NONE',  ( 5.150683391976684788, 2.089615912265533559, 0.3601871064465370087 ) ) ;
#63167 = CARTESIAN_POINT ( 'NONE',  ( 7.354371980770088690, 7.544798497178720531, 0.000000000000000000 ) ) ;
#63169 = CARTESIAN_POINT ( 'NONE',  ( -3.177206141917424009, 8.963489737286273851, -2.500000000000001332 ) ) ;
#63170 = CARTESIAN_POINT ( 'NONE',  ( 2.701700744156261713, 1.353761940859641966, 1.350867010771430676 ) ) ;
#63171 = CARTESIAN_POINT ( 'NONE',  ( 5.232446707518059625, 6.618332276934084213, -1.382299536160000120 ) ) ;
#63172 = CARTESIAN_POINT ( 'NONE',  ( 6.983263157960393208, 0.5798717822590447879, 1.998431770337566027 ) ) ;
#63173 = CARTESIAN_POINT ( 'NONE',  ( 4.686278372178935392, 5.496354851410763409, 1.199719254218452047 ) ) ;
#63174 = VECTOR ( 'NONE', #166798, 1000.000000000000114 ) ;
#63175 = CARTESIAN_POINT ( 'NONE',  ( 5.039702193125279450, -1.910865547410881549, 0.6335069822010936935 ) ) ;
#63176 = CARTESIAN_POINT ( 'NONE',  ( -4.307832228787286333, 7.438438422310007958, -1.137755099753708254 ) ) ;
#63177 = CARTESIAN_POINT ( 'NONE',  ( 6.129513044595952032, -1.717388127611047421, 0.6198453807191862674 ) ) ;
#63178 = CARTESIAN_POINT ( 'NONE',  ( 1.293514844328220281, -1.872496763586928514, 0.8835221827151735763 ) ) ;
#63179 = CARTESIAN_POINT ( 'NONE',  ( -7.944714827928056167, 10.29191993738131927, 1.443375672974090751 ) ) ;
#63180 =( BOUNDED_SURFACE ( )  B_SPLINE_SURFACE ( 3, 3, ( 
 ( #24239, #90341, #107720, #109857, #191012, #144467, #175871, #173747, #208332, #10137, #125057, #156410, #25324, #207273, #27459, #141265, #76212, #94629, #108787, #26389, #7997, #58904, #189959, #92501, #193162, #126118, #174813, #188890, #158540, #140180, #192078, #74089, #93557, #160672, #122933, #110916, #159601, #78344, #11199, #77280, #61034, #49063, #181178, #83667, #128268, #146586, #45874, #163887, #197421, #31749, #30684, #132475, #165999, #62109, #97822, #96767, #80486, #145535, #65275, #210471, #114132, #95697, #15462, #14395, #81548, #180124, #177998, #129334, #17584, #131421, #147631, #111996, #213649, #182232, #179065, #32803, #82605, #194230, #115183, #29612, #63168, #98877, #48015, #33856, #164930, #195310, #99937, #211533, #16522, #148690, #259, #198477, #161752, #13343, #50122, #46941, #116243, #113059, #79418, #212603, #162818, #64241, #130385, #196375, #85814, #201667, #86883, #149758, #100984, #3468, #186507, #69537, #150833, #168133, #185434, #37054, #151893, #103137, #135644, #137784, #184365, #2395, #202739, #154024, #200603, #5591, #68474, #18665, #183305, #52250, #167073, #84745, #53314, #187573, #134602, #4525, #203803, #118377, #19735, #35987, #1335, #133537, #119446, #102068, #169195, #199544, #171326, #20788, #152950, #70600, #136714, #55449, #87950, #54390, #67396, #120528, #38138, #104210, #121601, #170257, #21842, #71670, #39198, #105290, #51186, #117309, #34912, #84114, #150202, #135024, #6041, #170697, #100366, #87321, #68905, #36425, #35356, #117756, #199984, #71039, #19102, #201038, #51631, #22283, #21217, #119888, #166436, #153389, #154463, #4960, #137152, #18027, #1773, #102501, #67829, #53755, #54824, #136080, #52681, #88396, #55886, #133976, #202097, #20164, #86251, #167504, #169634, #85180, #151264, #138221, #2836, #183746, #152321, #3898, #185865, #120973, #103576, #37500, #186942, #38575, #72112, #204234, #191203, #25513, #212520, #162739, #91621, #95622, #42868, #174995, #108976, #80406, #106828, #13266, #79339, #8196, #157672, #172858, #145456, #9269, #206393, #75340, #211453, #26580, #63087, #129257, #173940, #146503, #64162, #141457, #207464, #205319, #59083, #90541, #24429, #195227, #107914, #46864, #125243, #161673, #130304, #112977, #39634, #178989, #89475, #105743, #171769, #123130, #30604, #96692, #74281, #14311, #23366, #155530, #7110, #73183, #139289, #56958, #156606, #189089, #40722, #140375, #58020, #124184, #190147, #41801, #50037, #81473, #164851, #132394, #183225, #32715, #149673, #101982, #182147, #165918, #163803, #181099, #197342, #17503, #118295, #51102, #131347, #114052, #115102, #65194, #199460, #15379, #82523, #168051, #47938, #35907, #117227, #19653, #69456, #67312, #1254, #116161, #147550, #16443, #198396, #34831, #98797, #133455, #85727, #33777, #83591, #213572, #148609, #48984, #100905, #184281, #166994, #178, #180045, #66246, #99856, #18585, #84663, #150752, #151813, #31667, #3386, #2313, #196292, #97744, #68390, #134519, #200523, #52169, #8742, #53232, #71588, #185350, #88949, #122595, #171239, #170171, #205869, #91089, #201585, #22835, #21759, #5508, #70513, #204782, #136628, #202655, #173405, #120442, #157149, #186416, #87867, #39119, #188558, #138765, #6588, #152865, #7660, #54304, #153939, #72667, #121518, #135561, #41273, #187489, #40189 ),
 ( #105202, #137697, #155003, #106301, #56436, #172323, #156074, #55365, #24986, #119362, #23913, #90017, #86799, #73744, #38053, #104125, #139840, #203717, #57503, #123662, #189625, #36972, #107382, #103055, #169108, #20705, #4443, #30340, #158215, #94292, #209052, #43400, #78008, #60688, #112713, #190680, #46595, #124720, #42339, #125783, #127935, #126852, #162476, #61766, #191745, #79070, #109522, #145188, #141986, #9804, #108454, #175530, #92163, #75879, #192809, #178725, #59626, #144132, #128980, #27119, #93225, #208000, #74823, #58566, #143057, #159257, #10858, #174474, #96425, #76931, #44468, #160332, #110584, #62820, #12995, #176586, #206937, #28198, #11936, #210125, #194959, #193887, #45535, #177661, #111649, #26049, #211194, #29269, #95361, #161411, #140923, #48722, #51917, #118040, #147289, #213321, #32461, #164591, #16177, #82261, #148354, #214353, #65983, #83322, #151295, #55918, #121005, #4992, #73216, #200013, #103607, #2866, #21248, #69999, #137186, #87355, #167534, #118845, #51664, #54854, #203208, #19132, #38604, #171803, #168595, #22317, #138253, #68936, #153423, #117787, #52712, #104682, #37530, #23395, #170731, #184827, #89508, #201070, #88430, #154494, #188038, #39667, #135058, #36457, #105778, #102533, #155562, #20195, #86283, #136113, #152354, #202128, #53789, #119920, #185895, #16630, #116345, #179170, #130494, #32906, #1437, #98984, #180233, #197527, #361, #66433, #181280, #132576, #165037, #167177, #213755, #31856, #17690, #198579, #97932, #18766, #117419, #82714, #96873, #148791, #163990, #196481, #84850, #81652, #50226, #67502, #15565, #48123, #183416, #147739, #131524, #162923, #14503, #65378, #150940, #35019, #30794, #166104, #49171, #115289, #114235, #182336, #64348, #149869, #33964, #100041, #83776, #101090, #133648, #199647, #52358, #80595, #51294, #2503, #68575, #134702, #200707, #146691, #212707, #37165, #140034, #187674, #137891, #168238, #55557, #90207, #86984, #155196, #204980, #102171, #88056, #184470, #185537, #23027, #170361, #156271, #105399, #103243, #7853, #119551, #21946, #72852, #56625, #171437, #36087, #19837, #138959, #169303, #122790, #20887, #6777, #54491, #188749, #136815, #53414, #89142, #120635, #154128, #121712, #118486, #69642, #186613, #40388, #38239, #153054, #202842, #5698, #71775, #104312, #203910, #39304, #106492, #4630, #70702, #172518, #24103, #73940, #206059, #85923, #201774, #151996, #3568, #135750, #207129, #175716, #95553, #42534, #127043, #111846, #108638, #76070, #58755, #57694, #41464, #125973, #124907, #190870, #107573, #79271, #142170, #75009, #161605, #173607, #29463, #25179, #91281, #174666, #110770, #191930, #145388, #44656, #26240, #143250, #11049, #43594, #157340, #92357, #208186, #176770, #158395, #77128, #177851, #109712, #27308, #8928, #9993, #59819, #93413, #194074, #193003, #159451, #189814, #209240, #141118, #60884, #28385, #94480, #13194, #123851, #160520, #12124, #78196, #144323, #210321, #61958, #128116, #45727, #84597, #129183, #147484, #46796, #164784, #198328, #32648, #31598, #67251, #166925, #63013, #98725, #97674, #81401, #146434, #66177, #212448, #64092, #34767, #196227, #18519, #47869, #163731, #115032, #49968, #110, #82455, #14239, #83521, #130234, #15312, #148544, #197272, #211387, #117160, #48912, #116087, #132322, #182077, #33709 ),
 ( #99786, #165852, #17437, #149602, #131285, #100840, #195161, #181031, #16376, #162669, #1187, #113980, #179977, #133386, #65127, #199391, #51037, #183163, #112909, #178920, #30535, #96615, #80333, #213506, #106235, #19588, #170105, #70450, #119294, #153876, #136565, #134454, #4378, #3318, #69387, #200457, #172260, #20640, #167983, #21691, #151747, #138701, #88886, #202586, #68323, #54238, #135495, #85661, #204719, #53166, #152799, #39054, #201518, #101917, #154940, #185281, #102985, #52103, #118232, #36903, #56369, #6524, #150685, #137635, #169043, #86729, #120376, #186351, #35839, #121453, #37986, #104059, #87803, #72601, #71524, #5445, #23848, #2247, #203654, #55304, #187424, #105139, #171179, #22770, #184216, #122532, #188493, #40125, #109458, #139776, #27049, #61699, #58500, #126787, #176519, #73677, #59556, #156006, #157083, #208989, #141922, #127868, #76869, #8671, #193818, #91021, #207934, #44398, #28131, #142989, #7593, #205803, #110519, #74754, #94227, #140856, #192743, #25985, #160265, #108383, #24917, #60625, #92093, #125715, #93157, #89955, #41206, #158147, #11867, #9739, #206869, #174408, #191676, #43338, #75814, #175464, #159195, #77944, #124656, #190612, #144065, #210060, #42271, #45466, #10795, #173337, #123595, #111583, #107313, #177593, #57434, #189560, #13990, #98467, #83262, #80074, #47609, #30273, #29205, #66995, #116905, #164532, #149348, #82201, #214292, #95295, #161344, #179727, #79005, #197024, #16118, #64888, #63830, #99535, #199132, #12925, #131034, #129988, #113723, #178661, #148294, #96358, #162413, #133133, #146177, #50777, #212192, #195976, #147233, #65926, #32401, #114777, #46531, #115840, #31346, #97420, #180775, #15056, #145122, #928, #81148, #132073, #198084, #49711, #181826, #211128, #163474, #33459, #165596, #213261, #48661, #17187, #62752, #128912, #194893, #112652, #156554, #189037, #8149, #206344, #102737, #75292, #141407, #168792, #70200, #134196, #139235, #19331, #35583, #57971, #36651, #124135, #20398, #24378, #207415, #86481, #59034, #40675, #18259, #9220, #182904, #51858, #205266, #152545, #151494, #106778, #4131, #34521, #84342, #157623, #150430, #1995, #85409, #90491, #56907, #100593, #172806, #3063, #123080, #74233, #140326, #68060, #69133, #119042, #190096, #135255, #41750, #91571, #107862, #173888, #200205, #167730, #183971, #25463, #166668, #117980, #101662, #201269, #52909, #185026, #128404, #158680, #11340, #96905, #191155, #179204, #194371, #177064, #62245, #125192, #76353, #193304, #161893, #44949, #126263, #143538, #160815, #12406, #127335, #78486, #111057, #113198, #159742, #192220, #178137, #129468, #176009, #195452, #43883, #208468, #10278, #27601, #142460, #60104, #28680, #162956, #109997, #46014, #30828, #93701, #209532, #77421, #42822, #108928, #94767, #61174, #144603, #174949, #146723, #210618, #112134, #29752, #95837, #14534, #63307, #13480, #26531, #79556, #145674, #211671, #80631, #47080, #212741, #92639, #131557, #15598, #2533, #49202, #16663, #48155, #114268, #99014, #184501, #134732, #64376, #51324, #32941, #148821, #213786, #81684, #164023, #35050, #197558, #165071, #147770, #68609, #199681, #83808, #152030, #130522, #182366, #65409, #100070, #82748, #149900, #33996, #31888, #115323, #85955, #133676, #1468, #180264, #67534, #36120, #394, #101121, #150969 ),
 ( #196512, #166132, #66465, #132606, #181313, #117452, #198612, #50259, #102204, #116378, #19870, #17719, #183446, #167209, #18797, #84882, #200739, #52389, #118517, #168270, #97965, #185569, #70735, #103273, #20920, #154163, #24135, #4663, #39337, #40421, #136849, #186644, #87015, #3599, #201805, #21980, #202873, #54521, #53447, #7886, #104347, #169336, #121742, #153087, #106524, #56661, #88090, #119586, #5729, #120666, #38270, #172550, #170391, #71808, #72887, #137919, #203939, #122824, #55587, #187709, #37199, #105434, #171470, #90237, #188785, #69676, #23059, #89176, #155228, #6809, #138994, #205015, #156303, #135782, #165770, #82372, #201431, #118145, #2157, #70363, #197190, #100754, #148462, #18432, #1103, #68234, #166836, #164699, #116008, #4292, #52020, #134367, #32563, #200372, #168955, #17353, #19495, #69297, #180943, #84506, #48828, #49883, #101827, #34685, #20559, #184130, #181994, #86642, #198245, #150595, #151660, #135409, #35753, #114943, #98640, #3231, #33627, #53071, #99700, #85570, #133298, #119204, #67162, #132237, #167895, #199304, #185190, #36814, #16286, #30, #50949, #102896, #117074, #83435, #183073, #152709, #66094, #149517, #23764, #138609, #124567, #171087, #203564, #189475, #38966, #204632, #24830, #55217, #87711, #74663, #121362, #88794, #120287, #186262, #22682, #42183, #206780, #136477, #123511, #105051, #6436, #71434, #153782, #21604, #107227, #187337, #154852, #5352, #140767, #57346, #155920, #9649, #202499, #40037, #137546, #172172, #72512, #7504, #106148, #103974, #56283, #158063, #205712, #73588, #37897, #139690, #108298, #122442, #173250, #8583, #170016, #89869, #54150, #188400, #41117, #90930, #174319, #156996, #58413, #25893, #190527, #92003, #30174, #162315, #62659, #207845, #191588, #96263, #60533, #13901, #142900, #112554, #11776, #79982, #94137, #10710, #128817, #77849, #127775, #12833, #75726, #26959, #143972, #178567, #209965, #76778, #160176, #111492, #177499, #61605, #29112, #193731, #63734, #110429, #208901, #194800, #146085, #126693, #212097, #192655, #159109, #109368, #44307, #93066, #176433, #45376, #113627, #28044, #145029, #129892, #95195, #161247, #78907, #141840, #59470, #211033, #46436, #195877, #125629, #97328, #47515, #179631, #31253, #163384, #43249, #175376, #149256, #147141, #83173, #214203, #32308, #2977, #213167, #130940, #183882, #65834, #35494, #82110, #51770, #165501, #101572, #33364, #164438, #67966, #17094, #66899, #166577, #14958, #180682, #829, #117890, #133039, #16026, #99446, #50686, #116811, #199038, #182812, #34428, #69045, #49618, #148203, #134109, #19241, #131982, #85321, #197990, #98375, #48572, #115743, #181732, #100502, #18164, #52819, #84252, #150338, #135164, #1906, #200118, #167639, #81056, #64796, #151404, #201181, #118957, #196933, #36560, #184936, #102648, #114690, #169770, #156745, #106972, #88542, #86393, #22432, #153534, #186006, #8335, #71179, #170842, #57097, #21360, #120031, #172996, #5103, #121117, #152462, #4042, #203315, #74420, #24577, #168704, #155667, #137298, #38715, #103719, #37641, #53895, #139429, #87467, #54965, #187082, #90684, #89616, #188152, #41938, #20308, #72251, #104795, #204377, #154604, #39784, #138359, #136223, #6183, #190280, #23511, #105889, #70110, #171915, #140519, #56033, #205464, #40867, #202244, #122186 ),
 ( #206533, #7251, #73327, #123263, #189228, #58163, #124321, #143727, #142647, #178329, #63495, #174075, #209720, #208656, #192408, #43005, #177252, #109118, #175132, #145851, #92821, #129650, #158866, #60286, #11534, #94951, #111249, #193495, #125376, #194553, #26720, #126445, #45137, #93892, #195635, #13663, #159931, #160999, #28864, #12591, #78665, #211858, #10462, #144792, #210799, #76536, #77604, #44064, #62422, #61366, #110182, #127524, #128587, #46196, #112314, #29937, #27794, #108050, #25647, #96021, #162073, #59218, #79735, #176193, #91758, #157811, #9410, #75481, #141592, #207598, #191339, #33119, #134906, #116554, #97086, #85059, #2713, #130701, #66638, #181490, #15781, #50435, #99197, #151145, #163139, #18975, #14722, #80813, #98145, #100244, #165248, #47268, #34172, #164194, #132783, #572, #115495, #146904, #81866, #197738, #166312, #147952, #198786, #167385, #16841, #82923, #212923, #32058, #48331, #148996, #183622, #182548, #196692, #179391, #180442, #114441, #17902, #64557, #213965, #68786, #113383, #101305, #83987, #31011, #65585, #150075, #131732, #1647, #67705, #49377, #133853, #199863, #51506, #117631, #35230, #186818, #171641, #204107, #23238, #6980, #120844, #90411, #156481, #38446, #88268, #152203, #154336, #37374, #53629, #73061, #54693, #139160, #104526, #39512, #8070, #170572, #74156, #55759, #36298, #24306, #200912, #69845, #5911, #22153, #169509, #121915, #71985, #52560, #102374, #172728, #168444, #20043, #103449, #105610, #138094, #118692, #187884, #21091, #89350, #155398, #205190, #86130, #87195, #137024, #56831, #153259, #123002, #106704, #188958, #40598, #3771, #185740, #201971, #184676, #135956, #119761, #4834, #70914, #203051, #9148, #143461, #173813, #26459, #112063, #206272, #194300, #209459, #178063, #13408, #61103, #45944, #193233, #110986, #140250, #57896, #76282, #190025, #93627, #127262, #175936, #174879, #210543, #95765, #124060, #27530, #92568, #10207, #75223, #44880, #141334, #207347, #29681, #125123, #161819, #191081, #158610, #43812, #176991, #28609, #11271, #157552, #12333, #58968, #142390, #77349, #126184, #41677, #107788, #192148, #94698, #160739, #78413, #144534, #25392, #42748, #62177, #128336, #108853, #91491, #208399, #60033, #109925, #159669, #65339, #212665, #33928, #131486, #31816, #197491, #50189, #82673, #100003, #17657, #213716, #34985, #145603, #49133, #181241, #30752, #32869, #130452, #146651, #83740, #147698, #149832, #164999, #132545, #211598, #16591, #129397, #327, #195376, #117382, #47008, #162883, #66397, #198543, #48084, #1402, #67463, #113124, #96833, #51258, #14462, #80553, #196440, #114195, #180195, #97892, #15529, #81614, #104280, #186578, #86953, #118450, #201740, #169268, #5661, #69607, #38206, #138926, #4596, #202809, #200671, #3533, #19802, #54457, #155162, #88021, #168203, #150903, #151962, #102134, #21912, #52321, #119516, #204943, #84814, #72822, #154093, #56594, #106459, #71741, #122756, #137855, #203876, #18730, #2464, #20854, #68540, #170325, #55520, #120601, #53381, #89108, #188717, #134669, #121676, #185502, #103206, #85886, #187641, #135714, #37127, #40354, #153021, #184437, #70670, #136780, #39269, #105363, #171400, #22990, #36054, #6744, #107538, #58720, #109681, #158367, #130976, #81087, #9960, #11017, #175684, #93380, #27273, #146118 ),
 ( #25141, #195914, #26208, #113662, #92325, #80015, #196967, #76037, #48604, #159416, #7816, #213201, #172483, #41430, #191899, #142139, #141082, #212131, #208154, #64830, #73909, #147175, #140002, #206023, #8893, #63767, #59784, #24070, #129926, #74972, #43561, #125941, #47551, #57660, #207092, #108604, #179666, #124870, #31285, #90173, #97361, #163419, #123819, #157303, #173570, #14994, #156239, #189779, #91243, #190836, #42496, #174632, #117925, #148236, #871, #86429, #180719, #168740, #183919, #152494, #202279, #35531, #20343, #167674, #85357, #114722, #32343, #50722, #164473, #68005, #101607, #150373, #149290, #184970, #70148, #98409, #1943, #66936, #199076, #49656, #19275, #115779, #181768, #4077, #99480, #136259, #165538, #133078, #18203, #151439, #3010, #200153, #132017, #201217, #33401, #116847, #51807, #100538, #16060, #82144, #166613, #69080, #135200, #52858, #118991, #214238, #17131, #36595, #102682, #83207, #84287, #182848, #65868, #134145, #34467, #198027, #203347, #123296, #55000, #121151, #91790, #38748, #9441, #104830, #6217, #171950, #40898, #57129, #139466, #71214, #140554, #187116, #154636, #205496, #39818, #75512, #174109, #105926, #107003, #189259, #173028, #24610, #157846, #170875, #90718, #156781, #22467, #23539, #88578, #8367, #89648, #72286, #155702, #74450, #206568, #58195, #124353, #188183, #141623, #53932, #7283, #73360, #5138, #190311, #138394, #204412, #41969, #122223, #108080, #25681, #120068, #186044, #37679, #103756, #169805, #21394, #87505, #153569, #137331, #56066, #127560, #176225, #210833, #193528, #31047, #109154, #179426, #43041, #175166, #44098, #46233, #45171, #80850, #194588, #110218, #78700, #161034, #61397, #92854, #27827, #143762, #112350, #93924, #12629, #113420, #111283, #177288, #26753, #192443, #208692, #28903, #129687, #62459, #142681, #125408, #126479, #76570, #128622, #158900, #159964, #97122, #59251, #47306, #178363, #163175, #207632, #29971, #14759, #96056, #162109, #191375, #10497, #209756, #60319, #144826, #13698, #94988, #11570, #63532, #77640, #79771, #145884, #211894, #195670, #1691, #81903, #64595, #65622, #15818, #150118, #180478, #33156, #118729, #212956, #200952, #67745, #184714, #20083, #133895, #52601, #199902, #117672, #146941, #130735, #82961, #196728, #100285, #51548, #182589, #181528, #2755, #102416, #48368, #34212, #99237, #16880, #147991, #183665, #214001, #131771, #36338, #197775, #168484, #49412, #165286, #50474, #35269, #101346, #17942, #164230, #19018, #115533, #149034, #84028, #132825, #114481, #32096, #198829, #167426, #85098, #151183, #68824, #98182, #610, #134946, #66677, #116595, #166351, #4877, #123048, #72025, #38490, #138137, #56872, #89391, #188999, #106745, #5954, #190066, #41718, #204146, #187922, #37415, #39553, #137066, #153301, #172772, #154377, #24346, #55801, #139201, #107828, #121956, #173853, #155439, #135997, #124103, #86171, #169552, #105654, #171682, #54736, #7024, #23279, #152241, #202011, #57938, #53670, #119802, #203091, #205231, #73100, #3813, #40642, #120886, #90456, #156522, #8113, #185781, #186860, #22200, #74201, #104568, #140295, #206314, #69885, #103491, #21133, #70956, #87237, #170613, #88313, #211639, #26499, #77387, #194340, #112103, #12374, #157594, #141374, #45982, #10247, #178106, #92606, #62216, #175977, #29722 ),
 ( #145644, #11309, #78454, #28648, #160781, #177031, #63275, #158649, #210586, #128373, #208437, #143503, #76323, #95804, #209500, #192188, #61140, #161860, #94735, #13450, #79526, #159710, #129437, #195420, #127302, #193273, #191121, #44918, #142428, #60071, #47050, #93668, #113166, #111026, #144572, #25429, #91535, #9189, #75260, #207385, #59006, #125162, #108896, #42787, #174919, #126227, #43852, #109966, #27570, #172245, #28113, #106219, #23832, #107297, #109441, #190597, #144046, #43322, #173320, #141906, #9724, #124640, #155990, #24899, #206852, #175447, #91005, #75799, #176502, #42254, #25969, #89938, #41190, #57417, #92075, #192725, #125698, #205787, #188478, #189542, #139761, #59538, #7577, #157067, #94207, #122515, #110502, #191658, #160247, #56352, #27031, #11848, #93140, #159177, #40108, #73662, #58484, #123580, #207918, #10778, #158132, #8656, #76852, #77926, #108368, #142971, #74735, #140840, #174392, #208973, #44379, #60608, #126767, #127850, #128894, #78988, #213242, #29186, #96340, #181811, #61681, #49695, #64872, #33443, #83246, #131017, #115823, #48645, #180759, #210042, #193801, #146159, #45449, #163459, #197009, #31327, #30255, #65910, #165578, #111565, #97403, #162396, #80058, #145105, #114763, #211110, #62735, #99519, #194876, #17172, #46511, #13972, #113705, #32387, #98452, #81130, #12908, #82185, #112634, #212175, #147216, #195956, #177573, #95276, #47591, #164516, #16101, #148278, #214277, #161324, #178644, #132057, #198067, #63809, #179710, #129969, #15038, #50759, #199115, #116888, #34504, #182887, #100577, #166650, #18241, #149331, #911, #66979, #133117, #90155, #92306, #189759, #41412, #159399, #190817, #77075, #42478, #43543, #94430, #108587, #12076, #59765, #40335, #176721, #160469, #139984, #158350, #174615, #173549, #125925, #26191, #28333, #106441, #110721, #172464, #24052, #25123, #27255, #10998, #204926, #143203, #8876, #209193, #60833, #126994, #74955, #192953, #44605, #180718, #128853, #177532, #53931, #120067, #186043, #37678, #103755, #76569, #58194, #22466, #10496, #54999, #56065, #206567, #123295, #155701, #190310, #24609, #187115, #154635, #6216, #105925, #139465, #205495, #41968, #91789, #157845, #75511, #59250, #109153, #79770, #62458, #27826, #111282, #78699, #129686, #45170, #211893, #48367, #128621, #29970, #110217, #127559, #143761, #47305, #130734, #113419, #77639, #126478, #177287, #11569, #31046, #176224, #28902, #114480, #208691, #196727, #163174, #32095, #15817, #98181, #164229, #142680, #192442, #44097, #94987, #194587, #161033, #12628, #71761, #117671, #116594, #155184, #40377, #147990, #183664, #182588, #166350, #16879, #154114, #82960, #149033, #122778, #66676, #106479, #132824, #34211, #199901, #137877, #88043, #170348, #99236, #171425, #609, #100284, #21933, #67744, #172506, #204967, #133894, #203898, #5684, #55543, #121697, #188738, #198828, #187662, #39290, #50473, #51547, #17941, #105385, #35268, #84027, #101345, #23012, #89129, #6767, #72842, #1690, #81902, #214000, #138946, #56614, #33155, #65621, #150117, #131770, #197774, #49411, #115532, #181527, #165285, #92345, #176757, #158385, #77114, #194062, #9980, #111833, #93401, #73929, #61945, #45715, #107560, #43583, #76058, #207117, #27294, #142157, #128104, #140021, #210309, #206047, #57683, #74997, #143238, #208173 ) ),
 .UNSPECIFIED., .T., .F., .T. ) 
 B_SPLINE_SURFACE_WITH_KNOTS ( ( 4, 3, 4 ),
 ( 4, 1, 1, 1, 1, 1, 1, 1, 1, 1, 1, 1, 1, 1, 1, 1, 1, 1, 1, 1, 1, 1, 1, 1, 1, 1, 1, 1, 1, 1, 1, 1, 1, 1, 1, 1, 1, 1, 1, 1, 1, 1, 1, 1, 1, 1, 1, 1, 1, 1, 1, 1, 1, 1, 1, 1, 1, 1, 1, 1, 1, 1, 1, 1, 1, 1, 1, 1, 1, 1, 1, 1, 1, 1, 1, 1, 1, 1, 1, 1, 1, 1, 1, 1, 1, 1, 1, 1, 1, 1, 1, 1, 1, 1, 1, 1, 1, 1, 1, 1, 1, 1, 1, 1, 1, 1, 1, 1, 1, 1, 1, 1, 1, 1, 1, 1, 1, 1, 1, 1, 1, 1, 1, 1, 1, 1, 1, 1, 1, 1, 1, 1, 1, 1, 1, 1, 1, 1, 1, 1, 1, 1, 1, 1, 1, 1, 1, 1, 1, 1, 1, 1, 1, 1, 1, 1, 1, 1, 1, 1, 1, 1, 1, 1, 1, 1, 1, 1, 1, 1, 1, 1, 1, 1, 1, 1, 1, 1, 1, 1, 1, 1, 1, 1, 1, 1, 1, 1, 1, 1, 1, 1, 1, 1, 1, 1, 1, 1, 1, 1, 1, 1, 1, 1, 1, 1, 1, 1, 1, 1, 1, 1, 1, 1, 1, 1, 1, 1, 1, 1, 1, 1, 1, 1, 1, 1, 1, 1, 1, 1, 1, 1, 1, 1, 1, 1, 1, 1, 1, 1, 1, 1, 1, 1, 1, 1, 1, 1, 1, 1, 1, 1, 1, 1, 1, 1, 1, 1, 1, 1, 1, 1, 1, 1, 1, 1, 1, 1, 1, 1, 1, 1, 1, 1, 1, 1, 1, 1, 1, 1, 1, 1, 1, 1, 1, 1, 1, 1, 1, 1, 1, 1, 1, 1, 1, 1, 1, 1, 1, 1, 1, 1, 1, 1, 1, 1, 1, 1, 1, 1, 1, 1, 1, 1, 1, 1, 1, 1, 1, 1, 1, 1, 1, 1, 1, 1, 1, 1, 1, 1, 1, 1, 1, 1, 1, 1, 1, 1, 1, 1, 1, 1, 1, 1, 1, 1, 1, 1, 1, 1, 1, 1, 1, 1, 1, 1, 1, 1, 1, 1, 1, 1, 1, 1, 1, 1, 1, 1, 1, 1, 1, 1, 1, 1, 1, 1, 1, 1, 1, 1, 1, 1, 1, 1, 4 ),
 ( 0.000000000000000000, 0.5000000000000000000, 1.000000000000000000 ),
 ( 0.000000000000000000, 0.002599942752653872004, 0.005208763852970823248, 0.007813103504395044890, 0.01041666580238601383, 0.01302040446826325734, 0.01562503794709516405, 0.01822898659850798186, 0.02083325479626091381, 0.02343751936515397344, 0.02604147156932860516, 0.02864593660736421826, 0.03124971754428982826, 0.03385421962853985695, 0.03645805019290717514, 0.03906245553539786086, 0.04166655880408994678, 0.04427067902208449424, 0.04687506736766395427, 0.04947890482860387018, 0.05208340383233839299, 0.05468718329397467132, 0.05729165635893663372, 0.05989559287350183087, 0.06249988401580178210, 0.06510415622071820396, 0.06770810475871495704, 0.07031256650665723695, 0.07291634835701975292, 0.07552085129243907291, 0.07812468146351797538, 0.08072908640827750060, 0.08333318980393969455, 0.08593730989448074287, 0.08854169822802662737, 0.09114553558425014801, 0.09375003453682481669, 0.09635381396055957282, 0.09895828689139142542, 0.1015622234206122604, 0.1041665143989399522, 0.1067707866525781646, 0.1093747350801187734, 0.1119791968332524285, 0.1145829786367304204, 0.1171874814968899975, 0.1197913116783300008, 0.1223957164865987768, 0.1249998199429257079, 0.1276039399106482508, 0.1302083283009266290, 0.1328121656006459317, 0.1354166645410730119, 0.1380204439687620910, 0.1406249168095159707, 0.1432288533966223909, 0.1458331442541831724, 0.1484374165996726891, 0.1510413649597071029, 0.1536458267615184170, 0.1562496085608837959, 0.1588541113892728840, 0.1614579416238982879, 0.1640623463390579739, 0.1666664498991252963, 0.1692705697871219883, 0.1718749582774928841, 0.1744787955635339893, 0.1770832945353020271, 0.1796870740097127606, 0.1822915468038420750, 0.1848954834917516388, 0.1874997742717963711, 0.1901040467523684718, 0.1927079950878241021, 0.1953124569817516476, 0.1979162388197689970, 0.2005207416598733527, 0.2031245719904950509, 0.2057289766559125821, 0.2083330803627857220, 0.2109372002141371993, 0.2135415888479497148, 0.2161454261631269858, 0.2187499252097131475, 0.2213537047736018060, 0.2239581775645482220, 0.2265621143961681627, 0.2291664051419355919, 0.2317706778008114532, 0.2343746261546043874, 0.2369790881840763974, 0.2395828701034999064, 0.2421873729987945312, 0.2447912034682135918, 0.2473956081272447038, 0.2499997120239797754, 0.2526038318817556694, 0.2552082207023498306, 0.2578120580894675551, 0.2604165572543392093, 0.2630203369504529598, 0.2656248097816475973, 0.2682287467998764607, 0.2708330375545950908, 0.2734373104349877015, 0.2760412588500244513, 0.2786457210584605826, 0.2812495031020356140, 0.2838540060959860445, 0.2864578367469951536, 0.2890622414429859233, 0.2916663455726313803, 0.2942704654798921071, 0.2968748545306000852, 0.2994786920324540302, 0.3020831913590704687, 0.3046869712301484290, 0.3072914441450140810, 0.3098953813927431966, 0.3124996721996327054, 0.3151039453447485039, 0.3177078938639273376, 0.3203123562947402525, 0.3229161385052047861, 0.3255206416412691484, 0.3281244725166545528, 0.3307288772929431464, 0.3333329816985414751, 0.3359371016983396796, 0.3385414910224879836, 0.3411453286818670882, 0.3437498282136811634, 0.3463536083024566503, 0.3489580813444087548, 0.3515620188645239841, 0.3541663097667969717, 0.3567705832198370119, 0.3593745318860498972, 0.3619789945826469846, 0.3645827770027332826, 0.3671872803243637073, 0.3697911114669067967, 0.3723955163668249413, 0.3749996210914142147, 0.3776037412267966853, 0.3802081308677072724, 0.3828119687273952576, 0.3854164685078552144, 0.3880202488570567709, 0.3906247220695055478, 0.3932286599048890885, 0.3958329509457525486, 0.3984372247499146091, 0.4010411736060487398, 0.4036456366118335581, 0.4062494192842699414, 0.4088539228349143406, 0.4114577542873927851, 0.4140621593542673784, 0.4166662644408827831, 0.4192703847548917562, 0.4218747747558840855, 0.4244786128586610641, 0.4270831129312115948, 0.4296868935835649328, 0.4322913670099168826, 0.4348953052034483235, 0.4374995964261053638, 0.4401038706245853915, 0.4427078197135246862, 0.4453122830718987402, 0.4479160660394111426, 0.4505205698625146526, 0.4531244016677045128, 0.4557288069448597878, 0.4583329124365353446, 0.4609370329722101700, 0.4635414233766025904, 0.4661452617652466213, 0.4687497621733308639, 0.4713535431715604185, 0.4739580168552197104, 0.4765619554497781962, 0.4791662468974299260, 0.4817705215334236457, 0.4843744708980504132, 0.4869789346524148743, 0.4895827179577280641, 0.4921872220967347111, 0.4947910542974118808, 0.4973954598281701278, 0.4999995657679404681, 0.5026036865683194410, 0.5052080774194306345, 0.5078119161367193879, 0.5104164169237808135, 0.5130201983106112973, 0.5156246722949818784, 0.5182286113334474420, 0.5208329030492938605, 0.5234371781659985512, 0.5260411278491948783, 0.5286455920429519173, 0.5312493757287917173, 0.5338538802271461936, 0.5364577128660878991, 0.5390621186937718523, 0.5416662251246735504, 0.5442703462327953545, 0.5468747375739465566, 0.5494785766626585355, 0.5520830778721422805, 0.5546868596903002935, 0.5572913340187868325, 0.5598952735440421158, 0.5624995655712847764, 0.5651038412119004928, 0.5677077912565504647, 0.5703122559331050834, 0.5729160400421993149, 0.5755205449433484777, 0.5781243780633351648, 0.5807287842312690573, 0.5833328911963423513, 0.5859370126552478908, 0.5885414045297637786, 0.5911452440326808722, 0.5937497457080352925, 0.5963535280002507655, 0.5989580027162609843, 0.6015619427711926814, 0.6041662351530351360, 0.6067705113607667622, 0.6093744618097575172, 0.6119789270125192138, 0.6145827115875999169, 0.6171872169349945647, 0.6197910505788110092, 0.6223954571303226269, 0.6249995646726131948, 0.6276036865253464825, 0.6302080789765573954, 0.6328119189364656005, 0.6354164211211439373, 0.6380202039301521300, 0.6406246790770983024, 0.6432286197045988807, 0.6458329124842493441, 0.6484371893023079814, 0.6510411401985315427, 0.6536456059709156996, 0.6562493910547204656, 0.6588538968918166150, 0.6614577311022542538, 0.6640621380806766005, 0.6666662462432366709, 0.6692703685328477148, 0.6718747616040910975, 0.6744786020637821844, 0.6770831048012443398, 0.6796868881697873954, 0.6822913637910873463, 0.6848953050340567117, 0.6874995982547292828, 0.6901038757263339152, 0.6927078271126885234, 0.6953122934981186276, 0.6979160791333920422, 0.7005205855036529261, 0.7031244203235108570, 0.7057288277721832648, 0.7083329365980738368, 0.7109370593676189731, 0.7135414531022405971, 0.7161452941045143294, 0.7187497974382286436, 0.7213535814090563658, 0.7239580575481356917, 0.7265619994494829648, 0.7291662931543987369, 0.7317705713227778963, 0.7343745232421703406, 0.7369789902840787610, 0.7395827765135741805, 0.7421872834604720248, 0.7447911189325585601, 0.7473955268948287989, 0.7499996364271210858, 0.7526037597196653106, 0.7552081541610216053, 0.7578119957486867397, 0.7604164997221309896, 0.7630202843380037292, 0.7656247610382975743, 0.7682287036409420899, 0.7708329978733315935, 0.7734372767817252470, 0.7760412292770711984, 0.7786456970189011839, 0.7812494838853828449, 0.7838539914523996455, 0.7864578276195345330, 0.7890622361387605865, 0.7916663464205372369, 0.7942704702791556493, 0.7968748654706151457, 0.7994787076864910969, 0.8020832123431549388, 0.8046869976468442598, 0.8072914749517984268, 0.8098954182986718431, 0.8124997131017763774, 0.8151039927934364826, 0.8177079459076636025, 0.8203124143928716139, 0.8229162019391148553, 0.8255207101697450423, 0.8281245470747605752, 0.8307289561943111966, 0.8333330672686687368, 0.8359371917364484261, 0.8385415877213925340, 0.8411454306083117061, 0.8437499359916976749, 0.8463537220259882421, 0.8489581999790609679, 0.8515621441131088210, 0.8541664395301816759, 0.8567707200483754004, 0.8593746738244238959, 0.8619791430964799384, 0.8645829313652741988, 0.8671874403030259693, 0.8697912779887684298, 0.8723956877520262498, 0.8749997996620757501, 0.8776039247821166844, 0.8802083216039426894, 0.8828121652047509205, 0.8854166713583762061, 0.8880204581660676721, 0.8906249368107317377, 0.8932288817749149956, 0.8958331778492237829, 0.8984374592372342816, 0.9010414137180589034, 0.9036458838204490807, 0.9062496728545991198, 0.9088541825429954368, 0.9114580210523274273, 0.9140624315026897317, 0.9166665442915585826, 0.9192706701069754960, 0.9218750678090992245, 0.9244789121666602272, 0.9270834191340497910, 0.9296872067579531329, 0.9322916861377325004, 0.9348956319750387767, 0.9374999287497546296, 0.9401042110508202043, 0.9427081662796877870, 0.9453126372565492375, 0.9479164270979697493, 0.9505209375757615042, 0.9531247769568838013, 0.9557291881641908349, 0.9583333018366511080, 0.9609374282806871781, 0.9635418271385329803, 0.9661456726567504427, 0.9687501794391485399, 0.9713539669241311181, 0.9739584505366999378, 0.9765624007674321705, 0.9791666904763859369, 0.9817709514985233366, 0.9843749191276834898, 0.9869795472165283634, 0.9895832986789295793, 0.9921868791097946394, 0.9947912178632822844, 0.9974000636350187632, 1.000000000000000000 ),
 .UNSPECIFIED. ) 
 GEOMETRIC_REPRESENTATION_ITEM ( )  RATIONAL_B_SPLINE_SURFACE ( (
 ( 1.000000000000000222, 1.000000000000000222, 1.000000000000000444, 1.000000000000000000, 1.000000000000000444, 1.000000000000000222, 1.000000000000000444, 0.9999999999999997780, 1.000000000000000444, 1.000000000000000000, 1.000000000000000444, 1.000000000000000000, 1.000000000000000444, 1.000000000000000222, 1.000000000000000000, 1.000000000000000666, 0.9999999999999997780, 1.000000000000000444, 1.000000000000000444, 1.000000000000000444, 1.000000000000000222, 1.000000000000000222, 1.000000000000000444, 1.000000000000000444, 1.000000000000000000, 1.000000000000000222, 1.000000000000000222, 1.000000000000000444, 1.000000000000000222, 1.000000000000000444, 1.000000000000000000, 1.000000000000000222, 1.000000000000000444, 1.000000000000000000, 1.000000000000000444, 1.000000000000000222, 1.000000000000000444, 1.000000000000000444, 1.000000000000000222, 1.000000000000000000, 1.000000000000000444, 1.000000000000000222, 1.000000000000000000, 1.000000000000000222, 1.000000000000000444, 1.000000000000000444, 1.000000000000000444, 1.000000000000000444, 1.000000000000000222, 1.000000000000000444, 1.000000000000000000, 1.000000000000000444, 1.000000000000000222, 1.000000000000000222, 1.000000000000000444, 1.000000000000000000, 1.000000000000000222, 1.000000000000000444, 1.000000000000000222, 1.000000000000000000, 1.000000000000000444, 1.000000000000000222, 1.000000000000000222, 1.000000000000000000, 1.000000000000000444, 0.9999999999999997780, 1.000000000000000444, 1.000000000000000000, 1.000000000000000444, 1.000000000000000000, 1.000000000000000444, 0.9999999999999997780, 1.000000000000000222, 1.000000000000000444, 1.000000000000000444, 1.000000000000000000, 1.000000000000000444, 1.000000000000000222, 1.000000000000000000, 1.000000000000000666, 1.000000000000000000, 1.000000000000000444, 1.000000000000000222, 1.000000000000000444, 0.9999999999999997780, 1.000000000000000444, 1.000000000000000000, 1.000000000000000444, 1.000000000000000444, 1.000000000000000222, 1.000000000000000222, 1.000000000000000444, 1.000000000000000222, 1.000000000000000444, 1.000000000000000444, 1.000000000000000222, 1.000000000000000444, 1.000000000000000222, 1.000000000000000444, 1.000000000000000000, 1.000000000000000444, 1.000000000000000000, 1.000000000000000000, 1.000000000000000444, 1.000000000000000222, 1.000000000000000222, 1.000000000000000444, 1.000000000000000000, 1.000000000000000444, 1.000000000000000000, 1.000000000000000222, 1.000000000000000444, 0.9999999999999997780, 1.000000000000000444, 1.000000000000000222, 1.000000000000000444, 1.000000000000000000, 1.000000000000000444, 1.000000000000000000, 1.000000000000000222, 1.000000000000000222, 1.000000000000000444, 1.000000000000000222, 1.000000000000000000, 1.000000000000000444, 1.000000000000000222, 1.000000000000000222, 1.000000000000000222, 1.000000000000000444, 0.9999999999999997780, 1.000000000000000666, 0.9999999999999996669, 1.000000000000000444, 1.000000000000000444, 1.000000000000000222, 1.000000000000000444, 1.000000000000000444, 1.000000000000000222, 1.000000000000000000, 1.000000000000000444, 1.000000000000000000, 1.000000000000000444, 1.000000000000000222, 1.000000000000000444, 1.000000000000000000, 1.000000000000000444, 1.000000000000000222, 1.000000000000000222, 1.000000000000000444, 1.000000000000000222, 0.9999999999999997780, 1.000000000000000444, 1.000000000000000444, 1.000000000000000444, 1.000000000000000222, 1.000000000000000444, 1.000000000000000444, 1.000000000000000222, 1.000000000000000444, 1.000000000000000000, 1.000000000000000222, 1.000000000000000444, 1.000000000000000000, 1.000000000000000222, 1.000000000000000444, 1.000000000000000000, 1.000000000000000444, 0.9999999999999997780, 1.000000000000000222, 1.000000000000000444, 1.000000000000000000, 1.000000000000000222, 1.000000000000000222, 1.000000000000000444, 1.000000000000000000, 1.000000000000000666, 0.9999999999999996669, 1.000000000000000666, 1.000000000000000222, 1.000000000000000444, 1.000000000000000222, 1.000000000000000444, 1.000000000000000222, 1.000000000000000222, 1.000000000000000000, 1.000000000000000444, 0.9999999999999997780, 1.000000000000000444, 1.000000000000000222, 1.000000000000000444, 0.9999999999999997780, 1.000000000000000444, 1.000000000000000000, 1.000000000000000222, 1.000000000000000444, 1.000000000000000000, 1.000000000000000444, 1.000000000000000444, 1.000000000000000222, 1.000000000000000222, 1.000000000000000000, 1.000000000000000444, 1.000000000000000444, 1.000000000000000000, 1.000000000000000222, 1.000000000000000222, 1.000000000000000444, 1.000000000000000222, 1.000000000000000222, 1.000000000000000444, 1.000000000000000222, 1.000000000000000000, 1.000000000000000444, 1.000000000000000000, 1.000000000000000222, 1.000000000000000444, 1.000000000000000222, 1.000000000000000222, 1.000000000000000444, 1.000000000000000000, 1.000000000000000222, 1.000000000000000222, 1.000000000000000222, 1.000000000000000000, 1.000000000000000222, 1.000000000000000222, 1.000000000000000000, 1.000000000000000222, 1.000000000000000222, 1.000000000000000444, 1.000000000000000000, 1.000000000000000000, 1.000000000000000222, 1.000000000000000000, 1.000000000000000888, 1.000000000000000000, 1.000000000000000444, 1.000000000000000222, 1.000000000000000222, 1.000000000000000444, 1.000000000000000222, 1.000000000000000222, 1.000000000000000444, 1.000000000000000444, 1.000000000000000222, 1.000000000000000444, 1.000000000000000222, 1.000000000000000000, 1.000000000000000222, 1.000000000000000444, 1.000000000000000444, 1.000000000000000222, 1.000000000000000444, 1.000000000000000222, 1.000000000000000444, 1.000000000000000222, 1.000000000000000444, 1.000000000000000222, 1.000000000000000000, 1.000000000000000444, 1.000000000000000000, 1.000000000000000666, 1.000000000000000000, 1.000000000000000000, 1.000000000000000444, 1.000000000000000222, 1.000000000000000444, 0.9999999999999997780, 1.000000000000000666, 1.000000000000000222, 1.000000000000000444, 1.000000000000000222, 1.000000000000000444, 1.000000000000000222, 1.000000000000000444, 0.9999999999999997780, 1.000000000000000666, 1.000000000000000222, 1.000000000000000222, 1.000000000000000444, 1.000000000000000444, 0.9999999999999997780, 1.000000000000000444, 1.000000000000000222, 1.000000000000000222, 1.000000000000000000, 1.000000000000000000, 1.000000000000000444, 1.000000000000000444, 1.000000000000000222, 1.000000000000000000, 1.000000000000000444, 0.9999999999999997780, 1.000000000000000444, 1.000000000000000222, 1.000000000000000000, 1.000000000000000222, 1.000000000000000000, 1.000000000000000444, 1.000000000000000000, 1.000000000000000444, 1.000000000000000222, 1.000000000000000222, 1.000000000000000222, 1.000000000000000222, 1.000000000000000222, 1.000000000000000444, 1.000000000000000222, 1.000000000000000444, 1.000000000000000222, 1.000000000000000000, 1.000000000000000888, 0.9999999999999996669, 1.000000000000000444, 1.000000000000000444, 1.000000000000000222, 1.000000000000000444, 1.000000000000000000, 1.000000000000000444, 0.9999999999999997780, 1.000000000000000444, 1.000000000000000222, 1.000000000000000444, 0.9999999999999997780, 1.000000000000000222, 1.000000000000000222, 1.000000000000000444, 1.000000000000000000, 1.000000000000000444, 1.000000000000000444, 1.000000000000000222, 1.000000000000000000, 1.000000000000000444, 1.000000000000000000, 1.000000000000000222, 1.000000000000000222, 1.000000000000000444, 1.000000000000000000, 1.000000000000000666, 1.000000000000000000, 1.000000000000000444, 1.000000000000000222, 1.000000000000000444, 1.000000000000000222, 1.000000000000000444, 1.000000000000000222, 1.000000000000000222, 1.000000000000000222, 1.000000000000000444, 1.000000000000000444, 1.000000000000000222, 1.000000000000000000, 1.000000000000000444, 1.000000000000000444, 1.000000000000000000, 1.000000000000000444, 0.9999999999999997780, 1.000000000000000444, 1.000000000000000222, 1.000000000000000222, 1.000000000000000444, 1.000000000000000222, 1.000000000000000222, 1.000000000000000444, 1.000000000000000444, 1.000000000000000444, 1.000000000000000000, 1.000000000000000444, 1.000000000000000222, 1.000000000000000222, 1.000000000000000000, 1.000000000000000444, 0.9999999999999997780, 1.000000000000000444, 1.000000000000000000, 1.000000000000000444, 1.000000000000000000, 1.000000000000000444, 1.000000000000000222, 1.000000000000000000, 1.000000000000000444, 1.000000000000000222, 1.000000000000000444, 0.9999999999999997780, 1.000000000000000444, 1.000000000000000222, 1.000000000000000222),
 ( 0.3333333333333334259, 0.3333333333333334259, 0.3333333333333334814, 0.3333333333333333703, 0.3333333333333335369, 0.3333333333333334259, 0.3333333333333334814, 0.3333333333333333703, 0.3333333333333334259, 0.3333333333333333703, 0.3333333333333335369, 0.3333333333333333703, 0.3333333333333334259, 0.3333333333333334259, 0.3333333333333333703, 0.3333333333333335369, 0.3333333333333333703, 0.3333333333333334259, 0.3333333333333335369, 0.3333333333333334259, 0.3333333333333333703, 0.3333333333333334259, 0.3333333333333334814, 0.3333333333333335369, 0.3333333333333333148, 0.3333333333333334259, 0.3333333333333334259, 0.3333333333333334814, 0.3333333333333334259, 0.3333333333333334259, 0.3333333333333334259, 0.3333333333333333148, 0.3333333333333335924, 0.3333333333333333148, 0.3333333333333335369, 0.3333333333333333703, 0.3333333333333335369, 0.3333333333333334259, 0.3333333333333333703, 0.3333333333333333703, 0.3333333333333335924, 0.3333333333333333148, 0.3333333333333334259, 0.3333333333333334259, 0.3333333333333335369, 0.3333333333333334814, 0.3333333333333334259, 0.3333333333333334259, 0.3333333333333334259, 0.3333333333333334259, 0.3333333333333333703, 0.3333333333333335369, 0.3333333333333334259, 0.3333333333333334259, 0.3333333333333334814, 0.3333333333333333703, 0.3333333333333333703, 0.3333333333333334814, 0.3333333333333334259, 0.3333333333333333703, 0.3333333333333334814, 0.3333333333333333703, 0.3333333333333334814, 0.3333333333333332593, 0.3333333333333335924, 0.3333333333333333148, 0.3333333333333335924, 0.3333333333333333148, 0.3333333333333335924, 0.3333333333333334259, 0.3333333333333334814, 0.3333333333333333703, 0.3333333333333333703, 0.3333333333333334814, 0.3333333333333335369, 0.3333333333333333703, 0.3333333333333334814, 0.3333333333333334259, 0.3333333333333333703, 0.3333333333333335369, 0.3333333333333333148, 0.3333333333333335369, 0.3333333333333334259, 0.3333333333333334259, 0.3333333333333333703, 0.3333333333333334259, 0.3333333333333333703, 0.3333333333333335369, 0.3333333333333333703, 0.3333333333333334259, 0.3333333333333334259, 0.3333333333333334814, 0.3333333333333333703, 0.3333333333333335924, 0.3333333333333333703, 0.3333333333333334259, 0.3333333333333334814, 0.3333333333333334259, 0.3333333333333335369, 0.3333333333333333148, 0.3333333333333335369, 0.3333333333333333148, 0.3333333333333334259, 0.3333333333333333703, 0.3333333333333334259, 0.3333333333333334259, 0.3333333333333335924, 0.3333333333333333703, 0.3333333333333335924, 0.3333333333333333148, 0.3333333333333335369, 0.3333333333333335369, 0.3333333333333333148, 0.3333333333333334259, 0.3333333333333334259, 0.3333333333333334814, 0.3333333333333333703, 0.3333333333333335369, 0.3333333333333333703, 0.3333333333333333703, 0.3333333333333334814, 0.3333333333333334814, 0.3333333333333334259, 0.3333333333333333703, 0.3333333333333334814, 0.3333333333333334814, 0.3333333333333334259, 0.3333333333333334259, 0.3333333333333334259, 0.3333333333333333703, 0.3333333333333335369, 0.3333333333333333703, 0.3333333333333334259, 0.3333333333333334814, 0.3333333333333334259, 0.3333333333333334814, 0.3333333333333334259, 0.3333333333333333703, 0.3333333333333333703, 0.3333333333333334259, 0.3333333333333333148, 0.3333333333333334814, 0.3333333333333334814, 0.3333333333333334259, 0.3333333333333333703, 0.3333333333333334259, 0.3333333333333334259, 0.3333333333333333703, 0.3333333333333335369, 0.3333333333333334259, 0.3333333333333333148, 0.3333333333333333703, 0.3333333333333335369, 0.3333333333333335369, 0.3333333333333333148, 0.3333333333333335369, 0.3333333333333334259, 0.3333333333333334259, 0.3333333333333335369, 0.3333333333333333703, 0.3333333333333333703, 0.3333333333333334259, 0.3333333333333333703, 0.3333333333333334259, 0.3333333333333334259, 0.3333333333333333703, 0.3333333333333335369, 0.3333333333333333703, 0.3333333333333334259, 0.3333333333333335369, 0.3333333333333333703, 0.3333333333333333703, 0.3333333333333334814, 0.3333333333333334259, 0.3333333333333333703, 0.3333333333333335369, 0.3333333333333332593, 0.3333333333333335369, 0.3333333333333335369, 0.3333333333333333703, 0.3333333333333334814, 0.3333333333333334814, 0.3333333333333334259, 0.3333333333333333703, 0.3333333333333334259, 0.3333333333333334814, 0.3333333333333333148, 0.3333333333333335369, 0.3333333333333333703, 0.3333333333333334259, 0.3333333333333333703, 0.3333333333333334259, 0.3333333333333333148, 0.3333333333333334259, 0.3333333333333334814, 0.3333333333333333703, 0.3333333333333334814, 0.3333333333333334259, 0.3333333333333333703, 0.3333333333333334259, 0.3333333333333333703, 0.3333333333333334259, 0.3333333333333334814, 0.3333333333333332593, 0.3333333333333334259, 0.3333333333333333703, 0.3333333333333335369, 0.3333333333333334259, 0.3333333333333333703, 0.3333333333333334259, 0.3333333333333334259, 0.3333333333333333148, 0.3333333333333335369, 0.3333333333333333703, 0.3333333333333334259, 0.3333333333333335924, 0.3333333333333333703, 0.3333333333333334259, 0.3333333333333335369, 0.3333333333333333703, 0.3333333333333334259, 0.3333333333333334259, 0.3333333333333334259, 0.3333333333333333703, 0.3333333333333334259, 0.3333333333333334259, 0.3333333333333333703, 0.3333333333333333148, 0.3333333333333334814, 0.3333333333333334259, 0.3333333333333334259, 0.3333333333333333703, 0.3333333333333333703, 0.3333333333333334259, 0.3333333333333335369, 0.3333333333333333703, 0.3333333333333335369, 0.3333333333333333703, 0.3333333333333334259, 0.3333333333333335369, 0.3333333333333333148, 0.3333333333333334259, 0.3333333333333334814, 0.3333333333333335369, 0.3333333333333333148, 0.3333333333333335369, 0.3333333333333333703, 0.3333333333333334259, 0.3333333333333333703, 0.3333333333333335369, 0.3333333333333334259, 0.3333333333333334259, 0.3333333333333334259, 0.3333333333333333703, 0.3333333333333335924, 0.3333333333333334259, 0.3333333333333335369, 0.3333333333333333148, 0.3333333333333333703, 0.3333333333333334814, 0.3333333333333333703, 0.3333333333333335924, 0.3333333333333333148, 0.3333333333333333703, 0.3333333333333335369, 0.3333333333333333703, 0.3333333333333335924, 0.3333333333333332593, 0.3333333333333335924, 0.3333333333333334259, 0.3333333333333335369, 0.3333333333333334259, 0.3333333333333334814, 0.3333333333333333703, 0.3333333333333334814, 0.3333333333333333148, 0.3333333333333335369, 0.3333333333333333148, 0.3333333333333334814, 0.3333333333333334814, 0.3333333333333334814, 0.3333333333333333148, 0.3333333333333335369, 0.3333333333333333148, 0.3333333333333335369, 0.3333333333333333703, 0.3333333333333333703, 0.3333333333333335369, 0.3333333333333334259, 0.3333333333333334259, 0.3333333333333333703, 0.3333333333333335369, 0.3333333333333333148, 0.3333333333333335924, 0.3333333333333334259, 0.3333333333333334259, 0.3333333333333333703, 0.3333333333333333703, 0.3333333333333334259, 0.3333333333333334259, 0.3333333333333334259, 0.3333333333333334259, 0.3333333333333334259, 0.3333333333333334259, 0.3333333333333334259, 0.3333333333333333703, 0.3333333333333335369, 0.3333333333333333703, 0.3333333333333334814, 0.3333333333333333703, 0.3333333333333333148, 0.3333333333333337034, 0.3333333333333332038, 0.3333333333333334814, 0.3333333333333335369, 0.3333333333333334814, 0.3333333333333334259, 0.3333333333333334259, 0.3333333333333334814, 0.3333333333333333703, 0.3333333333333334814, 0.3333333333333334259, 0.3333333333333334814, 0.3333333333333333148, 0.3333333333333333703, 0.3333333333333335369, 0.3333333333333334259, 0.3333333333333333703, 0.3333333333333335369, 0.3333333333333334814, 0.3333333333333334259, 0.3333333333333333703, 0.3333333333333334259, 0.3333333333333333148, 0.3333333333333335369, 0.3333333333333333148, 0.3333333333333335369, 0.3333333333333333703, 0.3333333333333335369, 0.3333333333333334259, 0.3333333333333334814, 0.3333333333333334259, 0.3333333333333335369, 0.3333333333333334259, 0.3333333333333334259, 0.3333333333333333703, 0.3333333333333334259, 0.3333333333333333703, 0.3333333333333335369, 0.3333333333333334814, 0.3333333333333333703, 0.3333333333333333148, 0.3333333333333335369, 0.3333333333333333703, 0.3333333333333333703, 0.3333333333333334814, 0.3333333333333333148, 0.3333333333333334814, 0.3333333333333333703, 0.3333333333333334259, 0.3333333333333334814, 0.3333333333333334814, 0.3333333333333334259, 0.3333333333333334259, 0.3333333333333335369, 0.3333333333333334814, 0.3333333333333333148, 0.3333333333333335369, 0.3333333333333334259, 0.3333333333333333703, 0.3333333333333334259, 0.3333333333333334259, 0.3333333333333333148, 0.3333333333333334814, 0.3333333333333333703, 0.3333333333333334259, 0.3333333333333333148, 0.3333333333333334814, 0.3333333333333334259, 0.3333333333333333148, 0.3333333333333334814, 0.3333333333333334259, 0.3333333333333334814, 0.3333333333333332593, 0.3333333333333335924, 0.3333333333333334259, 0.3333333333333334259),
 ( 0.3333333333333334259, 0.3333333333333334259, 0.3333333333333334814, 0.3333333333333333703, 0.3333333333333335369, 0.3333333333333334259, 0.3333333333333334814, 0.3333333333333333703, 0.3333333333333334259, 0.3333333333333333703, 0.3333333333333335369, 0.3333333333333333703, 0.3333333333333334259, 0.3333333333333334259, 0.3333333333333333703, 0.3333333333333335369, 0.3333333333333333703, 0.3333333333333334259, 0.3333333333333335369, 0.3333333333333334259, 0.3333333333333333703, 0.3333333333333334259, 0.3333333333333334814, 0.3333333333333335369, 0.3333333333333333148, 0.3333333333333334259, 0.3333333333333334259, 0.3333333333333334814, 0.3333333333333334259, 0.3333333333333334259, 0.3333333333333334259, 0.3333333333333333148, 0.3333333333333335924, 0.3333333333333333148, 0.3333333333333335369, 0.3333333333333333703, 0.3333333333333335369, 0.3333333333333334259, 0.3333333333333333703, 0.3333333333333333703, 0.3333333333333335924, 0.3333333333333333148, 0.3333333333333334259, 0.3333333333333334259, 0.3333333333333335369, 0.3333333333333334814, 0.3333333333333334259, 0.3333333333333334259, 0.3333333333333334259, 0.3333333333333334259, 0.3333333333333333703, 0.3333333333333335369, 0.3333333333333334259, 0.3333333333333334259, 0.3333333333333334814, 0.3333333333333333703, 0.3333333333333333703, 0.3333333333333334814, 0.3333333333333334259, 0.3333333333333333703, 0.3333333333333334814, 0.3333333333333333703, 0.3333333333333334814, 0.3333333333333332593, 0.3333333333333335924, 0.3333333333333333148, 0.3333333333333335924, 0.3333333333333333148, 0.3333333333333335924, 0.3333333333333334259, 0.3333333333333334814, 0.3333333333333333703, 0.3333333333333333703, 0.3333333333333334814, 0.3333333333333335369, 0.3333333333333333703, 0.3333333333333334814, 0.3333333333333334259, 0.3333333333333333703, 0.3333333333333335369, 0.3333333333333333148, 0.3333333333333335369, 0.3333333333333334259, 0.3333333333333334259, 0.3333333333333333703, 0.3333333333333334259, 0.3333333333333333703, 0.3333333333333335369, 0.3333333333333333703, 0.3333333333333334259, 0.3333333333333334259, 0.3333333333333334814, 0.3333333333333333703, 0.3333333333333335924, 0.3333333333333333703, 0.3333333333333334259, 0.3333333333333334814, 0.3333333333333334259, 0.3333333333333335369, 0.3333333333333333148, 0.3333333333333335369, 0.3333333333333333148, 0.3333333333333334259, 0.3333333333333333703, 0.3333333333333334259, 0.3333333333333334259, 0.3333333333333335924, 0.3333333333333333703, 0.3333333333333335924, 0.3333333333333333148, 0.3333333333333335369, 0.3333333333333335369, 0.3333333333333333148, 0.3333333333333334259, 0.3333333333333334259, 0.3333333333333334814, 0.3333333333333333703, 0.3333333333333335369, 0.3333333333333333703, 0.3333333333333333703, 0.3333333333333334814, 0.3333333333333334814, 0.3333333333333334259, 0.3333333333333333703, 0.3333333333333334814, 0.3333333333333334814, 0.3333333333333334259, 0.3333333333333334259, 0.3333333333333334259, 0.3333333333333333703, 0.3333333333333335369, 0.3333333333333333703, 0.3333333333333334259, 0.3333333333333334814, 0.3333333333333334259, 0.3333333333333334814, 0.3333333333333334259, 0.3333333333333333703, 0.3333333333333333703, 0.3333333333333334259, 0.3333333333333333148, 0.3333333333333334814, 0.3333333333333334814, 0.3333333333333334259, 0.3333333333333333703, 0.3333333333333334259, 0.3333333333333334259, 0.3333333333333333703, 0.3333333333333335369, 0.3333333333333334259, 0.3333333333333333148, 0.3333333333333333703, 0.3333333333333335369, 0.3333333333333335369, 0.3333333333333333148, 0.3333333333333335369, 0.3333333333333334259, 0.3333333333333334259, 0.3333333333333335369, 0.3333333333333333703, 0.3333333333333333703, 0.3333333333333334259, 0.3333333333333333703, 0.3333333333333334259, 0.3333333333333334259, 0.3333333333333333703, 0.3333333333333335369, 0.3333333333333333703, 0.3333333333333334259, 0.3333333333333335369, 0.3333333333333333703, 0.3333333333333333703, 0.3333333333333334814, 0.3333333333333334259, 0.3333333333333333703, 0.3333333333333335369, 0.3333333333333332593, 0.3333333333333335369, 0.3333333333333335369, 0.3333333333333333703, 0.3333333333333334814, 0.3333333333333334814, 0.3333333333333334259, 0.3333333333333333703, 0.3333333333333334259, 0.3333333333333334814, 0.3333333333333333148, 0.3333333333333335369, 0.3333333333333333703, 0.3333333333333334259, 0.3333333333333333703, 0.3333333333333334259, 0.3333333333333333148, 0.3333333333333334259, 0.3333333333333334814, 0.3333333333333333703, 0.3333333333333334814, 0.3333333333333334259, 0.3333333333333333703, 0.3333333333333334259, 0.3333333333333333703, 0.3333333333333334259, 0.3333333333333334814, 0.3333333333333332593, 0.3333333333333334259, 0.3333333333333333703, 0.3333333333333335369, 0.3333333333333334259, 0.3333333333333333703, 0.3333333333333334259, 0.3333333333333334259, 0.3333333333333333148, 0.3333333333333335369, 0.3333333333333333703, 0.3333333333333334259, 0.3333333333333335924, 0.3333333333333333703, 0.3333333333333334259, 0.3333333333333335369, 0.3333333333333333703, 0.3333333333333334259, 0.3333333333333334259, 0.3333333333333334259, 0.3333333333333333703, 0.3333333333333334259, 0.3333333333333334259, 0.3333333333333333703, 0.3333333333333333148, 0.3333333333333334814, 0.3333333333333334259, 0.3333333333333334259, 0.3333333333333333703, 0.3333333333333333703, 0.3333333333333334259, 0.3333333333333335369, 0.3333333333333333703, 0.3333333333333335369, 0.3333333333333333703, 0.3333333333333334259, 0.3333333333333335369, 0.3333333333333333148, 0.3333333333333334259, 0.3333333333333334814, 0.3333333333333335369, 0.3333333333333333148, 0.3333333333333335369, 0.3333333333333333703, 0.3333333333333334259, 0.3333333333333333703, 0.3333333333333335369, 0.3333333333333334259, 0.3333333333333334259, 0.3333333333333334259, 0.3333333333333333703, 0.3333333333333335924, 0.3333333333333334259, 0.3333333333333335369, 0.3333333333333333148, 0.3333333333333333703, 0.3333333333333334814, 0.3333333333333333703, 0.3333333333333335924, 0.3333333333333333148, 0.3333333333333333703, 0.3333333333333335369, 0.3333333333333333703, 0.3333333333333335924, 0.3333333333333332593, 0.3333333333333335924, 0.3333333333333334259, 0.3333333333333335369, 0.3333333333333334259, 0.3333333333333334814, 0.3333333333333333703, 0.3333333333333334814, 0.3333333333333333148, 0.3333333333333335369, 0.3333333333333333148, 0.3333333333333334814, 0.3333333333333334814, 0.3333333333333334814, 0.3333333333333333148, 0.3333333333333335369, 0.3333333333333333148, 0.3333333333333335369, 0.3333333333333333703, 0.3333333333333333703, 0.3333333333333335369, 0.3333333333333334259, 0.3333333333333334259, 0.3333333333333333703, 0.3333333333333335369, 0.3333333333333333148, 0.3333333333333335924, 0.3333333333333334259, 0.3333333333333334259, 0.3333333333333333703, 0.3333333333333333703, 0.3333333333333334259, 0.3333333333333334259, 0.3333333333333334259, 0.3333333333333334259, 0.3333333333333334259, 0.3333333333333334259, 0.3333333333333334259, 0.3333333333333333703, 0.3333333333333335369, 0.3333333333333333703, 0.3333333333333334814, 0.3333333333333333703, 0.3333333333333333148, 0.3333333333333337034, 0.3333333333333332038, 0.3333333333333334814, 0.3333333333333335369, 0.3333333333333334814, 0.3333333333333334259, 0.3333333333333334259, 0.3333333333333334814, 0.3333333333333333703, 0.3333333333333334814, 0.3333333333333334259, 0.3333333333333334814, 0.3333333333333333148, 0.3333333333333333703, 0.3333333333333335369, 0.3333333333333334259, 0.3333333333333333703, 0.3333333333333335369, 0.3333333333333334814, 0.3333333333333334259, 0.3333333333333333703, 0.3333333333333334259, 0.3333333333333333148, 0.3333333333333335369, 0.3333333333333333148, 0.3333333333333335369, 0.3333333333333333703, 0.3333333333333335369, 0.3333333333333334259, 0.3333333333333334814, 0.3333333333333334259, 0.3333333333333335369, 0.3333333333333334259, 0.3333333333333334259, 0.3333333333333333703, 0.3333333333333334259, 0.3333333333333333703, 0.3333333333333335369, 0.3333333333333334814, 0.3333333333333333703, 0.3333333333333333148, 0.3333333333333335369, 0.3333333333333333703, 0.3333333333333333703, 0.3333333333333334814, 0.3333333333333333148, 0.3333333333333334814, 0.3333333333333333703, 0.3333333333333334259, 0.3333333333333334814, 0.3333333333333334814, 0.3333333333333334259, 0.3333333333333334259, 0.3333333333333335369, 0.3333333333333334814, 0.3333333333333333148, 0.3333333333333335369, 0.3333333333333334259, 0.3333333333333333703, 0.3333333333333334259, 0.3333333333333334259, 0.3333333333333333148, 0.3333333333333334814, 0.3333333333333333703, 0.3333333333333334259, 0.3333333333333333148, 0.3333333333333334814, 0.3333333333333334259, 0.3333333333333333148, 0.3333333333333334814, 0.3333333333333334259, 0.3333333333333334814, 0.3333333333333332593, 0.3333333333333335924, 0.3333333333333334259, 0.3333333333333334259),
 ( 1.000000000000000222, 1.000000000000000222, 1.000000000000000444, 1.000000000000000000, 1.000000000000000444, 1.000000000000000222, 1.000000000000000444, 0.9999999999999997780, 1.000000000000000444, 1.000000000000000000, 1.000000000000000444, 1.000000000000000000, 1.000000000000000444, 1.000000000000000222, 1.000000000000000000, 1.000000000000000666, 0.9999999999999997780, 1.000000000000000444, 1.000000000000000444, 1.000000000000000444, 1.000000000000000222, 1.000000000000000222, 1.000000000000000444, 1.000000000000000444, 1.000000000000000000, 1.000000000000000222, 1.000000000000000222, 1.000000000000000444, 1.000000000000000222, 1.000000000000000444, 1.000000000000000000, 1.000000000000000222, 1.000000000000000444, 1.000000000000000000, 1.000000000000000444, 1.000000000000000222, 1.000000000000000444, 1.000000000000000444, 1.000000000000000222, 1.000000000000000000, 1.000000000000000444, 1.000000000000000222, 1.000000000000000000, 1.000000000000000222, 1.000000000000000444, 1.000000000000000444, 1.000000000000000444, 1.000000000000000444, 1.000000000000000222, 1.000000000000000444, 1.000000000000000000, 1.000000000000000444, 1.000000000000000222, 1.000000000000000222, 1.000000000000000444, 1.000000000000000000, 1.000000000000000222, 1.000000000000000444, 1.000000000000000222, 1.000000000000000000, 1.000000000000000444, 1.000000000000000222, 1.000000000000000222, 1.000000000000000000, 1.000000000000000444, 0.9999999999999997780, 1.000000000000000444, 1.000000000000000000, 1.000000000000000444, 1.000000000000000000, 1.000000000000000444, 0.9999999999999997780, 1.000000000000000222, 1.000000000000000444, 1.000000000000000444, 1.000000000000000000, 1.000000000000000444, 1.000000000000000222, 1.000000000000000000, 1.000000000000000666, 1.000000000000000000, 1.000000000000000444, 1.000000000000000222, 1.000000000000000444, 0.9999999999999997780, 1.000000000000000444, 1.000000000000000000, 1.000000000000000444, 1.000000000000000444, 1.000000000000000222, 1.000000000000000222, 1.000000000000000444, 1.000000000000000222, 1.000000000000000444, 1.000000000000000444, 1.000000000000000222, 1.000000000000000444, 1.000000000000000222, 1.000000000000000444, 1.000000000000000000, 1.000000000000000444, 1.000000000000000000, 1.000000000000000000, 1.000000000000000444, 1.000000000000000222, 1.000000000000000222, 1.000000000000000444, 1.000000000000000000, 1.000000000000000444, 1.000000000000000000, 1.000000000000000222, 1.000000000000000444, 0.9999999999999997780, 1.000000000000000444, 1.000000000000000222, 1.000000000000000444, 1.000000000000000000, 1.000000000000000444, 1.000000000000000000, 1.000000000000000222, 1.000000000000000222, 1.000000000000000444, 1.000000000000000222, 1.000000000000000000, 1.000000000000000444, 1.000000000000000222, 1.000000000000000222, 1.000000000000000222, 1.000000000000000444, 0.9999999999999997780, 1.000000000000000666, 0.9999999999999996669, 1.000000000000000444, 1.000000000000000444, 1.000000000000000222, 1.000000000000000444, 1.000000000000000444, 1.000000000000000222, 1.000000000000000000, 1.000000000000000444, 1.000000000000000000, 1.000000000000000444, 1.000000000000000222, 1.000000000000000444, 1.000000000000000000, 1.000000000000000444, 1.000000000000000222, 1.000000000000000222, 1.000000000000000444, 1.000000000000000222, 0.9999999999999997780, 1.000000000000000444, 1.000000000000000444, 1.000000000000000444, 1.000000000000000222, 1.000000000000000444, 1.000000000000000444, 1.000000000000000222, 1.000000000000000444, 1.000000000000000000, 1.000000000000000222, 1.000000000000000444, 1.000000000000000000, 1.000000000000000222, 1.000000000000000444, 1.000000000000000000, 1.000000000000000444, 0.9999999999999997780, 1.000000000000000222, 1.000000000000000444, 1.000000000000000000, 1.000000000000000222, 1.000000000000000222, 1.000000000000000444, 1.000000000000000000, 1.000000000000000666, 0.9999999999999996669, 1.000000000000000666, 1.000000000000000222, 1.000000000000000444, 1.000000000000000222, 1.000000000000000444, 1.000000000000000222, 1.000000000000000222, 1.000000000000000000, 1.000000000000000444, 0.9999999999999997780, 1.000000000000000444, 1.000000000000000222, 1.000000000000000444, 0.9999999999999997780, 1.000000000000000444, 1.000000000000000000, 1.000000000000000222, 1.000000000000000444, 1.000000000000000000, 1.000000000000000444, 1.000000000000000444, 1.000000000000000222, 1.000000000000000222, 1.000000000000000000, 1.000000000000000444, 1.000000000000000444, 1.000000000000000000, 1.000000000000000222, 1.000000000000000222, 1.000000000000000444, 1.000000000000000222, 1.000000000000000222, 1.000000000000000444, 1.000000000000000222, 1.000000000000000000, 1.000000000000000444, 1.000000000000000000, 1.000000000000000222, 1.000000000000000444, 1.000000000000000222, 1.000000000000000222, 1.000000000000000444, 1.000000000000000000, 1.000000000000000222, 1.000000000000000222, 1.000000000000000222, 1.000000000000000000, 1.000000000000000222, 1.000000000000000222, 1.000000000000000000, 1.000000000000000222, 1.000000000000000222, 1.000000000000000444, 1.000000000000000000, 1.000000000000000000, 1.000000000000000222, 1.000000000000000000, 1.000000000000000888, 1.000000000000000000, 1.000000000000000444, 1.000000000000000222, 1.000000000000000222, 1.000000000000000444, 1.000000000000000222, 1.000000000000000222, 1.000000000000000444, 1.000000000000000444, 1.000000000000000222, 1.000000000000000444, 1.000000000000000222, 1.000000000000000000, 1.000000000000000222, 1.000000000000000444, 1.000000000000000444, 1.000000000000000222, 1.000000000000000444, 1.000000000000000222, 1.000000000000000444, 1.000000000000000222, 1.000000000000000444, 1.000000000000000222, 1.000000000000000000, 1.000000000000000444, 1.000000000000000000, 1.000000000000000666, 1.000000000000000000, 1.000000000000000000, 1.000000000000000444, 1.000000000000000222, 1.000000000000000444, 0.9999999999999997780, 1.000000000000000666, 1.000000000000000222, 1.000000000000000444, 1.000000000000000222, 1.000000000000000444, 1.000000000000000222, 1.000000000000000444, 0.9999999999999997780, 1.000000000000000666, 1.000000000000000222, 1.000000000000000222, 1.000000000000000444, 1.000000000000000444, 0.9999999999999997780, 1.000000000000000444, 1.000000000000000222, 1.000000000000000222, 1.000000000000000000, 1.000000000000000000, 1.000000000000000444, 1.000000000000000444, 1.000000000000000222, 1.000000000000000000, 1.000000000000000444, 0.9999999999999997780, 1.000000000000000444, 1.000000000000000222, 1.000000000000000000, 1.000000000000000222, 1.000000000000000000, 1.000000000000000444, 1.000000000000000000, 1.000000000000000444, 1.000000000000000222, 1.000000000000000222, 1.000000000000000222, 1.000000000000000222, 1.000000000000000222, 1.000000000000000444, 1.000000000000000222, 1.000000000000000444, 1.000000000000000222, 1.000000000000000000, 1.000000000000000888, 0.9999999999999996669, 1.000000000000000444, 1.000000000000000444, 1.000000000000000222, 1.000000000000000444, 1.000000000000000000, 1.000000000000000444, 0.9999999999999997780, 1.000000000000000444, 1.000000000000000222, 1.000000000000000444, 0.9999999999999997780, 1.000000000000000222, 1.000000000000000222, 1.000000000000000444, 1.000000000000000000, 1.000000000000000444, 1.000000000000000444, 1.000000000000000222, 1.000000000000000000, 1.000000000000000444, 1.000000000000000000, 1.000000000000000222, 1.000000000000000222, 1.000000000000000444, 1.000000000000000000, 1.000000000000000666, 1.000000000000000000, 1.000000000000000444, 1.000000000000000222, 1.000000000000000444, 1.000000000000000222, 1.000000000000000444, 1.000000000000000222, 1.000000000000000222, 1.000000000000000222, 1.000000000000000444, 1.000000000000000444, 1.000000000000000222, 1.000000000000000000, 1.000000000000000444, 1.000000000000000444, 1.000000000000000000, 1.000000000000000444, 0.9999999999999997780, 1.000000000000000444, 1.000000000000000222, 1.000000000000000222, 1.000000000000000444, 1.000000000000000222, 1.000000000000000222, 1.000000000000000444, 1.000000000000000444, 1.000000000000000444, 1.000000000000000000, 1.000000000000000444, 1.000000000000000222, 1.000000000000000222, 1.000000000000000000, 1.000000000000000444, 0.9999999999999997780, 1.000000000000000444, 1.000000000000000000, 1.000000000000000444, 1.000000000000000000, 1.000000000000000444, 1.000000000000000222, 1.000000000000000000, 1.000000000000000444, 1.000000000000000222, 1.000000000000000444, 0.9999999999999997780, 1.000000000000000444, 1.000000000000000222, 1.000000000000000222),
 ( 0.3333333333333334259, 0.3333333333333334259, 0.3333333333333334814, 0.3333333333333333703, 0.3333333333333335369, 0.3333333333333334259, 0.3333333333333334814, 0.3333333333333333703, 0.3333333333333334259, 0.3333333333333333703, 0.3333333333333335369, 0.3333333333333333703, 0.3333333333333334259, 0.3333333333333334259, 0.3333333333333333703, 0.3333333333333335369, 0.3333333333333333703, 0.3333333333333334259, 0.3333333333333335369, 0.3333333333333334259, 0.3333333333333333703, 0.3333333333333334259, 0.3333333333333334814, 0.3333333333333335369, 0.3333333333333333148, 0.3333333333333334259, 0.3333333333333334259, 0.3333333333333334814, 0.3333333333333334259, 0.3333333333333334259, 0.3333333333333334259, 0.3333333333333333148, 0.3333333333333335924, 0.3333333333333333148, 0.3333333333333335369, 0.3333333333333333703, 0.3333333333333335369, 0.3333333333333334259, 0.3333333333333333703, 0.3333333333333333703, 0.3333333333333335924, 0.3333333333333333148, 0.3333333333333334259, 0.3333333333333334259, 0.3333333333333335369, 0.3333333333333334814, 0.3333333333333334259, 0.3333333333333334259, 0.3333333333333334259, 0.3333333333333334259, 0.3333333333333333703, 0.3333333333333335369, 0.3333333333333334259, 0.3333333333333334259, 0.3333333333333334814, 0.3333333333333333703, 0.3333333333333333703, 0.3333333333333334814, 0.3333333333333334259, 0.3333333333333333703, 0.3333333333333334814, 0.3333333333333333703, 0.3333333333333334814, 0.3333333333333332593, 0.3333333333333335924, 0.3333333333333333148, 0.3333333333333335924, 0.3333333333333333148, 0.3333333333333335924, 0.3333333333333334259, 0.3333333333333334814, 0.3333333333333333703, 0.3333333333333333703, 0.3333333333333334814, 0.3333333333333335369, 0.3333333333333333703, 0.3333333333333334814, 0.3333333333333334259, 0.3333333333333333703, 0.3333333333333335369, 0.3333333333333333148, 0.3333333333333335369, 0.3333333333333334259, 0.3333333333333334259, 0.3333333333333333703, 0.3333333333333334259, 0.3333333333333333703, 0.3333333333333335369, 0.3333333333333333703, 0.3333333333333334259, 0.3333333333333334259, 0.3333333333333334814, 0.3333333333333333703, 0.3333333333333335924, 0.3333333333333333703, 0.3333333333333334259, 0.3333333333333334814, 0.3333333333333334259, 0.3333333333333335369, 0.3333333333333333148, 0.3333333333333335369, 0.3333333333333333148, 0.3333333333333334259, 0.3333333333333333703, 0.3333333333333334259, 0.3333333333333334259, 0.3333333333333335924, 0.3333333333333333703, 0.3333333333333335924, 0.3333333333333333148, 0.3333333333333335369, 0.3333333333333335369, 0.3333333333333333148, 0.3333333333333334259, 0.3333333333333334259, 0.3333333333333334814, 0.3333333333333333703, 0.3333333333333335369, 0.3333333333333333703, 0.3333333333333333703, 0.3333333333333334814, 0.3333333333333334814, 0.3333333333333334259, 0.3333333333333333703, 0.3333333333333334814, 0.3333333333333334814, 0.3333333333333334259, 0.3333333333333334259, 0.3333333333333334259, 0.3333333333333333703, 0.3333333333333335369, 0.3333333333333333703, 0.3333333333333334259, 0.3333333333333334814, 0.3333333333333334259, 0.3333333333333334814, 0.3333333333333334259, 0.3333333333333333703, 0.3333333333333333703, 0.3333333333333334259, 0.3333333333333333148, 0.3333333333333334814, 0.3333333333333334814, 0.3333333333333334259, 0.3333333333333333703, 0.3333333333333334259, 0.3333333333333334259, 0.3333333333333333703, 0.3333333333333335369, 0.3333333333333334259, 0.3333333333333333148, 0.3333333333333333703, 0.3333333333333335369, 0.3333333333333335369, 0.3333333333333333148, 0.3333333333333335369, 0.3333333333333334259, 0.3333333333333334259, 0.3333333333333335369, 0.3333333333333333703, 0.3333333333333333703, 0.3333333333333334259, 0.3333333333333333703, 0.3333333333333334259, 0.3333333333333334259, 0.3333333333333333703, 0.3333333333333335369, 0.3333333333333333703, 0.3333333333333334259, 0.3333333333333335369, 0.3333333333333333703, 0.3333333333333333703, 0.3333333333333334814, 0.3333333333333334259, 0.3333333333333333703, 0.3333333333333335369, 0.3333333333333332593, 0.3333333333333335369, 0.3333333333333335369, 0.3333333333333333703, 0.3333333333333334814, 0.3333333333333334814, 0.3333333333333334259, 0.3333333333333333703, 0.3333333333333334259, 0.3333333333333334814, 0.3333333333333333148, 0.3333333333333335369, 0.3333333333333333703, 0.3333333333333334259, 0.3333333333333333703, 0.3333333333333334259, 0.3333333333333333148, 0.3333333333333334259, 0.3333333333333334814, 0.3333333333333333703, 0.3333333333333334814, 0.3333333333333334259, 0.3333333333333333703, 0.3333333333333334259, 0.3333333333333333703, 0.3333333333333334259, 0.3333333333333334814, 0.3333333333333332593, 0.3333333333333334259, 0.3333333333333333703, 0.3333333333333335369, 0.3333333333333334259, 0.3333333333333333703, 0.3333333333333334259, 0.3333333333333334259, 0.3333333333333333148, 0.3333333333333335369, 0.3333333333333333703, 0.3333333333333334259, 0.3333333333333335924, 0.3333333333333333703, 0.3333333333333334259, 0.3333333333333335369, 0.3333333333333333703, 0.3333333333333334259, 0.3333333333333334259, 0.3333333333333334259, 0.3333333333333333703, 0.3333333333333334259, 0.3333333333333334259, 0.3333333333333333703, 0.3333333333333333148, 0.3333333333333334814, 0.3333333333333334259, 0.3333333333333334259, 0.3333333333333333703, 0.3333333333333333703, 0.3333333333333334259, 0.3333333333333335369, 0.3333333333333333703, 0.3333333333333335369, 0.3333333333333333703, 0.3333333333333334259, 0.3333333333333335369, 0.3333333333333333148, 0.3333333333333334259, 0.3333333333333334814, 0.3333333333333335369, 0.3333333333333333148, 0.3333333333333335369, 0.3333333333333333703, 0.3333333333333334259, 0.3333333333333333703, 0.3333333333333335369, 0.3333333333333334259, 0.3333333333333334259, 0.3333333333333334259, 0.3333333333333333703, 0.3333333333333335924, 0.3333333333333334259, 0.3333333333333335369, 0.3333333333333333148, 0.3333333333333333703, 0.3333333333333334814, 0.3333333333333333703, 0.3333333333333335924, 0.3333333333333333148, 0.3333333333333333703, 0.3333333333333335369, 0.3333333333333333703, 0.3333333333333335924, 0.3333333333333332593, 0.3333333333333335924, 0.3333333333333334259, 0.3333333333333335369, 0.3333333333333334259, 0.3333333333333334814, 0.3333333333333333703, 0.3333333333333334814, 0.3333333333333333148, 0.3333333333333335369, 0.3333333333333333148, 0.3333333333333334814, 0.3333333333333334814, 0.3333333333333334814, 0.3333333333333333148, 0.3333333333333335369, 0.3333333333333333148, 0.3333333333333335369, 0.3333333333333333703, 0.3333333333333333703, 0.3333333333333335369, 0.3333333333333334259, 0.3333333333333334259, 0.3333333333333333703, 0.3333333333333335369, 0.3333333333333333148, 0.3333333333333335924, 0.3333333333333334259, 0.3333333333333334259, 0.3333333333333333703, 0.3333333333333333703, 0.3333333333333334259, 0.3333333333333334259, 0.3333333333333334259, 0.3333333333333334259, 0.3333333333333334259, 0.3333333333333334259, 0.3333333333333334259, 0.3333333333333333703, 0.3333333333333335369, 0.3333333333333333703, 0.3333333333333334814, 0.3333333333333333703, 0.3333333333333333148, 0.3333333333333337034, 0.3333333333333332038, 0.3333333333333334814, 0.3333333333333335369, 0.3333333333333334814, 0.3333333333333334259, 0.3333333333333334259, 0.3333333333333334814, 0.3333333333333333703, 0.3333333333333334814, 0.3333333333333334259, 0.3333333333333334814, 0.3333333333333333148, 0.3333333333333333703, 0.3333333333333335369, 0.3333333333333334259, 0.3333333333333333703, 0.3333333333333335369, 0.3333333333333334814, 0.3333333333333334259, 0.3333333333333333703, 0.3333333333333334259, 0.3333333333333333148, 0.3333333333333335369, 0.3333333333333333148, 0.3333333333333335369, 0.3333333333333333703, 0.3333333333333335369, 0.3333333333333334259, 0.3333333333333334814, 0.3333333333333334259, 0.3333333333333335369, 0.3333333333333334259, 0.3333333333333334259, 0.3333333333333333703, 0.3333333333333334259, 0.3333333333333333703, 0.3333333333333335369, 0.3333333333333334814, 0.3333333333333333703, 0.3333333333333333148, 0.3333333333333335369, 0.3333333333333333703, 0.3333333333333333703, 0.3333333333333334814, 0.3333333333333333148, 0.3333333333333334814, 0.3333333333333333703, 0.3333333333333334259, 0.3333333333333334814, 0.3333333333333334814, 0.3333333333333334259, 0.3333333333333334259, 0.3333333333333335369, 0.3333333333333334814, 0.3333333333333333148, 0.3333333333333335369, 0.3333333333333334259, 0.3333333333333333703, 0.3333333333333334259, 0.3333333333333334259, 0.3333333333333333148, 0.3333333333333334814, 0.3333333333333333703, 0.3333333333333334259, 0.3333333333333333148, 0.3333333333333334814, 0.3333333333333334259, 0.3333333333333333148, 0.3333333333333334814, 0.3333333333333334259, 0.3333333333333334814, 0.3333333333333332593, 0.3333333333333335924, 0.3333333333333334259, 0.3333333333333334259),
 ( 0.3333333333333334259, 0.3333333333333334259, 0.3333333333333334814, 0.3333333333333333703, 0.3333333333333335369, 0.3333333333333334259, 0.3333333333333334814, 0.3333333333333333703, 0.3333333333333334259, 0.3333333333333333703, 0.3333333333333335369, 0.3333333333333333703, 0.3333333333333334259, 0.3333333333333334259, 0.3333333333333333703, 0.3333333333333335369, 0.3333333333333333703, 0.3333333333333334259, 0.3333333333333335369, 0.3333333333333334259, 0.3333333333333333703, 0.3333333333333334259, 0.3333333333333334814, 0.3333333333333335369, 0.3333333333333333148, 0.3333333333333334259, 0.3333333333333334259, 0.3333333333333334814, 0.3333333333333334259, 0.3333333333333334259, 0.3333333333333334259, 0.3333333333333333148, 0.3333333333333335924, 0.3333333333333333148, 0.3333333333333335369, 0.3333333333333333703, 0.3333333333333335369, 0.3333333333333334259, 0.3333333333333333703, 0.3333333333333333703, 0.3333333333333335924, 0.3333333333333333148, 0.3333333333333334259, 0.3333333333333334259, 0.3333333333333335369, 0.3333333333333334814, 0.3333333333333334259, 0.3333333333333334259, 0.3333333333333334259, 0.3333333333333334259, 0.3333333333333333703, 0.3333333333333335369, 0.3333333333333334259, 0.3333333333333334259, 0.3333333333333334814, 0.3333333333333333703, 0.3333333333333333703, 0.3333333333333334814, 0.3333333333333334259, 0.3333333333333333703, 0.3333333333333334814, 0.3333333333333333703, 0.3333333333333334814, 0.3333333333333332593, 0.3333333333333335924, 0.3333333333333333148, 0.3333333333333335924, 0.3333333333333333148, 0.3333333333333335924, 0.3333333333333334259, 0.3333333333333334814, 0.3333333333333333703, 0.3333333333333333703, 0.3333333333333334814, 0.3333333333333335369, 0.3333333333333333703, 0.3333333333333334814, 0.3333333333333334259, 0.3333333333333333703, 0.3333333333333335369, 0.3333333333333333148, 0.3333333333333335369, 0.3333333333333334259, 0.3333333333333334259, 0.3333333333333333703, 0.3333333333333334259, 0.3333333333333333703, 0.3333333333333335369, 0.3333333333333333703, 0.3333333333333334259, 0.3333333333333334259, 0.3333333333333334814, 0.3333333333333333703, 0.3333333333333335924, 0.3333333333333333703, 0.3333333333333334259, 0.3333333333333334814, 0.3333333333333334259, 0.3333333333333335369, 0.3333333333333333148, 0.3333333333333335369, 0.3333333333333333148, 0.3333333333333334259, 0.3333333333333333703, 0.3333333333333334259, 0.3333333333333334259, 0.3333333333333335924, 0.3333333333333333703, 0.3333333333333335924, 0.3333333333333333148, 0.3333333333333335369, 0.3333333333333335369, 0.3333333333333333148, 0.3333333333333334259, 0.3333333333333334259, 0.3333333333333334814, 0.3333333333333333703, 0.3333333333333335369, 0.3333333333333333703, 0.3333333333333333703, 0.3333333333333334814, 0.3333333333333334814, 0.3333333333333334259, 0.3333333333333333703, 0.3333333333333334814, 0.3333333333333334814, 0.3333333333333334259, 0.3333333333333334259, 0.3333333333333334259, 0.3333333333333333703, 0.3333333333333335369, 0.3333333333333333703, 0.3333333333333334259, 0.3333333333333334814, 0.3333333333333334259, 0.3333333333333334814, 0.3333333333333334259, 0.3333333333333333703, 0.3333333333333333703, 0.3333333333333334259, 0.3333333333333333148, 0.3333333333333334814, 0.3333333333333334814, 0.3333333333333334259, 0.3333333333333333703, 0.3333333333333334259, 0.3333333333333334259, 0.3333333333333333703, 0.3333333333333335369, 0.3333333333333334259, 0.3333333333333333148, 0.3333333333333333703, 0.3333333333333335369, 0.3333333333333335369, 0.3333333333333333148, 0.3333333333333335369, 0.3333333333333334259, 0.3333333333333334259, 0.3333333333333335369, 0.3333333333333333703, 0.3333333333333333703, 0.3333333333333334259, 0.3333333333333333703, 0.3333333333333334259, 0.3333333333333334259, 0.3333333333333333703, 0.3333333333333335369, 0.3333333333333333703, 0.3333333333333334259, 0.3333333333333335369, 0.3333333333333333703, 0.3333333333333333703, 0.3333333333333334814, 0.3333333333333334259, 0.3333333333333333703, 0.3333333333333335369, 0.3333333333333332593, 0.3333333333333335369, 0.3333333333333335369, 0.3333333333333333703, 0.3333333333333334814, 0.3333333333333334814, 0.3333333333333334259, 0.3333333333333333703, 0.3333333333333334259, 0.3333333333333334814, 0.3333333333333333148, 0.3333333333333335369, 0.3333333333333333703, 0.3333333333333334259, 0.3333333333333333703, 0.3333333333333334259, 0.3333333333333333148, 0.3333333333333334259, 0.3333333333333334814, 0.3333333333333333703, 0.3333333333333334814, 0.3333333333333334259, 0.3333333333333333703, 0.3333333333333334259, 0.3333333333333333703, 0.3333333333333334259, 0.3333333333333334814, 0.3333333333333332593, 0.3333333333333334259, 0.3333333333333333703, 0.3333333333333335369, 0.3333333333333334259, 0.3333333333333333703, 0.3333333333333334259, 0.3333333333333334259, 0.3333333333333333148, 0.3333333333333335369, 0.3333333333333333703, 0.3333333333333334259, 0.3333333333333335924, 0.3333333333333333703, 0.3333333333333334259, 0.3333333333333335369, 0.3333333333333333703, 0.3333333333333334259, 0.3333333333333334259, 0.3333333333333334259, 0.3333333333333333703, 0.3333333333333334259, 0.3333333333333334259, 0.3333333333333333703, 0.3333333333333333148, 0.3333333333333334814, 0.3333333333333334259, 0.3333333333333334259, 0.3333333333333333703, 0.3333333333333333703, 0.3333333333333334259, 0.3333333333333335369, 0.3333333333333333703, 0.3333333333333335369, 0.3333333333333333703, 0.3333333333333334259, 0.3333333333333335369, 0.3333333333333333148, 0.3333333333333334259, 0.3333333333333334814, 0.3333333333333335369, 0.3333333333333333148, 0.3333333333333335369, 0.3333333333333333703, 0.3333333333333334259, 0.3333333333333333703, 0.3333333333333335369, 0.3333333333333334259, 0.3333333333333334259, 0.3333333333333334259, 0.3333333333333333703, 0.3333333333333335924, 0.3333333333333334259, 0.3333333333333335369, 0.3333333333333333148, 0.3333333333333333703, 0.3333333333333334814, 0.3333333333333333703, 0.3333333333333335924, 0.3333333333333333148, 0.3333333333333333703, 0.3333333333333335369, 0.3333333333333333703, 0.3333333333333335924, 0.3333333333333332593, 0.3333333333333335924, 0.3333333333333334259, 0.3333333333333335369, 0.3333333333333334259, 0.3333333333333334814, 0.3333333333333333703, 0.3333333333333334814, 0.3333333333333333148, 0.3333333333333335369, 0.3333333333333333148, 0.3333333333333334814, 0.3333333333333334814, 0.3333333333333334814, 0.3333333333333333148, 0.3333333333333335369, 0.3333333333333333148, 0.3333333333333335369, 0.3333333333333333703, 0.3333333333333333703, 0.3333333333333335369, 0.3333333333333334259, 0.3333333333333334259, 0.3333333333333333703, 0.3333333333333335369, 0.3333333333333333148, 0.3333333333333335924, 0.3333333333333334259, 0.3333333333333334259, 0.3333333333333333703, 0.3333333333333333703, 0.3333333333333334259, 0.3333333333333334259, 0.3333333333333334259, 0.3333333333333334259, 0.3333333333333334259, 0.3333333333333334259, 0.3333333333333334259, 0.3333333333333333703, 0.3333333333333335369, 0.3333333333333333703, 0.3333333333333334814, 0.3333333333333333703, 0.3333333333333333148, 0.3333333333333337034, 0.3333333333333332038, 0.3333333333333334814, 0.3333333333333335369, 0.3333333333333334814, 0.3333333333333334259, 0.3333333333333334259, 0.3333333333333334814, 0.3333333333333333703, 0.3333333333333334814, 0.3333333333333334259, 0.3333333333333334814, 0.3333333333333333148, 0.3333333333333333703, 0.3333333333333335369, 0.3333333333333334259, 0.3333333333333333703, 0.3333333333333335369, 0.3333333333333334814, 0.3333333333333334259, 0.3333333333333333703, 0.3333333333333334259, 0.3333333333333333148, 0.3333333333333335369, 0.3333333333333333148, 0.3333333333333335369, 0.3333333333333333703, 0.3333333333333335369, 0.3333333333333334259, 0.3333333333333334814, 0.3333333333333334259, 0.3333333333333335369, 0.3333333333333334259, 0.3333333333333334259, 0.3333333333333333703, 0.3333333333333334259, 0.3333333333333333703, 0.3333333333333335369, 0.3333333333333334814, 0.3333333333333333703, 0.3333333333333333148, 0.3333333333333335369, 0.3333333333333333703, 0.3333333333333333703, 0.3333333333333334814, 0.3333333333333333148, 0.3333333333333334814, 0.3333333333333333703, 0.3333333333333334259, 0.3333333333333334814, 0.3333333333333334814, 0.3333333333333334259, 0.3333333333333334259, 0.3333333333333335369, 0.3333333333333334814, 0.3333333333333333148, 0.3333333333333335369, 0.3333333333333334259, 0.3333333333333333703, 0.3333333333333334259, 0.3333333333333334259, 0.3333333333333333148, 0.3333333333333334814, 0.3333333333333333703, 0.3333333333333334259, 0.3333333333333333148, 0.3333333333333334814, 0.3333333333333334259, 0.3333333333333333148, 0.3333333333333334814, 0.3333333333333334259, 0.3333333333333334814, 0.3333333333333332593, 0.3333333333333335924, 0.3333333333333334259, 0.3333333333333334259),
 ( 1.000000000000000222, 1.000000000000000222, 1.000000000000000444, 1.000000000000000000, 1.000000000000000444, 1.000000000000000222, 1.000000000000000444, 0.9999999999999997780, 1.000000000000000444, 1.000000000000000000, 1.000000000000000444, 1.000000000000000000, 1.000000000000000444, 1.000000000000000222, 1.000000000000000000, 1.000000000000000666, 0.9999999999999997780, 1.000000000000000444, 1.000000000000000444, 1.000000000000000444, 1.000000000000000222, 1.000000000000000222, 1.000000000000000444, 1.000000000000000444, 1.000000000000000000, 1.000000000000000222, 1.000000000000000222, 1.000000000000000444, 1.000000000000000222, 1.000000000000000444, 1.000000000000000000, 1.000000000000000222, 1.000000000000000444, 1.000000000000000000, 1.000000000000000444, 1.000000000000000222, 1.000000000000000444, 1.000000000000000444, 1.000000000000000222, 1.000000000000000000, 1.000000000000000444, 1.000000000000000222, 1.000000000000000000, 1.000000000000000222, 1.000000000000000444, 1.000000000000000444, 1.000000000000000444, 1.000000000000000444, 1.000000000000000222, 1.000000000000000444, 1.000000000000000000, 1.000000000000000444, 1.000000000000000222, 1.000000000000000222, 1.000000000000000444, 1.000000000000000000, 1.000000000000000222, 1.000000000000000444, 1.000000000000000222, 1.000000000000000000, 1.000000000000000444, 1.000000000000000222, 1.000000000000000222, 1.000000000000000000, 1.000000000000000444, 0.9999999999999997780, 1.000000000000000444, 1.000000000000000000, 1.000000000000000444, 1.000000000000000000, 1.000000000000000444, 0.9999999999999997780, 1.000000000000000222, 1.000000000000000444, 1.000000000000000444, 1.000000000000000000, 1.000000000000000444, 1.000000000000000222, 1.000000000000000000, 1.000000000000000666, 1.000000000000000000, 1.000000000000000444, 1.000000000000000222, 1.000000000000000444, 0.9999999999999997780, 1.000000000000000444, 1.000000000000000000, 1.000000000000000444, 1.000000000000000444, 1.000000000000000222, 1.000000000000000222, 1.000000000000000444, 1.000000000000000222, 1.000000000000000444, 1.000000000000000444, 1.000000000000000222, 1.000000000000000444, 1.000000000000000222, 1.000000000000000444, 1.000000000000000000, 1.000000000000000444, 1.000000000000000000, 1.000000000000000000, 1.000000000000000444, 1.000000000000000222, 1.000000000000000222, 1.000000000000000444, 1.000000000000000000, 1.000000000000000444, 1.000000000000000000, 1.000000000000000222, 1.000000000000000444, 0.9999999999999997780, 1.000000000000000444, 1.000000000000000222, 1.000000000000000444, 1.000000000000000000, 1.000000000000000444, 1.000000000000000000, 1.000000000000000222, 1.000000000000000222, 1.000000000000000444, 1.000000000000000222, 1.000000000000000000, 1.000000000000000444, 1.000000000000000222, 1.000000000000000222, 1.000000000000000222, 1.000000000000000444, 0.9999999999999997780, 1.000000000000000666, 0.9999999999999996669, 1.000000000000000444, 1.000000000000000444, 1.000000000000000222, 1.000000000000000444, 1.000000000000000444, 1.000000000000000222, 1.000000000000000000, 1.000000000000000444, 1.000000000000000000, 1.000000000000000444, 1.000000000000000222, 1.000000000000000444, 1.000000000000000000, 1.000000000000000444, 1.000000000000000222, 1.000000000000000222, 1.000000000000000444, 1.000000000000000222, 0.9999999999999997780, 1.000000000000000444, 1.000000000000000444, 1.000000000000000444, 1.000000000000000222, 1.000000000000000444, 1.000000000000000444, 1.000000000000000222, 1.000000000000000444, 1.000000000000000000, 1.000000000000000222, 1.000000000000000444, 1.000000000000000000, 1.000000000000000222, 1.000000000000000444, 1.000000000000000000, 1.000000000000000444, 0.9999999999999997780, 1.000000000000000222, 1.000000000000000444, 1.000000000000000000, 1.000000000000000222, 1.000000000000000222, 1.000000000000000444, 1.000000000000000000, 1.000000000000000666, 0.9999999999999996669, 1.000000000000000666, 1.000000000000000222, 1.000000000000000444, 1.000000000000000222, 1.000000000000000444, 1.000000000000000222, 1.000000000000000222, 1.000000000000000000, 1.000000000000000444, 0.9999999999999997780, 1.000000000000000444, 1.000000000000000222, 1.000000000000000444, 0.9999999999999997780, 1.000000000000000444, 1.000000000000000000, 1.000000000000000222, 1.000000000000000444, 1.000000000000000000, 1.000000000000000444, 1.000000000000000444, 1.000000000000000222, 1.000000000000000222, 1.000000000000000000, 1.000000000000000444, 1.000000000000000444, 1.000000000000000000, 1.000000000000000222, 1.000000000000000222, 1.000000000000000444, 1.000000000000000222, 1.000000000000000222, 1.000000000000000444, 1.000000000000000222, 1.000000000000000000, 1.000000000000000444, 1.000000000000000000, 1.000000000000000222, 1.000000000000000444, 1.000000000000000222, 1.000000000000000222, 1.000000000000000444, 1.000000000000000000, 1.000000000000000222, 1.000000000000000222, 1.000000000000000222, 1.000000000000000000, 1.000000000000000222, 1.000000000000000222, 1.000000000000000000, 1.000000000000000222, 1.000000000000000222, 1.000000000000000444, 1.000000000000000000, 1.000000000000000000, 1.000000000000000222, 1.000000000000000000, 1.000000000000000888, 1.000000000000000000, 1.000000000000000444, 1.000000000000000222, 1.000000000000000222, 1.000000000000000444, 1.000000000000000222, 1.000000000000000222, 1.000000000000000444, 1.000000000000000444, 1.000000000000000222, 1.000000000000000444, 1.000000000000000222, 1.000000000000000000, 1.000000000000000222, 1.000000000000000444, 1.000000000000000444, 1.000000000000000222, 1.000000000000000444, 1.000000000000000222, 1.000000000000000444, 1.000000000000000222, 1.000000000000000444, 1.000000000000000222, 1.000000000000000000, 1.000000000000000444, 1.000000000000000000, 1.000000000000000666, 1.000000000000000000, 1.000000000000000000, 1.000000000000000444, 1.000000000000000222, 1.000000000000000444, 0.9999999999999997780, 1.000000000000000666, 1.000000000000000222, 1.000000000000000444, 1.000000000000000222, 1.000000000000000444, 1.000000000000000222, 1.000000000000000444, 0.9999999999999997780, 1.000000000000000666, 1.000000000000000222, 1.000000000000000222, 1.000000000000000444, 1.000000000000000444, 0.9999999999999997780, 1.000000000000000444, 1.000000000000000222, 1.000000000000000222, 1.000000000000000000, 1.000000000000000000, 1.000000000000000444, 1.000000000000000444, 1.000000000000000222, 1.000000000000000000, 1.000000000000000444, 0.9999999999999997780, 1.000000000000000444, 1.000000000000000222, 1.000000000000000000, 1.000000000000000222, 1.000000000000000000, 1.000000000000000444, 1.000000000000000000, 1.000000000000000444, 1.000000000000000222, 1.000000000000000222, 1.000000000000000222, 1.000000000000000222, 1.000000000000000222, 1.000000000000000444, 1.000000000000000222, 1.000000000000000444, 1.000000000000000222, 1.000000000000000000, 1.000000000000000888, 0.9999999999999996669, 1.000000000000000444, 1.000000000000000444, 1.000000000000000222, 1.000000000000000444, 1.000000000000000000, 1.000000000000000444, 0.9999999999999997780, 1.000000000000000444, 1.000000000000000222, 1.000000000000000444, 0.9999999999999997780, 1.000000000000000222, 1.000000000000000222, 1.000000000000000444, 1.000000000000000000, 1.000000000000000444, 1.000000000000000444, 1.000000000000000222, 1.000000000000000000, 1.000000000000000444, 1.000000000000000000, 1.000000000000000222, 1.000000000000000222, 1.000000000000000444, 1.000000000000000000, 1.000000000000000666, 1.000000000000000000, 1.000000000000000444, 1.000000000000000222, 1.000000000000000444, 1.000000000000000222, 1.000000000000000444, 1.000000000000000222, 1.000000000000000222, 1.000000000000000222, 1.000000000000000444, 1.000000000000000444, 1.000000000000000222, 1.000000000000000000, 1.000000000000000444, 1.000000000000000444, 1.000000000000000000, 1.000000000000000444, 0.9999999999999997780, 1.000000000000000444, 1.000000000000000222, 1.000000000000000222, 1.000000000000000444, 1.000000000000000222, 1.000000000000000222, 1.000000000000000444, 1.000000000000000444, 1.000000000000000444, 1.000000000000000000, 1.000000000000000444, 1.000000000000000222, 1.000000000000000222, 1.000000000000000000, 1.000000000000000444, 0.9999999999999997780, 1.000000000000000444, 1.000000000000000000, 1.000000000000000444, 1.000000000000000000, 1.000000000000000444, 1.000000000000000222, 1.000000000000000000, 1.000000000000000444, 1.000000000000000222, 1.000000000000000444, 0.9999999999999997780, 1.000000000000000444, 1.000000000000000222, 1.000000000000000222) ) ) 
 REPRESENTATION_ITEM ( '' )  SURFACE ( )  );
#63181 = CARTESIAN_POINT ( 'NONE',  ( -6.486551268120854807, 6.767445667853342783, -0.2095380678983837508 ) ) ;
#63182 = CARTESIAN_POINT ( 'NONE',  ( -3.285556943750000514, -2.938541666188710266, -1.896917185911906722 ) ) ;
#63183 = CARTESIAN_POINT ( 'NONE',  ( 6.154511665599609493, 9.267681812253174556, 1.199719254218462483 ) ) ;
#63184 = CARTESIAN_POINT ( 'NONE',  ( -10.57214848667379314, 5.653292861472692721, 5.679042682613224535 ) ) ;
#63185 = CARTESIAN_POINT ( 'NONE',  ( 1.364683531250000303, 9.817708333674735499, -0.7879004041258355073 ) ) ;
#63186 = CARTESIAN_POINT ( 'NONE',  ( -4.761938266897808525, 6.578680616179308771, 1.599625672291267398 ) ) ;
#63188 = CARTESIAN_POINT ( 'NONE',  ( -3.133342898089680695, 6.669667457830990465, 0.7216878364870338292 ) ) ;
#63187 =( LENGTH_UNIT ( ) NAMED_UNIT ( * ) SI_UNIT ( .MILLI., .METRE. ) );
#63189 = CIRCLE ( 'NONE', #18167, 0.4800000000000000933 ) ;
#63190 = CARTESIAN_POINT ( 'NONE',  ( -5.392392409933270514, 7.314210449720692786, 1.599625672291269396 ) ) ;
#63191 = AXIS2_PLACEMENT_3D ( 'NONE', #87300, #54802, #2814 ) ;
#63192 = CARTESIAN_POINT ( 'NONE',  ( 1.112269271232646739, 2.068042923180101411, -0.09779880236997220977 ) ) ;
#63193 = CARTESIAN_POINT ( 'NONE',  ( 2.460703409257146923, -2.027034307268358315, -0.6114533316685047959 ) ) ;
#63194 = CARTESIAN_POINT ( 'NONE',  ( 7.079328764629950754, 11.41096732537697633, 0.7998128361456462443 ) ) ;
#63195 = CARTESIAN_POINT ( 'NONE',  ( 0.7499999999999902300, 3.514583334016149863, 1.299038105676669330 ) ) ;
#63196 = CARTESIAN_POINT ( 'NONE',  ( 1.006626315519317139, 0.5665869296403948097, 1.886213005043664515 ) ) ;
#63197 = CARTESIAN_POINT ( 'NONE',  ( 4.945911955618520928, 6.845357471522081738, 1.424928946000488583 ) ) ;
#63198 = CARTESIAN_POINT ( 'NONE',  ( 5.341549334104200852, 5.334155099317434257, 0.7216878364870317197 ) ) ;
#63200 = CARTESIAN_POINT ( 'NONE',  ( 0.1831564129048668388, 7.629137130509052511, -2.545826866328745997 ) ) ;
#63199 = CARTESIAN_POINT ( 'NONE',  ( -1.737500000000000266, -3.208333333333333925, -3.009438278150923907 ) ) ;
#63201 = CARTESIAN_POINT ( 'NONE',  ( 2.730776445121200435, 0.2818232878892740212, 2.274813446668845884 ) ) ;
#63202 = CARTESIAN_POINT ( 'NONE',  ( 0.2229205655521030172, -0.09321834626660817358, 1.823428419517532983 ) ) ;
#63203 = CARTESIAN_POINT ( 'NONE',  ( 2.021601768330282045, -0.4154675118966509317, 1.866563793090275203 ) ) ;
#63204 = CARTESIAN_POINT ( 'NONE',  ( 7.354371980770088690, 7.544798497178720531, 0.000000000000000000 ) ) ;
#63205 = CARTESIAN_POINT ( 'NONE',  ( 6.846504384776753049, 9.010674420371453053, -1.443375672974058777 ) ) ;
#63206 = CARTESIAN_POINT ( 'NONE',  ( 1.705339411233731672, 1.749488060808137790, -0.9960635233151514667 ) ) ;
#63207 = CARTESIAN_POINT ( 'NONE',  ( 2.237090426018002454, -0.09115598566783281176, -1.959741687340323946 ) ) ;
#63208 = CARTESIAN_POINT ( 'NONE',  ( -7.784352752540590004, 12.23349531127272094, 0.7998128361456481317 ) ) ;
#63209 = CARTESIAN_POINT ( 'NONE',  ( -6.418895661066105873, 9.576129806964074120, -1.199719254218440723 ) ) ;
#63210 = CARTESIAN_POINT ( 'NONE',  ( -5.734735788456140959, 5.792872629394733686, 0.7216878364870513707 ) ) ;
#63212 = CARTESIAN_POINT ( 'NONE',  ( 3.291635156611854462, -0.7182737719314927771, 1.617730789815795545 ) ) ;
#63211 = CARTESIAN_POINT ( 'NONE',  ( 4.593745122936496728, -2.090168268563397547, -0.05157397306862486486 ) ) ;
#63213 = CARTESIAN_POINT ( 'NONE',  ( -3.796053574492347593, 14.00000000000182254, 12.24940615670329080 ) ) ;
#63215 = CARTESIAN_POINT ( 'NONE',  ( 6.246038198481189241, 0.7129642902690846995, 2.178627299872720524 ) ) ;
#63214 = CARTESIAN_POINT ( 'NONE',  ( 0.4153311931458959494, 3.850000000000006306, 0.5000000000000064393 ) ) ;
#63216 = CARTESIAN_POINT ( 'NONE',  ( 4.646296158022299672, -1.395249218123927104, 1.039982334504330197 ) ) ;
#63218 = EDGE_CURVE ( 'NONE', #2895, #54417, #101431, .T. ) ;
#63217 = CIRCLE ( 'NONE', #191224, 12.00000000000000178 ) ;
#63219 = CARTESIAN_POINT ( 'NONE',  ( 9.915090410295563927, 10.46202698829998567, -0.7998128361456281477 ) ) ;
#63220 = CARTESIAN_POINT ( 'NONE',  ( -0.7499999999999972244, 4.108333333333360038, -1.299038105676652011 ) ) ;
#63221 = CARTESIAN_POINT ( 'NONE',  ( 3.971823236585111161, 1.486633142371917238, 0.8919779901093974894 ) ) ;
#63222 = CARTESIAN_POINT ( 'NONE',  ( 4.773980394326226673, -2.130202496963151670, 0.4190362392007019876 ) ) ;
#63223 = CARTESIAN_POINT ( 'NONE',  ( 5.007038802148489509, 4.735966778795008381, 0.7998128361456341429 ) ) ;
#63224 = CARTESIAN_POINT ( 'NONE',  ( 5.858611323429600226, -1.916351766245901977, -0.6279953093112633500 ) ) ;
#63225 = CARTESIAN_POINT ( 'NONE',  ( 5.093750000000003553, -1.895863743164187376, -0.7852924748297283042 ) ) ;
#63226 = CARTESIAN_POINT ( 'NONE',  ( -1.499999999999997780, 5.681250000682820378, 1.214306433183764966E-14 ) ) ;
#63227 = CARTESIAN_POINT ( 'NONE',  ( 3.715773558573881363, -1.898061356504710639, 0.3282749975898023309 ) ) ;
#63228 = CARTESIAN_POINT ( 'NONE',  ( 1.499999999999997113, 9.677083334016129967, -0.8660254037844378194 ) ) ;
#63229 = CARTESIAN_POINT ( 'NONE',  ( 0.3994919479695389075, -0.2781545790336605317, -2.203771652037065376 ) ) ;
#63230 = VERTEX_POINT ( 'NONE', #71038 ) ;
#63231 = CARTESIAN_POINT ( 'NONE',  ( 6.983263157960365675, 7.629137130509070275, 2.446189081643288521 ) ) ;
#63232 = CARTESIAN_POINT ( 'NONE',  ( -0.7499999999999972244, 3.358333333333359150, -1.299038105676652011 ) ) ;
#63233 = CARTESIAN_POINT ( 'NONE',  ( 4.449046963578762615, 8.342305224150557308, -0.7998128361456231517 ) ) ;
#63234 = EDGE_CURVE ( 'NONE', #60595, #119323, #11161, .T. ) ;
#63235 = CARTESIAN_POINT ( 'NONE',  ( 10.39649820107524825, 2.629643693813620509, -5.992760101887531832 ) ) ;
#63236 = CARTESIAN_POINT ( 'NONE',  ( 8.622622508611357262, 9.162073802909148412, -0.7216878364870197293 ) ) ;
#63237 = EDGE_CURVE ( 'NONE', #159976, #116082, #203475, .T. ) ;
#63238 = CARTESIAN_POINT ( 'NONE',  ( -8.907343734053998929, 12.37535620882957588, 1.082531754730558626 ) ) ;
#63239 = CARTESIAN_POINT ( 'NONE',  ( 3.878514461961128479, 6.682628084666728085, -1.199719254218448494 ) ) ;
#63240 = CARTESIAN_POINT ( 'NONE',  ( 0.05336153386781630759, -1.314994204386025434, 1.528742563917218078 ) ) ;
#63242 = CARTESIAN_POINT ( 'NONE',  ( 6.021949879679938000, 2.032782779420911456, -0.3490252056354887222 ) ) ;
#63241 = CARTESIAN_POINT ( 'NONE',  ( 9.890836756369282057, 11.49806328964105617, -1.199719254218440723 ) ) ;
#63243 = CARTESIAN_POINT ( 'NONE',  ( 0.000000000000000000, -8.233137084989849086, 0.000000000000000000 ) ) ;
#63244 = CARTESIAN_POINT ( 'NONE',  ( -3.578462479003122976, 6.262291094557191684, 1.199719254218464037 ) ) ;
#63245 = CARTESIAN_POINT ( 'NONE',  ( 1.499999999999990896, 5.556250000682820378, 1.214306433183764966E-14 ) ) ;
#63246 = CARTESIAN_POINT ( 'NONE',  ( -1.364683531250014514, 0.9885416670080898749, -0.7879004041258289570 ) ) ;
#63247 = CARTESIAN_POINT ( 'NONE',  ( 0.7195362622018970367, -0.9397137143956849625, -1.499438161327722341 ) ) ;
#63248 = CARTESIAN_POINT ( 'NONE',  ( 5.766190679352209969, 1.598854145598350929, -0.6720813200297001133 ) ) ;
#63249 = CARTESIAN_POINT ( 'NONE',  ( 5.091228679354776965, -0.6197342532976670704, 1.626566373401008070 ) ) ;
#63250 = CARTESIAN_POINT ( 'NONE',  ( 4.847203612085560387, 5.613824621309978724, -1.199719254218452047 ) ) ;
#63251 = CARTESIAN_POINT ( 'NONE',  ( 3.228363206396630769, 2.236961789864226002, 0.5003539455325100027 ) ) ;
#63252 = CARTESIAN_POINT ( 'NONE',  ( 1.364683531249990311, 5.426041667008086655, 0.7879004041258500513 ) ) ;
#63253 = CARTESIAN_POINT ( 'NONE',  ( 1.042614295247261680, -1.450156864641814369, -1.134287774663629733 ) ) ;
#63254 = DIRECTION ( 'NONE',  ( 0.000000000000000000, 1.000000000000000000, 0.000000000000000000 ) ) ;
#63255 = DIRECTION ( 'NONE',  ( 0.000000000000000000, -1.445602896647338917E-16, 1.000000000000000000 ) ) ;
#63256 = CARTESIAN_POINT ( 'NONE',  ( 2.186296784933777992, -1.789763940591000191, -0.3589617604915079085 ) ) ;
#63257 = CARTESIAN_POINT ( 'NONE',  ( 2.619767714365705658, 0.2496074646863334634, 2.000857082853441327 ) ) ;
#63258 = CARTESIAN_POINT ( 'NONE',  ( 1.517799938645987057, -1.219565478727736574, -1.820545776841306029 ) ) ;
#63259 = CARTESIAN_POINT ( 'NONE',  ( 8.597817685116813990, 14.01748360710000085, -7.912049044921352525 ) ) ;
#63260 = CARTESIAN_POINT ( 'NONE',  ( 4.682709062318923365, -2.042047207266047604, -0.5143438382350475901 ) ) ;
#63261 = CARTESIAN_POINT ( 'NONE',  ( -6.744291347794091784, 9.955758108146730123, -1.199719254218440723 ) ) ;
#63262 = CARTESIAN_POINT ( 'NONE',  ( 8.771848968578403571, 13.55328059063308999, 7.722295445558531313 ) ) ;
#63263 = CARTESIAN_POINT ( 'NONE',  ( 1.275928261265106833, -2.020323679977220621, 0.4517519998969782291 ) ) ;
#63264 = CARTESIAN_POINT ( 'NONE',  ( 3.669453130792974971, 7.432779085900453886, 1.040834085586084257E-14 ) ) ;
#63265 = CARTESIAN_POINT ( 'NONE',  ( -0.6801582343750229853, -0.3697916663252601155, -1.178068619123890270 ) ) ;
#63266 = CARTESIAN_POINT ( 'NONE',  ( 3.440189854244297241, -1.264556376030629981, -1.702001827410426049 ) ) ;
#63267 = CONTEXT_DEPENDENT_SHAPE_REPRESENTATION ( #154427, #97400 ) ;
#63268 = CARTESIAN_POINT ( 'NONE',  ( 6.721331454403435934, -0.1262074967819451221, 1.796610827203233063 ) ) ;
#63269 = ORIENTED_EDGE ( 'NONE', *, *, #163343, .F. ) ;
#63270 = CARTESIAN_POINT ( 'NONE',  ( -6.143779885648060102, 7.196773283791382703, 1.199719254218452047 ) ) ;
#63271 = CARTESIAN_POINT ( 'NONE',  ( 10.40996301719436090, 11.03937836301526687, 0.000000000000000000 ) ) ;
#63272 = CARTESIAN_POINT ( 'NONE',  ( 7.173672674962134899, 7.541908673643526129, -0.7216878364870317197 ) ) ;
#63273 = CARTESIAN_POINT ( 'NONE',  ( 0.000000000000000000, -2.493749999044085897, -4.012584370867899430 ) ) ;
#63274 = CARTESIAN_POINT ( 'NONE',  ( -3.879604511804807032, 7.677955697080923514, 0.7998128361456341429 ) ) ;
#63275 = CARTESIAN_POINT ( 'NONE',  ( 6.451439665316073935, -1.893653415279672902, 0.9546920624979161607 ) ) ;
#63276 = CARTESIAN_POINT ( 'NONE',  ( 1.167171324275569466, -1.903845421566036311, -0.9005605707013781824 ) ) ;
#63277 = CARTESIAN_POINT ( 'NONE',  ( -4.359828915246279024, 7.244161613499399799, -1.199719254218455378 ) ) ;
#63278 = CARTESIAN_POINT ( 'NONE',  ( 7.214910300766615769, 11.56914578420308715, -0.7998128361456291469 ) ) ;
#63279 = CARTESIAN_POINT ( 'NONE',  ( 5.313276548598107496, -1.570925495967404828, -0.9973500568975323111 ) ) ;
#63280 = CARTESIAN_POINT ( 'NONE',  ( 7.564559641420864899, 10.91273778404466199, -1.199719254218446718 ) ) ;
#63281 = CARTESIAN_POINT ( 'NONE',  ( -0.6386894617478927616, 4.335523901721595408, -0.1366332986426508633 ) ) ;
#63282 = ORIENTED_EDGE ( 'NONE', *, *, #158238, .F. ) ;
#63283 = CARTESIAN_POINT ( 'NONE',  ( -4.472210567661380587, 6.310941310395290493, 1.599625672291270506 ) ) ;
#63284 = CARTESIAN_POINT ( 'NONE',  ( -9.002250809794000830, 11.52571191622492464, -1.443375672974059665 ) ) ;
#63285 = AXIS2_PLACEMENT_3D ( 'NONE', #52562, #153261, #186820 ) ;
#63287 = CARTESIAN_POINT ( 'NONE',  ( 2.049198471137442912, 1.708465938063120637, -0.9642302061752603404 ) ) ;
#63286 = CARTESIAN_POINT ( 'NONE',  ( -7.152089726408780379, 8.302858421353754181, -1.199719254218446718 ) ) ;
#63288 = CARTESIAN_POINT ( 'NONE',  ( 0.6554165194554737450, -1.826866057147133349, -1.155366728873077342 ) ) ;
#63289 = AXIS2_PLACEMENT_3D ( 'NONE', #39388, #89225, #188837 ) ;
#63291 = CARTESIAN_POINT ( 'NONE',  ( -5.988731108142371085, 6.089685199429741402, 0.6933981374793452002 ) ) ;
#63290 = CARTESIAN_POINT ( 'NONE',  ( -4.125423880308188629, 8.035021303660014880, -0.7998128361456481317 ) ) ;
#63292 = CARTESIAN_POINT ( 'NONE',  ( -0.6823417656250212460, 0.8010416670080899859, 1.181850606188755259 ) ) ;
#63293 = CARTESIAN_POINT ( 'NONE',  ( 3.268574299048069953, -1.732005324549376279, 0.08218708453346619536 ) ) ;
#63294 = CARTESIAN_POINT ( 'NONE',  ( 2.009305037403839922, -0.8189296680943327633, -1.535607775426613086 ) ) ;
#63295 = CARTESIAN_POINT ( 'NONE',  ( 7.293923454472080792, 9.532663335016016148, 1.443375672974076540 ) ) ;
#63296 = CARTESIAN_POINT ( 'NONE',  ( -11.19349454483825212, 5.612381422204108183, 3.868266946477203927 ) ) ;
#63297 = CARTESIAN_POINT ( 'NONE',  ( 3.040362567271452487, 2.044824973086068809, 0.2555446107466197714 ) ) ;
#63298 = CARTESIAN_POINT ( 'NONE',  ( 0.6673420201736457447, -0.6766069248959759586, -1.899328980164962877 ) ) ;
#63299 = CARTESIAN_POINT ( 'NONE',  ( 6.825078400183579141, 1.241995729952071637, 2.258014901253778461 ) ) ;
#63300 = CARTESIAN_POINT ( 'NONE',  ( -4.339491684825780737, 7.220434844675483355, -1.199719254218455378 ) ) ;
#63301 = CARTESIAN_POINT ( 'NONE',  ( 0.9714808946714141857, 1.900638238906343425, -0.5234924991099793035 ) ) ;
#63303 = CARTESIAN_POINT ( 'NONE',  ( -5.126391479742927970, 8.994890803093138487, 0.7216878364870267237 ) ) ;
#63302 = CARTESIAN_POINT ( 'NONE',  ( 5.642805672956042962, 1.844803604357934779, 0.5037821151940986564 ) ) ;
#63304 = CARTESIAN_POINT ( 'NONE',  ( -5.872089928050201024, 8.904503111816948646, 1.082531754730550855 ) ) ;
#63305 = CARTESIAN_POINT ( 'NONE',  ( 6.230854113932139171, 9.427024345299638952, 1.199719254218452047 ) ) ;
#63306 = CARTESIAN_POINT ( 'NONE',  ( -6.363572996767778100, 8.517530811019446091, -1.599625672291271394 ) ) ;
#63307 = CARTESIAN_POINT ( 'NONE',  ( 0.7858139957730024827, 1.945786914974199089, -0.5409757216557200543 ) ) ;
#63308 = CARTESIAN_POINT ( 'NONE',  ( -2.000000000000000000, -2.856854249492362108, 0.000000000000000000 ) ) ;
#63309 = CARTESIAN_POINT ( 'NONE',  ( 5.051972272063284031, 0.7293918257267332228, -2.189345848185173082 ) ) ;
#63311 = EDGE_CURVE ( 'NONE', #162142, #78601, #133975, .T. ) ;
#63310 = CARTESIAN_POINT ( 'NONE',  ( 5.529730448059603454, 1.891198321494348633, -0.5216162335564683561 ) ) ;
#63312 = CARTESIAN_POINT ( 'NONE',  ( 2.307404798597446849, -1.572557994556064154, -1.172606125687980061 ) ) ;
#63313 = CARTESIAN_POINT ( 'NONE',  ( 8.563946585326370098, 13.14302144952281814, 0.7998128361456462443 ) ) ;
#63314 = CARTESIAN_POINT ( 'NONE',  ( 1.777638883463141806, 0.9165151389911742053, 1.199999999999999734 ) ) ;
#63315 = ORIENTED_EDGE ( 'NONE', *, *, #5255, .F. ) ;
#63316 = CARTESIAN_POINT ( 'NONE',  ( 1.270887751945870336, -0.3167050496251391234, -2.093436144997854687 ) ) ;
#63318 = CARTESIAN_POINT ( 'NONE',  ( -8.518600588087975822, 8.832788862391110385, 1.040834085586084257E-14 ) ) ;
#63317 = CARTESIAN_POINT ( 'NONE',  ( -3.460355519985875983, 5.060167411448709629, 1.599625672291267398 ) ) ;
#63319 = CARTESIAN_POINT ( 'NONE',  ( 1.376629057770164311, 1.701771572936720212, -0.7031625657484343872 ) ) ;
#63320 = VERTEX_POINT ( 'NONE', #165366 ) ;
#63321 = CARTESIAN_POINT ( 'NONE',  ( 4.223599041728074432, 0.2716450895321539383, -2.153977947863388476 ) ) ;
#63322 = CARTESIAN_POINT ( 'NONE',  ( 11.28449857580347526, 8.706470588888119977, 3.935098853210270420 ) ) ;
#63323 = CARTESIAN_POINT ( 'NONE',  ( 1.687894460584405731, 2.027760172737497424, -0.6205009303206151516 ) ) ;
#63324 = CARTESIAN_POINT ( 'NONE',  ( 1.499999999999990896, 3.556250000682818602, 1.214306433183764966E-14 ) ) ;
#63325 = CARTESIAN_POINT ( 'NONE',  ( 8.483651433849084711, 10.92067931095586886, 1.599625672291281386 ) ) ;
#63326 = CARTESIAN_POINT ( 'NONE',  ( -9.296355089585910693E-16, 2.750000000682797818, -1.225000000000007860 ) ) ;
#63327 = CARTESIAN_POINT ( 'NONE',  ( 3.251298195952691206, -1.682652751511631850, -1.189445392860078110 ) ) ;
#63328 =( GEOMETRIC_REPRESENTATION_CONTEXT ( 3 ) GLOBAL_UNCERTAINTY_ASSIGNED_CONTEXT ( ( #181522 ) ) GLOBAL_UNIT_ASSIGNED_CONTEXT ( ( #154558, #85275, #134068 ) ) REPRESENTATION_CONTEXT ( 'NONE', 'WORKASPACE' ) );
#63330 = CARTESIAN_POINT ( 'NONE',  ( 0.7140992756325339474, 1.701125707204936166, 0.7050099338341904165 ) ) ;
#63329 = CARTESIAN_POINT ( 'NONE',  ( -7.503547950159405566, 10.84155747757291266, 1.199719254218453823 ) ) ;
#63331 = CARTESIAN_POINT ( 'NONE',  ( 1.364683531249988535, 3.863541667008087543, 0.7879004041258500513 ) ) ;
#63332 = CARTESIAN_POINT ( 'NONE',  ( 0.07735805125222076917, 2.865712030211249761, -2.577262785371988496 ) ) ;
#63333 = EDGE_CURVE ( 'NONE', #92893, #5628, #100314, .T. ) ;
#63334 = FACE_OUTER_BOUND ( 'NONE', #86548, .T. ) ;
#63335 = CARTESIAN_POINT ( 'NONE',  ( 0.1884680354247054990, -1.036234488384666586, 1.948478269905975946 ) ) ;
#63336 = CARTESIAN_POINT ( 'NONE',  ( 2.407839351892237634, -0.4975810599385386834, 2.206854368276117917 ) ) ;
#63337 = CARTESIAN_POINT ( 'NONE',  ( -8.514157279702020631, 11.91663867875229776, -1.082531754730543971 ) ) ;
#63338 = CARTESIAN_POINT ( 'NONE',  ( 2.759786284469767814, 0.6482482438519759915, -1.691825979898635035 ) ) ;
#63339 = CARTESIAN_POINT ( 'NONE',  ( 2.149496333622540334, 1.877876629180765589, -0.3779552698702989266 ) ) ;
#63340 = CARTESIAN_POINT ( 'NONE',  ( 3.350112325975619587, -0.8415805752714689003, 1.891790567983504312 ) ) ;
#63341 = CARTESIAN_POINT ( 'NONE',  ( 1.364683531249986537, 1.967708333674750731, -0.7879004041258239610 ) ) ;
#63342 = CARTESIAN_POINT ( 'NONE',  ( 1.797671122125501952, -0.6659361598389621495, 1.855707729256075522 ) ) ;
#63343 = CARTESIAN_POINT ( 'NONE',  ( 0.2352082051719720512, -1.762675558584745783, 0.7775455664775063891 ) ) ;
#63344 = CARTESIAN_POINT ( 'NONE',  ( 2.817106861211693847, -0.1851908181382568019, 1.861470920997858380 ) ) ;
#63346 = CARTESIAN_POINT ( 'NONE',  ( 4.614865537624940117, 8.465324746759504748, 0.2878883051726736086 ) ) ;
#63345 = CARTESIAN_POINT ( 'NONE',  ( 1.190513350481865240, -1.033627929232444620, 2.063343651489284003 ) ) ;
#63347 = CARTESIAN_POINT ( 'NONE',  ( 3.051044903872371261, 1.597643715361036998, -0.9542115197753370248 ) ) ;
#63348 = CARTESIAN_POINT ( 'NONE',  ( -1.201851678989727383E-14, 2.946875000341419248, -1.575800808251660134 ) ) ;
#63349 = CARTESIAN_POINT ( 'NONE',  ( 5.635237469726069648, -0.04712981909091130961, -2.062292871413499373 ) ) ;
#63350 = CIRCLE ( 'NONE', #1001, 0.07999999999999998779 ) ;
#63351 = CARTESIAN_POINT ( 'NONE',  ( -6.573005544526917099, 6.562927978236513304, -0.7998128361456291469 ) ) ;
#63352 = CARTESIAN_POINT ( 'NONE',  ( 7.182068686937156166, 9.402166106225269715, 1.599625672291281386 ) ) ;
#63353 = CARTESIAN_POINT ( 'NONE',  ( -1.476571758179682670, 3.427372387846666424, 0.2774774824061063128 ) ) ;
#63354 = CARTESIAN_POINT ( 'NONE',  ( 6.370163019944321547, 1.079249059096079044, 1.808242165975785909 ) ) ;
#63355 = CARTESIAN_POINT ( 'NONE',  ( 1.364683531249986537, 2.467708333674753174, -0.7879004041258239610 ) ) ;
#63356 = CARTESIAN_POINT ( 'NONE',  ( 5.483715611629243369, 1.447241891022777560, 1.605803905980404123 ) ) ;
#63358 = EDGE_CURVE ( 'NONE', #44776, #162623, #119887, .T. ) ;
#63357 = CARTESIAN_POINT ( 'NONE',  ( 6.059241617823571957, -1.705078594313869988, 1.082191098076368929 ) ) ;
#63359 = CARTESIAN_POINT ( 'NONE',  ( -1.364683531250014514, -0.2614583329919080157, -0.7879004041258359514 ) ) ;
#63360 = CARTESIAN_POINT ( 'NONE',  ( -5.965224400332865606, 7.022145224218852455, 1.082531754730549967 ) ) ;
#63361 = EDGE_CURVE ( 'NONE', #56186, #191954, #149552, .T. ) ;
#63362 = CIRCLE ( 'NONE', #52991, 0.08000000000000014044 ) ;
#63365 = CARTESIAN_POINT ( 'NONE',  ( 5.504247177468186258, 6.484338464210099851, 1.082531754730558626 ) ) ;
#63364 = CARTESIAN_POINT ( 'NONE',  ( 1.642778471875001811, -0.3427083328553758301, 2.845375778867859751 ) ) ;
#63363 = CARTESIAN_POINT ( 'NONE',  ( 4.850785098639300408, 8.881276058379668825, -0.7998128361456481317 ) ) ;
#63366 = CARTESIAN_POINT ( 'NONE',  ( -5.666381855868691808, 5.575476684793721383, 0.000000000000000000 ) ) ;
#63367 = CARTESIAN_POINT ( 'NONE',  ( 5.067592334412735156, 1.357865985192594271, 1.490972259599515848 ) ) ;
#63368 = CARTESIAN_POINT ( 'NONE',  ( -6.692921386640485082, 10.96015871772258521, -0.7998128361456291469 ) ) ;
#63370 = CARTESIAN_POINT ( 'NONE',  ( -6.414416072596837104, 9.537216947121368804, -1.082531754730549967 ) ) ;
#63369 = CARTESIAN_POINT ( 'NONE',  ( -3.195971524519394702, 4.751719416737803847, -1.599625672291262513 ) ) ;
#63371 = CARTESIAN_POINT ( 'NONE',  ( -1.364683531250010295, 5.030208333674757171, 0.7879004041258379498 ) ) ;
#63373 = CARTESIAN_POINT ( 'NONE',  ( 1.364683531249996529, 8.963541667008069425, 0.7879004041258403923 ) ) ;
#63372 = CARTESIAN_POINT ( 'NONE',  ( 6.016527291255574283, 1.455332790597754000, -1.598591904487467463 ) ) ;
#63374 = CARTESIAN_POINT ( 'NONE',  ( 11.48243876534946217, 9.799999999999998934, -3.200000000000001510 ) ) ;
#63375 = CARTESIAN_POINT ( 'NONE',  ( -11.67636001396849998, 7.338531100771467308, 2.777371759657221162 ) ) ;
#63377 = CARTESIAN_POINT ( 'NONE',  ( 5.448842280278080707, -1.824126957265741256, -0.8596167168879662590 ) ) ;
#63376 = CARTESIAN_POINT ( 'NONE',  ( -7.022760381754429737, 7.295567988242705582, 1.040834085586084257E-14 ) ) ;
#63378 = CARTESIAN_POINT ( 'NONE',  ( -1.402160292154681736E-14, -0.3656249996585805295, 1.575800808251672791 ) ) ;
#63379 = PRESENTATION_LAYER_ASSIGNMENT (  '', '', ( #101406 ) ) ;
#63380 = CARTESIAN_POINT ( 'NONE',  ( 1.347838067242516313, 1.722766431120416941, 0.08778956860019770936 ) ) ;
#63381 = CARTESIAN_POINT ( 'NONE',  ( 4.549643065837591038, 7.465611455855944101, -1.199719254218452047 ) ) ;
#63383 = CARTESIAN_POINT ( 'NONE',  ( 7.452141709366786770, 8.723195411463290583, 1.199719254218452047 ) ) ;
#63382 = CARTESIAN_POINT ( 'NONE',  ( 7.795575138177731844, 8.197185204069915798, 1.040834085586084257E-14 ) ) ;
#63384 = CARTESIAN_POINT ( 'NONE',  ( 8.912450614902654777, 3.507114751586604129, 8.024806578262976942 ) ) ;
#63385 = CARTESIAN_POINT ( 'NONE',  ( 6.784453417974287248, -1.834524189944960693, -0.3643881242741816573 ) ) ;
#63386 = CARTESIAN_POINT ( 'NONE',  ( 0.5221354380547962304, -2.003184638039813503, 0.1996226354380666868 ) ) ;
#63387 = SURFACE_STYLE_USAGE ( .BOTH. , #144677 ) ;
#63388 = CARTESIAN_POINT ( 'NONE',  ( 2.977765718515757332, 2.095881712254169305, -0.6909776239150815513 ) ) ;
#63389 = CARTESIAN_POINT ( 'NONE',  ( 5.823135961761455981, -1.959396665126054815, -0.9353919727212963720 ) ) ;
#63390 = ORIENTED_EDGE ( 'NONE', *, *, #171151, .T. ) ;
#63391 = CARTESIAN_POINT ( 'NONE',  ( 1.499999999999987566, -0.7249999999999825473, 0.000000000000000000 ) ) ;
#63392 = CARTESIAN_POINT ( 'NONE',  ( 8.500599125643985232, 11.90082083235127008, -1.082531754730543083 ) ) ;
#63394 = CARTESIAN_POINT ( 'NONE',  ( 2.003530013310977242, -1.955168117277843898, 0.4926643476272293820 ) ) ;
#63393 = CARTESIAN_POINT ( 'NONE',  ( 3.317144061745095129, 1.670432841370917298, -1.306055464808851818 ) ) ;
#63396 = ORIENTED_EDGE ( 'NONE', *, *, #120662, .F. ) ;
#63395 = CARTESIAN_POINT ( 'NONE',  ( 2.654344044762357413, 1.798353594787518217, 0.2176890031466270636 ) ) ;
#63397 = CARTESIAN_POINT ( 'NONE',  ( 5.363132282657546490, 8.414682208812571673, -1.199719254218452047 ) ) ;
#63398 = CARTESIAN_POINT ( 'NONE',  ( 5.341022448779654930, 8.318611059296550536, 1.199719254218462483 ) ) ;
#63399 = EDGE_CURVE ( 'NONE', #57984, #83886, #38854, .T. ) ;
#63401 = CARTESIAN_POINT ( 'NONE',  ( 1.657307721912592458, 1.831997054396968361, -0.5600143317019135036 ) ) ;
#63400 = CARTESIAN_POINT ( 'NONE',  ( -3.405069135326500351, 7.124331091189553433, 1.040834085586084257E-14 ) ) ;
#63402 = CARTESIAN_POINT ( 'NONE',  ( 0.3867890553498105066, 3.235871879154613051, -11.62250415223146938 ) ) ;
#63403 = CARTESIAN_POINT ( 'NONE',  ( 0.000000000000000000, 12.30000000000000071, 0.000000000000000000 ) ) ;
#63404 = CARTESIAN_POINT ( 'NONE',  ( 4.975479186090839612, 8.748550117173898855, 0.7216878364870438212 ) ) ;
#63405 = CARTESIAN_POINT ( 'NONE',  ( 1.364683531249988757, -0.05312499965857975237, 0.000000000000000000 ) ) ;
#63406 = CARTESIAN_POINT ( 'NONE',  ( 4.908293137491657632, 4.795002863307560759, 0.000000000000000000 ) ) ;
#63407 = CARTESIAN_POINT ( 'NONE',  ( -8.971744963941075568, 11.49012176272984931, 1.599625672291269396 ) ) ;
#63408 = ORIENTED_EDGE ( 'NONE', *, *, #150659, .F. ) ;
#63409 = CARTESIAN_POINT ( 'NONE',  ( 4.803692121107413726, -0.5798474923815257753, 2.082409481564663434 ) ) ;
#63410 = CARTESIAN_POINT ( 'NONE',  ( -3.824808732831001201, 7.476377598362539345, 0.7216878364870338292 ) ) ;
#63411 = CARTESIAN_POINT ( 'NONE',  ( 6.048345925472191631, 7.189396680206621149, 1.082531754730549967 ) ) ;
#63412 = CARTESIAN_POINT ( 'NONE',  ( 1.512141599020993432, -0.7094941370262075608, 1.998545949238240027 ) ) ;
#63414 = CARTESIAN_POINT ( 'NONE',  ( -12.06798728936711385, 5.701251286509326555, 4.345411722927631004 ) ) ;
#63413 = CARTESIAN_POINT ( 'NONE',  ( -1.001543065824772872E-14, 5.712500000000022560, 1.732050807568877637 ) ) ;
#63415 = CARTESIAN_POINT ( 'NONE',  ( 3.550034410471062163, 1.971530340838826278, 0.003394978380427334484 ) ) ;
#63416 = CARTESIAN_POINT ( 'NONE',  ( 5.924064563541377559, -1.897137492723115049, 0.2407653536913647030 ) ) ;
#63417 = ORIENTED_EDGE ( 'NONE', *, *, #76005, .F. ) ;
#63418 = CARTESIAN_POINT ( 'NONE',  ( -15.75000000000000000, 12.29999999999998295, 3.199999999999997957 ) ) ;
#63419 = CARTESIAN_POINT ( 'NONE',  ( 0.2036857628631080219, -1.599406074100502506, -1.314310892166506095 ) ) ;
#63420 = CARTESIAN_POINT ( 'NONE',  ( 2.449080105735270685, 0.5175099976203160201, -1.871664248846743872 ) ) ;
#63421 = ORIENTED_EDGE ( 'NONE', *, *, #188015, .F. ) ;
#63422 = CARTESIAN_POINT ( 'NONE',  ( 2.284651335525438309, 5.570284631188780367, 0.4445386711868243856 ) ) ;
#63424 = DIRECTION ( 'NONE',  ( 0.000000000000000000, -1.000000000000000000, 0.000000000000000000 ) ) ;
#63423 = CARTESIAN_POINT ( 'NONE',  ( -7.458393901293492334, 7.874083437696761223, 0.7216878364870317197 ) ) ;
#63426 = CARTESIAN_POINT ( 'NONE',  ( 6.817052309572890323, 6.847649204123507083, 0.7998128361456341429 ) ) ;
#63425 = CARTESIAN_POINT ( 'NONE',  ( 2.554727279587006183, -1.819456544085126026, -1.029573916123826427 ) ) ;
#63427 = CARTESIAN_POINT ( 'NONE',  ( 7.095713291905693332, 9.371694488680407886, 1.599625672291268286 ) ) ;
#63429 = ORIENTED_EDGE ( 'NONE', *, *, #10155, .F. ) ;
#63428 = CARTESIAN_POINT ( 'NONE',  ( 6.182274467271688501, 0.9872068455926674702, 1.637624497839342608 ) ) ;
#63430 = CARTESIAN_POINT ( 'NONE',  ( 4.442132104469964204, 0.9450947508268662256, -1.994404356956205548 ) ) ;
#63431 = CARTESIAN_POINT ( 'NONE',  ( 3.628125149645112568, -1.312672481567092708, -1.773765351669121415 ) ) ;
#63432 = CARTESIAN_POINT ( 'NONE',  ( 9.257519960032755790, 9.694861462993381807, 0.7998128361456462443 ) ) ;
#63433 = CARTESIAN_POINT ( 'NONE',  ( 1.822773347178743286, 1.416086463930026573, -1.285276961632122683 ) ) ;
#63434 = CARTESIAN_POINT ( 'NONE',  ( -4.083708824282378913, 7.596498746673441715, 0.5977277219625460880 ) ) ;
#63435 = CARTESIAN_POINT ( 'NONE',  ( 9.911173986789782120, 11.52179005846497972, -1.199719254218440723 ) ) ;
#63437 = CARTESIAN_POINT ( 'NONE',  ( 4.738769824615551407, -2.007376682328159134, -0.5062664373569197851 ) ) ;
#63436 = B_SPLINE_CURVE_WITH_KNOTS ( 'NONE', 3,
 ( #182537, #130693, #114433, #98137, #131724, #34164, #49369, #165238, #100235, #12583 ),
 .UNSPECIFIED., .F., .F.,
 ( 4, 3, 3, 4 ),
 ( 0.000000000000000000, 4.502046072369050747E-05, 9.004093402560574516E-05, 0.0001800865003196817178 ),
 .UNSPECIFIED. ) ;
#63438 = PRESENTATION_LAYER_ASSIGNMENT (  '', '', ( #156843 ) ) ;
#63440 = CARTESIAN_POINT ( 'NONE',  ( 1.991316529349271836, 1.880942973025516940, -1.065213018539921563 ) ) ;
#63439 = CARTESIAN_POINT ( 'NONE',  ( -3.358669367883384105, 4.941533567329135401, -1.599625672291262513 ) ) ;
#63441 = CARTESIAN_POINT ( 'NONE',  ( 5.319949580897746166, 1.306013235697962571, -1.759773446019400778 ) ) ;
#63442 = CARTESIAN_POINT ( 'NONE',  ( -5.993453320721772393, 6.500486263839809098, 0.7145505879262403770 ) ) ;
#63443 = CARTESIAN_POINT ( 'NONE',  ( -1.500000000000039524, 8.500000000000000000, -10.89724735885167739 ) ) ;
#63444 = CARTESIAN_POINT ( 'NONE',  ( 5.306037014901791693, 7.283738832175834510, 1.599625672291269396 ) ) ;
#63445 = CARTESIAN_POINT ( 'NONE',  ( -8.012344526598182026E-15, 14.10937500034139802, -1.575800808251669460 ) ) ;
#63446 = CARTESIAN_POINT ( 'NONE',  ( -6.005335696210345020, 5.970922831858983315, 0.7998128361456281477 ) ) ;
#63447 = CARTESIAN_POINT ( 'NONE',  ( 0.03578008775950020093, -1.617816776142148250, 1.203357013023528932 ) ) ;
#63448 = COLOUR_RGB ( '', 0.66274510, 0.83137255, 0.94901961) ;
#63449 = CARTESIAN_POINT ( 'NONE',  ( -9.354762803749327560, 10.01623748057011376, 0.7216878364870438212 ) ) ;
#63450 = CARTESIAN_POINT ( 'NONE',  ( 4.838769763947080804, -2.006773940031422399, -0.5081810985937407210 ) ) ;
#63451 = CARTESIAN_POINT ( 'NONE',  ( 3.686086919817387564, -0.9488725894866935073, 1.676545010912360745 ) ) ;
#63452 = CARTESIAN_POINT ( 'NONE',  ( 6.064083512088704886, -1.132370213454384045, 1.788784107109566701 ) ) ;
#63453 = CARTESIAN_POINT ( 'NONE',  ( 6.661133543015731462, 6.665743976473484267, -0.7998128361456281477 ) ) ;
#63454 = CARTESIAN_POINT ( 'NONE',  ( -1.364683531249997417, 5.759375000341418804, 1.214306433183764966E-14 ) ) ;
#63455 = CARTESIAN_POINT ( 'NONE',  ( 4.381674357853755808, -1.885861198437089437, 0.5677522405800348171 ) ) ;
#63456 = CARTESIAN_POINT ( 'NONE',  ( 5.894527261468666346, 1.877221869688485700, -1.315242172555250555 ) ) ;
#63457 = CARTESIAN_POINT ( 'NONE',  ( 4.072732355924274295, -1.704239406772959153, -0.6552279023967975125 ) ) ;
#63458 = CARTESIAN_POINT ( 'NONE',  ( 7.187230829020130329, 7.557726520044554697, 0.7216878364870267237 ) ) ;
#63459 = CARTESIAN_POINT ( 'NONE',  ( 3.321384445223597659, 6.818772919495430074, -0.7216878364870267237 ) ) ;
#63460 = CARTESIAN_POINT ( 'NONE',  ( -6.149505192250180663, 9.332117270003974951, -1.199719254218452047 ) ) ;
#63461 = CARTESIAN_POINT ( 'NONE',  ( 6.527324610336440180, 6.579909898339485252, 0.7998128361456331437 ) ) ;
#63462 = ORIENTED_EDGE ( 'NONE', *, *, #188812, .T. ) ;
#63464 = CARTESIAN_POINT ( 'NONE',  ( 5.484640381798278952, -1.273743769317101648, 1.559065439997550762 ) ) ;
#63463 = CARTESIAN_POINT ( 'NONE',  ( 1.716098596715152746, 1.718394358364897068, 0.6617865747741287219 ) ) ;
#63465 = CARTESIAN_POINT ( 'NONE',  ( 5.766309430914762224, 2.125181855325126712, -0.8765443895848085143 ) ) ;
#63466 = CARTESIAN_POINT ( 'NONE',  ( 5.418788444413384475, -1.423528547644649755, 1.350099487149841071 ) ) ;
#63467 = CARTESIAN_POINT ( 'NONE',  ( -5.032047568966410367, 9.022472597102808578, 1.214306433183764966E-14 ) ) ;
#63468 = CARTESIAN_POINT ( 'NONE',  ( -5.786632634934295361, 5.645492917045106473, 0.7998128361456341429 ) ) ;
#63469 = PRESENTATION_STYLE_ASSIGNMENT (( #12568 ) ) ;
#63470 = CARTESIAN_POINT ( 'NONE',  ( -4.797606254389363833, 6.690569611577942943, 1.599625672291263179 ) ) ;
#63472 = CARTESIAN_POINT ( 'NONE',  ( 0.4615142869485132637, 1.850934062480696252, -0.2700578556205368574 ) ) ;
#63471 = CARTESIAN_POINT ( 'NONE',  ( 1.751626234865871767, 2.084932195785852649, -0.1569159079413025293 ) ) ;
#63473 = CARTESIAN_POINT ( 'NONE',  ( 0.4963857527935924274, 7.354535952643626473, -1.939768365030055897 ) ) ;
#63474 = CARTESIAN_POINT ( 'NONE',  ( 6.351511478899689145, 1.936555568076937295, -0.1455203235936879114 ) ) ;
#63475 = CARTESIAN_POINT ( 'NONE',  ( -0.1106727585415837045, 2.871245121144291090, -2.491938459964110120 ) ) ;
#63476 = CARTESIAN_POINT ( 'NONE',  ( 0.9776059304600862587, -1.697647217183468449, -0.3827929467696991050 ) ) ;
#63477 = CARTESIAN_POINT ( 'NONE',  ( 7.474622759835693131, 7.614814729430110951, -0.7998128361456281477 ) ) ;
#63479 = CARTESIAN_POINT ( 'NONE',  ( 1.224999999999961231, 1.708333334016140181, -0.7072540797573118043 ) ) ;
#63478 = DIRECTION ( 'NONE',  ( 0.000000000000000000, -1.000000000000000000, 0.000000000000000000 ) ) ;
#63480 = CARTESIAN_POINT ( 'NONE',  ( 1.840065157383737438, 1.705764225012149859, 0.2551292777918309773 ) ) ;
#63481 = CARTESIAN_POINT ( 'NONE',  ( 1.242012060539962492, 2.189267750446591609, 0.1026977899005257211 ) ) ;
#63482 = CARTESIAN_POINT ( 'NONE',  ( -0.1405533004718754753, 0.003749010675345095921, -1.720146753850458010 ) ) ;
#63483 = CARTESIAN_POINT ( 'NONE',  ( 4.143358556170802842, -1.920740624720223666, 1.086653567583625746 ) ) ;
#63484 = CARTESIAN_POINT ( 'NONE',  ( -10.12724049293007766, 3.240713040256745003, -5.870485300885818880 ) ) ;
#63485 = CARTESIAN_POINT ( 'NONE',  ( 1.710090495726908966, 0.6328077935687204114, -2.076762233347277053 ) ) ;
#63486 = CARTESIAN_POINT ( 'NONE',  ( 1.257518954444996062, 3.091479010054028809, -0.7749999999999926947 ) ) ;
#63487 = CARTESIAN_POINT ( 'NONE',  ( 2.132168502032088409, 2.116975549207784635, 0.04667972686168975205 ) ) ;
#63488 = CARTESIAN_POINT ( 'NONE',  ( 5.477130869796502211, 5.492333557625114437, 1.040834085586084257E-14 ) ) ;
#63489 = ORIENTED_EDGE ( 'NONE', *, *, #27948, .F. ) ;
#63491 = CARTESIAN_POINT ( 'NONE',  ( -1.364683531250014514, -0.6572916663252459379, 0.7879004041258379498 ) ) ;
#63490 = CARTESIAN_POINT ( 'NONE',  ( 2.507732108623667688, -2.266951094411073786, 0.3397945559272512739 ) ) ;
#63492 = CARTESIAN_POINT ( 'NONE',  ( 0.07755575628183571102, 2.860544851022389867, -2.677061994759164065 ) ) ;
#63493 = CARTESIAN_POINT ( 'NONE',  ( 3.981290663907289140, 7.796589541200495965, -0.7998128361456221525 ) ) ;
#63494 = EDGE_CURVE ( 'NONE', #181120, #183276, #139288, .T. ) ;
#63495 = CARTESIAN_POINT ( 'NONE',  ( 6.481102860290734569, -2.029466250747449685, -0.9033904549611364576 ) ) ;
#63496 = CARTESIAN_POINT ( 'NONE',  ( -5.897433632264490910, 9.824163637709826702, 0.000000000000000000 ) ) ;
#63497 = CARTESIAN_POINT ( 'NONE',  ( 3.389175213736285386, 6.897862149426897460, 0.7216878364870317197 ) ) ;
#63498 = AXIS2_PLACEMENT_3D ( 'NONE', #40583, #60017, #38433 ) ;
#63499 = CARTESIAN_POINT ( 'NONE',  ( -7.876924059415400414, 9.252461493148505411, 1.082531754730558626 ) ) ;
#63500 = CIRCLE ( 'NONE', #15077, 0.08000000000000041800 ) ;
#63501 = CARTESIAN_POINT ( 'NONE',  ( 4.800995793014950941, 5.734154859006458160, -1.082531754730548412 ) ) ;
#63502 = ORIENTED_EDGE ( 'NONE', *, *, #132223, .T. ) ;
#63503 = CARTESIAN_POINT ( 'NONE',  ( 3.498672800139957406, -1.986100699840901651, 0.3474671148789992836 ) ) ;
#63505 = CARTESIAN_POINT ( 'NONE',  ( 2.202078444200939789, 0.7933530804136761372, -1.904077301569401914 ) ) ;
#63504 = CARTESIAN_POINT ( 'NONE',  ( 5.764187864104357573, 9.876636274763768597, 1.040834085586084257E-14 ) ) ;
#63506 = DIRECTION ( 'NONE',  ( 0.000000000000000000, 0.000000000000000000, 1.000000000000000000 ) ) ;
#63507 = CARTESIAN_POINT ( 'NONE',  ( 4.217995187182920880, 6.974725914138481642, 1.082531754730549078 ) ) ;
#63508 = CIRCLE ( 'NONE', #87776, 0.4000000000000001887 ) ;
#63509 = CARTESIAN_POINT ( 'NONE',  ( -9.606148981167596190, -6.583980363595129504, 0.4355862708379978354 ) ) ;
#63510 = CARTESIAN_POINT ( 'NONE',  ( -1.001543065824772872E-14, 5.571875000341416140, 1.575800808251672791 ) ) ;
#63511 = CARTESIAN_POINT ( 'NONE',  ( 4.787173061057010237, 1.622617466453496471, 1.473133629693436975 ) ) ;
#63512 = CARTESIAN_POINT ( 'NONE',  ( 2.022111496571117772, -1.799922141918413487, 0.9091460122201827643 ) ) ;
#63513 = CARTESIAN_POINT ( 'NONE',  ( 1.944624168438695566, -1.479605912621816621, -1.095697124569312564 ) ) ;
#63514 = CARTESIAN_POINT ( 'NONE',  ( 8.945682426918439845, 9.331051007693339727, 1.040834085586084257E-14 ) ) ;
#63516 = EDGE_CURVE ( 'NONE', #135108, #19237, #208445, .T. ) ;
#63515 =( NAMED_UNIT ( * ) PLANE_ANGLE_UNIT ( ) SI_UNIT ( $, .RADIAN. ) );
#63517 = CARTESIAN_POINT ( 'NONE',  ( 5.790036952090301448, -0.8187086143041850672, 1.631793460665122986 ) ) ;
#63518 = AXIS2_PLACEMENT_3D ( 'NONE', #204869, #85815, #69538 ) ;
#63519 = CARTESIAN_POINT ( 'NONE',  ( 6.311172677262812059, 1.158691452862798954, -1.650079838712660063 ) ) ;
#63520 = CARTESIAN_POINT ( 'NONE',  ( -7.714753101375940503, 8.959299025482085455, 1.199719254218462483 ) ) ;
#63522 = CARTESIAN_POINT ( 'NONE',  ( -5.794130544993808307, 7.853181283949808744, 1.599625672291263179 ) ) ;
#63521 = CARTESIAN_POINT ( 'NONE',  ( 5.805634902324096736, -0.5560928936223124008, 2.193004490925544392 ) ) ;
#63523 = CARTESIAN_POINT ( 'NONE',  ( 1.172648168047723649, -1.334858166028422222, 1.629009436104215558 ) ) ;
#63524 = CARTESIAN_POINT ( 'NONE',  ( -6.454563648557663846, 9.688018802362710957, -1.199719254218452047 ) ) ;
#63525 = CARTESIAN_POINT ( 'NONE',  ( 8.215351014876830504, 11.67199438640995801, -1.199719254218446718 ) ) ;
#63526 = CARTESIAN_POINT ( 'NONE',  ( 8.378074386686996888, 16.00815134976859611, 15.76159487570643414 ) ) ;
#63527 = CARTESIAN_POINT ( 'NONE',  ( -8.199983978166823562, 8.461069484149769337, -0.7998128361456291469 ) ) ;
#63528 = CARTESIAN_POINT ( 'NONE',  ( 0.5341120678215394157, 6.541965215396897904, 3.355953620529147141 ) ) ;
#63529 = CARTESIAN_POINT ( 'NONE',  ( 3.079110283634975964, 6.606396074300548982, 0.7216878364870257245 ) ) ;
#63530 = CARTESIAN_POINT ( 'NONE',  ( 5.298667053604809496, 6.361919491657284986, -1.123377533431538566 ) ) ;
#63531 = CARTESIAN_POINT ( 'NONE',  ( -8.351459436338023679, 12.68719374246231624, -0.7216878364870267237 ) ) ;
#63532 = CARTESIAN_POINT ( 'NONE',  ( 2.373529451608622054, -1.935128245189758012, -1.090680762624636868 ) ) ;
#63533 = CARTESIAN_POINT ( 'NONE',  ( 3.257290338497324633, 6.415022595892624580, -0.9198371423531578328 ) ) ;
#63534 = CARTESIAN_POINT ( 'NONE',  ( -5.315678745009726924, 8.359319748223434487, -1.199719254218453823 ) ) ;
#63535 = CARTESIAN_POINT ( 'NONE',  ( 5.880485940025228508, 7.883652901494672349, 1.599625672291267398 ) ) ;
#63536 = CARTESIAN_POINT ( 'NONE',  ( 3.051168888765115828, 1.684027830550902882, -1.006202029777767848 ) ) ;
#63537 = CARTESIAN_POINT ( 'NONE',  ( 6.322179702674084467, 6.270297829408224111, 1.040834085586084257E-14 ) ) ;
#63538 = CARTESIAN_POINT ( 'NONE',  ( -4.099542569701578820, 7.506983624740954930, -0.5818660602148464367 ) ) ;
#63539 = CARTESIAN_POINT ( 'NONE',  ( 4.871457266011829823, 4.577788319968905562, -0.7998128361456221525 ) ) ;
#63540 = CARTESIAN_POINT ( 'NONE',  ( -4.990809943606286048, 5.955604701363006015, -1.082531754730549967 ) ) ;
#63541 = CARTESIAN_POINT ( 'NONE',  ( -5.856759171423528088, 8.816340885760650892, 1.082531754730548412 ) ) ;
#63542 = CARTESIAN_POINT ( 'NONE',  ( 2.812858766682566181, -0.6196351552101020399, -2.028021595557969015 ) ) ;
#63543 = CARTESIAN_POINT ( 'NONE',  ( -4.610654757099099221, 7.536791762327691657, 1.199719254218452935 ) ) ;
#63544 = CARTESIAN_POINT ( 'NONE',  ( 4.047864428982482110, 0.7307185629543844207, -2.034579650689218866 ) ) ;
#63545 = CARTESIAN_POINT ( 'NONE',  ( 3.368544699895597461, 0.04196216268675251326, -1.840931771443871101 ) ) ;
#63546 = CARTESIAN_POINT ( 'NONE',  ( -4.373253022481784491, 7.180661499490419430, 1.044565980707335529 ) ) ;
#63547 = CARTESIAN_POINT ( 'NONE',  ( -1.402160292154681736E-14, 0.2593750003414224681, -1.575800808251665908 ) ) ;
#63548 = CARTESIAN_POINT ( 'NONE',  ( 5.613164593121685364, -1.696513092703657799, 0.3873091720919922265 ) ) ;
#63549 = CARTESIAN_POINT ( 'NONE',  ( 6.727182134110237577, 2.483225874290733159, 2.096421262816303255 ) ) ;
#63550 = CARTESIAN_POINT ( 'NONE',  ( 5.341549334104200852, 5.334155099317434257, 0.7216878364870317197 ) ) ;
#63551 = CARTESIAN_POINT ( 'NONE',  ( 0.7499999999999902300, 3.597916667349487785, -1.299038105676658228 ) ) ;
#63552 = CARTESIAN_POINT ( 'NONE',  ( 2.694378501574711926, -2.155843008138720762, -0.1600555415394027403 ) ) ;
#63553 = CARTESIAN_POINT ( 'NONE',  ( 4.095077249698628741, 1.080899603560569799, -1.701687522498253946 ) ) ;
#63554 = CARTESIAN_POINT ( 'NONE',  ( -9.476786185827959841, 10.15859809299519334, 0.7216878364870438212 ) ) ;
#63555 = CARTESIAN_POINT ( 'NONE',  ( 2.835029207381420502, 0.2633842809251253358, 2.145520918749081574 ) ) ;
#63556 = CARTESIAN_POINT ( 'NONE',  ( 2.425019040235734558, -0.003784258722050458899, 1.971530340264670889 ) ) ;
#63557 = CARTESIAN_POINT ( 'NONE',  ( -0.9311234436981447038, -2.828119629485603248, -3.475000000000004086 ) ) ;
#63558 = CARTESIAN_POINT ( 'NONE',  ( 5.056170473960743372, -1.404048225252243265, 1.341958350743667205 ) ) ;
#63561 = ORIENTED_EDGE ( 'NONE', *, *, #50156, .F. ) ;
#63560 = CARTESIAN_POINT ( 'NONE',  ( 10.99962150373185210, -9.919999999999998153, -0.09125116240077391083 ) ) ;
#63559 = CARTESIAN_POINT ( 'NONE',  ( -7.321039761255057066, 11.48503745486550365, 0.000000000000000000 ) ) ;
#63562 = CARTESIAN_POINT ( 'NONE',  ( -7.608060475923978494, 8.905100639113307182, 1.199719254218452047 ) ) ;
#63563 = CARTESIAN_POINT ( 'NONE',  ( 3.088225128862704949, 6.824956093640315302, 0.7998128361456281477 ) ) ;
#63565 = ORIENTED_EDGE ( 'NONE', *, *, #14173, .F. ) ;
#63564 = CARTESIAN_POINT ( 'NONE',  ( -5.991777542596674166, 5.955104985976372944, 0.000000000000000000 ) ) ;
#63566 = CARTESIAN_POINT ( 'NONE',  ( -9.476786185827959841, 10.15859809299519334, 0.7216878364870438212 ) ) ;
#63567 = CARTESIAN_POINT ( 'NONE',  ( 1.571597221169357628, 0.1616201177277211132, -2.200922231076734459 ) ) ;
#63569 = EDGE_CURVE ( 'NONE', #173630, #109313, #118410, .T. ) ;
#63568 = CARTESIAN_POINT ( 'NONE',  ( 1.001543065824772753E-15, -2.121874999522043836, 3.793834371823811669 ) ) ;
#63570 = CARTESIAN_POINT ( 'NONE',  ( 5.119951393648711324, 1.940949770148656661, -0.2839766199017114690 ) ) ;
#63571 = CARTESIAN_POINT ( 'NONE',  ( 1.364683531249990311, 4.946875000341417916, 1.214306433183764966E-14 ) ) ;
#63572 = CARTESIAN_POINT ( 'NONE',  ( -1.499999999999997780, 4.431250000682819490, 1.214306433183764966E-14 ) ) ;
#63573 = CARTESIAN_POINT ( 'NONE',  ( 5.142929413680796813, 6.687119857356774055, -1.406168165883972421 ) ) ;
#63574 = CARTESIAN_POINT ( 'NONE',  ( 7.777967379493318845, -6.134628647623485698, 7.664830294503448549 ) ) ;
#63575 = CARTESIAN_POINT ( 'NONE',  ( 3.784953330938052751, 1.334695924059103644, 1.268461399425282909 ) ) ;
#63576 = ORIENTED_EDGE ( 'NONE', *, *, #154299, .F. ) ;
#63577 = CARTESIAN_POINT ( 'NONE',  ( 1.360316468749949825, -0.9635416663252907021, -0.7853790794159282163 ) ) ;
#63578 = CARTESIAN_POINT ( 'NONE',  ( -6.832419346282942563, 10.05857410638369487, 1.199719254218453823 ) ) ;
#63579 = DIRECTION ( 'NONE',  ( -1.207943261119674327E-30, -2.168404344971008079E-15, 1.000000000000000000 ) ) ;
#63580 = CARTESIAN_POINT ( 'NONE',  ( 6.029554895997981667, -0.2579198037528374066, 2.104758538420265168 ) ) ;
#63581 = CARTESIAN_POINT ( 'NONE',  ( 10.89083482556480575, 8.284139440907676288, -4.931153283774001750 ) ) ;
#63582 = CARTESIAN_POINT ( 'NONE',  ( 6.972971076130050072, 7.029554431773520129, 1.040834085586084257E-14 ) ) ;
#63583 = CARTESIAN_POINT ( 'NONE',  ( 6.889916301919797981, -0.8861221739737500380, 1.859037482098152338 ) ) ;
#63586 = CARTESIAN_POINT ( 'NONE',  ( 4.036529152626888717, -1.599951230533543267, 0.9111318136766360931 ) ) ;
#63585 = CARTESIAN_POINT ( 'NONE',  ( 1.381066672459789979, -0.05041352683890670816, 1.860554536023711458 ) ) ;
#63584 = CARTESIAN_POINT ( 'NONE',  ( 4.858757509019057785, 5.629766575900002401, -2.420000000000000373 ) ) ;
#63587 = CARTESIAN_POINT ( 'NONE',  ( 8.606728586576791074, 8.935604860628076906, 0.7998128361456462443 ) ) ;
#63588 =( NAMED_UNIT ( * ) SI_UNIT ( $, .STERADIAN. ) SOLID_ANGLE_UNIT ( ) );
#63589 = CIRCLE ( 'NONE', #170727, 0.5000000000000005551 ) ;
#63590 = CARTESIAN_POINT ( 'NONE',  ( -6.526270840131767059, 8.707344961610770540, -1.599625672291271394 ) ) ;
#63591 = CARTESIAN_POINT ( 'NONE',  ( 1.499999999999990896, 5.525000000000022560, 1.214306433183764966E-14 ) ) ;
#63592 = VECTOR ( 'NONE', #48178, 1000.000000000000000 ) ;
#63593 = CARTESIAN_POINT ( 'NONE',  ( 2.789901687333019797, 1.561178712900921584, 1.560079944692857046 ) ) ;
#63594 = CARTESIAN_POINT ( 'NONE',  ( 6.327429347084096101, -2.133486974870369313, 0.7532543551938327697 ) ) ;
#63595 = CARTESIAN_POINT ( 'NONE',  ( -5.748293942514172805, 8.689798118699771479, -1.082531754730538864 ) ) ;
#63596 = CARTESIAN_POINT ( 'NONE',  ( 6.099861030166984222, 1.256130149795838813, 1.305615287863689078 ) ) ;
#63597 = B_SPLINE_CURVE_WITH_KNOTS ( 'NONE', 3,
 ( #122415, #53047, #22658, #40012, #123486, #88769 ),
 .UNSPECIFIED., .F., .F.,
 ( 4, 2, 4 ),
 ( 0.001916662113439827810, 0.002237152494173779652, 0.002557642874907731494 ),
 .UNSPECIFIED. ) ;
#63598 = CARTESIAN_POINT ( 'NONE',  ( 5.788286065124909285, -0.6962570634414954052, -1.784894364769493924 ) ) ;
#63599 = DIRECTION ( 'NONE',  ( 0.000000000000000000, 1.000000000000000000, 0.000000000000000000 ) ) ;
#63600 = CARTESIAN_POINT ( 'NONE',  ( 5.910993886665249164, 1.650546521282238110, 0.8803886038859505270 ) ) ;
#63601 = CARTESIAN_POINT ( 'NONE',  ( 6.057066403244290242, 1.520950583283819935, -1.072200347198979831 ) ) ;
#63602 = CARTESIAN_POINT ( 'NONE',  ( -0.7500000000000179856, 13.04166666666666607, 1.299038105676658228 ) ) ;
#63603 = CARTESIAN_POINT ( 'NONE',  ( 0.08069323953814251660, -0.1329233695197447052, -1.840450602299897431 ) ) ;
#63604 = CARTESIAN_POINT ( 'NONE',  ( 1.499232818411553536, -0.2420282084563407654, 2.001858358113464575 ) ) ;
#63606 = CARTESIAN_POINT ( 'NONE',  ( 3.035867697866540205, -1.414839191968674470, -1.560218430392734446 ) ) ;
#63605 = CARTESIAN_POINT ( 'NONE',  ( -7.994504133552415404, 12.47867192245318435, -0.7998128361456281477 ) ) ;
#63607 = CARTESIAN_POINT ( 'NONE',  ( 9.284636267260101050, 9.726497154758602548, -0.7998128361456281477 ) ) ;
#63609 = CARTESIAN_POINT ( 'NONE',  ( -8.371269781434001800, 11.85389961405997816, -1.199719254218446718 ) ) ;
#63608 = DIRECTION ( 'NONE',  ( 0.000000000000000000, 0.000000000000000000, 1.000000000000000000 ) ) ;
#63610 = FILL_AREA_STYLE_COLOUR ( '', #193117 ) ;
#63612 = EDGE_CURVE ( 'NONE', #210868, #133229, #187583, .T. ) ;
#63611 = CARTESIAN_POINT ( 'NONE',  ( 3.041275741140234246, 0.05373089442234183638, 2.019258232931480546 ) ) ;
#63613 = CARTESIAN_POINT ( 'NONE',  ( -1.201851678989727383E-14, 3.696875000341422801, -1.575800808251660134 ) ) ;
#63614 = CARTESIAN_POINT ( 'NONE',  ( 3.521367211247359741, 5.131347717920458962, -1.599625672291262513 ) ) ;
#63615 = CARTESIAN_POINT ( 'NONE',  ( 3.602937629199114866, 1.706465849011790104, -1.326752773236601346 ) ) ;
#63616 = CARTESIAN_POINT ( 'NONE',  ( 11.37385970535889257, 1.000000000000000888, -3.825613075418463627 ) ) ;
#63618 = LINE ( 'NONE', #65711, #76019 ) ;
#63617 = CARTESIAN_POINT ( 'NONE',  ( 7.340813827156391191, 7.528980651296110160, 0.7998128361456281477 ) ) ;
#63620 = EDGE_CURVE ( 'NONE', #163746, #20648, #205318, .T. ) ;
#63619 = CARTESIAN_POINT ( 'NONE',  ( 8.229436053370658755, 12.54483312900040026, 0.7216878364870438212 ) ) ;
#63622 = CARTESIAN_POINT ( 'NONE',  ( 7.501393976679871400, 15.44052946730700349, -9.372683453397971931 ) ) ;
#63621 = CARTESIAN_POINT ( 'NONE',  ( 0.7487581336349375949, -2.154818914559033072, -0.2656684361399003214 ) ) ;
#63623 = CARTESIAN_POINT ( 'NONE',  ( -6.182154858151506893, 9.195969186943299789, 1.082531754730548412 ) ) ;
#63624 = ADVANCED_FACE ( 'NONE', ( #105741 ), #39632, .T. ) ;
#63625 = CARTESIAN_POINT ( 'NONE',  ( -1.364683531250000748, 1.259375000341421469, 0.000000000000000000 ) ) ;
#63626 = CARTESIAN_POINT ( 'NONE',  ( 2.437293137456029157, -1.626093413141915134, -1.469474007205706645 ) ) ;
#63627 = CARTESIAN_POINT ( 'NONE',  ( 0.09868764650533826122, 7.157731444430377898, 1.998865700660830358 ) ) ;
#63628 = CARTESIAN_POINT ( 'NONE',  ( 2.747247497433321861, -1.881545503785379436, 1.256212651835092231 ) ) ;
#63629 = CARTESIAN_POINT ( 'NONE',  ( -6.995117189646935962, 10.24838825697502109, 1.199719254218453823 ) ) ;
#63630 = CARTESIAN_POINT ( 'NONE',  ( -3.755245360860931303, 5.404205559136275205, -1.443375672974051449 ) ) ;
#63631 = CARTESIAN_POINT ( 'NONE',  ( -0.6823417656249969321, 3.280208333674754062, -1.181850606188749264 ) ) ;
#63632 = CARTESIAN_POINT ( 'NONE',  ( 5.732961426666957294, 7.278201736375829789, 1.206439608388230500 ) ) ;
#63633 = CARTESIAN_POINT ( 'NONE',  ( 1.500000000000001332, 10.37499999999999467, 0.000000000000000000 ) ) ;
#63634 = CARTESIAN_POINT ( 'NONE',  ( 5.072158865288222351, 8.931619419562697004, 0.7216878364870317197 ) ) ;
#63635 = CARTESIAN_POINT ( 'NONE',  ( 3.110363945789674123, 1.284354398739546266, -1.217803596734900573 ) ) ;
#63636 = CARTESIAN_POINT ( 'NONE',  ( 9.260382613333817403, 10.76253345609967660, -1.199719254218446718 ) ) ;
#63637 = CARTESIAN_POINT ( 'NONE',  ( 5.948300505803370442, 2.203960110721484789, 0.1139900122707343255 ) ) ;
#63638 = CARTESIAN_POINT ( 'NONE',  ( 0.6823417656249969321, 9.026041667008065872, -1.181850606188757036 ) ) ;
#63639 = CARTESIAN_POINT ( 'NONE',  ( -3.610214042988883598, 7.433943160120816351, 0.7998128361456352531 ) ) ;
#63640 = DIRECTION ( 'NONE',  ( 0.000000000000000000, 0.000000000000000000, 1.000000000000000000 ) ) ;
#63641 = ORIENTED_EDGE ( 'NONE', *, *, #118518, .F. ) ;
#63642 = CARTESIAN_POINT ( 'NONE',  ( 3.572993900519233712, 0.04689164532409998559, -1.870237235490713079 ) ) ;
#63643 = CARTESIAN_POINT ( 'NONE',  ( 3.432542862244458259, -1.236986750340131724, 1.659893174209552846 ) ) ;
#63644 = AXIS2_PLACEMENT_3D ( 'NONE', #188449, #92050, #9696 ) ;
#63645 = EDGE_CURVE ( 'NONE', #176780, #199252, #163481, .T. ) ;
#63646 = CARTESIAN_POINT ( 'NONE',  ( -1.813763795902447518, 3.999999999999955147, 0.4499999999999590994 ) ) ;
#63647 = DIRECTION ( 'NONE',  ( 0.000000000000000000, 1.000000000000000000, 0.000000000000000000 ) ) ;
#63648 = CARTESIAN_POINT ( 'NONE',  ( -10.10707714348148301, 4.359868340440408829, -5.857196085253971063 ) ) ;
#63649 = CARTESIAN_POINT ( 'NONE',  ( 9.452953268198900361, 3.481540744127369802, 7.393265152228856607 ) ) ;
#63650 = CIRCLE ( 'NONE', #198460, 11.00000000000000000 ) ;
#63651 = CARTESIAN_POINT ( 'NONE',  ( -1.201851678989727383E-14, 3.759375000341422801, -1.575800808251660134 ) ) ;
#63652 = CARTESIAN_POINT ( 'NONE',  ( 1.283307755816986528, 0.1377011610334301639, -1.907463248872851347 ) ) ;
#63653 = CARTESIAN_POINT ( 'NONE',  ( 2.646866301197240645, -0.3325320220872363675, -1.933311746529025266 ) ) ;
#63654 = CARTESIAN_POINT ( 'NONE',  ( 1.264999722075825561, -2.016288307338756525, -0.002813990012486000669 ) ) ;
#63655 = CARTESIAN_POINT ( 'NONE',  ( -5.984998465789844069, 5.947196063035064206, 0.7998128361456281477 ) ) ;
#63657 =( NAMED_UNIT ( * ) SI_UNIT ( $, .STERADIAN. ) SOLID_ANGLE_UNIT ( ) );
#63656 = CARTESIAN_POINT ( 'NONE',  ( 8.959240580532112475, 9.346868853575953651, -0.7998128361456221525 ) ) ;
#63658 = CARTESIAN_POINT ( 'NONE',  ( 6.889933812677610625, -0.8438472966565238043, 1.779621742589713618 ) ) ;
#63659 = CARTESIAN_POINT ( 'NONE',  ( 0.6823417656249899377, 4.176041667008085767, -1.181850606188754593 ) ) ;
#63660 = CARTESIAN_POINT ( 'NONE',  ( 1.406495263175694399, -2.003875642784687994, -0.1933051647188162026 ) ) ;
#63662 = CARTESIAN_POINT ( 'NONE',  ( 2.741944773236061117, 2.106750310803459758, -0.2105854985169057503 ) ) ;
#63661 = CARTESIAN_POINT ( 'NONE',  ( -7.049876689426113785, 8.287572894827684777, -1.082531754730544860 ) ) ;
#63663 = CARTESIAN_POINT ( 'NONE',  ( 8.880206826883428661, 12.81886467739263402, -8.003364354211651488 ) ) ;
#63664 = CARTESIAN_POINT ( 'NONE',  ( 3.385274849524767316, 0.04804411014160993310, 2.069964801482151895 ) ) ;
#63665 = CARTESIAN_POINT ( 'NONE',  ( 3.223806664999388172, 6.983134552466421674, -0.7998128361456362523 ) ) ;
#63667 = CARTESIAN_POINT ( 'NONE',  ( 4.216749469050096621, 4.878294787768598262, -1.199719254218452047 ) ) ;
#63666 = CARTESIAN_POINT ( 'NONE',  ( 6.246049398119083662, 0.6547385654485110562, 1.985528007121174943 ) ) ;
#63669 = ORIENTED_EDGE ( 'NONE', *, *, #3140, .F. ) ;
#63668 = CARTESIAN_POINT ( 'NONE',  ( 4.084828617465196210, -0.1788469021064206521, -1.816781805555576668 ) ) ;
#63670 = CARTESIAN_POINT ( 'NONE',  ( 8.367353357928214663, 12.91366268422496688, 1.040834085586084257E-14 ) ) ;
#63671 = CARTESIAN_POINT ( 'NONE',  ( 7.788485247869523675, -6.306978362809961602, -7.768428355095886140 ) ) ;
#63672 = CARTESIAN_POINT ( 'NONE',  ( 10.32570460010716396, 11.37497670666806826, 7.285500311179339938 ) ) ;
#63673 = CARTESIAN_POINT ( 'NONE',  ( 6.352570083819033542, 0.6862697483850827007, 2.097430819677794656 ) ) ;
#63674 = CARTESIAN_POINT ( 'NONE',  ( -1.402160292154681736E-14, 11.23437500034139624, 1.575800808251682339 ) ) ;
#63675 = CARTESIAN_POINT ( 'NONE',  ( 5.338497774373327509, 1.135723818413657549, -1.538349510941657838 ) ) ;
#63676 = CARTESIAN_POINT ( 'NONE',  ( -8.462260433223891098, 13.02438760540324481, -0.7998128361456281477 ) ) ;
#63677 = CARTESIAN_POINT ( 'NONE',  ( 6.435316467980822353, 10.65961964595298817, 1.040834085586084257E-14 ) ) ;
#63678 = CARTESIAN_POINT ( 'NONE',  ( -0.6801582343750334214, 1.213541667008023683, 1.178068619123810334 ) ) ;
#63679 = CARTESIAN_POINT ( 'NONE',  ( 2.995988758495615745, 6.439144618312774959, -0.7216878364870267237 ) ) ;
#63680 = PRESENTATION_STYLE_ASSIGNMENT (( #160118 ) ) ;
#63681 = CARTESIAN_POINT ( 'NONE',  ( 0.4152503475762689411, -0.9843521281015167324, -1.555853522519357712 ) ) ;
#63682 = ORIENTED_EDGE ( 'NONE', *, *, #181883, .T. ) ;
#63683 = CARTESIAN_POINT ( 'NONE',  ( 4.182764291190976813, -0.1809548918480126112, -1.861743760598027597 ) ) ;
#63684 = CARTESIAN_POINT ( 'NONE',  ( -0.02319159430947368913, 6.948789054712430691, -2.406029888528108618 ) ) ;
#63685 = CARTESIAN_POINT ( 'NONE',  ( 4.993145711582793744, 9.047363440147082159, -0.7998128361456481317 ) ) ;
#63686 = CARTESIAN_POINT ( 'NONE',  ( -1.499999999999996003, 8.226475397236011844, -3.114076396431513682 ) ) ;
#63687 = CARTESIAN_POINT ( 'NONE',  ( -5.472807559815892731, 7.501441282320147508, 1.250076539767187578 ) ) ;
#63688 = SHAPE_REPRESENTATION ( 'air flow regulation', ( #200407 ), #83064 ) ;
#63690 = CARTESIAN_POINT ( 'NONE',  ( -5.748293942514172805, 8.689798118699771479, -1.082531754730538864 ) ) ;
#63689 =( GEOMETRIC_REPRESENTATION_CONTEXT ( 3 ) GLOBAL_UNCERTAINTY_ASSIGNED_CONTEXT ( ( #161602 ) ) GLOBAL_UNIT_ASSIGNED_CONTEXT ( ( #201277, #170931, #105994 ) ) REPRESENTATION_CONTEXT ( 'NONE', 'WORKASPACE' ) );
#63691 = CARTESIAN_POINT ( 'NONE',  ( 3.310162060030825248, 7.013606170011280838, -0.7998128361456291469 ) ) ;
#63692 = CARTESIAN_POINT ( 'NONE',  ( 0.9538786243144499188, -0.7140540310214549269, 1.835613268467409576 ) ) ;
#63693 = CARTESIAN_POINT ( 'NONE',  ( 2.794546173781168541, 1.458544728081469177, -1.392559875802508396 ) ) ;
#63694 = CARTESIAN_POINT ( 'NONE',  ( -8.830438121202295321, 9.196599317691152464, -0.7998128361456291469 ) ) ;
#63695 = CARTESIAN_POINT ( 'NONE',  ( 5.337069745634900997, 6.255611453776062980, 1.199719254218452047 ) ) ;
#63696 = CARTESIAN_POINT ( 'NONE',  ( 0.2999999999999686806, 3.950000000000016165, 1.007084189318352863 ) ) ;
#63697 = CARTESIAN_POINT ( 'NONE',  ( 2.080269975650438585, -2.149535124392497831, -0.4257020960420563882 ) ) ;
#63698 = CARTESIAN_POINT ( 'NONE',  ( -9.053093885623068715, 11.58502883802551153, -1.599625672291263179 ) ) ;
#63699 = CARTESIAN_POINT ( 'NONE',  ( 6.825078400183570260, 4.696493799637426747, 2.518305144748238966 ) ) ;
#63700 = LINE ( 'NONE', #47478, #101999 ) ;
#63701 = FACE_OUTER_BOUND ( 'NONE', #207342, .T. ) ;
#63702 = CARTESIAN_POINT ( 'NONE',  ( 8.341290820905593151, 10.75459192918846618, 1.599625672291281386 ) ) ;
#63703 = CARTESIAN_POINT ( 'NONE',  ( 6.211043768836173484, 8.339580045099285854, 1.443375672974065660 ) ) ;
#63704 = VERTEX_POINT ( 'NONE', #25511 ) ;
#63706 = CARTESIAN_POINT ( 'NONE',  ( 1.664698924820615433, 0.6334283372178346472, 1.910891431425953302 ) ) ;
#63705 = CARTESIAN_POINT ( 'NONE',  ( 5.337399561049260832, 0.7408347518493042516, -1.685818907712175019 ) ) ;
#63707 = CARTESIAN_POINT ( 'NONE',  ( 3.128558558221442354, 0.3401759809690939051, -2.272988164180503201 ) ) ;
#63709 = CARTESIAN_POINT ( 'NONE',  ( 2.324856365976185391, -1.699136111967664453, -0.7594513203179918959 ) ) ;
#63708 = DIRECTION ( 'NONE',  ( -0.7592566023653004592, -0.6507913734559641616, 0.000000000000000000 ) ) ;
#63710 = CARTESIAN_POINT ( 'NONE',  ( 1.642778471875001811, -2.092708332855373943, 2.845375778867859751 ) ) ;
#63711 = CARTESIAN_POINT ( 'NONE',  ( -9.367496996292747014, 15.51845925588232333, -7.500000001629758550 ) ) ;
#63712 = CARTESIAN_POINT ( 'NONE',  ( 5.994389040191065554, -1.017321598621454548, 1.619163160827830517 ) ) ;
#63713 = CARTESIAN_POINT ( 'NONE',  ( -9.006694118179950692, 9.402231314165087284, 1.040834085586084257E-14 ) ) ;
#63714 = CARTESIAN_POINT ( 'NONE',  ( -4.638297949650955765, 8.425448351319163365, 0.7216878364870267237 ) ) ;
#63716 = CARTESIAN_POINT ( 'NONE',  ( 3.660894226558962128, -1.649352935060313552, -0.8826137995501317501 ) ) ;
#63715 = CARTESIAN_POINT ( 'NONE',  ( 4.968349523292523884, -1.969100025901071360, -0.7031758509000278767 ) ) ;
#63717 = CARTESIAN_POINT ( 'NONE',  ( 7.456621297836072415, 9.722477485607340597, 1.443375672974076540 ) ) ;
#63718 = CARTESIAN_POINT ( 'NONE',  ( 6.392148736875968851, -0.4980823202534767624, -1.772533436741857260 ) ) ;
#63719 = CARTESIAN_POINT ( 'NONE',  ( 4.033714395265605823, 4.664753868353354704, -1.199719254218446718 ) ) ;
#63720 = CARTESIAN_POINT ( 'NONE',  ( -1.500000000000022204, 6.200000000000045475, 2.580000000000011173 ) ) ;
#63721 = CARTESIAN_POINT ( 'NONE',  ( 5.057137062068671973, -1.459852279745242010, -0.9183987515692086934 ) ) ;
#63722 = CARTESIAN_POINT ( 'NONE',  ( -4.903245109636583443, 8.872203061218007392, -0.7998128361456281477 ) ) ;
#63723 = CARTESIAN_POINT ( 'NONE',  ( 1.874158809982156670, 3.299964346911599122, 0.3999999999999681033 ) ) ;
#63724 = CARTESIAN_POINT ( 'NONE',  ( -3.621833129746822255, 4.096114899008192367, -2.420000000000000373 ) ) ;
#63725 = CARTESIAN_POINT ( 'NONE',  ( 4.364261492936694076, -2.165649721281979190, 0.1538544128360258556 ) ) ;
#63726 = CARTESIAN_POINT ( 'NONE',  ( 3.510199737632841543, -0.7410081052188906003, -1.668730646197075673 ) ) ;
#63727 = CARTESIAN_POINT ( 'NONE',  ( 1.604273143990111672, 1.959273547513197711, 0.1016356785708133759 ) ) ;
#63728 = CARTESIAN_POINT ( 'NONE',  ( 0.2810647479330531939, 1.757583132164267647, -1.180221762011339326 ) ) ;
#63730 = CARTESIAN_POINT ( 'NONE',  ( 1.364683531249988535, 3.926041667008087543, 0.7879004041258500513 ) ) ;
#63729 = CARTESIAN_POINT ( 'NONE',  ( 6.480031627576305020, -2.247188937338239434, -0.4521185302251101157 ) ) ;
#63731 = CARTESIAN_POINT ( 'NONE',  ( 3.332168893502837737, 7.719402352559943559, 2.450693629706348631 ) ) ;
#63732 = CARTESIAN_POINT ( 'NONE',  ( 7.540305987494599016, 11.94877408538573427, -0.7998128361456291469 ) ) ;
#63733 = EDGE_CURVE ( 'NONE', #179825, #183713, #102994, .T. ) ;
#63734 = CARTESIAN_POINT ( 'NONE',  ( 2.578903501431661915, -1.460476376761214556, 1.537597662120089081 ) ) ;
#63735 = CARTESIAN_POINT ( 'NONE',  ( -3.741687207691642314, 6.348756928073427730, 1.082531754730560403 ) ) ;
#63736 = CLOSED_SHELL ( 'NONE', ( #172437, #78294, #160656, #34764, #101479, #64064, #45767, #34888 ) ) ;
#63737 = CARTESIAN_POINT ( 'NONE',  ( -5.707619481228834779, 5.761236937629489852, -0.7216878364870197293 ) ) ;
#63738 = CARTESIAN_POINT ( 'NONE',  ( 0.2392000317489213768, -0.1454578200970526591, -2.037356452166842580 ) ) ;
#63740 = CARTESIAN_POINT ( 'NONE',  ( 1.499999999999997113, 13.92708333401613352, -0.8660254037844378194 ) ) ;
#63739 = CARTESIAN_POINT ( 'NONE',  ( 6.883263157960330503, 7.629137130509037412, 2.553810918356711479 ) ) ;
#63742 = ORIENTED_EDGE ( 'NONE', *, *, #149120, .F. ) ;
#63741 = CARTESIAN_POINT ( 'NONE',  ( 2.614199364429617756, -0.6941352821057051870, 2.110140411616817868 ) ) ;
#63743 = CARTESIAN_POINT ( 'NONE',  ( 0.1593517250534680629, 1.330572521919655360, 1.874314102060254505 ) ) ;
#63745 = CARTESIAN_POINT ( 'NONE',  ( 5.717653809678179044, 0.4078037869292486239, -2.021697613586806774 ) ) ;
#63744 = CARTESIAN_POINT ( 'NONE',  ( 4.304877467538922531, 4.981110786005563007, 1.199719254218464037 ) ) ;
#63747 = CARTESIAN_POINT ( 'NONE',  ( -1.737500000000000266, -1.808333333333332016, -3.009438278150923907 ) ) ;
#63746 = CARTESIAN_POINT ( 'NONE',  ( 5.448397627845284141, 7.449826213943242514, 1.599625672291268286 ) ) ;
#63748 = CARTESIAN_POINT ( 'NONE',  ( 4.929271367020211514, 7.908511140569038922, 1.199719254218452047 ) ) ;
#63749 = CARTESIAN_POINT ( 'NONE',  ( -3.285556943750000514, -3.376041666188708490, -1.896917185911906500 ) ) ;
#63750 = CARTESIAN_POINT ( 'NONE',  ( 0.1331565106231328566, 1.371277436080810208, -2.201942895618694607 ) ) ;
#63751 = CARTESIAN_POINT ( 'NONE',  ( 5.495603940606402560, -1.841430844871448258, 0.006098274996368944698 ) ) ;
#63752 = CARTESIAN_POINT ( 'NONE',  ( 5.681030059326015014, 6.586622143090519188, -1.199719254218445830 ) ) ;
#63753 = SHAPE_REPRESENTATION_RELATIONSHIP ( 'NONE' , 'NONE' ,  #203468, #37156 ) ;
#63754 = CARTESIAN_POINT ( 'NONE',  ( 1.904884197260014567, 1.431573929998239958, 0.9616530215695131556 ) ) ;
#63755 = CARTESIAN_POINT ( 'NONE',  ( 1.622280145275534435, 1.995268681201247452, 0.2910785328335343536 ) ) ;
#63756 = CARTESIAN_POINT ( 'NONE',  ( 2.268584743917153368, 2.099868620093465754, -0.9355518099330699666 ) ) ;
#63757 = CARTESIAN_POINT ( 'NONE',  ( -1.201851678989727383E-14, 4.009375000341416140, -1.575800808251660134 ) ) ;
#63758 = CARTESIAN_POINT ( 'NONE',  ( 1.968429645022830465, 1.162096202078844120, 1.940986467279571359 ) ) ;
#63759 = CARTESIAN_POINT ( 'NONE',  ( 4.301466803424673913, 1.691180239654224815, 1.254954771472403641 ) ) ;
#63760 = CARTESIAN_POINT ( 'NONE',  ( -4.981695098378565945, 4.776675467721892332, -0.7998128361456362523 ) ) ;
#63761 = CARTESIAN_POINT ( 'NONE',  ( 2.846658922380195911, -1.473647421164023141, 0.9796213258056789552 ) ) ;
#63762 = CARTESIAN_POINT ( 'NONE',  ( 7.311924916471702396, 7.425000578838787391, -0.7998128361456281477 ) ) ;
#63764 = CARTESIAN_POINT ( 'NONE',  ( 5.636350782834250062, 0.4440221345313396517, 2.248805093627189500 ) ) ;
#63763 = CARTESIAN_POINT ( 'NONE',  ( 3.879041346841291649, 7.539648981374564407, 1.040834085586084257E-14 ) ) ;
#63765 = CARTESIAN_POINT ( 'NONE',  ( -5.284980951228653190, 5.060232619388524533, 0.000000000000000000 ) ) ;
#63766 = CARTESIAN_POINT ( 'NONE',  ( -1.500000000000013101, 2.170833333333357373, 0.8660254037844403729 ) ) ;
#63767 = CARTESIAN_POINT ( 'NONE',  ( 6.117462548578989967, 1.846355941783444976, 1.234888080409371369 ) ) ;
#63768 = CARTESIAN_POINT ( 'NONE',  ( 4.365290731249091394, 2.125951747006165959, -0.5312598475561494116 ) ) ;
#63769 = CARTESIAN_POINT ( 'NONE',  ( -4.569261463005423352, 5.289558780716470565, -1.199719254218446718 ) ) ;
#63770 = CARTESIAN_POINT ( 'NONE',  ( 0.4942023283146224633, 7.349555083877798545, -1.940391385854344897 ) ) ;
#63771 = CARTESIAN_POINT ( 'NONE',  ( 6.604144390287855160, -0.9070803646254663732, 1.914764756563241965 ) ) ;
#63772 =( BOUNDED_SURFACE ( )  B_SPLINE_SURFACE ( 3, 3, ( 
 ( #57961, #124126, #190088, #92631, #41741, #107852, #173878, #5979, #157615, #72050, #25452 ),
 ( #141397, #207407, #55825, #125184, #108918, #174940, #26522, #158672, #10269, #121981, #95827 ),
 ( #94757, #194363, #143527, #213777, #49192, #131547, #197548, #160806, #15587, #130514, #178128 ),
 ( #144595, #78476, #96897, #195442, #176001, #12397, #128396, #79547, #209523, #46005, #161884 ),
 ( #48145, #111048, #62237, #113189, #179195, #210609, #147760, #145665, #14526, #30818, #162946 ),
 ( #177055, #212730, #77411, #97956, #27593, #28672, #61164, #81674, #13471, #112124, #211663 ),
 ( #93691, #127326, #80623, #29744, #164012, #47072, #159734, #146713, #63299, #11332, #193296 ) ),
 .UNSPECIFIED., .T., .F., .F. ) 
 B_SPLINE_SURFACE_WITH_KNOTS ( ( 4, 3, 4 ),
 ( 4, 1, 1, 1, 1, 1, 1, 1, 4 ),
 ( 0.000000000000000000, 0.5000000000000000000, 1.000000000000000000 ),
 ( 0.000000000000000000, 0.2256337125576066971, 0.3978389261578171299, 0.5257960283851228489, 0.6187025735204009225, 0.6856790771877526725, 0.7354782194756434022, 0.7762620033627533056, 0.9999999999999998890 ),
 .UNSPECIFIED. ) 
 GEOMETRIC_REPRESENTATION_ITEM ( )  RATIONAL_B_SPLINE_SURFACE ( (
 ( 1.000000000000000000, 1.000000000000000000, 1.000000000000000222, 1.000000000000000000, 0.9999999999999997780, 1.000000000000000222, 0.9999999999999997780, 1.000000000000000222, 0.9999999999999992228, 1.000000000000000000, 1.000000000000000000),
 ( 0.3333333333333333703, 0.3333333333333334259, 0.3333333333333334259, 0.3333333333333333703, 0.3333333333333333148, 0.3333333333333334259, 0.3333333333333333703, 0.3333333333333334259, 0.3333333333333330928, 0.3333333333333333703, 0.3333333333333333703),
 ( 0.3333333333333333703, 0.3333333333333334259, 0.3333333333333334259, 0.3333333333333333703, 0.3333333333333333148, 0.3333333333333334259, 0.3333333333333333703, 0.3333333333333334259, 0.3333333333333330928, 0.3333333333333333703, 0.3333333333333333703),
 ( 1.000000000000000000, 1.000000000000000000, 1.000000000000000222, 1.000000000000000000, 0.9999999999999997780, 1.000000000000000222, 0.9999999999999997780, 1.000000000000000222, 0.9999999999999992228, 1.000000000000000000, 1.000000000000000000),
 ( 0.3333333333333333703, 0.3333333333333334259, 0.3333333333333334259, 0.3333333333333333703, 0.3333333333333333148, 0.3333333333333334259, 0.3333333333333333703, 0.3333333333333334259, 0.3333333333333330928, 0.3333333333333333703, 0.3333333333333333703),
 ( 0.3333333333333333703, 0.3333333333333334259, 0.3333333333333334259, 0.3333333333333333703, 0.3333333333333333148, 0.3333333333333334259, 0.3333333333333333703, 0.3333333333333334259, 0.3333333333333330928, 0.3333333333333333703, 0.3333333333333333703),
 ( 1.000000000000000000, 1.000000000000000000, 1.000000000000000222, 1.000000000000000000, 0.9999999999999997780, 1.000000000000000222, 0.9999999999999997780, 1.000000000000000222, 0.9999999999999992228, 1.000000000000000000, 1.000000000000000000) ) ) 
 REPRESENTATION_ITEM ( '' )  SURFACE ( )  );
#63773 = CARTESIAN_POINT ( 'NONE',  ( -1.364683531249997417, 3.509375000341423245, 1.214306433183764966E-14 ) ) ;
#63774 = CARTESIAN_POINT ( 'NONE',  ( -0.6823417656250039265, 8.567708333674733723, -1.181850606188755259 ) ) ;
#63775 = CARTESIAN_POINT ( 'NONE',  ( -3.470524135418300737, 6.032400010421219427, -1.082531754730549967 ) ) ;
#63776 = CARTESIAN_POINT ( 'NONE',  ( 5.994406619193555663, -1.133004004027007294, 1.792352430775605798 ) ) ;
#63777 = CARTESIAN_POINT ( 'NONE',  ( -5.153507786970262572, 9.026526494858359229, -0.7216878364870338292 ) ) ;
#63778 = ORIENTED_EDGE ( 'NONE', *, *, #173881, .T. ) ;
#63780 = CARTESIAN_POINT ( 'NONE',  ( 4.393008644795362905, 7.016788222801661590, 1.284222742053114041 ) ) ;
#63779 = CARTESIAN_POINT ( 'NONE',  ( -3.526529353330350336, 7.128384988945109413, -0.7216878364870458196 ) ) ;
#63781 = CARTESIAN_POINT ( 'NONE',  ( 3.354752944377597856, 6.001296637494123232, -1.199719254218446718 ) ) ;
#63782 = CARTESIAN_POINT ( 'NONE',  ( 5.671403949121008203, 1.101820082107987098, 1.475039313902235305 ) ) ;
#63783 = SURFACE_SIDE_STYLE ('',( #178619 ) ) ;
#63784 = FACE_OUTER_BOUND ( 'NONE', #95844, .T. ) ;
#63785 = CARTESIAN_POINT ( 'NONE',  ( 1.364683531249988535, 4.176041667008081326, 0.7879004041258500513 ) ) ;
#63786 = CARTESIAN_POINT ( 'NONE',  ( 1.733560280482333571, 1.721479560191770730, 0.2551580012965410371 ) ) ;
#63787 = DIRECTION ( 'NONE',  ( 0.000000000000000000, -1.000000000000000000, 0.000000000000000000 ) ) ;
#63788 = CARTESIAN_POINT ( 'NONE',  ( 0.1390251588108057101, -0.1389306544097475005, -1.930426113910483688 ) ) ;
#63789 = CARTESIAN_POINT ( 'NONE',  ( 0.6823417656249882723, -0.01145833299191073573, -1.181850606188749264 ) ) ;
#63790 = DIRECTION ( 'NONE',  ( -0.1669130127894878912, 0.9056625952363902554, -0.3897631457067520788 ) ) ;
#63791 = CARTESIAN_POINT ( 'NONE',  ( 6.315313271410192719, -0.2696487299426887363, 2.144762774094311375 ) ) ;
#63792 = AXIS2_PLACEMENT_3D ( 'NONE', #95712, #198490, #195324 ) ;
#63793 = CARTESIAN_POINT ( 'NONE',  ( -2.123823618835070537, 5.629544655282869847, 1.040834085586084257E-14 ) ) ;
#63794 = CARTESIAN_POINT ( 'NONE',  ( -6.033015167956805591, 8.061603667414825480, -1.443375672974058777 ) ) ;
#63795 = CARTESIAN_POINT ( 'NONE',  ( 5.770447993230207295, -1.374857387916775364, 1.668144713590607120 ) ) ;
#63797 = VERTEX_POINT ( 'NONE', #40720 ) ;
#63796 = CARTESIAN_POINT ( 'NONE',  ( -1.499999999999997780, 6.200000000000045475, -2.579999999999995630 ) ) ;
#63798 = CARTESIAN_POINT ( 'NONE',  ( 1.364683531249988535, 3.905208333674751842, -0.7879004041258239610 ) ) ;
#63799 = CARTESIAN_POINT ( 'NONE',  ( 5.800065155369113157, -1.971530342684927772, -0.002616305567698303924 ) ) ;
#63800 = CARTESIAN_POINT ( 'NONE',  ( 5.360564742968721319, -0.6223997329263281086, 1.618453672356393147 ) ) ;
#63802 = CARTESIAN_POINT ( 'NONE',  ( 1.400213348495438437, -0.7931047570679079506, -2.043190674350242819 ) ) ;
#63801 = CARTESIAN_POINT ( 'NONE',  ( -0.6801582343750213200, -0.3177083329919394572, 1.178068619123815663 ) ) ;
#63803 = CARTESIAN_POINT ( 'NONE',  ( 3.839178312322106823, 0.3354718084071331430, 2.282954970297036201 ) ) ;
#63804 = CARTESIAN_POINT ( 'NONE',  ( 5.466112512051848782, 1.011855222795062348, 1.795159749414678929 ) ) ;
#63805 = CARTESIAN_POINT ( 'NONE',  ( 1.130689739129210336, -1.755767597885007136, 0.8300169520328912753 ) ) ;
#63806 = CARTESIAN_POINT ( 'NONE',  ( -6.683806541412776525, 7.860491055478785682, -1.082531754730543083 ) ) ;
#63807 = CARTESIAN_POINT ( 'NONE',  ( -4.329849954717889915, 6.144853928627882489, 1.599625672291270506 ) ) ;
#63808 = CARTESIAN_POINT ( 'NONE',  ( 0.000000000000000000, -0.5000000000000004441, 0.000000000000000000 ) ) ;
#63809 = CARTESIAN_POINT ( 'NONE',  ( 3.515986968957810266, -0.6120941298391362473, 2.030368431519948391 ) ) ;
#63810 = FILL_AREA_STYLE ('',( #142972 ) ) ;
#63811 = CARTESIAN_POINT ( 'NONE',  ( 2.057267738415057057, -1.238319999287675888, 1.591319116112683618 ) ) ;
#63812 = CARTESIAN_POINT ( 'NONE',  ( -6.358410854684793279, 7.480862754296137673, -1.082531754730543083 ) ) ;
#63813 = CARTESIAN_POINT ( 'NONE',  ( 4.436686946050734548, 2.163524548302516060, 0.4339203326570104102 ) ) ;
#63814 = CARTESIAN_POINT ( 'NONE',  ( -5.606595252507366567, 5.572856915785063592, -0.3451608010808376870 ) ) ;
#63815 = B_SPLINE_CURVE_WITH_KNOTS ( 'NONE', 3,
 ( #35905, #153937, #185348, #136626, #21757, #34829 ),
 .UNSPECIFIED., .F., .F.,
 ( 4, 2, 4 ),
 ( 0.000000000000000000, 0.0003346294579448544793, 0.0006692589158897089587 ),
 .UNSPECIFIED. ) ;
#63816 = CARTESIAN_POINT ( 'NONE',  ( -10.15205317230718407, 3.956598013261175772, 5.494609294606044081 ) ) ;
#63817 = AXIS2_PLACEMENT_3D ( 'NONE', #177483, #141826, #206764 ) ;
#63818 = CARTESIAN_POINT ( 'NONE',  ( -1.499999999999997780, 4.931250000682820378, 1.214306433183764808E-14 ) ) ;
#63819 = CARTESIAN_POINT ( 'NONE',  ( -5.966470118465691641, 9.118576350588734059, -1.199719254218452047 ) ) ;
#63821 = CARTESIAN_POINT ( 'NONE',  ( 0.000000000000000000, 13.87999999999998302, 0.000000000000000000 ) ) ;
#63820 = CARTESIAN_POINT ( 'NONE',  ( -5.137161949866410282, 7.898551110135567654, 1.241398918778359173 ) ) ;
#63822 = CARTESIAN_POINT ( 'NONE',  ( -3.023105066167347310, 5.702484939155337607, 2.420000000000010587 ) ) ;
#63823 = ORIENTED_EDGE ( 'NONE', *, *, #57465, .T. ) ;
#63824 = CARTESIAN_POINT ( 'NONE',  ( 3.942301955389547974, 2.050809467686238285, 0.2036389587714466376 ) ) ;
#63825 = CARTESIAN_POINT ( 'NONE',  ( 1.360316468749947605, 2.536458333674726173, -0.7853790794159141164 ) ) ;
#63826 = UNCERTAINTY_MEASURE_WITH_UNIT (LENGTH_MEASURE( 1.000000000000000082E-05 ), #58068, 'distance_accuracy_value', 'NONE');
#63827 = CARTESIAN_POINT ( 'NONE',  ( 0.4655551865852024518, -8.176568542494939251, 9.512045263456274213 ) ) ;
#63828 = CARTESIAN_POINT ( 'NONE',  ( -4.232116505760120440, 8.089219690028791376, -0.7998128361456281477 ) ) ;
#63829 = CARTESIAN_POINT ( 'NONE',  ( -5.655686355556086120, 6.627330832017406692, 1.199719254218452935 ) ) ;
#63830 = CARTESIAN_POINT ( 'NONE',  ( 3.633467297704314980, -0.1462457305761339643, 2.014424004083538833 ) ) ;
#63831 = CARTESIAN_POINT ( 'NONE',  ( -0.7500000000000006661, 1.358333333333357151, -1.299038105676652011 ) ) ;
#63832 = CARTESIAN_POINT ( 'NONE',  ( 3.602716132929354664, 5.226254793216122074, 1.599625672291267398 ) ) ;
#63833 = CARTESIAN_POINT ( 'NONE',  ( 5.947222937888848371, 10.09017719417900416, 1.040834085586084257E-14 ) ) ;
#63834 = CARTESIAN_POINT ( 'NONE',  ( 3.274343757225039120, -1.228935477529419451, 1.654214949985348904 ) ) ;
#63835 = CARTESIAN_POINT ( 'NONE',  ( -6.328041841479842056, 6.870487382198048998, 0.6860574420480938240 ) ) ;
#63836 = CARTESIAN_POINT ( 'NONE',  ( 5.518332215962025167, 6.396807992499198292, -1.199719254218445830 ) ) ;
#63837 = CARTESIAN_POINT ( 'NONE',  ( -0.1616376092239741047, 8.277406474725948371, -1.999409923707612391 ) ) ;
#63839 =( GEOMETRIC_REPRESENTATION_CONTEXT ( 3 ) GLOBAL_UNCERTAINTY_ASSIGNED_CONTEXT ( ( #149286 ) ) GLOBAL_UNIT_ASSIGNED_CONTEXT ( ( #76691, #205618, #159022 ) ) REPRESENTATION_CONTEXT ( 'NONE', 'WORKASPACE' ) );
#63838 = CARTESIAN_POINT ( 'NONE',  ( 1.675478281319711549, -0.9859397310463119402, 1.554705294492392254 ) ) ;
#63840 = CARTESIAN_POINT ( 'NONE',  ( 0.03047818801908425135, -1.425887938121385590, -1.815451699675968644 ) ) ;
#63841 = CARTESIAN_POINT ( 'NONE',  ( 4.362691568547328202, 8.311833606605697256, -0.7998128361456381397 ) ) ;
#63842 = CARTESIAN_POINT ( 'NONE',  ( 2.601032539102793084, 1.737798908178284307, -1.285340053188685383 ) ) ;
#63843 = CARTESIAN_POINT ( 'NONE',  ( -2.480778921620681921, 5.838066475291996404, 1.040834085586084257E-14 ) ) ;
#63844 = CARTESIAN_POINT ( 'NONE',  ( 4.048151681910251654, 1.001636719310808887, 1.865476516996619649 ) ) ;
#63845 = CARTESIAN_POINT ( 'NONE',  ( 2.935265884076414977, 1.227738246725296634, 1.942841054583419602 ) ) ;
#63846 = DIRECTION ( 'NONE',  ( -0.7071067811865457964, 0.7071067811865492381, 6.410781031902129473E-32 ) ) ;
#63847 = CARTESIAN_POINT ( 'NONE',  ( 0.9009904985227291663, 1.526999960511504772, 1.080287613699250304 ) ) ;
#63848 = CARTESIAN_POINT ( 'NONE',  ( 4.328955620115590541, 0.09577655398496780215, 1.969249263103334702 ) ) ;
#63849 = PRESENTATION_LAYER_ASSIGNMENT (  '', '', ( #178131 ) ) ;
#63850 = CARTESIAN_POINT ( 'NONE',  ( 4.803922858132807505, -1.082837210388952309, -1.700963621564715700 ) ) ;
#63852 = SPHERICAL_SURFACE ( 'NONE', #88176, 0.08000000000000000167 ) ;
#63851 = CARTESIAN_POINT ( 'NONE',  ( 1.364683531249988535, 3.113541667008083991, 0.7879004041258500513 ) ) ;
#63854 = CARTESIAN_POINT ( 'NONE',  ( 5.742829910930518977, 0.4094298153964996967, 2.065706902019475599 ) ) ;
#63853 = CARTESIAN_POINT ( 'NONE',  ( -5.554036483092550824, 9.631459663583308739, -0.7998128361456231517 ) ) ;
#63855 = CARTESIAN_POINT ( 'NONE',  ( 6.549288556030710140, 1.803345607721940524, -1.016871928424132099 ) ) ;
#63856 = CARTESIAN_POINT ( 'NONE',  ( 6.440286661691305703, 7.472421512516709718, 1.199719254218462483 ) ) ;
#63857 = CARTESIAN_POINT ( 'NONE',  ( -4.876128802409253282, 8.840567369452784874, 0.7998128361456481317 ) ) ;
#63858 = CARTESIAN_POINT ( 'NONE',  ( 6.639320575229288757, 4.694344378759712555, 2.565881548192010975 ) ) ;
#63859 = CARTESIAN_POINT ( 'NONE',  ( 4.961777154302105863, 1.950117994852887282, -0.2885197095366370257 ) ) ;
#63860 = CARTESIAN_POINT ( 'NONE',  ( 6.275650217586050239, 0.3411474428106214263, -1.990588700022011714 ) ) ;
#63861 = CARTESIAN_POINT ( 'NONE',  ( -1.402160292154681736E-14, -0.2562499993171780122, 1.732050807568877637 ) ) ;
#63862 = CARTESIAN_POINT ( 'NONE',  ( 4.881611394917170443, 2.154576904714616603, -0.8270325966449257882 ) ) ;
#63863 = AXIS2_PLACEMENT_3D ( 'NONE', #88787, #170009, #137539 ) ;
#63864 = CARTESIAN_POINT ( 'NONE',  ( 2.307554651200398599, -1.654038752482372088, -1.231991790176652612 ) ) ;
#63865 = CARTESIAN_POINT ( 'NONE',  ( 6.466876084038451822, 10.48851316477946582, 1.040834085586084257E-14 ) ) ;
#63866 = CARTESIAN_POINT ( 'NONE',  ( 4.420840606507738357, 7.315341919971147355, 1.199719254218451159 ) ) ;
#63867 = CARTESIAN_POINT ( 'NONE',  ( 5.086243903782109221, 5.962981304947771122, -1.199719254218452047 ) ) ;
#63868 = CARTESIAN_POINT ( 'NONE',  ( -1.201851678989727383E-14, 1.634375000341421025, 1.575800808251672791 ) ) ;
#63869 = CARTESIAN_POINT ( 'NONE',  ( 5.063044020060520900, 4.871582543017558109, 0.7998128361456352531 ) ) ;
#63870 = CARTESIAN_POINT ( 'NONE',  ( 6.683806541412754321, 8.820860269780128604, -1.443375672974058777 ) ) ;
#63871 = CARTESIAN_POINT ( 'NONE',  ( 3.895131827238162536, 0.3151296210822142063, 2.148063795774640461 ) ) ;
#63872 = CARTESIAN_POINT ( 'NONE',  ( -3.273028085023368394, -0.8887487162373572946, -0.3592362057191292868 ) ) ;
#63874 = CARTESIAN_POINT ( 'NONE',  ( 2.964219115174483665, -1.702287218311925310, -0.7022057971969236645 ) ) ;
#63873 = CARTESIAN_POINT ( 'NONE',  ( -2.467220768007014176, 5.822248629409386922, 0.7216878364870317197 ) ) ;
#63875 = EDGE_CURVE ( 'NONE', #164527, #54346, #173938, .T. ) ;
#63876 = CARTESIAN_POINT ( 'NONE',  ( 1.364683531249990311, 4.134375000341417028, 1.214306433183764966E-14 ) ) ;
#63877 = CARTESIAN_POINT ( 'NONE',  ( 5.372676843235411503, -0.05303982195071360595, -2.191091664329389399 ) ) ;
#63878 = CARTESIAN_POINT ( 'NONE',  ( 9.579665964948885559, -7.246166700194470067, 0.07999999999999847511 ) ) ;
#63879 = CARTESIAN_POINT ( 'NONE',  ( 6.455986150183742112, 2.257016316038124693, -0.1587017259171065731 ) ) ;
#63880 = CARTESIAN_POINT ( 'NONE',  ( -5.775737613422593952, 6.228167737865282660, -1.031624843267029190 ) ) ;
#63881 = CARTESIAN_POINT ( 'NONE',  ( 5.469253881944042384, 7.602781119232224327, 1.336104631850141944 ) ) ;
#63882 = CARTESIAN_POINT ( 'NONE',  ( -4.950135482320918712, 7.828889591799445213, -1.082531754730549967 ) ) ;
#63883 = CARTESIAN_POINT ( 'NONE',  ( -0.1236583036082171405, 1.000000000000000888, 11.99936284241579898 ) ) ;
#63884 = CARTESIAN_POINT ( 'NONE',  ( 6.362547694819080668, -1.249765848162401438, 1.253281529121505589 ) ) ;
#63885 = CARTESIAN_POINT ( 'NONE',  ( 4.459639246686514902, -1.557681092447872784, -1.275236256583739403 ) ) ;
#63886 = CARTESIAN_POINT ( 'NONE',  ( 7.305145839664861640, 7.417091655897478653, 0.7998128361456341429 ) ) ;
#63887 = CARTESIAN_POINT ( 'NONE',  ( 2.749164281075014760, -1.751614713500139198, 1.168827980950073009 ) ) ;
#63888 = CARTESIAN_POINT ( 'NONE',  ( 2.601083430876732105, -0.1850255667073404386, 1.906624535778883578 ) ) ;
#63889 = CARTESIAN_POINT ( 'NONE',  ( 3.440018289565364817, 5.036440642624797626, 1.599625672291267398 ) ) ;
#63890 = CARTESIAN_POINT ( 'NONE',  ( 3.684007040126308752, -1.171275171843730867, -1.583282632743492790 ) ) ;
#63891 = CARTESIAN_POINT ( 'NONE',  ( 1.604156678829884886, -0.6703249191640224813, -1.746612230856612769 ) ) ;
#63892 = CARTESIAN_POINT ( 'NONE',  ( 2.418345249890076154, 0.8361516037145629854, 1.774881043358336630 ) ) ;
#63895 = ORIENTED_EDGE ( 'NONE', *, *, #72507, .F. ) ;
#63894 = CARTESIAN_POINT ( 'NONE',  ( 0.3340484552533556362, -1.024938778295768849, -1.614363347046356756 ) ) ;
#63893 = CARTESIAN_POINT ( 'NONE',  ( 3.598037535421601429, -1.723020282968828809, -0.08274337828741322454 ) ) ;
#63897 = CARTESIAN_POINT ( 'NONE',  ( 6.480434237652135998, 6.662854153456708950, 0.7216878364870317197 ) ) ;
#63896 = CARTESIAN_POINT ( 'NONE',  ( 1.717678464306471309, -0.2677704892378242607, 2.190511422692428045 ) ) ;
#63898 = CARTESIAN_POINT ( 'NONE',  ( -0.6823417656250212460, 1.113541667008083325, 1.181850606188755259 ) ) ;
#63899 = CARTESIAN_POINT ( 'NONE',  ( 11.48767021851168124, 12.26995772536169227, -3.470194894594655910 ) ) ;
#63900 = CARTESIAN_POINT ( 'NONE',  ( 1.123270288254022198, 3.158552654332631882, -0.7749999999939810591 ) ) ;
#63901 = CARTESIAN_POINT ( 'NONE',  ( 6.663994888585877518, -7.154544010627095219, -6.770610912236881163 ) ) ;
#63902 = CARTESIAN_POINT ( 'NONE',  ( 6.877786287229037399, -2.009644702432196617, 0.4970176993947388322 ) ) ;
#63903 = EDGE_CURVE ( 'NONE', #90583, #147438, #70046, .T. ) ;
#63904 = CARTESIAN_POINT ( 'NONE',  ( 1.416557266959647787, 0.8372786474034592530, 1.893679232998768391 ) ) ;
#63905 = CARTESIAN_POINT ( 'NONE',  ( 0.7499999999999885647, 2.316666666666689078, -1.299038105676652899 ) ) ;
#63906 = CARTESIAN_POINT ( 'NONE',  ( 6.856673000209174695, 9.022537805042615489, 1.599625672291281386 ) ) ;
#63907 = CARTESIAN_POINT ( 'NONE',  ( -7.167456763118792651, 11.51378332361394818, 0.000000000000000000 ) ) ;
#63908 = CARTESIAN_POINT ( 'NONE',  ( 5.499767588998890844, 6.445425604367387429, 1.199719254218451159 ) ) ;
#63909 = CARTESIAN_POINT ( 'NONE',  ( 5.461630201184114242, -1.671734486004393450, -1.304435072541964447 ) ) ;
#63910 = CARTESIAN_POINT ( 'NONE',  ( 1.781714131423858791E-15, -3.430288072414404179E-15, 0.2598076211376221800 ) ) ;
#63911 = CARTESIAN_POINT ( 'NONE',  ( -1.201851678989727383E-14, 2.946875000341419248, -1.575800808251660134 ) ) ;
#63912 = CARTESIAN_POINT ( 'NONE',  ( 1.499999999999987121, 2.795833333333352488, -0.8660254037844262731 ) ) ;
#63914 = CARTESIAN_POINT ( 'NONE',  ( 3.009020027229115879, 5.597941567487558778, -1.199719254218446718 ) ) ;
#63913 = CARTESIAN_POINT ( 'NONE',  ( 6.443807124430430910, 1.351966286592180211, 1.421895456074427688 ) ) ;
#63915 = CARTESIAN_POINT ( 'NONE',  ( 3.813827237909522605, -1.649828814528127907, 1.158511658058670957 ) ) ;
#63916 = CARTESIAN_POINT ( 'NONE',  ( 4.047977829471119726, 0.9080738158676031624, 1.686857792009839097 ) ) ;
#63917 = DIRECTION ( 'NONE',  ( -0.6507913734559640506, -0.7592566023653004592, 0.000000000000000000 ) ) ;
#63918 = CARTESIAN_POINT ( 'NONE',  ( 1.716621854089026344, 2.046377219401524616, 0.7848826361863748824 ) ) ;
#63919 = CARTESIAN_POINT ( 'NONE',  ( -11.04536101718726293, 11.00581159806359288, -1.100000000000000311 ) ) ;
#63920 = CARTESIAN_POINT ( 'NONE',  ( 1.499999999999987121, 0.8270833340161471980, -0.8660254037844253849 ) ) ;
#63921 = CARTESIAN_POINT ( 'NONE',  ( 4.974862723197266412, -1.455255168294814272, 1.391337642457886270 ) ) ;
#63922 = CARTESIAN_POINT ( 'NONE',  ( -6.989391883044787868, 8.113044270762433285, -1.199719254218446718 ) ) ;
#63924 = CARTESIAN_POINT ( 'NONE',  ( 5.800440434243619769, 1.421441630026821112, -1.569310636533404635 ) ) ;
#63923 = CARTESIAN_POINT ( 'NONE',  ( -2.955314298098991266, 6.391691081183366485, 0.7216878364870317197 ) ) ;
#63925 = CARTESIAN_POINT ( 'NONE',  ( 0.6823417656249934904, 9.005208333674726617, 1.181850606188764807 ) ) ;
#63927 = CARTESIAN_POINT ( 'NONE',  ( -7.781453819600577582, 8.043060642480948985, 0.000000000000000000 ) ) ;
#63926 = CARTESIAN_POINT ( 'NONE',  ( 2.560199545759346496, -1.439800679921798165, 1.516228354532923372 ) ) ;
#63929 = ORIENTED_EDGE ( 'NONE', *, *, #106815, .T. ) ;
#63928 = CARTESIAN_POINT ( 'NONE',  ( 0.3578718668165404293, 0.6529773653428347924, 1.596609206317510132 ) ) ;
#63930 = CARTESIAN_POINT ( 'NONE',  ( 6.856673000209174695, 9.022537805042615489, 1.599625672291281386 ) ) ;
#63931 = DIRECTION ( 'NONE',  ( 0.000000000000000000, 0.000000000000000000, -1.000000000000000000 ) ) ;
#63932 = PLANE ( 'NONE',  #16988 ) ;
#63933 = SURFACE_STYLE_FILL_AREA ( #62863 ) ;
#63935 = CARTESIAN_POINT ( 'NONE',  ( 8.053180056393003383, 12.33920113252646367, 1.040834085586084257E-14 ) ) ;
#63934 = CARTESIAN_POINT ( 'NONE',  ( 5.621827251160867789, 9.710548892996357040, 1.040834085586084257E-14 ) ) ;
#63937 = ORIENTED_EDGE ( 'NONE', *, *, #71089, .F. ) ;
#63936 = B_SPLINE_CURVE_WITH_KNOTS ( 'NONE', 3,
 ( #204294, #172917, #42925, #171832, #106890, #24492, #90603, #156663, #142567, #158786, #10383, #8255 ),
 .UNSPECIFIED., .F., .F.,
 ( 4, 2, 2, 2, 2, 4 ),
 ( 4.249187360970357138E-18, 0.0007306567756924711851, 0.001095985163538703254, 0.001461313551384934998, 0.002191970327077403472, 0.002922627102769872164 ),
 .UNSPECIFIED. ) ;
#63938 = CARTESIAN_POINT ( 'NONE',  ( 1.403499169903295263, 7.376709478543810761, -4.304123474983216902 ) ) ;
#63939 = ORIENTED_EDGE ( 'NONE', *, *, #137980, .T. ) ;
#63941 = CARTESIAN_POINT ( 'NONE',  ( 1.875370188833940244, 0.3090493442242334132, -1.784726349569294213 ) ) ;
#63940 = CARTESIAN_POINT ( 'NONE',  ( 5.529746549527311039, 7.544733289238903851, -1.599625672291281386 ) ) ;
#63942 = CARTESIAN_POINT ( 'NONE',  ( -5.357443255694392725, 9.402100898285455699, 0.000000000000000000 ) ) ;
#63943 = CARTESIAN_POINT ( 'NONE',  ( 4.330940004561544043, 7.140181541042074365, -1.199719254218452047 ) ) ;
#63944 = CARTESIAN_POINT ( 'NONE',  ( 4.715203562502613188, 8.723097599553565118, 0.7998128361456341429 ) ) ;
#63945 = LINE ( 'NONE', #49827, #142946 ) ;
#63946 = CARTESIAN_POINT ( 'NONE',  ( 2.359223927328457648E-13, 7.078193277237625480, 2.121339347286388843 ) ) ;
#63947 = CARTESIAN_POINT ( 'NONE',  ( 4.052428274714076295, 7.522979123003127988, 0.4826459875755910733 ) ) ;
#63948 = CARTESIAN_POINT ( 'NONE',  ( 10.38518247838791986, 11.21839376764850726, 0.7216878364870438212 ) ) ;
#63949 = VERTEX_POINT ( 'NONE', #124182 ) ;
#63950 = CARTESIAN_POINT ( 'NONE',  ( 3.191705266286504639, -1.248028223939607884, -1.380750640708436006 ) ) ;
#63951 = CARTESIAN_POINT ( 'NONE',  ( 0.7904806358284102163, 1.449672126929082872, -1.252262404471200075 ) ) ;
#63952 = CARTESIAN_POINT ( 'NONE',  ( 6.633821588623410648, -1.258873362295178655, -1.458256629947017879 ) ) ;
#63953 = VECTOR ( 'NONE', #149804, 1000.000000000000114 ) ;
#63954 = CARTESIAN_POINT ( 'NONE',  ( -1.333315192109771230, 8.250054423670807324, -10.85938449304424402 ) ) ;
#63955 = CARTESIAN_POINT ( 'NONE',  ( -11.86145016429273191, 10.90000000000000036, 1.099999999999996758 ) ) ;
#63956 = CARTESIAN_POINT ( 'NONE',  ( 4.644395130292630292, 8.311692339142366492, -0.4369040224408097250 ) ) ;
#63957 = CARTESIAN_POINT ( 'NONE',  ( 11.86239285000045740, 11.37999999999999901, -1.812080536912752837 ) ) ;
#63958 = CARTESIAN_POINT ( 'NONE',  ( -4.134873662487946966, 3.926366815765101936, 1.214306433183764966E-14 ) ) ;
#63959 = AXIS2_PLACEMENT_3D ( 'NONE', #180909, #198211, #131167 ) ;
#63960 = CARTESIAN_POINT ( 'NONE',  ( 8.446366511633696561, 8.956441806435218922, 1.040834085586084257E-14 ) ) ;
#63961 = CARTESIAN_POINT ( 'NONE',  ( 4.785976182654667177, -1.208483435658064487, -1.555025035033012148 ) ) ;
#63962 = CARTESIAN_POINT ( 'NONE',  ( 1.383610671357866639, 0.1525377206293351273, -2.115047022047947589 ) ) ;
#63963 = CARTESIAN_POINT ( 'NONE',  ( -4.229253852459088137, 7.021547696922494808, 1.199719254218464037 ) ) ;
#63964 = CARTESIAN_POINT ( 'NONE',  ( -11.95485154007906914, 9.001110132796746655, 0.3045117111943428934 ) ) ;
#63965 = CARTESIAN_POINT ( 'NONE',  ( -3.103560622218558329, 6.448189014018472776, -0.7351483804875698080 ) ) ;
#63966 = CARTESIAN_POINT ( 'NONE',  ( 5.578137875217415775, -2.137416510240647494, -0.4829537091169676666 ) ) ;
#63967 = CARTESIAN_POINT ( 'NONE',  ( -6.305925513666572613, 6.529536985466737775, -1.006778644550405474E-06 ) ) ;
#63968 = CARTESIAN_POINT ( 'NONE',  ( 5.350583055395741638, 0.5590458624239265095, 1.843501136262601037 ) ) ;
#63969 = CARTESIAN_POINT ( 'NONE',  ( -6.287230548435221777, 8.358188277972981695, -1.599625672291263179 ) ) ;
#63970 = CARTESIAN_POINT ( 'NONE',  ( 0.09436191691250192526, -0.3928898508825870439, -1.789253991261535726 ) ) ;
#63971 = CARTESIAN_POINT ( 'NONE',  ( 1.120068590173186163, -2.152398693614396397, 0.4866647226241942459 ) ) ;
#63972 = CARTESIAN_POINT ( 'NONE',  ( -6.097415271940877624, 7.027018469112610077, 0.9862998271150682505 ) ) ;
#63973 = CARTESIAN_POINT ( 'NONE',  ( -0.2108831679770960255, -0.001785917861228669690, -1.896958272444612792 ) ) ;
#63974 =( BOUNDED_CURVE ( )  B_SPLINE_CURVE ( 2, ( #78422, #1143, #110995, #142399, #208407, #13417, #175944 ),
 .UNSPECIFIED., .F., .T. ) 
 B_SPLINE_CURVE_WITH_KNOTS ( ( 3, 2, 2, 3 ),
 ( 0.07142857142857149400, 0.07738095238095236972, 0.08333333333333324544, 0.08928571428571412116 ),
 .UNSPECIFIED. ) 
 CURVE ( )  GEOMETRIC_REPRESENTATION_ITEM ( )  RATIONAL_B_SPLINE_CURVE ( ( 0.9999999999999984457, 0.8660254037844402619, 1.000000000000000000, 0.8660254037844387076, 1.000000000000000000, 0.8660254037844424824, 0.9999999999999962252 ) ) 
 REPRESENTATION_ITEM ( '' )  );
#63975 = ORIENTED_EDGE ( 'NONE', *, *, #179709, .T. ) ;
#63976 = CIRCLE ( 'NONE', #167259, 0.08000000000000044575 ) ;
#63977 = VERTEX_POINT ( 'NONE', #70669 ) ;
#63978 = CARTESIAN_POINT ( 'NONE',  ( 6.086760365903021608, 1.896989206666617633, 0.5289026096024685986 ) ) ;
#63979 = CARTESIAN_POINT ( 'NONE',  ( 1.927192517792934101, -1.269957001497720395, -1.469349730274618571 ) ) ;
#63980 = ORIENTED_EDGE ( 'NONE', *, *, #24241, .F. ) ;
#63981 = CARTESIAN_POINT ( 'NONE',  ( 0.9837497097957871306, 1.861730512597782550, 0.7742002051285418185 ) ) ;
#63983 = CARTESIAN_POINT ( 'NONE',  ( 5.963677626732073023, -0.4536248188283693583, 1.804646041804882195 ) ) ;
#63982 = CARTESIAN_POINT ( 'NONE',  ( -6.954406449166956605, 7.078172043641714595, -0.7998128361456362523 ) ) ;
#63984 = CARTESIAN_POINT ( 'NONE',  ( 6.574778147984297938, 6.635272358928617997, -0.7998128361456481317 ) ) ;
#63985 =( NAMED_UNIT ( * ) PLANE_ANGLE_UNIT ( ) SI_UNIT ( $, .RADIAN. ) );
#63986 = CARTESIAN_POINT ( 'NONE',  ( 4.081882008079450230, 3.980588341361369853, -0.7346435760097062007 ) ) ;
#63987 = CARTESIAN_POINT ( 'NONE',  ( -6.013204822860843457, 6.974159367214481264, -1.199719254218446718 ) ) ;
#63988 = CARTESIAN_POINT ( 'NONE',  ( -7.587723245503481095, 8.881373870289390737, 1.199719254218452047 ) ) ;
#63989 = CARTESIAN_POINT ( 'NONE',  ( 1.997856853652695497, -2.190977152517746163, 0.05759783203293508680 ) ) ;
#63990 = CARTESIAN_POINT ( 'NONE',  ( 4.202664430556257713, 4.965825259479493603, 1.082531754730560403 ) ) ;
#63991 = CARTESIAN_POINT ( 'NONE',  ( -1.123270288249905713, 3.300000000000025135, 0.7750000000000117906 ) ) ;
#63992 = PRESENTATION_STYLE_ASSIGNMENT (( #65035 ) ) ;
#63993 = CARTESIAN_POINT ( 'NONE',  ( 1.224926655537651676, -0.04696546880481740349, 1.825250005322680780 ) ) ;
#63994 = CARTESIAN_POINT ( 'NONE',  ( -2.611917148927046295, 6.198987107056845858, 1.040834085586084257E-14 ) ) ;
#63995 = CARTESIAN_POINT ( 'NONE',  ( -6.218052724642120666, 7.025831364812846758, -1.032658732443512584 ) ) ;
#63996 = CARTESIAN_POINT ( 'NONE',  ( 6.609000000000047947, 7.052356515605485932, 2.698153947863399793 ) ) ;
#63997 = CIRCLE ( 'NONE', #25938, 2.500000000000007994 ) ;
#63998 = CARTESIAN_POINT ( 'NONE',  ( 8.028399517586572998, 12.51821653715971472, -0.7998128361456352531 ) ) ;
#63999 = CARTESIAN_POINT ( 'NONE',  ( 6.674438497507635404, -1.118711561685633349, 1.443368817030561635 ) ) ;
#64000 = CARTESIAN_POINT ( 'NONE',  ( 5.014483083204026137, 0.7471541359172823027, 1.814103259000845680 ) ) ;
#64001 = CARTESIAN_POINT ( 'NONE',  ( -7.720478407978036195, 11.09464301169468037, -1.199719254218446718 ) ) ;
#64002 = CARTESIAN_POINT ( 'NONE',  ( 6.311484202361478779, 7.322151976631905868, -1.199719254218446718 ) ) ;
#64003 = EDGE_CURVE ( 'NONE', #130351, #157630, #35432, .T. ) ;
#64004 = CARTESIAN_POINT ( 'NONE',  ( 3.404031855413204966, -0.8899279105200922357, -2.002928011436304612 ) ) ;
#64005 = STYLED_ITEM ( 'NONE', ( #22040 ), #86932 ) ;
#64006 = CARTESIAN_POINT ( 'NONE',  ( -1.500000000000008216, 9.781250000682799595, 3.469446951953614189E-15 ) ) ;
#64007 = CARTESIAN_POINT ( 'NONE',  ( 3.696198088285786998, 0.9351842759567146057, -1.847102243037239910 ) ) ;
#64009 = CARTESIAN_POINT ( 'NONE',  ( -0.6823417656250212460, 1.113541667008083325, 1.181850606188755259 ) ) ;
#64008 = DIRECTION ( 'NONE',  ( 0.000000000000000000, 0.000000000000000000, -1.000000000000000000 ) ) ;
#64010 = ORIENTED_EDGE ( 'NONE', *, *, #171411, .T. ) ;
#64011 = CARTESIAN_POINT ( 'NONE',  ( 3.727375017909192234, 2.287664543646179105, 0.2247039424928508056 ) ) ;
#64012 = CARTESIAN_POINT ( 'NONE',  ( 7.782016984564060103, 9.141736572488651902, 1.082531754730558626 ) ) ;
#64014 = CARTESIAN_POINT ( 'NONE',  ( -3.285556943750000514, -0.4885416661887091450, -1.896917185911906500 ) ) ;
#64013 = CARTESIAN_POINT ( 'NONE',  ( 6.712695452541852070, 7.004101914153185504, 0.000000000000000000 ) ) ;
#64015 = CARTESIAN_POINT ( 'NONE',  ( 6.620655732516649294, 2.985444497229528427, 2.280274006979409407 ) ) ;
#64016 = CARTESIAN_POINT ( 'NONE',  ( -9.670288946796535612, 4.446955533403587069, -7.032531191595068343 ) ) ;
#64017 = CARTESIAN_POINT ( 'NONE',  ( 4.136618238866495822, -1.688923885309162376, 0.9583718017313649362 ) ) ;
#64018 = ORIENTED_EDGE ( 'NONE', *, *, #47626, .F. ) ;
#64021 = EDGE_CURVE ( 'NONE', #118628, #126440, #53012, .T. ) ;
#64020 = CARTESIAN_POINT ( 'NONE',  ( -0.1363799957457066114, -9.242177669965698783, 9.620888806888750366 ) ) ;
#64019 = AXIS2_PLACEMENT_3D ( 'NONE', #152689, #100737, #184110 ) ;
#64022 = CARTESIAN_POINT ( 'NONE',  ( 3.797043250571481732, -0.1924442655423033721, -1.902711443722324258 ) ) ;
#64023 = PLANE ( 'NONE',  #196871 ) ;
#64024 = CARTESIAN_POINT ( 'NONE',  ( 5.227475398614537916, -1.636741361296644603, 0.5442337529403593610 ) ) ;
#64025 = CARTESIAN_POINT ( 'NONE',  ( 4.259000112335223243, -0.004834882008357410665, -2.016708403958865414 ) ) ;
#64026 = CARTESIAN_POINT ( 'NONE',  ( 5.133504205653830255, 0.6649215086056580182, 2.200401518963719383 ) ) ;
#64027 = CARTESIAN_POINT ( 'NONE',  ( 1.220146605508150803E-14, 9.687500000000000000, -1.499999999999998446 ) ) ;
#64028 = CARTESIAN_POINT ( 'NONE',  ( 1.190363680384380229, -0.9894552095768920363, 1.972713631218452557 ) ) ;
#64030 = CARTESIAN_POINT ( 'NONE',  ( -4.014622883422322985, 7.697827440719083647, -0.7216878364870458196 ) ) ;
#64029 = CARTESIAN_POINT ( 'NONE',  ( -9.236128959407555072, 11.79856975744075598, -1.599625672291263179 ) ) ;
#64031 = CARTESIAN_POINT ( 'NONE',  ( 6.344957943996793581, -1.493715166628902580, 0.9487403735100213842 ) ) ;
#64033 = CARTESIAN_POINT ( 'NONE',  ( 2.502247188656173016, -0.8787990176886916194, -2.117303525603573267 ) ) ;
#64032 = CARTESIAN_POINT ( 'NONE',  ( 5.040599249230596435, 9.102725900736217568, 0.7998128361456341429 ) ) ;
#64034 = CARTESIAN_POINT ( 'NONE',  ( 1.306181984371343585, 1.533458449073618057, 0.8229166363448844335 ) ) ;
#64035 = B_SPLINE_CURVE_WITH_KNOTS ( 'NONE', 3,
 ( #46109, #212836, #77514, #29850, #163053, #112227 ),
 .UNSPECIFIED., .F., .F.,
 ( 4, 2, 4 ),
 ( 0.3940582275541298363, 0.4471490536060385157, 0.5002398796579472506 ),
 .UNSPECIFIED. ) ;
#64036 = DIRECTION ( 'NONE',  ( 0.6507913734559641616, -0.7592566023653004592, 0.000000000000000000 ) ) ;
#64037 = CARTESIAN_POINT ( 'NONE',  ( 1.334805274328724867, -1.105471761691357191, 1.335692278477951689 ) ) ;
#64038 = CARTESIAN_POINT ( 'NONE',  ( 1.360316468749978469, 1.046875000341403128, -2.602085213965210642E-14 ) ) ;
#64039 = CARTESIAN_POINT ( 'NONE',  ( -11.44786932348540986, 12.29999999999998295, 3.303370173849762725 ) ) ;
#64040 = CARTESIAN_POINT ( 'NONE',  ( 1.469425047783163407, 1.914459939344328010, 1.024175319008380658 ) ) ;
#64041 = CARTESIAN_POINT ( 'NONE',  ( 2.483611571103708116, -0.6279893487078171965, 1.916353726171161620 ) ) ;
#64042 = CARTESIAN_POINT ( 'NONE',  ( 1.499999999999987121, 0.2854166673494805684, 0.8660254037844524744 ) ) ;
#64043 = CARTESIAN_POINT ( 'NONE',  ( 0.09454951164026764721, -0.4206464163897213893, -1.887090839307656864 ) ) ;
#64044 = CARTESIAN_POINT ( 'NONE',  ( -8.012344526598182026E-15, 13.54687500034139269, -1.575800808251669460 ) ) ;
#64045 = CARTESIAN_POINT ( 'NONE',  ( 2.391161334010579509, -2.127237363102509882, -0.6400520371602820280 ) ) ;
#64046 = ORIENTED_EDGE ( 'NONE', *, *, #109647, .T. ) ;
#64047 = CARTESIAN_POINT ( 'NONE',  ( 6.396834479292727416, -8.176568542494925040, 7.055228938193930155 ) ) ;
#64048 = DIRECTION ( 'NONE',  ( -7.387867266669436732E-31, 1.000000000000000000, 8.546850786086424434E-32 ) ) ;
#64050 = EDGE_CURVE ( 'NONE', #202127, #193425, #79432, .T. ) ;
#64049 = CARTESIAN_POINT ( 'NONE',  ( 8.914649696185335870, 10.35917838609310593, -1.199719254218446718 ) ) ;
#64051 = LINE ( 'NONE', #116050, #118488 ) ;
#64052 = SURFACE_SIDE_STYLE ('',( #197233 ) ) ;
#64053 = CARTESIAN_POINT ( 'NONE',  ( 5.056098682708163317, -1.255628792201430644, 1.205468413292756669 ) ) ;
#64054 = CARTESIAN_POINT ( 'NONE',  ( 3.121486724888074882, 0.2905151309811822569, -1.940125473959073421 ) ) ;
#64056 = CARTESIAN_POINT ( 'NONE',  ( -7.049876689426106680, 9.247942109129029475, -1.443375672974059665 ) ) ;
#64055 = CARTESIAN_POINT ( 'NONE',  ( 3.334415713957098681, 5.977569868670206787, -1.199719254218446718 ) ) ;
#64057 = DIRECTION ( 'NONE',  ( 0.000000000000000000, 0.000000000000000000, -1.000000000000000000 ) ) ;
#64058 = CARTESIAN_POINT ( 'NONE',  ( 5.132209903004834928, 1.169260703421838743, -1.936728657785217411 ) ) ;
#64059 = CARTESIAN_POINT ( 'NONE',  ( 1.363816705371086568, -0.5030291501087379435, 2.000271598109978566 ) ) ;
#64060 = CARTESIAN_POINT ( 'NONE',  ( -6.073162743917628781, 9.172774736957510555, -1.199719254218440723 ) ) ;
#64061 = CARTESIAN_POINT ( 'NONE',  ( 2.044175283654376951, 0.8654258166664110519, -2.090645895884978955 ) ) ;
#64062 = ORIENTED_EDGE ( 'NONE', *, *, #14091, .T. ) ;
#64064 = ADVANCED_FACE ( 'NONE', ( #176936 ), #125216, .T. ) ;
#64063 = CARTESIAN_POINT ( 'NONE',  ( -1.402160292154681736E-14, 1.868750000682816381, -1.732050807568863648 ) ) ;
#64065 = CARTESIAN_POINT ( 'NONE',  ( 2.969827553264007047, 0.9974664638083343693, 1.582205488144486250 ) ) ;
#64066 = CARTESIAN_POINT ( 'NONE',  ( 1.933800834616914877, -1.393042465158848886, -1.032573028607612464 ) ) ;
#64067 = CARTESIAN_POINT ( 'NONE',  ( 5.794512526436308875, 1.792401445336734733, -1.260760892635464980 ) ) ;
#64068 = CARTESIAN_POINT ( 'NONE',  ( 6.809642309899604840, -0.5188996100353564511, 2.257106211077652969 ) ) ;
#64069 = CARTESIAN_POINT ( 'NONE',  ( 4.311504812833309330, -0.3723461477018601973, 2.129241309423899775 ) ) ;
#64070 = CARTESIAN_POINT ( 'NONE',  ( 4.558499613049934673, -1.735246752265024561, -0.8719658702049468690 ) ) ;
#64071 = CARTESIAN_POINT ( 'NONE',  ( -9.480175724453545172, 12.08329098332774265, 1.599625672291281386 ) ) ;
#64072 = EDGE_CURVE ( 'NONE', #189856, #90864, #194541, .T. ) ;
#64073 = CARTESIAN_POINT ( 'NONE',  ( 1.436838838544733044, 7.449283400311756509, -4.203727439823553347 ) ) ;
#64074 = CARTESIAN_POINT ( 'NONE',  ( 1.031250000000000888, -0.7852924748300426083, -1.895863743164066584 ) ) ;
#64075 = CARTESIAN_POINT ( 'NONE',  ( 4.589221341884758942, 6.929947237659640713, 1.197292633685101748 ) ) ;
#64076 = DIRECTION ( 'NONE',  ( -1.561558963378126405E-12, 1.000000000000000000, -1.535693738323023938E-12 ) ) ;
#64077 = CARTESIAN_POINT ( 'NONE',  ( 3.553645660557675612, 6.199651466408984568, -1.082531754730549967 ) ) ;
#64078 = CARTESIAN_POINT ( 'NONE',  ( 1.360316468749997565, 2.744791667008062763, 0.7853790794158921340 ) ) ;
#64079 = CARTESIAN_POINT ( 'NONE',  ( 5.713517581197447015, 1.944070655204039433, 0.5350908816983344085 ) ) ;
#64080 = CARTESIAN_POINT ( 'NONE',  ( -9.317477881089553549, 11.89347683273641820, 1.599625672291281386 ) ) ;
#64081 = CARTESIAN_POINT ( 'NONE',  ( 8.620286740190458374, 8.951422706510690830, 1.040834085586084257E-14 ) ) ;
#64082 = CARTESIAN_POINT ( 'NONE',  ( -2.535011536075351124, 5.133042487381361596, -2.419999999999995044 ) ) ;
#64084 = CARTESIAN_POINT ( 'NONE',  ( -4.163763581353360443, 7.871824920094959488, -5.011504818508299590E-05 ) ) ;
#64083 = CARTESIAN_POINT ( 'NONE',  ( 3.756323439517950558, 0.6585720284536450420, 1.702948436616057881 ) ) ;
#64085 = CARTESIAN_POINT ( 'NONE',  ( 11.86239285000045740, 9.719999999999998863, -1.812080536912752837 ) ) ;
#64086 = ORIENTED_EDGE ( 'NONE', *, *, #172230, .F. ) ;
#64087 = CARTESIAN_POINT ( 'NONE',  ( -3.811250578772977349, 7.460559751961507224, -0.7216878364870458196 ) ) ;
#64088 = CIRCLE ( 'NONE', #185117, 1.250000000000000222 ) ;
#64089 = B_SPLINE_CURVE_WITH_KNOTS ( 'NONE', 3,
 ( #184918, #117872, #120011, #69027, #18145, #35476, #20289, #101554 ),
 .UNSPECIFIED., .F., .F.,
 ( 4, 2, 2, 4 ),
 ( 0.000000000000000000, 0.0002567066673176282847, 0.0005134133346352565694, 0.001026826669270514006 ),
 .UNSPECIFIED. ) ;
#64090 = DIRECTION ( 'NONE',  ( -0.03984146075563027578, 0.000000000000000000, 0.9992060137953822085 ) ) ;
#64091 = CARTESIAN_POINT ( 'NONE',  ( -8.350932551013499960, 11.83017284523606172, -1.199719254218446718 ) ) ;
#64092 = CARTESIAN_POINT ( 'NONE',  ( 0.1584709747761771925, 2.014675524564497167, 0.1441611394625528231 ) ) ;
#64093 = CARTESIAN_POINT ( 'NONE',  ( 1.049659257133638945, -1.915429643647760249, 0.9100379840868355608 ) ) ;
#64094 = ORIENTED_EDGE ( 'NONE', *, *, #81974, .T. ) ;
#64095 = CARTESIAN_POINT ( 'NONE',  ( -4.827585214917754719, 7.789877296449459365, -1.199719254218453823 ) ) ;
#64096 = CARTESIAN_POINT ( 'NONE',  ( 4.867540842506059562, 5.637551390133895168, -1.199719254218452047 ) ) ;
#64098 = CARTESIAN_POINT ( 'NONE',  ( 6.561407802241105536, 0.3549014609278942078, -2.029936712941163623 ) ) ;
#64097 = PRODUCT_RELATED_PRODUCT_CATEGORY ( 'part', '', ( #26328 ) ) ;
#64099 = CARTESIAN_POINT ( 'NONE',  ( 6.434220164165640021, -1.621181005584397372, -1.198863592720422977 ) ) ;
#64100 = VERTEX_POINT ( 'NONE', #190426 ) ;
#64101 = CARTESIAN_POINT ( 'NONE',  ( -5.148345644887285744, 7.029489223833707001, -1.599625672291256295 ) ) ;
#64102 = CARTESIAN_POINT ( 'NONE',  ( -10.15913717534155047, 10.74674821418697057, 0.7998128361456462443 ) ) ;
#64103 = CARTESIAN_POINT ( 'NONE',  ( 1.737500000000001155, -1.239583332377419689, 3.009438278150922130 ) ) ;
#64106 = ORIENTED_EDGE ( 'NONE', *, *, #128500, .F. ) ;
#64105 = CARTESIAN_POINT ( 'NONE',  ( -1.230761180058556281, 3.185133534840179248, -0.7749999999999918066 ) ) ;
#64104 = CARTESIAN_POINT ( 'NONE',  ( -3.820365424000704557, 7.679119771301277098, -0.7998128361456481317 ) ) ;
#64107 = CARTESIAN_POINT ( 'NONE',  ( 5.502223863662048409, 7.574938096329499437, 1.338028725624084148 ) ) ;
#64108 = CARTESIAN_POINT ( 'NONE',  ( 6.274767501101933043, -2.001204493855372579, 0.2439949869823473949 ) ) ;
#64109 = CARTESIAN_POINT ( 'NONE',  ( 4.892441406782115365, 1.528958278715689234, -1.025397978904031060 ) ) ;
#64110 = CARTESIAN_POINT ( 'NONE',  ( -0.02299388927988129522, 0.2517100516001030686, -1.946460665317284011 ) ) ;
#64111 = CARTESIAN_POINT ( 'NONE',  ( 3.246982502279437188, 0.5605648102574630753, 2.238460633888791573 ) ) ;
#64112 = CARTESIAN_POINT ( 'NONE',  ( 5.017399365509065845, 8.011327138806002779, -1.199719254218450271 ) ) ;
#64113 = CARTESIAN_POINT ( 'NONE',  ( 6.151685507011436904, 0.6340151041426717038, -2.066508600247290328 ) ) ;
#64114 = CARTESIAN_POINT ( 'NONE',  ( 5.770966940911189447, 9.884545197705074671, -0.7998128361456291469 ) ) ;
#64115 = CARTESIAN_POINT ( 'NONE',  ( 1.206472709818911637, 1.713414686832109179, 0.9141866466196489904 ) ) ;
#64116 = CARTESIAN_POINT ( 'NONE',  ( -3.761497552787613330, 6.475832013972435242, 1.199719254218464037 ) ) ;
#64117 = VERTEX_POINT ( 'NONE', #55113 ) ;
#64118 = CARTESIAN_POINT ( 'NONE',  ( 4.921405902946369260, 0.8734970824106644827, 2.126109943308290617 ) ) ;
#64119 = CARTESIAN_POINT ( 'NONE',  ( 7.320879633048903241E-15, 0.3750000006828252408, 1.224999999999981659 ) ) ;
#64121 = STYLED_ITEM ( 'NONE', ( #155445 ), #122337 ) ;
#64120 = CARTESIAN_POINT ( 'NONE',  ( -5.652823702255029836, 5.559658838911111900, -0.7998128361456362523 ) ) ;
#64122 = CARTESIAN_POINT ( 'NONE',  ( 4.399188623838041323, 1.502396186649012311, 1.114296746780506497 ) ) ;
#64125 = CARTESIAN_POINT ( 'NONE',  ( -6.798487682609798632, 6.896266815991691779, 0.7998128361456341429 ) ) ;
#64124 = CARTESIAN_POINT ( 'NONE',  ( -1.402160292154681736E-14, 0.4937500006828175469, 1.732050807568877637 ) ) ;
#64123 = CARTESIAN_POINT ( 'NONE',  ( 1.265713261412576562, 0.5522810963098608861, -1.830935845731461953 ) ) ;
#64126 = CARTESIAN_POINT ( 'NONE',  ( 3.229339687698820072, 0.05429069646168545316, 2.206380697113208722 ) ) ;
#64127 = CARTESIAN_POINT ( 'NONE',  ( 6.883263157960371359, 6.037760411968411844, 2.441088155713948549 ) ) ;
#64128 = CARTESIAN_POINT ( 'NONE',  ( 3.704402285031850539, 5.344888637335695414, -1.599625672291262513 ) ) ;
#64129 = CARTESIAN_POINT ( 'NONE',  ( 6.997416677984476863, 7.336276677169590421, 0.000000000000000000 ) ) ;
#64130 = CARTESIAN_POINT ( 'NONE',  ( -4.081167932913447594, 4.720116328942494555, -1.199719254218452047 ) ) ;
#64131 = CARTESIAN_POINT ( 'NONE',  ( -6.305950843687521790, 7.489935751457798219, 1.082531754730548412 ) ) ;
#64132 = CARTESIAN_POINT ( 'NONE',  ( 2.178924785135676334, -0.09298872875643586500, -1.969266502737290425 ) ) ;
#64133 = CARTESIAN_POINT ( 'NONE',  ( 0.7105614292102403473, -2.296071549169254489, 0.2300874200455073904 ) ) ;
#64134 = CARTESIAN_POINT ( 'NONE',  ( 1.715213470010600538, -1.680963409367957295, -1.011360081469035999 ) ) ;
#64135 = CARTESIAN_POINT ( 'NONE',  ( 5.524308913217452321, 1.011932313297726038, 1.797175476313887188 ) ) ;
#64136 = CARTESIAN_POINT ( 'NONE',  ( 4.148431816101584957, 6.823292304551739740, -1.082531754730548412 ) ) ;
#64137 = CARTESIAN_POINT ( 'NONE',  ( 6.378184920586140727, 6.405913593630768510, 0.000000000000000000 ) ) ;
#64138 = ORIENTED_EDGE ( 'NONE', *, *, #4855, .T. ) ;
#64139 = CARTESIAN_POINT ( 'NONE',  ( -8.611400122974211868, 13.19838391011195888, 1.040834085586084257E-14 ) ) ;
#64140 = DIRECTION ( 'NONE',  ( 0.000000000000000000, 0.000000000000000000, 1.000000000000000000 ) ) ;
#64141 = CARTESIAN_POINT ( 'NONE',  ( 3.999292125906911188, 4.728557570721922509, 1.082531754730560403 ) ) ;
#64142 = CARTESIAN_POINT ( 'NONE',  ( 1.358521007292138538, -2.171239805896512554, -0.002410242577662382712 ) ) ;
#64144 = CARTESIAN_POINT ( 'NONE',  ( 5.812015183962491172, 1.231757822100377320, -1.368757117762291253 ) ) ;
#64143 = CARTESIAN_POINT ( 'NONE',  ( -11.94655611907590220, 11.15200944546904083, 1.134828163062136852 ) ) ;
#64145 = EDGE_CURVE ( 'NONE', #76712, #136086, #118543, .T. ) ;
#64146 = CARTESIAN_POINT ( 'NONE',  ( 11.32145367647655476, 0.9706168436483538775, -3.678563289475825560 ) ) ;
#64147 = CARTESIAN_POINT ( 'NONE',  ( -2.324088772396477673E-16, -1.837499999999999245, -3.475000000000000089 ) ) ;
#64148 = CARTESIAN_POINT ( 'NONE',  ( 1.827212670807505379, -1.763035892288829620, 0.6254473451912796467 ) ) ;
#64149 = CARTESIAN_POINT ( 'NONE',  ( 6.257120919624137301, -1.850417449585840313, -1.117149918570578437 ) ) ;
#64150 = CARTESIAN_POINT ( 'NONE',  ( -6.007394967034264788, 6.077829431587280062, -0.6506939886842719734 ) ) ;
#64151 = CARTESIAN_POINT ( 'NONE',  ( -0.02264175331116376200, 2.864903628641465971, -2.577409799940860946 ) ) ;
#64152 = CARTESIAN_POINT ( 'NONE',  ( -1.402160292154681736E-14, -0.4281249996585808071, 1.575800808251672791 ) ) ;
#64153 = CARTESIAN_POINT ( 'NONE',  ( 2.156764536687346467, 0.4205103164258168769, 1.865301821287323136 ) ) ;
#64154 = CARTESIAN_POINT ( 'NONE',  ( 4.240886712856615226, -1.539575280908970223, 0.8727758839858139606 ) ) ;
#64155 = STYLED_ITEM ( 'NONE', ( #100694 ), #94059 ) ;
#64156 = CARTESIAN_POINT ( 'NONE',  ( 0.3637282827039616251, 0.5997036651611362679, -1.815894722023647656 ) ) ;
#64157 = CARTESIAN_POINT ( 'NONE',  ( -4.367698041896780126, 8.247398148854895084, 0.7998128361456481317 ) ) ;
#64159 = CARTESIAN_POINT ( 'NONE',  ( 5.044510182127093678, -1.384340171167136369, 1.324308159167127075 ) ) ;
#64158 = CARTESIAN_POINT ( 'NONE',  ( 1.850927770832884622, -3.228592521950734096, 2.725326427519580541 ) ) ;
#64160 = CARTESIAN_POINT ( 'NONE',  ( 6.496546994228061145, 1.947915994809066076, 0.2903317952503216559 ) ) ;
#64161 = CARTESIAN_POINT ( 'NONE',  ( -1.201851678989727383E-14, 4.837500000000018119, -1.732050807568863648 ) ) ;
#64162 = CARTESIAN_POINT ( 'NONE',  ( 2.197662576721173266, 1.936918166296027977, -0.8637449004969055544 ) ) ;
#64163 = CARTESIAN_POINT ( 'NONE',  ( 5.119927267529915227, -1.001353885182048931, -1.579878405157906673 ) ) ;
#64165 = ORIENTED_EDGE ( 'NONE', *, *, #210348, .T. ) ;
#64164 = CARTESIAN_POINT ( 'NONE',  ( 0.2229205655521030172, -0.09321834626660817358, 1.823428419517532983 ) ) ;
#64167 = CARTESIAN_POINT ( 'NONE',  ( 4.675188888464441028, 8.274035074156913083, -0.5495550137140058355 ) ) ;
#64166 = CARTESIAN_POINT ( 'NONE',  ( 4.793709216081707858, 1.633822259641436903, 1.483752339651790653 ) ) ;
#64168 = CARTESIAN_POINT ( 'NONE',  ( -1.364683531250014514, -1.219791666325248602, 0.7879004041258379498 ) ) ;
#64169 = CARTESIAN_POINT ( 'NONE',  ( 1.680209433476518521, -1.144093268944153641, -1.716113171863597797 ) ) ;
#64170 = CARTESIAN_POINT ( 'NONE',  ( 5.555090253297246150, 7.504024600312024340, 1.599625672291267398 ) ) ;
#64171 = CARTESIAN_POINT ( 'NONE',  ( -7.232384877886063990, 10.52520055992070525, -1.199719254218446718 ) ) ;
#64172 = PRESENTATION_STYLE_ASSIGNMENT (( #82535 ) ) ;
#64173 = CARTESIAN_POINT ( 'NONE',  ( 8.757677159423465696, 12.30470822171437284, 1.199719254218450271 ) ) ;
#64174 = CARTESIAN_POINT ( 'NONE',  ( 11.97302537858596061, 11.29875989808017245, -0.8111997896467566527 ) ) ;
#64176 = CARTESIAN_POINT ( 'NONE',  ( -0.001932293024938683355, -9.922538603026485049, -10.91970414279958135 ) ) ;
#64175 = AXIS2_PLACEMENT_3D ( 'NONE', #212318, #2112, #17309 ) ;
#64177 = CARTESIAN_POINT ( 'NONE',  ( 6.398695753475230674, -1.876852914212179035, -0.3660984893600614520 ) ) ;
#64178 = ORIENTED_EDGE ( 'NONE', *, *, #174535, .F. ) ;
#64179 = CARTESIAN_POINT ( 'NONE',  ( 4.176279081494421952, -1.061646348645030713, -1.777293304589353085 ) ) ;
#64180 = CARTESIAN_POINT ( 'NONE',  ( -1.500000000000011324, 5.379166666666692187, -0.8660254037844313801 ) ) ;
#64181 = CARTESIAN_POINT ( 'NONE',  ( 1.581558009922879204, 1.997867266642009643, -0.8257073301623578665 ) ) ;
#64182 = CARTESIAN_POINT ( 'NONE',  ( -5.591215426272092337, 7.404592667505576209, -1.242541652263975172 ) ) ;
#64183 = CARTESIAN_POINT ( 'NONE',  ( 2.069016002695713397, -1.559697248980717266, 1.283103002569847106 ) ) ;
#64184 = CARTESIAN_POINT ( 'NONE',  ( 4.219703575591028155, 7.337867620521338452, -0.8994424175318147530 ) ) ;
#64185 = ORIENTED_EDGE ( 'NONE', *, *, #51352, .T. ) ;
#64186 = CIRCLE ( 'NONE', #212890, 11.92000000000000171 ) ;
#64188 = CARTESIAN_POINT ( 'NONE',  ( 7.131225611108085616, 10.30321839872603462, 1.082531754730558626 ) ) ;
#64187 = CARTESIAN_POINT ( 'NONE',  ( -1.737500000000000266, -3.908333333333333215, -3.009438278150923907 ) ) ;
#64189 = CARTESIAN_POINT ( 'NONE',  ( 0.2868663046952837914, -5.229832900979505261, 10.99643026930483636 ) ) ;
#64190 = CARTESIAN_POINT ( 'NONE',  ( -4.380693030546956912, 6.204170850428461392, 1.443375672974065660 ) ) ;
#64191 = CARTESIAN_POINT ( 'NONE',  ( 0.5148617154710420918, 0.1531739628206352510, 2.010800830040265996 ) ) ;
#64192 = CARTESIAN_POINT ( 'NONE',  ( 4.634432875810733599, 0.3748786239917040186, 2.159109584303263940 ) ) ;
#64193 = CARTESIAN_POINT ( 'NONE',  ( -1.499999999999997780, 4.681250000682819490, 1.214306433183764966E-14 ) ) ;
#64194 = CARTESIAN_POINT ( 'NONE',  ( 4.447458312869024155, -1.746245811230531908, 0.7801085911468000900 ) ) ;
#64195 = CARTESIAN_POINT ( 'NONE',  ( -4.172158584703340445, 5.890604320285754980, -1.599625672291256295 ) ) ;
#64196 = CARTESIAN_POINT ( 'NONE',  ( 5.273758565591489145, 9.096542726591325234, -0.7216878364870267237 ) ) ;
#64198 = CARTESIAN_POINT ( 'NONE',  ( 2.530875249677287719, -1.674875632724934338, 1.122518345125958383 ) ) ;
#64197 = LINE ( 'NONE', #52203, #194398 ) ;
#64199 = CARTESIAN_POINT ( 'NONE',  ( -1.364683531250000748, 12.42187500034139980, 0.000000000000000000 ) ) ;
#64201 = CARTESIAN_POINT ( 'NONE',  ( -5.340986169140711226, 5.195848383611072485, 0.000000000000000000 ) ) ;
#64200 = CARTESIAN_POINT ( 'NONE',  ( 0.06458782335966220534, -1.490751515076127465, 1.741559778653593238 ) ) ;
#64202 = CARTESIAN_POINT ( 'NONE',  ( 4.963727558602625933, 1.705580761961351444, -0.2555711148431466517 ) ) ;
#64203 = CARTESIAN_POINT ( 'NONE',  ( -0.1394461523061195918, 0.2309855492786689335, -2.314897844796594661 ) ) ;
#64204 = CARTESIAN_POINT ( 'NONE',  ( 3.521367211247359741, 5.131347717920458962, -1.599625672291262513 ) ) ;
#64205 = CARTESIAN_POINT ( 'NONE',  ( 0.7499999999999902300, 3.847916667349481123, -1.299038105676658228 ) ) ;
#64206 = CARTESIAN_POINT ( 'NONE',  ( 9.117697077525853899, 4.000007913748542698, -7.299999999891275237 ) ) ;
#64207 = CARTESIAN_POINT ( 'NONE',  ( 0.2685318824256071601, -0.8817220219094963340, -1.871193708407721035 ) ) ;
#64208 = ORIENTED_EDGE ( 'NONE', *, *, #45988, .T. ) ;
#64209 = CARTESIAN_POINT ( 'NONE',  ( 5.268131585227527225, 1.809134041791292002, -0.09470131462574123138 ) ) ;
#64210 = ORIENTED_EDGE ( 'NONE', *, *, #175320, .F. ) ;
#64211 = CARTESIAN_POINT ( 'NONE',  ( 4.044074958626150185, 7.940114228364351767, 0.7998128361456271485 ) ) ;
#64212 = CARTESIAN_POINT ( 'NONE',  ( 3.834746474454188013E-15, 12.34375000068279959, 1.500000000000001554 ) ) ;
#64213 = EDGE_CURVE ( 'NONE', #197886, #168244, #184168, .T. ) ;
#64214 = CARTESIAN_POINT ( 'NONE',  ( 6.199861008060345569, 1.254605797456327831, 1.306922710324806225 ) ) ;
#64215 = CARTESIAN_POINT ( 'NONE',  ( 5.167065940139554669, 9.042344340222555843, -0.7216878364870458196 ) ) ;
#64216 = CARTESIAN_POINT ( 'NONE',  ( 7.720982897393566802, -5.907420853759296264, -7.834948825496929281 ) ) ;
#64217 = CARTESIAN_POINT ( 'NONE',  ( 2.783357461837578484, 1.550338952211056220, 1.549093164327268068 ) ) ;
#64218 = ORIENTED_EDGE ( 'NONE', *, *, #116473, .F. ) ;
#64219 = EDGE_CURVE ( 'NONE', #80737, #109006, #125524, .T. ) ;
#64221 = CARTESIAN_POINT ( 'NONE',  ( 8.269583629331492602, 11.73526576994040482, 1.199719254218450271 ) ) ;
#64220 = CARTESIAN_POINT ( 'NONE',  ( 6.812964112091245639, -1.437450002374938585, 1.181853997439401116 ) ) ;
#64222 = CARTESIAN_POINT ( 'NONE',  ( 3.901880894453650050, -0.9877729052028583201, -1.641157072818617779 ) ) ;
#64223 = PLANE ( 'NONE',  #119212 ) ;
#64224 = CARTESIAN_POINT ( 'NONE',  ( -1.364683531250000748, -0.7406249996585803075, 0.000000000000000000 ) ) ;
#64225 = CARTESIAN_POINT ( 'NONE',  ( 5.016153647376201619, 7.835634441038803466, 1.082531754730558626 ) ) ;
#64226 = CARTESIAN_POINT ( 'NONE',  ( -9.354762803749327560, 10.01623748057011376, 0.7216878364870438212 ) ) ;
#64227 = CARTESIAN_POINT ( 'NONE',  ( 1.692469166403000491, -2.151312531270420436, -0.2117842694067117448 ) ) ;
#64228 = CARTESIAN_POINT ( 'NONE',  ( -6.286140498591554326, 7.362860665558790707, 1.199719254218452047 ) ) ;
#64229 = CARTESIAN_POINT ( 'NONE',  ( 4.366607992053101128, 7.252070536440704096, -1.199719254218448494 ) ) ;
#64230 = CARTESIAN_POINT ( 'NONE',  ( 1.500715674837904468, 1.494693011815557471, -1.047886037138339166 ) ) ;
#64231 = CARTESIAN_POINT ( 'NONE',  ( -3.928111819657352566, 5.605883094398769195, 1.599625672291267398 ) ) ;
#64232 = CARTESIAN_POINT ( 'NONE',  ( 3.557459645987316232, 0.4443818804308434789, -1.770531947851671006 ) ) ;
#64233 = CARTESIAN_POINT ( 'NONE',  ( 13.00510994571362033, 6.785533762518828560, -2.157135041233587902 ) ) ;
#64234 = ORIENTED_EDGE ( 'NONE', *, *, #202630, .F. ) ;
#64235 = CARTESIAN_POINT ( 'NONE',  ( 4.387129405986627262, 0.09430581837475923712, 1.967405897498993195 ) ) ;
#64236 = ORIENTED_EDGE ( 'NONE', *, *, #12527, .F. ) ;
#64237 = CARTESIAN_POINT ( 'NONE',  ( 5.144061591681034606, 0.5672955765679200679, 1.857344180792292354 ) ) ;
#64238 = ORIENTED_EDGE ( 'NONE', *, *, #6325, .F. ) ;
#64239 = CARTESIAN_POINT ( 'NONE',  ( -5.562588163356775972, 9.711712967216715953, 0.7998128361456291469 ) ) ;
#64241 = CARTESIAN_POINT ( 'NONE',  ( 4.781546299372162245, 0.2051969522943071500, -2.110614603223801122 ) ) ;
#64240 = CARTESIAN_POINT ( 'NONE',  ( 5.830888582329017744, 8.960397891762626799, -1.199719254218452047 ) ) ;
#64242 = FACE_OUTER_BOUND ( 'NONE', #89560, .T. ) ;
#64243 = CARTESIAN_POINT ( 'NONE',  ( 3.141163725242692273, 0.04933110545866059571, 1.911816780882446221 ) ) ;
#64244 = CARTESIAN_POINT ( 'NONE',  ( 5.089368577813358385, 6.729159871965151751, -1.415889853396500975 ) ) ;
#64245 = CARTESIAN_POINT ( 'NONE',  ( -9.611540586923190688, -6.723650695528641918, 0.1589091098076336750 ) ) ;
#64246 = ORIENTED_EDGE ( 'NONE', *, *, #16428, .T. ) ;
#64247 = CARTESIAN_POINT ( 'NONE',  ( 5.903649544107831382, 5.852288987739402870, -0.7998128361456481317 ) ) ;
#64248 = CARTESIAN_POINT ( 'NONE',  ( 5.684946482831785275, 5.526859072925533134, -0.7998128361456231517 ) ) ;
#64249 = CARTESIAN_POINT ( 'NONE',  ( 3.668611300974702782, 0.7265845916090816203, 1.877559629772174166 ) ) ;
#64250 = CARTESIAN_POINT ( 'NONE',  ( -11.92619526913699879, 10.89999999999998259, 1.328859060402684644 ) ) ;
#64251 = CARTESIAN_POINT ( 'NONE',  ( 5.022008369909983116, -0.9795521577263366364, -1.540466923627185292 ) ) ;
#64252 = CARTESIAN_POINT ( 'NONE',  ( 0.6958625912084139831, -1.462932864358768459, -1.465259690088885014 ) ) ;
#64253 = CARTESIAN_POINT ( 'NONE',  ( -8.514157279702033065, 9.995900250149611921, -1.082531754730543971 ) ) ;
#64254 = CARTESIAN_POINT ( 'NONE',  ( -6.468510628652166972, 6.779004017053734898, -0.3101152288892006781 ) ) ;
#64255 = CARTESIAN_POINT ( 'NONE',  ( -0.6125000000000244693, 1.520833334016126415, -1.060881119635955327 ) ) ;
#64256 = CARTESIAN_POINT ( 'NONE',  ( 5.489076674590072535, 1.649195787720953987, -0.8828566466120502110 ) ) ;
#64257 = CARTESIAN_POINT ( 'NONE',  ( 7.461064606222022277, 7.598996883547496139, 1.040834085586084257E-14 ) ) ;
#64258 = CARTESIAN_POINT ( 'NONE',  ( -5.610376637956639101, 5.439860920571172542, 0.000000000000000000 ) ) ;
#64259 = EDGE_CURVE ( 'NONE', #37868, #54318, #204528, .T. ) ;
#64260 = CARTESIAN_POINT ( 'NONE',  ( -1.364683531250014514, 10.90104166700806942, -0.7879004041258335089 ) ) ;
#64261 = CARTESIAN_POINT ( 'NONE',  ( -5.870844209917351009, 6.808071985447069707, -1.199719254218446718 ) ) ;
#64263 = CARTESIAN_POINT ( 'NONE',  ( -7.944151662964566540, 8.232874793072271657, 0.000000000000000000 ) ) ;
#64262 = CARTESIAN_POINT ( 'NONE',  ( 7.769310276573696328, -5.221243112839685452, -7.769310276573722085 ) ) ;
#64264 = VECTOR ( 'NONE', #83782, 1000.000000000000000 ) ;
#64265 = CARTESIAN_POINT ( 'NONE',  ( -5.687809136132860210, 6.594531066031826150, -1.199719254218446718 ) ) ;
#64266 = CARTESIAN_POINT ( 'NONE',  ( 0.9364849611055334755, -1.153160888946737961, 1.719151461320179042 ) ) ;
#64267 = CARTESIAN_POINT ( 'NONE',  ( 2.003655485592752861, -2.052825532818176590, 0.5177380972332337183 ) ) ;
#64268 = VECTOR ( 'NONE', #118263, 1000.000000000000000 ) ;
#64269 = CARTESIAN_POINT ( 'NONE',  ( 9.915090410295563927, 10.46202698829998567, -0.7998128361456281477 ) ) ;
#64270 = CARTESIAN_POINT ( 'NONE',  ( 0.4792732452305690782, -0.1022114018467655538, 1.966944630885968603 ) ) ;
#64271 = CARTESIAN_POINT ( 'NONE',  ( 4.344452866495080556, 7.409550296852231099, 1.129427019999120985 ) ) ;
#64272 = CARTESIAN_POINT ( 'NONE',  ( 5.829642864196171281, 5.903597551091405826, 0.7216878364870317197 ) ) ;
#64274 = CARTESIAN_POINT ( 'NONE',  ( 3.660338285565247762, 7.214219066560688454, 1.040834085586084257E-14 ) ) ;
#64273 = CARTESIAN_POINT ( 'NONE',  ( 3.475000000000000533, -2.974999999999998312, 0.000000000000000000 ) ) ;
#64275 = CARTESIAN_POINT ( 'NONE',  ( 2.888958383575964017, 1.965592292480751402, -1.179159595035377261 ) ) ;
#64276 = CARTESIAN_POINT ( 'NONE',  ( 0.6975366375942676500, -0.6598540886826111951, 1.702458561391326342 ) ) ;
#64277 = CARTESIAN_POINT ( 'NONE',  ( 2.338023529656753752, -1.104205016203146705, -1.561194055274425452 ) ) ;
#64278 = VERTEX_POINT ( 'NONE', #136374 ) ;
#64280 = EDGE_CURVE ( 'NONE', #26907, #172406, #25237, .T. ) ;
#64279 = CARTESIAN_POINT ( 'NONE',  ( 5.924549939047454750, 9.855799328956630134, -0.7216878364870267237 ) ) ;
#64281 = CARTESIAN_POINT ( 'NONE',  ( 1.828386956846822509, -0.9528715280972717139, -1.773455306963005462 ) ) ;
#64282 = CARTESIAN_POINT ( 'NONE',  ( 0.4968289091572677396, 0.3296062100675010154, 1.933703066120408209 ) ) ;
#64283 = CARTESIAN_POINT ( 'NONE',  ( -10.15913717534155047, 10.74674821418697057, 0.7998128361456462443 ) ) ;
#64284 = CARTESIAN_POINT ( 'NONE',  ( -5.689618019229208734, 9.789638122409414223, 0.7998128361456481317 ) ) ;
#64285 = CARTESIAN_POINT ( 'NONE',  ( -4.351804119862249465, 7.060559992272473551, 1.082531754730560403 ) ) ;
#64287 = CARTESIAN_POINT ( 'NONE',  ( 2.307162891426073337, -0.3907249415124186553, 1.725993255813297989 ) ) ;
#64286 = CARTESIAN_POINT ( 'NONE',  ( 4.330081446525359645, 2.050255175485806269, 0.4079974934644239326 ) ) ;
#64288 = DIRECTION ( 'NONE',  ( 0.000000000000000000, -1.000000000000000000, 0.000000000000000000 ) ) ;
#64289 = CARTESIAN_POINT ( 'NONE',  ( 4.822401350889861327, 2.192639013963990635, 0.6684651760814497301 ) ) ;
#64290 = CARTESIAN_POINT ( 'NONE',  ( 4.523245630038312370, -1.073764689188366317, -1.369494959904279829 ) ) ;
#64291 = CARTESIAN_POINT ( 'NONE',  ( 8.432281472695482449, 11.92507992053172572, 1.199719254218450271 ) ) ;
#64292 = CARTESIAN_POINT ( 'NONE',  ( -15.75000000000000000, 10.19999999999999929, -1.400000000000001910 ) ) ;
#64293 = CARTESIAN_POINT ( 'NONE',  ( 4.428821037005469030, 0.8169072895964669678, 1.529287752448208471 ) ) ;
#64294 = CARTESIAN_POINT ( 'NONE',  ( 4.510331875626576448, 2.170777084992558059, -0.04906379945510477847 ) ) ;
#64295 = CARTESIAN_POINT ( 'NONE',  ( 2.998324526916512411, 6.649795714711241423, 0.000000000000000000 ) ) ;
#64296 = CARTESIAN_POINT ( 'NONE',  ( 6.262907710099243630, -0.1037740067610822270, -2.014008436551452785 ) ) ;
#64298 = AXIS2_PLACEMENT_3D ( 'NONE', #123365, #156852, #204485 ) ;
#64297 = CARTESIAN_POINT ( 'NONE',  ( 0.1874999572450692098, -1.451030237095527475, 1.451031289061128993 ) ) ;
#64299 = CARTESIAN_POINT ( 'NONE',  ( -1.500000000000011324, 4.952083334016150751, 0.8660254037844403729 ) ) ;
#64300 = CARTESIAN_POINT ( 'NONE',  ( 3.610301043878104021, -0.7796817500047310556, -1.761725471645478436 ) ) ;
#64301 = CARTESIAN_POINT ( 'NONE',  ( -1.500000000000008216, 9.531250000682799595, 3.469446951953614189E-15 ) ) ;
#64302 = CARTESIAN_POINT ( 'NONE',  ( 5.976846119194893170, -1.571437351877506439, 1.570356403719268101 ) ) ;
#64303 = ORIENTED_EDGE ( 'NONE', *, *, #181711, .F. ) ;
#64304 = CARTESIAN_POINT ( 'NONE',  ( 6.983263157960402090, 0.5904152146812295943, 1.899285251901380089 ) ) ;
#64305 = CARTESIAN_POINT ( 'NONE',  ( -1.499999999999997780, 3.650000000000021227, 1.214306433183764966E-14 ) ) ;
#64306 = CARTESIAN_POINT ( 'NONE',  ( 5.717788096661236885, 7.693838750903348789, 1.599625672291267398 ) ) ;
#64307 = DIRECTION ( 'NONE',  ( 0.000000000000000000, 1.000000000000000000, -8.546850786086437571E-32 ) ) ;
#64308 = CARTESIAN_POINT ( 'NONE',  ( 8.107412671292047790, 8.560995659369956101, 0.7216878364870458196 ) ) ;
#64309 = CARTESIAN_POINT ( 'NONE',  ( -10.60211293576223213, 11.47147930125185589, 1.040834085586084257E-14 ) ) ;
#64310 = MECHANICAL_DESIGN_GEOMETRIC_PRESENTATION_REPRESENTATION (  '', ( #36620 ), #202667 ) ;
#64311 = CARTESIAN_POINT ( 'NONE',  ( 2.905190055078214595, 6.611415174225076186, 0.7998128361456271485 ) ) ;
#64312 = CARTESIAN_POINT ( 'NONE',  ( -4.665414256878304577, 5.575976400180357118, -1.082531754730549967 ) ) ;
#64314 = CARTESIAN_POINT ( 'NONE',  ( 4.580570881008502404, 1.271380961112581032, -1.624167499240388057 ) ) ;
#64313 = CARTESIAN_POINT ( 'NONE',  ( 8.543609354905870035, 13.11929468069890525, 0.7998128361456462443 ) ) ;
#64315 = CARTESIAN_POINT ( 'NONE',  ( -3.958090780185743451, 6.705190779270287393, -1.199719254218452047 ) ) ;
#64317 = EDGE_CURVE ( 'NONE', #130628, #175863, #202393, .T. ) ;
#64316 = CARTESIAN_POINT ( 'NONE',  ( -1.001543065824772872E-14, 4.743750000682822154, 1.732050807568877637 ) ) ;
#64318 = CARTESIAN_POINT ( 'NONE',  ( 1.364683531249986537, -0.3864583329919166199, 0.7879004041258500513 ) ) ;
#64319 = CARTESIAN_POINT ( 'NONE',  ( 6.538356921592370696, 1.850225872366149105, 0.2742375073267953045 ) ) ;
#64320 = CARTESIAN_POINT ( 'NONE',  ( 5.801316117833412278, 1.158123311926442911, -1.290955512118051818 ) ) ;
#64321 = CARTESIAN_POINT ( 'NONE',  ( 4.581465296696157097, -0.8148697087324536792, 1.537882137665383064 ) ) ;
#64322 = CARTESIAN_POINT ( 'NONE',  ( 5.345992642490140057, 5.131412925860272090, 1.040834085586084257E-14 ) ) ;
#64323 = CARTESIAN_POINT ( 'NONE',  ( 3.579850016053500728, -1.128938594042153021, 1.995021623459404703 ) ) ;
#64324 = CARTESIAN_POINT ( 'NONE',  ( -1.201851678989727383E-14, 5.009375000341421469, -1.575800808251660134 ) ) ;
#64325 = CARTESIAN_POINT ( 'NONE',  ( 1.464538624043790316, 0.1369371521719800755, -1.836096087760468398 ) ) ;
#64326 = VECTOR ( 'NONE', #107516, 1000.000000000000000 ) ;
#64327 = ADVANCED_FACE ( 'NONE', ( #103867 ), #134653, .T. ) ;
#64328 = CARTESIAN_POINT ( 'NONE',  ( 3.998552357014331982, 7.829812261164016185, 1.248643980066187585E-14 ) ) ;
#64329 = CARTESIAN_POINT ( 'NONE',  ( 0.000000000000000000, 3.999999999999996447, 0.000000000000000000 ) ) ;
#64330 = CARTESIAN_POINT ( 'NONE',  ( 1.641335390984842491, -1.319735721761399638, -1.261605215524951085 ) ) ;
#64331 = CARTESIAN_POINT ( 'NONE',  ( 3.094375128876575065, -0.3905979561782264575, 1.978050703236901686 ) ) ;
#64332 = CARTESIAN_POINT ( 'NONE',  ( 0.9729166594223404019, -0.05710519180573449260, -2.190871861337650994 ) ) ;
#64333 = CARTESIAN_POINT ( 'NONE',  ( 10.13422073961230119, 13.69230262657890762, -7.310424441678322616 ) ) ;
#64334 = CARTESIAN_POINT ( 'NONE',  ( 4.331157237497373025, 0.1008371559532254685, 2.103664472247131378 ) ) ;
#64335 = CARTESIAN_POINT ( 'NONE',  ( -6.204827856548512877, 10.39071626594860476, -0.7998128361456291469 ) ) ;
#64336 = CARTESIAN_POINT ( 'NONE',  ( 9.077897083885416052, 13.43124749139993312, 9.116240771241983509 ) ) ;
#64337 = CARTESIAN_POINT ( 'NONE',  ( 1.803268859043684058, -1.750145871244257467, 1.105767233283899920 ) ) ;
#64338 = CARTESIAN_POINT ( 'NONE',  ( 6.003563092752934871, 5.898578451166879510, 0.7998128361456341429 ) ) ;
#64339 = CARTESIAN_POINT ( 'NONE',  ( 0.6801582343749726922, -0.9947916663252467373, 1.178068619123801675 ) ) ;
#64340 = CARTESIAN_POINT ( 'NONE',  ( 3.211701520346501582, 1.672844727185973657, 1.303009041611735030 ) ) ;
#64341 = CARTESIAN_POINT ( 'NONE',  ( 0.1703666795057276195, -1.259402025324443564, 1.457936571737717735 ) ) ;
#64342 = ORIENTED_EDGE ( 'NONE', *, *, #92035, .T. ) ;
#64343 = CARTESIAN_POINT ( 'NONE',  ( -4.471156797456668386, 8.438376373666578445, -0.7998128361456362523 ) ) ;
#64344 = CARTESIAN_POINT ( 'NONE',  ( 10.55910270694468345, 11.21337466772398095, 0.7998128361456462443 ) ) ;
#64345 = CARTESIAN_POINT ( 'NONE',  ( 6.848276988234151652, 7.162280372460873679, -0.7216878364870317197 ) ) ;
#64346 = CARTESIAN_POINT ( 'NONE',  ( -3.475000000000000533, -3.485416665710752593, -2.006292185433948827 ) ) ;
#64347 = CARTESIAN_POINT ( 'NONE',  ( -5.579343907223557331, 6.467988298970945849, 1.199719254218450271 ) ) ;
#64348 = CARTESIAN_POINT ( 'NONE',  ( 3.006122514718052585, -0.8146449015280079475, 1.848388696978587875 ) ) ;
#64349 = CARTESIAN_POINT ( 'NONE',  ( 1.132014994273435216, -1.335988328115779167, -1.627952913800976731 ) ) ;
#64350 = CARTESIAN_POINT ( 'NONE',  ( -6.119526231721793330, 8.232809585132461194, 1.599625672291263179 ) ) ;
#64351 = CARTESIAN_POINT ( 'NONE',  ( 8.727698198895078363, 11.20540053684285553, -1.599625672291257406 ) ) ;
#64352 = CARTESIAN_POINT ( 'NONE',  ( 5.242936282186112962, -0.2253732266207208457, -1.847139840844784775 ) ) ;
#64353 = CARTESIAN_POINT ( 'NONE',  ( 9.264299036839600987, 9.702770385934682551, -0.7998128361456281477 ) ) ;
#64354 = CARTESIAN_POINT ( 'NONE',  ( 4.891850447398502943, 4.899046648864193720, -0.7063863167381065900 ) ) ;
#64355 = CARTESIAN_POINT ( 'NONE',  ( -10.03267048443264109, 11.76749898900197877, 1.082531754730558626 ) ) ;
#64356 = CARTESIAN_POINT ( 'NONE',  ( -7.182068686937172153, 9.402166106225269715, 1.599625672291283607 ) ) ;
#64357 = CARTESIAN_POINT ( 'NONE',  ( 6.596562995212404523, -0.5471746534140635720, -1.986858483302299083 ) ) ;
#64359 = CARTESIAN_POINT ( 'NONE',  ( -4.038103646828244742, 7.764432012698684105, 0.5462726908427618655 ) ) ;
#64358 = CARTESIAN_POINT ( 'NONE',  ( -6.635789839245807897, 6.706452665400368218, 0.7998128361456341429 ) ) ;
#64360 = CARTESIAN_POINT ( 'NONE',  ( 1.364683531249986537, 0.9052083336747533959, -0.7879004041258239610 ) ) ;
#64361 = CARTESIAN_POINT ( 'NONE',  ( 2.495074604456462009, 1.680611355344446389, 0.4256512511701947554 ) ) ;
#64362 = CARTESIAN_POINT ( 'NONE',  ( 1.112787002727889885, -1.698604791339110465, 0.3779700589620417217 ) ) ;
#64364 = CARTESIAN_POINT ( 'NONE',  ( 8.134528978519385944, 8.592631351135175066, -0.7216878364870267237 ) ) ;
#64363 = CARTESIAN_POINT ( 'NONE',  ( 0.1832606990049808204, -2.239562280805599492, -0.5557475372391910140 ) ) ;
#64365 = CARTESIAN_POINT ( 'NONE',  ( -12.06809232949933275, 5.701620653239091396, -4.345812045493805620 ) ) ;
#64366 = CARTESIAN_POINT ( 'NONE',  ( 2.847006562934909280, -1.715207642559450685, 1.141990792043580338 ) ) ;
#64367 = CARTESIAN_POINT ( 'NONE',  ( 1.229842044428463010, -1.821462008879136896, -0.8645945014377558469 ) ) ;
#64368 = PLANE ( 'NONE',  #86113 ) ;
#64369 = CARTESIAN_POINT ( 'NONE',  ( -6.310394152517827315, 6.326824364217716656, 0.7998128361456281477 ) ) ;
#64370 = CARTESIAN_POINT ( 'NONE',  ( 1.569145635881466605, 0.1472162271188414695, -1.966034296795520664 ) ) ;
#64372 = CARTESIAN_POINT ( 'NONE',  ( -5.641601317062239218, 8.635599732330991429, -1.082531754730549967 ) ) ;
#64371 = CARTESIAN_POINT ( 'NONE',  ( 4.799029005866479736, -0.2398712174674077491, -1.897248949554980024 ) ) ;
#64373 = CARTESIAN_POINT ( 'NONE',  ( -7.078765599666485997, 7.431183752465250869, 0.000000000000000000 ) ) ;
#64374 = CARTESIAN_POINT ( 'NONE',  ( 6.363572996767764778, 8.517530811019446091, -1.599625672291283607 ) ) ;
#64375 = CARTESIAN_POINT ( 'NONE',  ( -7.944151662964566540, 8.232874793072271657, 0.000000000000000000 ) ) ;
#64376 = CARTESIAN_POINT ( 'NONE',  ( 0.4342474147537092044, -1.082315208530496786, -1.704999936850047249 ) ) ;
#64377 = DIRECTION ( 'NONE',  ( 3.330669073875478989E-16, -3.540251991789410786E-16, -1.000000000000000000 ) ) ;
#64378 = CARTESIAN_POINT ( 'NONE',  ( 4.981611329956401768, 2.155202031093924830, -0.8251229701327715826 ) ) ;
#64379 = CARTESIAN_POINT ( 'NONE',  ( 6.426224708462171087, 1.007414738832881351, 1.683299376423300853 ) ) ;
#64380 = CARTESIAN_POINT ( 'NONE',  ( 2.201936455694650796, 0.7555380192853027310, -1.810630540845730385 ) ) ;
#64381 = CARTESIAN_POINT ( 'NONE',  ( 9.748476143425788720, 11.33197590787365172, -1.199719254218440723 ) ) ;
#64382 = CARTESIAN_POINT ( 'NONE',  ( -9.404345922957899617, 14.49023946781299621, 7.453791880843827933 ) ) ;
#64383 = ORIENTED_EDGE ( 'NONE', *, *, #148663, .F. ) ;
#64384 = CARTESIAN_POINT ( 'NONE',  ( 0.3744018202470792978, -2.102136181054746089, -0.2526282858289953248 ) ) ;
#64386 = CARTESIAN_POINT ( 'NONE',  ( -6.320072162264675164, 10.52516795595079557, 0.7998128361456481317 ) ) ;
#64385 = CARTESIAN_POINT ( 'NONE',  ( -6.112028321662274166, 6.025121218227761588, 0.7998128361456341429 ) ) ;
#64387 = CARTESIAN_POINT ( 'NONE',  ( 0.8668490835730925381, 1.774987751554598869, -0.4888055736953432207 ) ) ;
#64388 = EDGE_LOOP ( 'NONE', ( #34779, #6125, #157274, #157193, #47730, #202466, #16259, #52868, #15308, #36838, #23667, #119973, #13567 ) ) ;
#64390 = VECTOR ( 'NONE', #47160, 1000.000000000000000 ) ;
#64389 = CARTESIAN_POINT ( 'NONE',  ( 3.836941170392699885, -2.090934008593826832, -0.5840943183372940828 ) ) ;
#64391 = CARTESIAN_POINT ( 'NONE',  ( 11.21998530456308174, 8.824241765716642760, 4.114255910918044989 ) ) ;
#64392 = CARTESIAN_POINT ( 'NONE',  ( 1.670341986359990205, 2.114562342887704283, -0.1611296783964668855 ) ) ;
#64393 = CARTESIAN_POINT ( 'NONE',  ( -1.201851678989727383E-14, 3.493750000682815493, 1.732050807568877637 ) ) ;
#64394 = CARTESIAN_POINT ( 'NONE',  ( 9.738834413317897898, 10.25639499182604730, 0.000000000000000000 ) ) ;
#64395 = CARTESIAN_POINT ( 'NONE',  ( 7.785697387528199762E-15, 0.4375000000000076605, -1.225000000000032951 ) ) ;
#64396 = CARTESIAN_POINT ( 'NONE',  ( 3.655589845848466801, 0.5043569952981543647, -1.997962123967106374 ) ) ;
#64398 = CARTESIAN_POINT ( 'NONE',  ( -0.09456490281532430042, -0.7861721075429689565, -1.663503389917226460 ) ) ;
#64397 = CARTESIAN_POINT ( 'NONE',  ( -9.450196763925152510, 10.98398329845622001, -1.199719254218441611 ) ) ;
#64399 = CARTESIAN_POINT ( 'NONE',  ( -1.364683531250012516, 3.030208333674755394, 0.7879004041258379498 ) ) ;
#64400 = DIRECTION ( 'NONE',  ( 0.8594130494132222742, -0.03761243564701257508, -0.5098965730253202100 ) ) ;
#64401 =( BOUNDED_SURFACE ( )  B_SPLINE_SURFACE ( 3, 2, ( 
 ( #96565, #194024, #111791 ),
 ( #126995, #208136, #94431 ),
 ( #177796, #80281, #93364 ),
 ( #9944, #142123, #10999 ),
 ( #146380, #213452, #15261 ),
 ( #134398, #166866, #1132 ) ),
 .UNSPECIFIED., .F., .F., .F. ) 
 B_SPLINE_SURFACE_WITH_KNOTS ( ( 4, 2, 4 ),
 ( 3, 3 ),
 ( 0.000000000000000000, 0.0003766365702389426712, 0.0007532731404778853423 ),
 ( 0.000000000000000000, 1.000000000000000000 ),
 .UNSPECIFIED. ) 
 GEOMETRIC_REPRESENTATION_ITEM ( )  RATIONAL_B_SPLINE_SURFACE ( (
 ( 1.000000000000000000, 0.7452309222762957264, 1.000000000000000000),
 ( 1.000000000000000000, 0.7451892422669569305, 1.000000000000000000),
 ( 1.000000000000000000, 0.7429606254241488683, 1.000000000000000000),
 ( 1.000000000000000000, 0.7311462761262982335, 1.000000000000000000),
 ( 1.000000000000000000, 0.7212257702793296588, 1.000000000000000000),
 ( 1.000000000000000000, 0.7071067811865551223, 1.000000000000000000) ) ) 
 REPRESENTATION_ITEM ( '' )  SURFACE ( )  );
#64402 = CARTESIAN_POINT ( 'NONE',  ( 1.445243771768980556, 4.136534814424732254, -0.4166150551214564679 ) ) ;
#64403 = CARTESIAN_POINT ( 'NONE',  ( 0.01274299142895937362, -0.9473294304004549193, -1.991142614049784099 ) ) ;
#64404 = CARTESIAN_POINT ( 'NONE',  ( 1.652057636490380732, 0.6571787646297929664, -2.164825341390004709 ) ) ;
#64405 = CARTESIAN_POINT ( 'NONE',  ( -8.839552966430002101, 12.29626697993494666, -1.082531754730543971 ) ) ;
#64406 = CARTESIAN_POINT ( 'NONE',  ( 1.687489445765244289, 1.732788098368071461, -0.5283295289823899399 ) ) ;
#64407 = CARTESIAN_POINT ( 'NONE',  ( 1.463933648137748733, -1.021544554152100437, 1.620407321708102533 ) ) ;
#64408 = CARTESIAN_POINT ( 'NONE',  ( 3.227070907399377298, -1.911900318415656441, -0.7948586591664741352 ) ) ;
#64409 = CARTESIAN_POINT ( 'NONE',  ( 0.6823417656249899377, 0.9052083336747520637, 1.181850606188755259 ) ) ;
#64410 = CARTESIAN_POINT ( 'NONE',  ( 1.481257693138532616, 1.822349276556498143, -0.7526048170787935643 ) ) ;
#64411 = CARTESIAN_POINT ( 'NONE',  ( 5.250583079984638246, 0.5609921762826737268, 1.843012466491249723 ) ) ;
#64413 = CARTESIAN_POINT ( 'NONE',  ( 5.694759483343039719, 7.307619849039811655, -1.219011658351103478 ) ) ;
#64412 = CARTESIAN_POINT ( 'NONE',  ( 0.7862591250819307431, 1.553807182831347777, 1.706378029075397151 ) ) ;
#64414 = CARTESIAN_POINT ( 'NONE',  ( 2.769781630715903997, -1.841240947949342788, 0.2698520108674675733 ) ) ;
#64415 = CARTESIAN_POINT ( 'NONE',  ( 0.6823417656249882723, 2.426041667008084435, -1.181850606188749264 ) ) ;
#64416 = PRESENTATION_LAYER_ASSIGNMENT (  '', '', ( #9054 ) ) ;
#64417 = CARTESIAN_POINT ( 'NONE',  ( 5.389153705970353592, 0.1484172631736270231, 2.057380146747369576 ) ) ;
#64418 = CARTESIAN_POINT ( 'NONE',  ( -4.577849422908604637, 8.492574760035358494, -0.7998128361456281477 ) ) ;
#64419 = CARTESIAN_POINT ( 'NONE',  ( 11.01135777277262306, 13.39999999999998259, 1.399999999999998579 ) ) ;
#64420 = CARTESIAN_POINT ( 'NONE',  ( 6.792010069470917344, -0.9048057162561828903, 1.900113248071538585 ) ) ;
#64421 = CIRCLE ( 'NONE', #119830, 11.09999999999999964 ) ;
#64422 = CARTESIAN_POINT ( 'NONE',  ( 0.6823417656249882723, 2.238541667008084435, -1.181850606188749264 ) ) ;
#64423 = CARTESIAN_POINT ( 'NONE',  ( 6.046190728430958394, 2.158797838069245412, 0.1127497994189360364 ) ) ;
#64424 = CARTESIAN_POINT ( 'NONE',  ( 0.4855842612344652975, -1.827229208960782447, -0.2260576252584786672 ) ) ;
#64425 = CARTESIAN_POINT ( 'NONE',  ( 5.602215259268515268, -0.9060462314097734726, 1.805096023085197121 ) ) ;
#64426 = CARTESIAN_POINT ( 'NONE',  ( -0.1399997263889819765, 0.7174702203470960660, -2.082715917450683740 ) ) ;
#64427 = CARTESIAN_POINT ( 'NONE',  ( -5.924549939491850381, 6.014322472269677533, 0.000000000000000000 ) ) ;
#64428 = EDGE_CURVE ( 'NONE', #112384, #13123, #108336, .T. ) ;
#64431 = CARTESIAN_POINT ( 'NONE',  ( 4.772106882330221289, 6.590544000850479200, -1.443375672974051449 ) ) ;
#64430 = CARTESIAN_POINT ( 'NONE',  ( -1.642778471874998480, -1.451041666188708446, 2.845375778867863303 ) ) ;
#64429 = CARTESIAN_POINT ( 'NONE',  ( -3.530618963777973907, 14.55202870305305929, -11.43095565162720284 ) ) ;
#64432 = CARTESIAN_POINT ( 'NONE',  ( -3.494969737272722643, 7.299491470118629088, -0.7998128361456481317 ) ) ;
#64433 = CARTESIAN_POINT ( 'NONE',  ( 4.135954056172497673, 2.015980767636461835, -0.05432360925018697717 ) ) ;
#64434 = CARTESIAN_POINT ( 'NONE',  ( -8.688077508258798431, 9.030511935923748013, -0.7998128361456291469 ) ) ;
#64436 = CARTESIAN_POINT ( 'NONE',  ( -10.99976946526262900, -5.360092950639650411, 0.08269815893113317828 ) ) ;
#64435 = CARTESIAN_POINT ( 'NONE',  ( -3.090368948911150770, 5.692848642783215674, 1.199719254218462483 ) ) ;
#64437 = CARTESIAN_POINT ( 'NONE',  ( -1.364683531250010295, 5.280208333674758059, 0.7879004041258379498 ) ) ;
#64439 = CARTESIAN_POINT ( 'NONE',  ( 1.364683531250000748, 10.00520833367473017, -0.7879004041258355073 ) ) ;
#64438 = CARTESIAN_POINT ( 'NONE',  ( 6.491117449447131982, 1.883434485765375310, -1.060826435891427666 ) ) ;
#64440 =( NAMED_UNIT ( * ) SI_UNIT ( $, .STERADIAN. ) SOLID_ANGLE_UNIT ( ) );
#64441 = CARTESIAN_POINT ( 'NONE',  ( -11.91788789707409713, 8.018247624035817367, 1.065403267925175701 ) ) ;
#64443 = CARTESIAN_POINT ( 'NONE',  ( 5.167592292328679449, 1.356312711205298172, 1.492245250866150785 ) ) ;
#64442 = CARTESIAN_POINT ( 'NONE',  ( -7.171900071504754060, 7.469564292951421436, -0.7216878364870267237 ) ) ;
#64444 = CARTESIAN_POINT ( 'NONE',  ( 1.364683531249986537, -1.073958332991911790, 0.7879004041258500513 ) ) ;
#64445 = CARTESIAN_POINT ( 'NONE',  ( 2.209205535023693212, -0.3792257637574465434, 1.682495413129220907 ) ) ;
#64446 = CARTESIAN_POINT ( 'NONE',  ( 4.573896719763862251, 6.429575154514868274, -1.599625672291273171 ) ) ;
#64448 = CARTESIAN_POINT ( 'NONE',  ( 6.801350335910821165, 7.963938809097990124, 1.199719254218452047 ) ) ;
#64447 = CARTESIAN_POINT ( 'NONE',  ( 6.643132081016111634, 9.733775946952057723, 1.082531754730558626 ) ) ;
#64449 = CARTESIAN_POINT ( 'NONE',  ( -11.90461463783674390, 8.893589831543669888, 1.538977259646465701 ) ) ;
#64450 = CARTESIAN_POINT ( 'NONE',  ( 6.696569769017397533, -0.4992639023812006638, -1.802638941973549569 ) ) ;
#64451 = CARTESIAN_POINT ( 'NONE',  ( 1.277990700441207661, 1.982931799766519676, -0.3463461644656241623 ) ) ;
#64452 = CARTESIAN_POINT ( 'NONE',  ( 0.000000000000000000, -5.223431457505076203, 0.000000000000000000 ) ) ;
#64453 = CARTESIAN_POINT ( 'NONE',  ( 2.749284697512776710, -1.835294401387000285, 1.225074929180599792 ) ) ;
#64454 =( BOUNDED_SURFACE ( )  B_SPLINE_SURFACE ( 3, 2, ( 
 ( #40850, #20293, #172982 ),
 ( #202229, #37625, #104779 ),
 ( #139414, #73311, #56016 ),
 ( #57082, #103705, #21343 ),
 ( #87453, #8320, #153520 ),
 ( #6166, #188136, #122170 ),
 ( #5089, #123247, #71164 ),
 ( #39767, #72235, #74405 ),
 ( #105872, #23495, #89601 ),
 ( #155652, #24561, #137281 ) ),
 .UNSPECIFIED., .F., .F., .T. ) 
 B_SPLINE_SURFACE_WITH_KNOTS ( ( 4, 2, 2, 2, 4 ),
 ( 3, 3 ),
 ( 0.000000000000000000, 0.0003762496586418675494, 0.0007524993172837350988, 0.001128748975925602648, 0.001504998634567470198 ),
 ( 0.000000000000000000, 1.000000000000000000 ),
 .UNSPECIFIED. ) 
 GEOMETRIC_REPRESENTATION_ITEM ( )  RATIONAL_B_SPLINE_SURFACE ( (
 ( 1.000000000000000000, 0.7127558927793078425, 1.000000000000000000),
 ( 1.000000000000000000, 0.7005070939717433776, 1.000000000000000000),
 ( 1.000000000000000000, 0.7091518804501668605, 1.000000000000000000),
 ( 1.000000000000000000, 0.7448155602382602325, 1.000000000000000000),
 ( 1.000000000000000000, 0.7694546621959588162, 1.000000000000000000),
 ( 1.000000000000000000, 0.7891761707070057419, 1.000000000000000000),
 ( 1.000000000000000000, 0.7831667280482919047, 1.000000000000000000),
 ( 1.000000000000000000, 0.7490304966219030192, 1.000000000000000000),
 ( 1.000000000000000000, 0.7236037604914373755, 1.000000000000000000),
 ( 1.000000000000000000, 0.7127552757490021040, 1.000000000000000000) ) ) 
 REPRESENTATION_ITEM ( '' )  SURFACE ( )  );
#64455 = CARTESIAN_POINT ( 'NONE',  ( 5.348546061712845301, -2.153812021095147688, -0.2729773376510102323 ) ) ;
#64456 = VERTEX_POINT ( 'NONE', #126889 ) ;
#64457 = CARTESIAN_POINT ( 'NONE',  ( 8.554831740098654436, 11.00372300158037042, 1.443375672974076540 ) ) ;
#64459 = CARTESIAN_POINT ( 'NONE',  ( 2.232046197884657968, 2.016035414700023676, 0.04665772616015140262 ) ) ;
#64458 = CARTESIAN_POINT ( 'NONE',  ( 2.332823983099761911, 1.383068002389773454, -1.607457772141835717 ) ) ;
#64461 = ORIENTED_EDGE ( 'NONE', *, *, #104706, .T. ) ;
#64460 = CARTESIAN_POINT ( 'NONE',  ( 1.828075118979434865, -0.8562131971674535880, -1.596496639089627578 ) ) ;
#64462 = CARTESIAN_POINT ( 'NONE',  ( 6.225128807330042591, 7.291680359087043151, -1.199719254218452047 ) ) ;
#64463 = EDGE_CURVE ( 'NONE', #205093, #188607, #179823, .T. ) ;
#64464 = VERTEX_POINT ( 'NONE', #132171 ) ;
#64465 = EDGE_CURVE ( 'NONE', #11760, #134155, #94389, .T. ) ;
#64466 = CARTESIAN_POINT ( 'NONE',  ( 4.964256800898067645, 8.943383367689749619, 0.7998128361456462443 ) ) ;
#64468 = CARTESIAN_POINT ( 'NONE',  ( 1.727608309356289729, 0.7294743340424666433, -1.771600730223451547 ) ) ;
#64467 = CARTESIAN_POINT ( 'NONE',  ( -3.581325132304157943, 7.329963087663487364, -0.7998128361456281477 ) ) ;
#64469 = CARTESIAN_POINT ( 'NONE',  ( -2.621219598810449636, 0.3864874759363081114, -0.1754412237054647494 ) ) ;
#64470 = CARTESIAN_POINT ( 'NONE',  ( 4.894543267554960053, 4.887125941896303338, -0.6895117023006970269 ) ) ;
#64471 = CARTESIAN_POINT ( 'NONE',  ( 5.138177029454836564, 7.977995053463880382, 1.082531754730558626 ) ) ;
#64472 = CARTESIAN_POINT ( 'NONE',  ( -1.364683531250012516, 0.5927083336747520637, 0.7879004041258379498 ) ) ;
#64473 = DIRECTION ( 'NONE',  ( 0.000000000000000000, 1.000000000000000000, 0.000000000000000000 ) ) ;
#64474 = CARTESIAN_POINT ( 'NONE',  ( -9.297140650669053485, 11.86975006391249643, 1.599625672291281386 ) ) ;
#64475 = CIRCLE ( 'NONE', #143990, 2.025000000000006573 ) ;
#64476 = CARTESIAN_POINT ( 'NONE',  ( 5.700121470611750674, -2.161883445634639411, -0.004416275431240455560 ) ) ;
#64477 = CARTESIAN_POINT ( 'NONE',  ( -6.021229618244897885, 7.157760988441397743, 1.082531754730548412 ) ) ;
#64478 = CARTESIAN_POINT ( 'NONE',  ( 5.397554552016216256, 7.390509292142662723, 1.443375672974065660 ) ) ;
#64479 = CARTESIAN_POINT ( 'NONE',  ( 1.740644586495963209, 1.216819214799185866, -1.736574482785017137 ) ) ;
#64480 = FACE_OUTER_BOUND ( 'NONE', #202315, .T. ) ;
#64481 = CARTESIAN_POINT ( 'NONE',  ( 2.829319923597766628, -1.840754522440336327, 0.7060794426061881568 ) ) ;
#64482 = CARTESIAN_POINT ( 'NONE',  ( 5.537344615273096515, -0.04053095765194079242, 1.912125305397804009 ) ) ;
#64483 = ORIENTED_EDGE ( 'NONE', *, *, #48444, .F. ) ;
#64484 = CARTESIAN_POINT ( 'NONE',  ( 0.7837444799244470683, -1.966470238067185905, 0.6478734989143407619 ) ) ;
#64485 = CARTESIAN_POINT ( 'NONE',  ( 1.324054681829215818, 1.871493247920783753, 0.5181311518769672331 ) ) ;
#64486 = ORIENTED_EDGE ( 'NONE', *, *, #155922, .T. ) ;
#64487 = LINE ( 'NONE', #179318, #116328 ) ;
#64489 = FACE_OUTER_BOUND ( 'NONE', #54928, .T. ) ;
#64488 = CARTESIAN_POINT ( 'NONE',  ( -6.672020991700860826, 7.917017590806697314, 1.082531754730549078 ) ) ;
#64491 = CARTESIAN_POINT ( 'NONE',  ( 7.793239369756836510, 7.986534107671458216, 0.7998128361456341429 ) ) ;
#64490 = CARTESIAN_POINT ( 'NONE',  ( 2.519574111291386309, -1.204466598365286023, -1.708601439550963663 ) ) ;
#64492 = CARTESIAN_POINT ( 'NONE',  ( 4.624739795592929248, 6.488892076315451618, -1.443375672974068769 ) ) ;
#64494 = ORIENTED_EDGE ( 'NONE', *, *, #85988, .F. ) ;
#64493 = CARTESIAN_POINT ( 'NONE',  ( 5.936178161767468708, -1.066166440211462563, -1.587280745415058814 ) ) ;
#64495 = CARTESIAN_POINT ( 'NONE',  ( 4.319099500008596770, 2.017107695584336557, 0.8957252843501888329 ) ) ;
#64496 = CARTESIAN_POINT ( 'NONE',  ( 3.452368941479638131, 2.206952907609287973, 0.002057427529567057434 ) ) ;
#64497 = CARTESIAN_POINT ( 'NONE',  ( -0.4694063952341946955, -6.893137084989842123, -10.98997987423602751 ) ) ;
#64498 = CARTESIAN_POINT ( 'NONE',  ( 2.104032245951466429, -0.8162354410432022256, 1.729450509904674416 ) ) ;
#64499 = CARTESIAN_POINT ( 'NONE',  ( 4.991989969715272757, 4.726297878971393196, 2.420000000000010587 ) ) ;
#64500 = CARTESIAN_POINT ( 'NONE',  ( 8.723781775389312543, 12.26516360700784958, -1.199719254218446718 ) ) ;
#64501 = CARTESIAN_POINT ( 'NONE',  ( 4.053231837324381637, 1.750648263899981849, -1.104974720517466480 ) ) ;
#64503 = CARTESIAN_POINT ( 'NONE',  ( 1.270647086845246188, -1.370953960119488668, 1.671340013135722558 ) ) ;
#64502 = CARTESIAN_POINT ( 'NONE',  ( -4.437596350374534815, 4.071617251725375475, -0.7998128361456221525 ) ) ;
#64504 = CARTESIAN_POINT ( 'NONE',  ( 3.843468145482428877, 0.7371271433744167600, -2.064019554291535830 ) ) ;
#64505 = CARTESIAN_POINT ( 'NONE',  ( -10.99970480893081870, -9.999999999999994671, -0.08058608058607828750 ) ) ;
#64506 = CARTESIAN_POINT ( 'NONE',  ( -4.783564408578051541, 15.44696316110051804, 10.96618341542351160 ) ) ;
#64507 = CARTESIAN_POINT ( 'NONE',  ( 5.682802662783380754, 6.658966523782627434, 1.199719254218452935 ) ) ;
#64508 = CARTESIAN_POINT ( 'NONE',  ( -1.364683531250000748, 14.92187500034139447, 0.000000000000000000 ) ) ;
#64509 = CARTESIAN_POINT ( 'NONE',  ( -5.340986169140711226, 5.195848383611072485, 0.000000000000000000 ) ) ;
#64510 = B_SPLINE_CURVE_WITH_KNOTS ( 'NONE', 3,
 ( #192739, #110515, #79002, #213256, #160261, #15052, #111579, #210056, #80070, #176515, #27044, #159190, #12922 ),
 .UNSPECIFIED., .F., .F.,
 ( 4, 3, 3, 3, 4 ),
 ( 0.000000000000000000, 6.251649345123172139E-05, 0.0001877439649095022150, 0.0003000588009599786999, 0.0004131109743063360296 ),
 .UNSPECIFIED. ) ;
#64511 = CARTESIAN_POINT ( 'NONE',  ( 6.609999999999995879, 0.01081285896096205283, 1.720159828161060833 ) ) ;
#64512 = CARTESIAN_POINT ( 'NONE',  ( -4.302014814237876017, 3.913438792899272212, 0.7998128361456341429 ) ) ;
#64513 = CARTESIAN_POINT ( 'NONE',  ( 4.610256228194366201, 2.069909489248497714, -0.04556564433023241323 ) ) ;
#64514 = CARTESIAN_POINT ( 'NONE',  ( 3.229043484313653511, 0.04796440165338172745, 1.926065231962639679 ) ) ;
#64515 = CARTESIAN_POINT ( 'NONE',  ( 5.642236307234618664, 0.8587400236706268508, 1.935442681345787452 ) ) ;
#64516 = CARTESIAN_POINT ( 'NONE',  ( 4.611744806942754238, 8.532119374741881757, -0.7998128361456231517 ) ) ;
#64517 = CARTESIAN_POINT ( 'NONE',  ( -1.364683531250010740, 5.488541667008087543, -0.7879004041258300672 ) ) ;
#64518 = CARTESIAN_POINT ( 'NONE',  ( 3.854321288642187149, -1.967005588004781202, -0.1009957709416451771 ) ) ;
#64519 = CARTESIAN_POINT ( 'NONE',  ( 5.964811824374402605, 0.1744345966951440507, -2.285673535861055594 ) ) ;
#64520 = CARTESIAN_POINT ( 'NONE',  ( 3.967279163243800255, 0.2216459979678051528, -1.812115712870238537 ) ) ;
#64521 = PRODUCT_DEFINITION_SHAPE ( 'NONE', 'NONE',  #173573 ) ;
#64522 = CARTESIAN_POINT ( 'NONE',  ( 6.129694847154206983, 8.244672969803623630, -1.443375672974078761 ) ) ;
#64524 = EDGE_CURVE ( 'NONE', #106638, #122127, #174015, .T. ) ;
#64523 = CARTESIAN_POINT ( 'NONE',  ( 3.497640442201256139, 7.024404915969360452, 1.040834085586084257E-14 ) ) ;
#64525 = CARTESIAN_POINT ( 'NONE',  ( -6.363572996767778100, 8.517530811019446091, -1.599625672291271394 ) ) ;
#64526 = CARTESIAN_POINT ( 'NONE',  ( 6.866278450678116485, 6.975356045404744521, 0.000000000000000000 ) ) ;
#64527 = ORIENTED_EDGE ( 'NONE', *, *, #181792, .T. ) ;
#64528 = CARTESIAN_POINT ( 'NONE',  ( 5.449481901252090310, -1.818156339564154012, 0.8647962134734816786 ) ) ;
#64529 = CARTESIAN_POINT ( 'NONE',  ( 0.1405533004714097089, -0.003749010675423158478, -2.279853246149381452 ) ) ;
#64530 = CARTESIAN_POINT ( 'NONE',  ( 4.592600981049492326, 1.923087700504518605, 0.3867253955378775476 ) ) ;
#64531 = CARTESIAN_POINT ( 'NONE',  ( -6.693975156845199059, 8.832723654451292816, 1.599625672291283607 ) ) ;
#64532 = STYLED_ITEM ( 'NONE', ( #196186 ), #18139 ) ;
#64533 = CARTESIAN_POINT ( 'NONE',  ( -3.249150368769345043, 6.942425863539538611, 0.7998128361456341429 ) ) ;
#64534 = FACE_OUTER_BOUND ( 'NONE', #198324, .T. ) ;
#64535 = CARTESIAN_POINT ( 'NONE',  ( -5.152980901645737077, 8.169505597632108262, -1.199719254218453823 ) ) ;
#64537 = CARTESIAN_POINT ( 'NONE',  ( 0.09234973940512071489, -0.4041859633337717694, -1.833079292876439670 ) ) ;
#64536 = CARTESIAN_POINT ( 'NONE',  ( 0.5211768519108473940, -1.983982463993728906, 0.6597393503331959730 ) ) ;
#64538 = CARTESIAN_POINT ( 'NONE',  ( 4.879410147971470657, 4.944948943068641967, -0.7687999843507594688 ) ) ;
#64539 = CARTESIAN_POINT ( 'NONE',  ( 6.474560584146490605, -0.09798994077552795889, -1.939597741719009338 ) ) ;
#64540 = CARTESIAN_POINT ( 'NONE',  ( -0.2102771530458094895, 2.860119660625429550, -2.691685224125789588 ) ) ;
#64541 = CARTESIAN_POINT ( 'NONE',  ( 0.6611568445531558202, 0.8558493542428649015, 1.515405575314775044 ) ) ;
#64542 = CARTESIAN_POINT ( 'NONE',  ( 5.286789834324991055, 8.255339675766103724, -1.199719254218452935 ) ) ;
#64543 = CARTESIAN_POINT ( 'NONE',  ( -11.41381675112453564, 13.53005666089993397, -3.704697986577182522 ) ) ;
#64544 = CARTESIAN_POINT ( 'NONE',  ( 1.523609404914439969, -0.9557964113278711871, -1.435619824176268100 ) ) ;
#64546 = EDGE_CURVE ( 'NONE', #194727, #77529, #177408, .T. ) ;
#64545 = CARTESIAN_POINT ( 'NONE',  ( 1.980270094416748394, -2.150034404144373301, -0.4237573071887782983 ) ) ;
#64547 = CARTESIAN_POINT ( 'NONE',  ( 4.389439674793148782, 1.972019932058775016, -0.9908447712502415072 ) ) ;
#64548 = CARTESIAN_POINT ( 'NONE',  ( 1.129994725911891207, 2.092989821048664822, -0.5768834896340956364 ) ) ;
#64549 = CARTESIAN_POINT ( 'NONE',  ( -11.84668730067608600, 10.90000000000000036, -1.400000000000001910 ) ) ;
#64550 = CARTESIAN_POINT ( 'NONE',  ( 2.571616345043222118, 1.500848072127154653, 1.493768111954131284 ) ) ;
#64551 = DIRECTION ( 'NONE',  ( 0.000000000000000000, 0.000000000000000000, 1.000000000000000000 ) ) ;
#64552 = ORIENTED_EDGE ( 'NONE', *, *, #122982, .T. ) ;
#64554 = CARTESIAN_POINT ( 'NONE',  ( -1.402160292154681736E-14, -0.4906249996585810846, -1.575800808251665908 ) ) ;
#64553 = CARTESIAN_POINT ( 'NONE',  ( 2.384684040179287479, -0.3955501765894597344, -2.257852644028814915 ) ) ;
#64555 = CARTESIAN_POINT ( 'NONE',  ( 2.846322183865124700, 5.408127416896231665, -1.199719254218446718 ) ) ;
#64556 = CARTESIAN_POINT ( 'NONE',  ( 4.059776932288224671, 6.823824623389866950, 1.199719254218462483 ) ) ;
#64557 = CARTESIAN_POINT ( 'NONE',  ( 4.600346979525781421, -1.047586700562872286, 1.958737397810013325 ) ) ;
#64558 = CARTESIAN_POINT ( 'NONE',  ( -7.429504990608782222, 8.730472579540773381, 1.082531754730549967 ) ) ;
#64559 = CIRCLE ( 'NONE', #133856, 1.500000000000005107 ) ;
#64560 = CARTESIAN_POINT ( 'NONE',  ( 3.985733972737593778, 6.633478153960411738, -1.082531754730548412 ) ) ;
#64561 = CARTESIAN_POINT ( 'NONE',  ( -7.673551755210395342, 8.054824590608001600, 1.040834085586084257E-14 ) ) ;
#64562 = CARTESIAN_POINT ( 'NONE',  ( 4.258669648468281110, 6.061810238003387141, 1.443375672974058777 ) ) ;
#64564 = ORIENTED_EDGE ( 'NONE', *, *, #59450, .F. ) ;
#64563 = AXIS2_PLACEMENT_3D ( 'NONE', #9157, #42760, #156493 ) ;
#64565 = CARTESIAN_POINT ( 'NONE',  ( 3.445935549842124690, -1.779626424299302956, -0.9480406757386842242 ) ) ;
#64567 = CARTESIAN_POINT ( 'NONE',  ( 2.272402725641348820, -0.9685827254542198617, -1.820965734949228310 ) ) ;
#64566 = CARTESIAN_POINT ( 'NONE',  ( 6.479907352327590964, 9.647310113435821677, 1.199719254218462483 ) ) ;
#64568 = CARTESIAN_POINT ( 'NONE',  ( -11.91294103507080315, 13.61460089956407060, 1.446263142085468134 ) ) ;
#64569 = CARTESIAN_POINT ( 'NONE',  ( 4.950135482320912494, 6.868520377498098739, -1.443375672974068769 ) ) ;
#64571 = EDGE_CURVE ( 'NONE', #137371, #201176, #14734, .T. ) ;
#64570 = CARTESIAN_POINT ( 'NONE',  ( -2.091679895156829610E-15, 2.562499999999987121, 1.224999999999973888 ) ) ;
#64572 = CARTESIAN_POINT ( 'NONE',  ( 0.6823417656249917140, 3.592708333674754506, 1.181850606188765695 ) ) ;
#64573 = CARTESIAN_POINT ( 'NONE',  ( 5.542994302928621053, -1.725804593724251657, -1.350479894307685447 ) ) ;
#64574 = CARTESIAN_POINT ( 'NONE',  ( 2.110000207431836472, 0.002812218110825881467, 2.016597019944998959 ) ) ;
#64575 = CARTESIAN_POINT ( 'NONE',  ( 0.5734669319550633748, -1.023298125840161887, 1.530493987491374330 ) ) ;
#64576 = ADVANCED_FACE ( 'NONE', ( #148392 ), #141631, .F. ) ;
#64577 = CARTESIAN_POINT ( 'NONE',  ( 7.365103760721646076, 9.615707025640515937, 1.599625672291281386 ) ) ;
#64578 = CARTESIAN_POINT ( 'NONE',  ( 5.579063851370913873, -0.04688903583028104782, -1.825137680102270288 ) ) ;
#64579 = CARTESIAN_POINT ( 'NONE',  ( 6.416638760586134360, -1.319225726833603840, -1.525046029381103452 ) ) ;
#64580 = CARTESIAN_POINT ( 'NONE',  ( -6.503107236049161521, 10.73870887536603291, 0.7998128361456481317 ) ) ;
#64582 = CARTESIAN_POINT ( 'NONE',  ( -5.119085517611572378, 8.129960982925583224, 1.199719254218452935 ) ) ;
#64581 = CARTESIAN_POINT ( 'NONE',  ( 5.049841537476964959, 0.7145653451936549994, -2.146778123354900814 ) ) ;
#64583 = CARTESIAN_POINT ( 'NONE',  ( 0.3992258182855871196, 1.749727718737997373, -1.171850562161039777 ) ) ;
#64584 = CARTESIAN_POINT ( 'NONE',  ( -7.259464905474441565, 7.434073576000447048, -0.7998128361456362523 ) ) ;
#64585 = CARTESIAN_POINT ( 'NONE',  ( 4.404779037558821386, 0.5491149005726041477, 1.996164414091922135 ) ) ;
#64586 = CARTESIAN_POINT ( 'NONE',  ( 7.865701674222579598, 12.32840238656838139, -0.7998128361456352531 ) ) ;
#64587 = FILL_AREA_STYLE_COLOUR ( '', #69412 ) ;
#64588 = DIRECTION ( 'NONE',  ( 9.156709124048522599E-23, -1.000000000000000000, -1.108177624080986558E-22 ) ) ;
#64589 = CARTESIAN_POINT ( 'NONE',  ( -9.338868881714763148, 9.789768538289042255, -0.7998128361456291469 ) ) ;
#64590 = UNCERTAINTY_MEASURE_WITH_UNIT (LENGTH_MEASURE( 1.000000000000000082E-05 ), #63100, 'distance_accuracy_value', 'NONE');
#64591 = FILL_AREA_STYLE ('',( #98177 ) ) ;
#64592 = CARTESIAN_POINT ( 'NONE',  ( 5.501576472095266901, 9.640532660744973725, -0.7998128361456481317 ) ) ;
#64593 = CARTESIAN_POINT ( 'NONE',  ( 4.513260471453858003, 7.001907027245110271, -1.160773635454902530 ) ) ;
#64594 = CARTESIAN_POINT ( 'NONE',  ( -9.869972641068651242, 11.57768483841065787, 1.082531754730558626 ) ) ;
#64595 = CARTESIAN_POINT ( 'NONE',  ( 2.232967058637932656, 1.447036570497368446, -1.685575845266892747 ) ) ;
#64596 = CARTESIAN_POINT ( 'NONE',  ( -5.611095471209320174, 7.639640364534566075, 1.599625672291263179 ) ) ;
#64597 = CARTESIAN_POINT ( 'NONE',  ( 7.135668919494039031, 7.219368582364847242, 1.040834085586084257E-14 ) ) ;
#64598 = CARTESIAN_POINT ( 'NONE',  ( 3.719154087244529894, -1.729071306366702698, -0.9269775827704658244 ) ) ;
#64599 = CARTESIAN_POINT ( 'NONE',  ( 6.148786358997489820, 7.132337826040578754, -1.199719254218446718 ) ) ;
#64600 = CARTESIAN_POINT ( 'NONE',  ( -4.327620591935813721, 7.230343590456815406, 0.9971501367836959062 ) ) ;
#64601 = CARTESIAN_POINT ( 'NONE',  ( 4.009460741339333723, 5.700790169694431420, -1.599625672291256295 ) ) ;
#64602 = CARTESIAN_POINT ( 'NONE',  ( -6.468648687495877958, 6.719380688266201496, 0.000000000000000000 ) ) ;
#64604 = CARTESIAN_POINT ( 'NONE',  ( -7.537970219518091319, 7.896646132300314314, -0.7216878364870278340 ) ) ;
#64603 = AXIS2_PLACEMENT_3D ( 'NONE', #24764, #169953, #187272 ) ;
#64605 = CARTESIAN_POINT ( 'NONE',  ( 2.795306286867365486, -0.1602278063087131110, -2.114629986603839829 ) ) ;
#64606 = CARTESIAN_POINT ( 'NONE',  ( -6.069210040772897052, 7.109775131437022999, -1.199719254218453823 ) ) ;
#64607 = CARTESIAN_POINT ( 'NONE',  ( 5.793401095800717826, -1.774274828963496198, 0.8374297333502839225 ) ) ;
#64608 = CARTESIAN_POINT ( 'NONE',  ( 4.030267251519312310, 1.158562084521784108, -1.824840551714689507 ) ) ;
#64609 = CARTESIAN_POINT ( 'NONE',  ( 3.227900028218867234, 1.797025815167479390, 0.4004103908350764573 ) ) ;
#64610 = B_SPLINE_CURVE_WITH_KNOTS ( 'NONE', 3,
 ( #144044, #142970, #61680, #10777, #174391, #158131 ),
 .UNSPECIFIED., .F., .F.,
 ( 4, 2, 4 ),
 ( 0.000000000000000000, 0.0003172254002810711735, 0.0006344508005621423471 ),
 .UNSPECIFIED. ) ;
#64611 = CARTESIAN_POINT ( 'NONE',  ( -4.137838753588869878, 7.456630865025390520, 0.6858938789830407723 ) ) ;
#64612 = CARTESIAN_POINT ( 'NONE',  ( -1.402160292154681736E-14, 0.3843750003414230232, 1.575800808251672791 ) ) ;
#64613 = CARTESIAN_POINT ( 'NONE',  ( 5.771390581163715616, 1.041905927170128754, 1.393825671036960534 ) ) ;
#64614 = CARTESIAN_POINT ( 'NONE',  ( 6.727182134110200273, 2.469373133786161745, 2.195552656936059055 ) ) ;
#64615 = CARTESIAN_POINT ( 'NONE',  ( 4.311129659465574804, 7.013106455143060636, -1.082531754730548412 ) ) ;
#64616 = AXIS2_PLACEMENT_3D ( 'NONE', #25718, #124389, #9478 ) ;
#64617 = CARTESIAN_POINT ( 'NONE',  ( 3.186554565756247737, -2.129457467500107004, -0.3711038070777841202 ) ) ;
#64618 = CARTESIAN_POINT ( 'NONE',  ( 4.886092203009785528, -0.1017338195800701617, 2.013677658187912556 ) ) ;
#64619 = CARTESIAN_POINT ( 'NONE',  ( -7.470179451005382276, 11.65903375957422128, 0.7216878364870458196 ) ) ;
#64620 = CARTESIAN_POINT ( 'NONE',  ( 2.377987466095924152, 1.329388817951412394, 1.704534938537699995 ) ) ;
#64621 = CARTESIAN_POINT ( 'NONE',  ( 2.548066081221173729, 1.970837879163300332, 0.05219120132928834616 ) ) ;
#64622 = CARTESIAN_POINT ( 'NONE',  ( 6.509000000000032315, 0.5738235599486035676, 2.152438501345500743 ) ) ;
#64623 = CARTESIAN_POINT ( 'NONE',  ( 4.001460698126992455, -1.936627024540507946, 0.1462448094460607750 ) ) ;
#64626 = EDGE_LOOP ( 'NONE', ( #60330, #145788, #34876, #187504 ) ) ;
#64625 = SURFACE_SIDE_STYLE ('',( #145914 ) ) ;
#64624 = CARTESIAN_POINT ( 'NONE',  ( -8.446366511189330240, 12.79791866312216442, 0.7216878364870317197 ) ) ;
#64627 = CARTESIAN_POINT ( 'NONE',  ( -6.071018923869249129, 10.30488218781460574, 0.7998128361456291469 ) ) ;
#64628 = CARTESIAN_POINT ( 'NONE',  ( 5.259637247458703868, 5.100941308315409373, 0.000000000000000000 ) ) ;
#64630 = ORIENTED_EDGE ( 'NONE', *, *, #213004, .T. ) ;
#64629 = CARTESIAN_POINT ( 'NONE',  ( -5.336015975430226099, 8.383046517047350932, -1.199719254218453823 ) ) ;
#64631 = CARTESIAN_POINT ( 'NONE',  ( -8.554831740098665094, 11.00372300158037042, 1.443375672974064550 ) ) ;
#64632 = CARTESIAN_POINT ( 'NONE',  ( 0.9036964725192305758, 1.805054822729842190, 1.269220749904229839 ) ) ;
#64633 = CARTESIAN_POINT ( 'NONE',  ( 3.285556943750000070, -2.384374999522043126, 0.000000000000000000 ) ) ;
#64634 = CARTESIAN_POINT ( 'NONE',  ( 5.348475771816908697, -1.946495798708135938, -0.2439133590248846462 ) ) ;
#64635 = CARTESIAN_POINT ( 'NONE',  ( 1.364683531249990311, 4.696875000341417916, 1.214306433183764966E-14 ) ) ;
#64636 = CARTESIAN_POINT ( 'NONE',  ( -1.402160292154681736E-14, 2.618750000682819490, -1.732050807568863648 ) ) ;
#64637 = CARTESIAN_POINT ( 'NONE',  ( 0.07479286986305369589, 1.387406912293275729, -2.112587013352088317 ) ) ;
#64638 = CARTESIAN_POINT ( 'NONE',  ( 3.890429890068654917, 1.554390554365025379, -0.9864425779082321988 ) ) ;
#64639 = ORIENTED_EDGE ( 'NONE', *, *, #85988, .T. ) ;
#64640 = CARTESIAN_POINT ( 'NONE',  ( -0.6125000000000210276, 1.354166667349498976, 1.060881119635887604 ) ) ;
#64641 = CARTESIAN_POINT ( 'NONE',  ( -7.832860060393135093, 10.16142270859057462, 1.599625672291295375 ) ) ;
#64642 = CARTESIAN_POINT ( 'NONE',  ( 7.649321060469609357, -7.336076765398686028, -6.992767129439135587 ) ) ;
#64643 = CARTESIAN_POINT ( 'NONE',  ( 4.939744792934912532, -2.012803497507458683, 0.6676120485993168874 ) ) ;
#64644 = CARTESIAN_POINT ( 'NONE',  ( 1.499999999999976907, 4.327083334016148086, -0.8660254037844394848 ) ) ;
#64645 = CARTESIAN_POINT ( 'NONE',  ( 6.094553744542824170, 7.069066442510145265, 1.199719254218462483 ) ) ;
#64646 = CARTESIAN_POINT ( 'NONE',  ( 0.1630570004950296636, -1.840724325608022127, -0.9269800520197747362 ) ) ;
#64649 = CARTESIAN_POINT ( 'NONE',  ( 3.808014051635350672, 1.299385917162833692, -1.304790556973287163 ) ) ;
#64648 = CARTESIAN_POINT ( 'NONE',  ( 0.2735837943700462627, -1.826300444241350851, 0.3570272679806109073 ) ) ;
#64647 = CARTESIAN_POINT ( 'NONE',  ( 4.990809943606266508, 6.915973915664348937, -1.443375672974068769 ) ) ;
#64650 = CARTESIAN_POINT ( 'NONE',  ( 6.611572464958476836, 10.86525164242692298, 0.7998128361456462443 ) ) ;
#64651 = CARTESIAN_POINT ( 'NONE',  ( -5.257529707049291900, 9.355811434857983500, 0.7998128361456291469 ) ) ;
#64652 = DIRECTION ( 'NONE',  ( 1.000000000000000000, -0.000000000000000000, -0.000000000000000000 ) ) ;
#64653 = ADVANCED_FACE ( 'NONE', ( #207775 ), #77032, .T. ) ;
#64654 = CARTESIAN_POINT ( 'NONE',  ( 3.422699507934781060, 1.400174360247144589, -1.705827624971032686 ) ) ;
#64655 = CARTESIAN_POINT ( 'NONE',  ( 4.517028817706403743, 2.066010597640522750, 0.9224273224419097250 ) ) ;
#64656 = CARTESIAN_POINT ( 'NONE',  ( -5.585596099150174965, 9.460353182409786399, -0.7216878364870207285 ) ) ;
#64657 = CARTESIAN_POINT ( 'NONE',  ( 6.011934222899888880, -0.6017306232493442320, 1.708898994858050191 ) ) ;
#64658 = CARTESIAN_POINT ( 'NONE',  ( 5.120295473698084798, 1.888475294726537079, 0.3208887515022250669 ) ) ;
#64659 = CARTESIAN_POINT ( 'NONE',  ( 6.227412191919261986, -1.760757567598171480, 0.6321290105378990498 ) ) ;
#64660 = CARTESIAN_POINT ( 'NONE',  ( 5.529708137783917898, 1.793509118821761561, -0.4966223845426844252 ) ) ;
#64661 = CARTESIAN_POINT ( 'NONE',  ( 0.4634916963840204351, 7.369626292149082936, 4.459501722865414131 ) ) ;
#64662 = CARTESIAN_POINT ( 'NONE',  ( 6.403183007056281184, 1.474056081383187555, 0.9792082336040304202 ) ) ;
#64663 = CARTESIAN_POINT ( 'NONE',  ( 1.428923106112218067, -1.700960256238340573, 1.082842518468102089 ) ) ;
#64665 = CARTESIAN_POINT ( 'NONE',  ( 2.930406704442231725, 1.169546373139153328, -1.751267329298618280 ) ) ;
#64664 = CARTESIAN_POINT ( 'NONE',  ( -10.50487009249003378, 11.15010328419353947, 0.7998128361456462443 ) ) ;
#64666 = CARTESIAN_POINT ( 'NONE',  ( 7.750457368506414646, 12.19395069656619945, 0.7998128361456462443 ) ) ;
#64668 = CARTESIAN_POINT ( 'NONE',  ( -8.154339323615371171, 11.60081407993821045, 1.199719254218453823 ) ) ;
#64667 = CARTESIAN_POINT ( 'NONE',  ( 2.000000000000011990, 2.453103989352373237E-14, 0.5999999999999970912 ) ) ;
#64669 = DIRECTION ( 'NONE',  ( -0.6507913734559658270, -0.7592566023652989049, 0.000000000000000000 ) ) ;
#64670 = CARTESIAN_POINT ( 'NONE',  ( 1.406516720256438369, -2.010457973371252205, -0.1935789593500591155 ) ) ;
#64671 = CARTESIAN_POINT ( 'NONE',  ( 1.364683531249988535, 3.905208333674751842, -0.7879004041258239610 ) ) ;
#64672 = CARTESIAN_POINT ( 'NONE',  ( 2.672928840188529609, 6.270167413528593414, 0.000000000000000000 ) ) ;
#64673 = CARTESIAN_POINT ( 'NONE',  ( 2.917419293707240069, -0.2150262876145451196, 2.150894318904146729 ) ) ;
#64674 = CARTESIAN_POINT ( 'NONE',  ( 6.620655732516643965, 2.083750514537034970, 2.135603474206409835 ) ) ;
#64675 = CARTESIAN_POINT ( 'NONE',  ( 5.110497557708379546, 4.926945003606695295, -0.7998128361456481317 ) ) ;
#64676 = CARTESIAN_POINT ( 'NONE',  ( 10.35806617071623315, 11.18675807536486566, 0.000000000000000000 ) ) ;
#64677 = CARTESIAN_POINT ( 'NONE',  ( 9.348761378620913831, 13.52553930298125273, -7.449808453853660417 ) ) ;
#64678 = CARTESIAN_POINT ( 'NONE',  ( -6.548225005720456515, 10.58342024007512983, 0.000000000000000000 ) ) ;
#64679 =( GEOMETRIC_REPRESENTATION_CONTEXT ( 3 ) GLOBAL_UNCERTAINTY_ASSIGNED_CONTEXT ( ( #166345 ) ) GLOBAL_UNIT_ASSIGNED_CONTEXT ( ( #173248, #75722, #76775 ) ) REPRESENTATION_CONTEXT ( 'NONE', 'WORKASPACE' ) );
#64680 = CARTESIAN_POINT ( 'NONE',  ( -1.402160292154681736E-14, 0.4468750003414233563, -1.575800808251665908 ) ) ;
#64681 = CARTESIAN_POINT ( 'NONE',  ( 0.4334776158547505864, -1.553986563932317377, -1.545601477622601472 ) ) ;
#64682 = CARTESIAN_POINT ( 'NONE',  ( 0.2555917649597919117, 7.163498069673003066, 2.096924645512464824 ) ) ;
#64683 = CARTESIAN_POINT ( 'NONE',  ( 3.116390431409152395, -1.113901014592171723, -1.969235179105185640 ) ) ;
#64684 = CARTESIAN_POINT ( 'NONE',  ( -8.453672473320708036, 9.821371626084353323, -1.199719254218446718 ) ) ;
#64685 = CARTESIAN_POINT ( 'NONE',  ( 4.364470425680367249, -1.957169923074707274, -0.4852690807995581057 ) ) ;
#64686 = CARTESIAN_POINT ( 'NONE',  ( -4.080641047588914994, 5.783833860318930320, -1.443375672974051449 ) ) ;
#64687 = CARTESIAN_POINT ( 'NONE',  ( -1.201851678989727383E-14, 3.259375000341420581, -1.575800808251660134 ) ) ;
#64688 = CARTESIAN_POINT ( 'NONE',  ( 4.794097012578165007, 8.135614534340449566, -0.8214339667521903809 ) ) ;
#64689 = CARTESIAN_POINT ( 'NONE',  ( -0.7500000000000179856, 10.54166666666667140, 1.299038105676658228 ) ) ;
#64690 = CARTESIAN_POINT ( 'NONE',  ( 6.021229618244865023, 10.03886863134542828, -0.7216878364870458196 ) ) ;
#64691 = CARTESIAN_POINT ( 'NONE',  ( 3.145496161269778046, 0.6404232447230692182, -1.649968755877039506 ) ) ;
#64692 = CARTESIAN_POINT ( 'NONE',  ( 10.26082332744404368, 10.86538205830655279, -0.7998128361456281477 ) ) ;
#64693 = CARTESIAN_POINT ( 'NONE',  ( 6.633804142636003931, -1.436369002829580133, -1.675418478561958802 ) ) ;
#64694 = CARTESIAN_POINT ( 'NONE',  ( 1.364683531249997417, 9.234375000341396245, 2.602085213965210642E-15 ) ) ;
#64695 = CARTESIAN_POINT ( 'NONE',  ( -6.069210040772897052, 7.109775131437022999, -1.199719254218453823 ) ) ;
#64696 = CARTESIAN_POINT ( 'NONE',  ( 4.903922820734956112, -1.081083478763317007, -1.701937824264573518 ) ) ;
#64697 = ORIENTED_EDGE ( 'NONE', *, *, #46655, .F. ) ;
#64698 = EDGE_CURVE ( 'NONE', #16236, #130050, #122120, .T. ) ;
#64699 = CARTESIAN_POINT ( 'NONE',  ( 2.729206520949432946, -1.746158693253213379, 0.6715030345267187784 ) ) ;
#64700 = ADVANCED_FACE ( 'NONE', ( #120218 ), #7445, .T. ) ;
#64701 = CARTESIAN_POINT ( 'NONE',  ( 3.151297481648129395, 1.777980080355131109, -1.060267355625019281 ) ) ;
#64702 = CARTESIAN_POINT ( 'NONE',  ( -10.98545788874447915, 11.25743779547922507, 1.592267205258850460 ) ) ;
#64703 = CARTESIAN_POINT ( 'NONE',  ( -0.5773502691896261751, -4.295408888568413630, -0.9999999999999991118 ) ) ;
#64704 = CARTESIAN_POINT ( 'NONE',  ( -4.041773898501059392, 7.631402218382003610, 0.4027767917945597742 ) ) ;
#64705 = CARTESIAN_POINT ( 'NONE',  ( -0.6823417656250212460, 4.363541667008085767, 1.181850606188767472 ) ) ;
#64706 = CARTESIAN_POINT ( 'NONE',  ( 1.054777118923880597, 0.3758132965740559883, 1.874924941132802836 ) ) ;
#64707 = CARTESIAN_POINT ( 'NONE',  ( 2.312880826517309085, -1.518475810973318074, 1.242258525517292433 ) ) ;
#64708 = CARTESIAN_POINT ( 'NONE',  ( 0.9134352171796226161, 0.5825640498151598567, 1.930122961472901633 ) ) ;
#64709 = EDGE_CURVE ( 'NONE', #30458, #30345, #112484, .T. ) ;
#64710 = CARTESIAN_POINT ( 'NONE',  ( -5.472651281771599763, 6.413789912602166687, 1.199719254218452935 ) ) ;
#64712 = FILL_AREA_STYLE ('',( #79894 ) ) ;
#64711 = CARTESIAN_POINT ( 'NONE',  ( 8.015895134177609904, 10.37496362800581018, 1.599625672291281386 ) ) ;
#64713 = CARTESIAN_POINT ( 'NONE',  ( 0.3505827959322353471, -1.506356567903786470, 1.108807183729618062 ) ) ;
#64714 = CARTESIAN_POINT ( 'NONE',  ( -1.364683531250012516, 2.780208333674754506, 0.7879004041258379498 ) ) ;
#64715 = CARTESIAN_POINT ( 'NONE',  ( 1.582290772395946066, 1.038639357175192401, 1.724485448976780688 ) ) ;
#64717 = CARTESIAN_POINT ( 'NONE',  ( 1.950926998395795753, -1.937146449801559367, -0.8548520037577662656 ) ) ;
#64716 = CARTESIAN_POINT ( 'NONE',  ( -6.887178846062116833, 9.058127958537705027, -1.443375672974059665 ) ) ;
#64718 = CYLINDRICAL_SURFACE ( 'NONE', #170163, 2.750000000000008438 ) ;
#64719 = CARTESIAN_POINT ( 'NONE',  ( 3.666520218671379450, -0.8364210039109070127, -1.894060025281426807 ) ) ;
#64720 = CARTESIAN_POINT ( 'NONE',  ( 3.237364818613055473, 6.998952398349030268, -1.734723475976807094E-15 ) ) ;
#64722 = CARTESIAN_POINT ( 'NONE',  ( 3.571683402196252910, 6.254382171615883834, 1.199719254218462483 ) ) ;
#64721 = CARTESIAN_POINT ( 'NONE',  ( 5.613254157830992241, -2.039858995719573631, 0.4571984828403846124 ) ) ;
#64724 = EDGE_LOOP ( 'NONE', ( #136945, #131415, #143734, #73139 ) ) ;
#64723 = CARTESIAN_POINT ( 'NONE',  ( 4.067279105520240634, 0.2236234833344897255, -1.811772463268163547 ) ) ;
#64725 = CARTESIAN_POINT ( 'NONE',  ( 10.21336978979620191, 10.81001959771741205, 0.7998128361456462443 ) ) ;
#64726 = SURFACE_STYLE_USAGE ( .BOTH. , #80986 ) ;
#64727 = CARTESIAN_POINT ( 'NONE',  ( 9.276887557417550667, 13.43425136904641271, -6.782796418722834453 ) ) ;
#64728 = CARTESIAN_POINT ( 'NONE',  ( 6.106501571484221458, -0.7887142981495840477, -2.061199855587454444 ) ) ;
#64729 = CARTESIAN_POINT ( 'NONE',  ( 1.364683531249996529, 10.27604166700806410, 0.7879004041258403923 ) ) ;
#64730 = EDGE_LOOP ( 'NONE', ( #26538, #37224, #14690, #196184 ) ) ;
#64731 = CARTESIAN_POINT ( 'NONE',  ( 4.934190575774549892, -1.026228162776990027, -1.613408319405706504 ) ) ;
#64733 = CARTESIAN_POINT ( 'NONE',  ( -10.08065090696061716, 11.71951313199760136, -1.199719254218441611 ) ) ;
#64732 = VECTOR ( 'NONE', #206860, 1000.000000000000000 ) ;
#64734 = CARTESIAN_POINT ( 'NONE',  ( 7.470706336329915764, 8.674577799595093452, -1.199719254218441611 ) ) ;
#64735 = B_SPLINE_CURVE_WITH_KNOTS ( 'NONE', 3,
 ( #39354, #124959, #55603, #27365 ),
 .UNSPECIFIED., .F., .F.,
 ( 4, 4 ),
 ( -1.944647862008625085E-06, 0.0001035599091551142457 ),
 .UNSPECIFIED. ) ;
#64736 = CARTESIAN_POINT ( 'NONE',  ( 0.6801582343749917881, 1.255208333674727506, 1.178068619123834759 ) ) ;
#64737 = CARTESIAN_POINT ( 'NONE',  ( 4.161989969270895706, 5.878740935614591656, 1.443375672974062551 ) ) ;
#64738 = CARTESIAN_POINT ( 'NONE',  ( -11.89197415570408900, 12.30000000000000249, 0.8055989572471813354 ) ) ;
#64739 = CARTESIAN_POINT ( 'NONE',  ( 7.610320672457040914, 14.45631463746157408, -9.278899351044326949 ) ) ;
#64740 = CARTESIAN_POINT ( 'NONE',  ( 0.5734669319550633748, -1.023298125840161887, 1.530493987491374330 ) ) ;
#64741 = ORIENTED_EDGE ( 'NONE', *, *, #84646, .F. ) ;
#64742 = STYLED_ITEM ( 'NONE', ( #206622 ), #149431 ) ;
#64743 = CARTESIAN_POINT ( 'NONE',  ( -5.725286006720766707, 9.901527117808042178, 0.7998128361456291469 ) ) ;
#64744 = CARTESIAN_POINT ( 'NONE',  ( 4.411305886619627081, -0.3218996851035611506, 1.842484647571709822 ) ) ;
#64745 = CARTESIAN_POINT ( 'NONE',  ( -0.02299388927987088688, 7.629137130509112907, -2.510989390717012881 ) ) ;
#64746 = CARTESIAN_POINT ( 'NONE',  ( -6.773376349083143566, -7.215597533173308875, -6.661184041420940005 ) ) ;
#64747 = CARTESIAN_POINT ( 'NONE',  ( 0.07926560469698022693, 14.48280592990708726, 11.99972816967717293 ) ) ;
#64748 = CARTESIAN_POINT ( 'NONE',  ( -6.236387472606145010, 9.259240570473746601, -1.082531754730538864 ) ) ;
#64749 = CARTESIAN_POINT ( 'NONE',  ( 3.960953433486789521, 7.772862772376584850, -0.7998128361456221525 ) ) ;
#64750 = CARTESIAN_POINT ( 'NONE',  ( 1.657020797538899748, 1.613050045282127032, -1.129676354644502556 ) ) ;
#64751 = CARTESIAN_POINT ( 'NONE',  ( 2.513296185832504470, -1.880429104915388727, 0.7283969491318904588 ) ) ;
#64752 = CARTESIAN_POINT ( 'NONE',  ( -7.458957065812611198, 11.85386701009007204, 0.7998128361456481317 ) ) ;
#64753 = CARTESIAN_POINT ( 'NONE',  ( 5.123001941117305336, 7.070197912760590064, 1.599625672291268286 ) ) ;
#64754 = CARTESIAN_POINT ( 'NONE',  ( 6.776323679500987573, -7.189645481333916344, 6.777910281175898000 ) ) ;
#64755 = VECTOR ( 'NONE', #178583, 1000.000000000000114 ) ;
#64756 = CARTESIAN_POINT ( 'NONE',  ( 2.871223686158608679, 2.080653275041044026, -0.6881803712485771163 ) ) ;
#64757 = DIRECTION ( 'NONE',  ( 0.000000000000000000, 1.000000000000000000, 0.000000000000000000 ) ) ;
#64758 = CARTESIAN_POINT ( 'NONE',  ( -8.971744963941075568, 11.49012176272984931, 1.599625672291269396 ) ) ;
#64759 = CARTESIAN_POINT ( 'NONE',  ( 0.000000000000000000, 4.000000000000003553, 0.000000000000000000 ) ) ;
#64760 = DIRECTION ( 'NONE',  ( 0.6483454320283789096, 0.000000000000000000, -0.7613463080411795314 ) ) ;
#64761 = CARTESIAN_POINT ( 'NONE',  ( -9.812680342707254866, 4.108039100808300148, -6.337802944732694677 ) ) ;
#64763 = ADVANCED_FACE ( 'NONE', ( #96193 ), #75163, .T. ) ;
#64762 = CARTESIAN_POINT ( 'NONE',  ( 9.108380270282433244, 9.520865158284665952, 1.040834085586084257E-14 ) ) ;
#64764 = CARTESIAN_POINT ( 'NONE',  ( -9.407146676474756219, 15.38250095867105216, 7.348982780145517424 ) ) ;
#64765 = CARTESIAN_POINT ( 'NONE',  ( 7.349928672384120176, 7.747540670635879145, 0.7216878364870267237 ) ) ;
#64766 = ORIENTED_EDGE ( 'NONE', *, *, #156259, .F. ) ;
#64768 = CARTESIAN_POINT ( 'NONE',  ( 2.051433223282957297, -1.797157160989469427, 0.9072355583341712437 ) ) ;
#64767 = CARTESIAN_POINT ( 'NONE',  ( 4.722110844128335039, 1.763445737372179689, 0.5296355584529164329 ) ) ;
#64769 = CARTESIAN_POINT ( 'NONE',  ( 3.040662745855776006, 2.183360198754655812, -0.7182390863737651010 ) ) ;
#64771 = CARTESIAN_POINT ( 'NONE',  ( 1.551354284286353247, 1.404667267363783667, 1.220738542487237677 ) ) ;
#64770 = CARTESIAN_POINT ( 'NONE',  ( 2.684151225825664788, 5.114964949229812596, -1.082531754730543083 ) ) ;
#64772 = CARTESIAN_POINT ( 'NONE',  ( -1.642778471875000035, -2.967708332855374831, -2.845375778867859751 ) ) ;
#64773 = DIRECTION ( 'NONE',  ( 0.7592566023652994600, 0.6507913734559651608, 0.000000000000000000 ) ) ;
#64774 = CARTESIAN_POINT ( 'NONE',  ( 5.519756697582541172, -0.4584384640409416289, 1.856529252577573619 ) ) ;
#64775 = CARTESIAN_POINT ( 'NONE',  ( -6.997979842947967377, 11.31606025008131233, -0.7998128361456291469 ) ) ;
#64776 = CARTESIAN_POINT ( 'NONE',  ( -6.129694847154220305, 8.244672969803623630, -1.443375672974066548 ) ) ;
#64778 = CARTESIAN_POINT ( 'NONE',  ( 3.274138816734498025, -1.115311402298941656, 1.501645261301733481 ) ) ;
#64777 = CARTESIAN_POINT ( 'NONE',  ( 4.634370609685579900, 0.3589238887658425248, 2.059545865661859931 ) ) ;
#64779 = CARTESIAN_POINT ( 'NONE',  ( 6.968527767744093993, 10.11340424813470662, 1.082531754730558626 ) ) ;
#64780 = CARTESIAN_POINT ( 'NONE',  ( 5.495603940606402560, -1.841430844871448258, 0.006098274996368944698 ) ) ;
#64781 = CARTESIAN_POINT ( 'NONE',  ( 3.846762897975340767, 5.510976019103107859, -1.599625672291256295 ) ) ;
#64782 = CARTESIAN_POINT ( 'NONE',  ( 0.008694310353105784428, -8.101927612791786970, -11.00038155431018438 ) ) ;
#64783 = CARTESIAN_POINT ( 'NONE',  ( 4.670341630432963242, -1.123608009272176078, 1.308792564452855522 ) ) ;
#64784 = CARTESIAN_POINT ( 'NONE',  ( -5.900823170445743671, 7.907379670318584353, 1.599625672291269396 ) ) ;
#64785 = FILL_AREA_STYLE_COLOUR ( '', #144243 ) ;
#64786 = CARTESIAN_POINT ( 'NONE',  ( -3.563261906135775536, 6.332667919118538435, -2.500000000000000444 ) ) ;
#64787 =( LENGTH_UNIT ( ) NAMED_UNIT ( * ) SI_UNIT ( .MILLI., .METRE. ) );
#64788 = CARTESIAN_POINT ( 'NONE',  ( 4.452125263715247527, -0.8365346480432279686, 2.003629037444945471 ) ) ;
#64789 = CARTESIAN_POINT ( 'NONE',  ( 3.439906511156048285, 0.8199118703316324863, -1.631291955839441865 ) ) ;
#64790 = CARTESIAN_POINT ( 'NONE',  ( 1.094497266827038962, 1.931770780797737341, 0.3408682529649207926 ) ) ;
#64791 = CARTESIAN_POINT ( 'NONE',  ( 5.436746213213202061, -1.667492067756784158, 1.304688015722222039 ) ) ;
#64793 = CARTESIAN_POINT ( 'NONE',  ( -1.201851678989727383E-14, 3.884375000341423689, 1.575800808251672791 ) ) ;
#64792 = CARTESIAN_POINT ( 'NONE',  ( 6.023008118121612853, -2.159854764417634687, 0.7684156934805678185 ) ) ;
#64794 = CARTESIAN_POINT ( 'NONE',  ( -4.218512253981382187, 3.978430757497701364, -0.5307291018261834914 ) ) ;
#64795 = CARTESIAN_POINT ( 'NONE',  ( 8.890396042259068210, 11.39521468743417998, -1.599625672291257406 ) ) ;
#64796 = CARTESIAN_POINT ( 'NONE',  ( 1.014494059972574691, -2.120667955011676487, 0.003750198165439199392 ) ) ;
#64797 = CARTESIAN_POINT ( 'NONE',  ( -5.287316719649550301, 5.270883715786984780, 0.7216878364870317197 ) ) ;
#64798 = CARTESIAN_POINT ( 'NONE',  ( 5.596450457127522427, 5.765155227950554462, 0.6767625585771692709 ) ) ;
#64799 = CARTESIAN_POINT ( 'NONE',  ( -3.253593677155282471, 6.739683690082376444, 1.040834085586084257E-14 ) ) ;
#64800 = CARTESIAN_POINT ( 'NONE',  ( 6.157114316693172995, 1.779627781583184909, -1.243356570269833483 ) ) ;
#64802 = CARTESIAN_POINT ( 'NONE',  ( -1.500000000000008216, 13.03125000068279604, 3.469446951953614189E-15 ) ) ;
#64801 = CARTESIAN_POINT ( 'NONE',  ( 6.983263157960363010, -0.003310164959547181717, 1.953544951557646403 ) ) ;
#64804 = ORIENTED_EDGE ( 'NONE', *, *, #71437, .F. ) ;
#64803 = CARTESIAN_POINT ( 'NONE',  ( 2.086886708931742884, -1.363721155840109889, 1.753348597404544185 ) ) ;
#64805 = CARTESIAN_POINT ( 'NONE',  ( 5.836564609439236939, 0.5826586670559866787, -1.930416874340326938 ) ) ;
#64807 = CARTESIAN_POINT ( 'NONE',  ( 5.102416002207363022, 2.056666295747246576, 0.1571963825151497518 ) ) ;
#64806 = CARTESIAN_POINT ( 'NONE',  ( 3.472859903394816872, 7.203420320602605287, -0.7998128361456291469 ) ) ;
#64809 = CARTESIAN_POINT ( 'NONE',  ( -3.474999999999998312, -3.120833333333331350, 2.006292185433951047 ) ) ;
#64808 = CARTESIAN_POINT ( 'NONE',  ( 6.201928923608456046, 6.200281597156833691, 0.7998128361456352531 ) ) ;
#64810 = CARTESIAN_POINT ( 'NONE',  ( 4.376249722160992839, 8.327651452488305850, 0.000000000000000000 ) ) ;
#64812 = EDGE_CURVE ( 'NONE', #109653, #116176, #110019, .T. ) ;
#64811 = CARTESIAN_POINT ( 'NONE',  ( 3.285556943750000514, -2.851041666188706802, 1.896917185911906500 ) ) ;
#64813 = CARTESIAN_POINT ( 'NONE',  ( 0.2333540202161220045, 5.723122673495201873, -2.639760918834464398 ) ) ;
#64814 = CARTESIAN_POINT ( 'NONE',  ( 5.284640796330934087, 1.621094592300664328, -0.8731043043393662550 ) ) ;
#64815 = CARTESIAN_POINT ( 'NONE',  ( 3.506755287428983792, 7.242964935309132990, 1.040834085586084257E-14 ) ) ;
#64816 = CARTESIAN_POINT ( 'NONE',  ( 1.799380453634431998, -0.5854278125525367305, 1.622511832645438190 ) ) ;
#64817 = CARTESIAN_POINT ( 'NONE',  ( 0.5500180045474002410, 0.9981291480291036855, 1.752136972055001296 ) ) ;
#64818 = CARTESIAN_POINT ( 'NONE',  ( 2.127932615311285414, 0.5078372532463393263, 2.241765503411979221 ) ) ;
#64819 = CARTESIAN_POINT ( 'NONE',  ( 1.364683531249988535, 4.217708333674752730, -0.7879004041258239610 ) ) ;
#64820 = CARTESIAN_POINT ( 'NONE',  ( 2.372703478119597698, -1.393307465234068898, 1.782356930206913770 ) ) ;
#64821 = CARTESIAN_POINT ( 'NONE',  ( 4.055375990838584244, -1.750834834141304697, -1.170193647660602965 ) ) ;
#64822 = CARTESIAN_POINT ( 'NONE',  ( -5.334207092333882017, 5.187939460669764635, 0.7998128361456281477 ) ) ;
#64823 = CARTESIAN_POINT ( 'NONE',  ( 3.004884002558502853, 1.492965937746863148, 0.9499605963744962578 ) ) ;
#64824 = CIRCLE ( 'NONE', #185879, 0.04999999999999969746 ) ;
#64826 = EDGE_CURVE ( 'NONE', #111346, #109058, #182762, .T. ) ;
#64825 = CARTESIAN_POINT ( 'NONE',  ( 7.122110765880372618, 7.203550736482235095, 0.7998128361456341429 ) ) ;
#64827 = CARTESIAN_POINT ( 'NONE',  ( 4.380693030546905398, 8.124909279031149012, 0.7216878364870247253 ) ) ;
#64828 = CARTESIAN_POINT ( 'NONE',  ( -5.412729640353771465, 7.337937218544611895, 1.599625672291269396 ) ) ;
#64829 = CARTESIAN_POINT ( 'NONE',  ( -1.201851678989727383E-14, 2.712500000000023892, 1.732050807568877637 ) ) ;
#64830 = CARTESIAN_POINT ( 'NONE',  ( 6.222901868277154414, 1.646860780578407013, -1.490944794436506626 ) ) ;
#64831 = CARTESIAN_POINT ( 'NONE',  ( 2.923975034273151419, 1.216836049711809586, -1.822369523680394066 ) ) ;
#64832 = CARTESIAN_POINT ( 'NONE',  ( -5.284980951228653190, 5.060232619388524533, 0.000000000000000000 ) ) ;
#64833 = CARTESIAN_POINT ( 'NONE',  ( 0.4138605925102775140, 8.005950907165225061, -1.999879544075613191 ) ) ;
#64834 = CARTESIAN_POINT ( 'NONE',  ( 0.4655551865852050608, -8.176568542494919711, 9.512045263456268884 ) ) ;
#64835 = CARTESIAN_POINT ( 'NONE',  ( -1.201851678989727383E-14, 2.946875000341419248, -1.575800808251660134 ) ) ;
#64836 = CARTESIAN_POINT ( 'NONE',  ( -1.364683531250000748, 9.609375000341396245, 0.000000000000000000 ) ) ;
#64837 = CARTESIAN_POINT ( 'NONE',  ( -4.528060117284246289, 6.305822774963486310, 1.443375672974064550 ) ) ;
#64838 = CARTESIAN_POINT ( 'NONE',  ( 5.976833544478475702, -1.498421880457675215, 1.500811427713820478 ) ) ;
#64839 = CARTESIAN_POINT ( 'NONE',  ( -5.397554552016258889, 7.390509292142662723, 1.443375672974058777 ) ) ;
#64840 = ORIENTED_EDGE ( 'NONE', *, *, #188521, .T. ) ;
#64842 = CARTESIAN_POINT ( 'NONE',  ( -4.365362273920257330, 6.116008624372161862, 1.443375672974064550 ) ) ;
#64841 = CARTESIAN_POINT ( 'NONE',  ( -5.641601317062248988, 6.714861303728305586, -1.082531754730549967 ) ) ;
#64843 = CARTESIAN_POINT ( 'NONE',  ( 5.035963992472171746, 7.962709526937818083, 1.199719254218462483 ) ) ;
#64844 = LINE ( 'NONE', #885, #142884 ) ;
#64845 = CARTESIAN_POINT ( 'NONE',  ( 0.000000000000000000, 8.920000000000001705, 0.000000000000000000 ) ) ;
#64846 = CARTESIAN_POINT ( 'NONE',  ( 0.4705731923490074631, 6.890484253938548243, -3.710072764477224005 ) ) ;
#64847 = CARTESIAN_POINT ( 'NONE',  ( 0.6823417656249899377, 4.738541667008086655, -1.181850606188754593 ) ) ;
#64848 = CARTESIAN_POINT ( 'NONE',  ( 2.717972786412402364, 1.639536828598524121, 0.5844088115515410076 ) ) ;
#64849 = DIRECTION ( 'NONE',  ( -0.6483454320283800199, 0.000000000000000000, 0.7613463080411787542 ) ) ;
#64850 = CARTESIAN_POINT ( 'NONE',  ( -9.499690612162398295, -9.919996481418280609, 0.07742489488620404869 ) ) ;
#64851 = CARTESIAN_POINT ( 'NONE',  ( 0.6823417656249882723, 0.4052083336747516751, 1.181850606188755259 ) ) ;
#64852 = CARTESIAN_POINT ( 'NONE',  ( -0.4000000000000171196, 3.248764396332275872, -0.4641653677812850320 ) ) ;
#64853 = CARTESIAN_POINT ( 'NONE',  ( 6.297764839082774735, -0.7330946318361495351, 2.033732118066629457 ) ) ;
#64854 = CARTESIAN_POINT ( 'NONE',  ( -8.611400122974211868, 13.19838391011195888, 1.040834085586084257E-14 ) ) ;
#64855 = EDGE_CURVE ( 'NONE', #148211, #99015, #197205, .T. ) ;
#64856 = CARTESIAN_POINT ( 'NONE',  ( -7.348156068482412095, 7.675196289425353591, 1.040834085586084257E-14 ) ) ;
#64857 = CIRCLE ( 'NONE', #40769, 2.000000000000000000 ) ;
#64858 = CARTESIAN_POINT ( 'NONE',  ( 5.840740251263128791, 0.4172088472891195554, 2.120894824392767664 ) ) ;
#64860 = ORIENTED_EDGE ( 'NONE', *, *, #173047, .T. ) ;
#64859 = CARTESIAN_POINT ( 'NONE',  ( -2.972980823146582186, 6.690504403638126263, 0.000000000000000000 ) ) ;
#64861 = CARTESIAN_POINT ( 'NONE',  ( -0.6823417656249969321, 4.217708333674755394, -1.181850606188749264 ) ) ;
#64862 = CARTESIAN_POINT ( 'NONE',  ( 5.641858350889248364, 0.8014469270729590589, -1.801278572543635326 ) ) ;
#64863 = CARTESIAN_POINT ( 'NONE',  ( 5.378194026956880869, -0.2521426391564468572, 1.715267145961799411 ) ) ;
#64865 = CARTESIAN_POINT ( 'NONE',  ( 1.857222401600963302, 0.3706860215506869172, -2.159823580554325329 ) ) ;
#64864 = CARTESIAN_POINT ( 'NONE',  ( 1.360316468749981800, -1.005208332991882614, 0.7853790794158560518 ) ) ;
#64866 = CARTESIAN_POINT ( 'NONE',  ( 2.977863636430440941, 2.191611430486348766, -0.7225824955255434334 ) ) ;
#64867 = CARTESIAN_POINT ( 'NONE',  ( 4.341127749375134570, -1.794969056106166860, 1.012190969697931209 ) ) ;
#64868 = CARTESIAN_POINT ( 'NONE',  ( 0.7791178172221034925, 1.303614328124411692, 1.439515497156283796 ) ) ;
#64869 = CARTESIAN_POINT ( 'NONE',  ( -5.707619481228817904, 8.642344580533519505, -1.082531754730537976 ) ) ;
#64870 = CARTESIAN_POINT ( 'NONE',  ( -4.679499295372141709, 5.488445928469455559, 1.199719254218452935 ) ) ;
#64871 = DIRECTION ( 'NONE',  ( -0.000000000000000000, -1.000000000000000000, -0.000000000000000000 ) ) ;
#64872 = CARTESIAN_POINT ( 'NONE',  ( 4.412424163657523657, -2.120181911468725033, -0.04909571644767100895 ) ) ;
#64873 = CARTESIAN_POINT ( 'NONE',  ( 2.848279904836711118, 0.2930702634792031747, -1.994869876753922799 ) ) ;
#64874 = CARTESIAN_POINT ( 'NONE',  ( -5.219525951136845698, 8.072902128759544382, -1.082531754730543971 ) ) ;
#64875 = CARTESIAN_POINT ( 'NONE',  ( 4.893709131440695081, 1.632385321431808256, 1.485157849447714451 ) ) ;
#64876 = CARTESIAN_POINT ( 'NONE',  ( -1.642778471874998480, -0.4885416661887104217, 2.845375778867863303 ) ) ;
#64877 = CARTESIAN_POINT ( 'NONE',  ( -1.787771076284315308, -3.046595646931173906, 3.001059505585823572 ) ) ;
#64878 = CARTESIAN_POINT ( 'NONE',  ( -11.84668730067608600, 12.69999999999998153, 1.399999999999998579 ) ) ;
#64879 = CARTESIAN_POINT ( 'NONE',  ( -5.887983850084758330, 10.09134126839936840, 0.7998128361456291469 ) ) ;
#64881 = CARTESIAN_POINT ( 'NONE',  ( -0.02919842301645384983, -0.002306431287177927551, -2.073770398395402115 ) ) ;
#64880 = CARTESIAN_POINT ( 'NONE',  ( -4.804518813248800591, 8.239360463340183571, 0.8967481634083998010 ) ) ;
#64882 = CARTESIAN_POINT ( 'NONE',  ( 1.445184293213131577, 8.696352241143832984, -2.614796098495196119 ) ) ;
#64883 = ORIENTED_EDGE ( 'NONE', *, *, #194704, .F. ) ;
#64884 = CARTESIAN_POINT ( 'NONE',  ( 4.276283029400809177, -1.188189442049456535, 1.683678490072185285 ) ) ;
#64885 = CARTESIAN_POINT ( 'NONE',  ( -1.360316468750052854, 2.661458333674782573, 0.7853790794158580502 ) ) ;
#64886 = CARTESIAN_POINT ( 'NONE',  ( 0.3199376857464626411, -8.148349307653466767, 9.520891725236003467 ) ) ;
#64887 = CARTESIAN_POINT ( 'NONE',  ( -4.283486466913726254, 7.084819080452935403, -1.199719254218452047 ) ) ;
#64888 = CARTESIAN_POINT ( 'NONE',  ( 3.651039828637154372, 0.2984016815541118417, 1.997388552288078545 ) ) ;
#64889 = CARTESIAN_POINT ( 'NONE',  ( -1.402160292154681736E-14, -0.2874999999999741096, 1.732050807568877637 ) ) ;
#64890 = CARTESIAN_POINT ( 'NONE',  ( 8.920901888111986366, 12.39117405523060889, 1.082531754730546636 ) ) ;
#64891 = CARTESIAN_POINT ( 'NONE',  ( 5.784525094524856748, 9.900363043587685041, 1.040834085586084257E-14 ) ) ;
#64892 = CARTESIAN_POINT ( 'NONE',  ( 3.502855024581267518, 1.625569291660882598, -1.266701038991333572 ) ) ;
#64893 = CARTESIAN_POINT ( 'NONE',  ( 0.000000000000000000, 8.500000000000000000, 0.000000000000000000 ) ) ;
#64894 = CARTESIAN_POINT ( 'NONE',  ( 6.030679399980265920, 5.930214142932100252, -0.7998128361456281477 ) ) ;
#64895 = CIRCLE ( 'NONE', #151339, 9.479622692290801567 ) ;
#64896 = CARTESIAN_POINT ( 'NONE',  ( -0.1411974294642332484, 2.879603353482541817, -2.388950311486548461 ) ) ;
#64897 = CARTESIAN_POINT ( 'NONE',  ( 1.816098422328410900, 1.717562825535594140, 0.6636192267199735317 ) ) ;
#64898 = CARTESIAN_POINT ( 'NONE',  ( 0.2941754776928190429, 1.714430973684363257, 1.544913290951188012 ) ) ;
#64899 = CARTESIAN_POINT ( 'NONE',  ( 7.361151057576892143, 7.552707420120024828, 0.7998128361456291469 ) ) ;
#64900 = CARTESIAN_POINT ( 'NONE',  ( 2.056162960589353883, 2.155939639820044107, -0.1567802445739118478 ) ) ;
#64901 = CARTESIAN_POINT ( 'NONE',  ( -2.792616454734997866, 6.201876930592042925, 0.7216878364870317197 ) ) ;
#64902 = CARTESIAN_POINT ( 'NONE',  ( 2.255092540634635156, 0.09411513195021348199, -2.014433103604281960 ) ) ;
#64903 = AXIS2_PLACEMENT_3D ( 'NONE', #101132, #37210, #169346 ) ;
#64904 = CARTESIAN_POINT ( 'NONE',  ( 0.07933194154488537597, -7.246166700194011767, -9.499668754385634628 ) ) ;
#64905 = CARTESIAN_POINT ( 'NONE',  ( 0.07479286986305370977, 0.004866263145587856019, -1.855573292446038414 ) ) ;
#64906 = CARTESIAN_POINT ( 'NONE',  ( 4.645367602377043603, -1.523440194387800650, -1.251305281888495102 ) ) ;
#64907 = CARTESIAN_POINT ( 'NONE',  ( 4.628138809701114020, 2.011451458044950069, 0.1435230606586651581 ) ) ;
#64909 = CARTESIAN_POINT ( 'NONE',  ( 10.53432216769390095, 11.39239007183880581, -0.7216878364870257245 ) ) ;
#64908 = CARTESIAN_POINT ( 'NONE',  ( 0.6823417656249917140, 3.842708333674754506, 1.181850606188765695 ) ) ;
#64911 = CARTESIAN_POINT ( 'NONE',  ( 5.830723289215218763, 2.029276893092274658, 0.5632808350878695247 ) ) ;
#64910 = CARTESIAN_POINT ( 'NONE',  ( -5.052384799386910430, 9.046199365926717917, 1.214306433183764966E-14 ) ) ;
#64912 = CARTESIAN_POINT ( 'NONE',  ( 6.074686117427479992, 1.393331124738606652, -1.531503843499823381 ) ) ;
#64913 = CARTESIAN_POINT ( 'NONE',  ( 4.645640190976921602, 8.571663989448405019, 1.040834085586084257E-14 ) ) ;
#64914 = CARTESIAN_POINT ( 'NONE',  ( -5.442708600882160574, 8.437244903416123876, -1.199719254218446718 ) ) ;
#64915 = CARTESIAN_POINT ( 'NONE',  ( 6.539320575229274901, 4.692178491785949923, 2.665866134390063813 ) ) ;
#64916 = CARTESIAN_POINT ( 'NONE',  ( 5.836196223694859242, -1.125476168604349514, -1.676936384952235404 ) ) ;
#64917 = CARTESIAN_POINT ( 'NONE',  ( 0.7499999999999885647, 0.7645833340161543035, 1.299038105676657340 ) ) ;
#64918 = CARTESIAN_POINT ( 'NONE',  ( 4.090657727307928759, -2.282307194306469444, -0.3406017358680757390 ) ) ;
#64919 = CARTESIAN_POINT ( 'NONE',  ( 1.569262014403381755, 1.817060349070098724, 0.9760215062899217919 ) ) ;
#64920 = CARTESIAN_POINT ( 'NONE',  ( 6.317736394288131052, 9.354147645769410602, 1.082531754730558626 ) ) ;
#64921 = CARTESIAN_POINT ( 'NONE',  ( 6.964048179274811012, 8.153752959689313684, 1.199719254218452047 ) ) ;
#64922 = CARTESIAN_POINT ( 'NONE',  ( 5.574337433874081427, 6.532423756721743580, -1.199719254218452047 ) ) ;
#64923 = EDGE_CURVE ( 'NONE', #84740, #116525, #48844, .T. ) ;
#64924 = CARTESIAN_POINT ( 'NONE',  ( -1.364683531250000748, 1.321875000341421469, 0.000000000000000000 ) ) ;
#64925 = CARTESIAN_POINT ( 'NONE',  ( 3.553118775233146120, 6.302999783484076524, -1.199719254218453823 ) ) ;
#64926 = CARTESIAN_POINT ( 'NONE',  ( 5.951666246274792016, 8.927065806420504401, 1.082531754730558626 ) ) ;
#64927 = CARTESIAN_POINT ( 'NONE',  ( 4.193918837840154623, -1.494357529231920889, -1.575321265833210305 ) ) ;
#64929 = CARTESIAN_POINT ( 'NONE',  ( 3.473999211503727036, -1.775402473473717935, -0.4878004006634574230 ) ) ;
#64928 = CARTESIAN_POINT ( 'NONE',  ( -4.446711195602245148, 7.171284913969171448, -1.082531754730549967 ) ) ;
#64930 = CARTESIAN_POINT ( 'NONE',  ( -1.364683531249997417, 5.259375000341425022, 1.214306433183764966E-14 ) ) ;
#64931 = CARTESIAN_POINT ( 'NONE',  ( 5.355090213057959403, 0.4282289882464126451, -2.149144931432686256 ) ) ;
#64932 = CARTESIAN_POINT ( 'NONE',  ( 7.679921558703143525, 14.45948583456419101, 9.166094091849766201 ) ) ;
#64933 = CARTESIAN_POINT ( 'NONE',  ( 5.752851848433533810, -1.787673638215280913, 1.386716842396797489 ) ) ;
#64934 = CARTESIAN_POINT ( 'NONE',  ( -4.747088307715054967, 7.009658186011790804, -1.421664413759090806 ) ) ;
#64935 = CARTESIAN_POINT ( 'NONE',  ( 4.601164721245145195, 8.482418317249249995, 0.1585857521721554253 ) ) ;
#64936 = CARTESIAN_POINT ( 'NONE',  ( -4.285785955251283141, 8.014184357852876417, 0.000000000000000000 ) ) ;
#64937 = CARTESIAN_POINT ( 'NONE',  ( 5.234856708652233515, 6.240325927249993576, 1.082531754730549078 ) ) ;
#64938 = CARTESIAN_POINT ( 'NONE',  ( 6.239478240350173621, -1.283343308616216705, -1.218829697195593642 ) ) ;
#64939 = CARTESIAN_POINT ( 'NONE',  ( 4.125643262898153196, -0.3419791877451948681, 1.983678759314363438 ) ) ;
#64940 = CARTESIAN_POINT ( 'NONE',  ( 6.435316467980822353, 10.65961964595298817, 1.040834085586084257E-14 ) ) ;
#64941 = CARTESIAN_POINT ( 'NONE',  ( 3.206187942969561000, -2.103625563118251218, 0.1016139793386036383 ) ) ;
#64942 = CARTESIAN_POINT ( 'NONE',  ( 1.880356884260485195, -0.5129869988758984922, -1.845544782535366801 ) ) ;
#64943 = CARTESIAN_POINT ( 'NONE',  ( 3.596117507753269660, 0.8876951776618343670, -1.758253228584506944 ) ) ;
#64944 = CARTESIAN_POINT ( 'NONE',  ( 0.2857447052702493662, -0.8859512962964136706, 1.647562673099879138 ) ) ;
#64945 = CARTESIAN_POINT ( 'NONE',  ( 0.9593383959572501229, 1.601786533887459507, 1.132500672181527168 ) ) ;
#64947 = ORIENTED_EDGE ( 'NONE', *, *, #89214, .F. ) ;
#64946 = CARTESIAN_POINT ( 'NONE',  ( 0.3516297456669579269, -1.353986107606550471, -1.350798769753497552 ) ) ;
#64948 = CARTESIAN_POINT ( 'NONE',  ( 4.311129659465574804, 7.013106455143060636, -1.082531754730548412 ) ) ;
#64949 = ADVANCED_FACE ( 'NONE', ( #129113 ), #132124, .T. ) ;
#64950 = CARTESIAN_POINT ( 'NONE',  ( 1.364683531249988757, 0.4468750003414206917, 0.000000000000000000 ) ) ;
#64951 = CARTESIAN_POINT ( 'NONE',  ( 11.89317557362571698, 11.26275843837589186, 1.599935658896036283 ) ) ;
#64952 = FACE_OUTER_BOUND ( 'NONE', #18600, .T. ) ;
#64953 = CARTESIAN_POINT ( 'NONE',  ( 6.860220180191213046, -2.069926439015772335, 0.04462916171246724545 ) ) ;
#64954 =( BOUNDED_CURVE ( )  B_SPLINE_CURVE ( 2, ( #66593, #51459, #134860, #18926, #117580, #184631, #135908, #199815, #53580 ),
 .UNSPECIFIED., .F., .T. ) 
 B_SPLINE_CURVE_WITH_KNOTS ( ( 3, 2, 2, 2, 3 ),
 ( 0.4218749999999998890, 0.4270833333333333148, 0.4375000000000000000, 0.4479166666666666852, 0.4531250000000002220 ),
 .UNSPECIFIED. ) 
 CURVE ( )  GEOMETRIC_REPRESENTATION_ITEM ( )  RATIONAL_B_SPLINE_CURVE ( ( 0.9330127018922192983, 0.9330127018922178550, 1.000000000000000000, 0.8660254037844387076, 1.000000000000000000, 0.8660254037844387076, 1.000000000000000000, 0.9330127018922165227, 0.9330127018922194093 ) ) 
 REPRESENTATION_ITEM ( '' )  );
#64955 = CARTESIAN_POINT ( 'NONE',  ( 0.6431357727456864515, -0.2518013131528433757, -2.054909676291870380 ) ) ;
#64956 = CARTESIAN_POINT ( 'NONE',  ( 1.499999999999987121, 2.004166666666684637, 0.8660254037844524744 ) ) ;
#64957 = CARTESIAN_POINT ( 'NONE',  ( 5.926885707468349196, 10.06645042535509660, 1.040834085586084257E-14 ) ) ;
#64958 = CARTESIAN_POINT ( 'NONE',  ( -7.503547950159405566, 10.84155747757291266, 1.199719254218453823 ) ) ;
#64959 = CARTESIAN_POINT ( 'NONE',  ( 4.854701522145073334, 7.821512988214679218, -1.199719254218450271 ) ) ;
#64960 = CARTESIAN_POINT ( 'NONE',  ( 5.514351353798126354, -2.120667953778174741, 0.0001357579994532010219 ) ) ;
#64961 = CARTESIAN_POINT ( 'NONE',  ( 3.464990776744291345, 6.200183785247111778, 1.199719254218452047 ) ) ;
#64962 = CARTESIAN_POINT ( 'NONE',  ( -0.6823417656250003738, 0.7177083336747519526, -1.181850606188749264 ) ) ;
#64963 = CARTESIAN_POINT ( 'NONE',  ( -0.7500000000000215383, 2.441666666666689078, 1.299038105676671107 ) ) ;
#64965 = CARTESIAN_POINT ( 'NONE',  ( 3.662674053986138656, 7.424870162959149589, 0.7998128361456321445 ) ) ;
#64964 = CARTESIAN_POINT ( 'NONE',  ( 6.215287892896892430, -1.681934637451238279, -1.009743211781432670 ) ) ;
#64966 = CARTESIAN_POINT ( 'NONE',  ( 4.798203786142633653, -1.844427309015805649, 0.8145022673629878085 ) ) ;
#64967 = CARTESIAN_POINT ( 'NONE',  ( 3.942530958389865781, -1.415603592240498365, 1.290913190617749118 ) ) ;
#64968 = EDGE_CURVE ( 'NONE', #76787, #155586, #184145, .T. ) ;
#64969 = CARTESIAN_POINT ( 'NONE',  ( 1.488088480104592826, -2.181432686776756835, -0.2102995727721947705 ) ) ;
#64970 = DIRECTION ( 'NONE',  ( 0.000000000000000000, 1.000000000000000000, 0.000000000000000000 ) ) ;
#64971 = CARTESIAN_POINT ( 'NONE',  ( 3.725732288501612199, -1.111853074318921664, -1.504101509696729400 ) ) ;
#64972 = CARTESIAN_POINT ( 'NONE',  ( -1.402160292154681736E-14, -0.7562499993171803991, 1.732050807568877637 ) ) ;
#64973 = CARTESIAN_POINT ( 'NONE',  ( -7.379715684540041565, 7.504089808251839244, 1.040834085586084257E-14 ) ) ;
#64975 = CARTESIAN_POINT ( 'NONE',  ( 5.255504845270437819, 2.040225721616812482, -0.5655070190290175658 ) ) ;
#64974 = CARTESIAN_POINT ( 'NONE',  ( -3.578989364327652467, 6.158942777482099729, 1.082531754730560403 ) ) ;
#64977 = CARTESIAN_POINT ( 'NONE',  ( -6.957269102468015554, 8.145844036748005834, 1.199719254218452047 ) ) ;
#64976 = CARTESIAN_POINT ( 'NONE',  ( 1.892240118738715005, -0.5608018070641508368, -2.014042591102585877 ) ) ;
#64979 = ORIENTED_EDGE ( 'NONE', *, *, #84492, .T. ) ;
#64978 = CARTESIAN_POINT ( 'NONE',  ( 0.6391468373067762387, -1.214715217071378195, -1.224744053251116904 ) ) ;
#64980 = CARTESIAN_POINT ( 'NONE',  ( 7.610204295972345712, 7.772993188256215547, 0.7998128361456341429 ) ) ;
#64981 = CYLINDRICAL_SURFACE ( 'NONE', #195866, 0.3999999999999997446 ) ;
#64982 = CARTESIAN_POINT ( 'NONE',  ( 0.001932266794894933271, -9.922538451904662438, 9.579662758527193844 ) ) ;
#64983 = CARTESIAN_POINT ( 'NONE',  ( -7.721398836998405457, -6.134628647623499909, -7.721398836998363713 ) ) ;
#64985 = CARTESIAN_POINT ( 'NONE',  ( 9.368320956918614328, 10.99242454023565507, 1.082531754730549967 ) ) ;
#64984 = CARTESIAN_POINT ( 'NONE',  ( 4.957477724091233995, 8.935474444748447098, -0.7998128361456281477 ) ) ;
#64986 = DIRECTION ( 'NONE',  ( 1.000000000000000000, 0.000000000000000000, -3.491481338843133355E-15 ) ) ;
#64988 = CARTESIAN_POINT ( 'NONE',  ( 2.051130129875160968, -1.617795175136220509, 0.8151331081446986371 ) ) ;
#64987 = CARTESIAN_POINT ( 'NONE',  ( 7.015418140428412386, 7.149352350113456822, 0.7998128361456331437 ) ) ;
#64989 = CARTESIAN_POINT ( 'NONE',  ( -6.856673000209188906, 9.022537805042615489, 1.599625672291283607 ) ) ;
#64990 = AXIS2_PLACEMENT_3D ( 'NONE', #113887, #47773, #30439 ) ;
#64991 = CARTESIAN_POINT ( 'NONE',  ( 3.680148631105580215, 6.380924938676771241, -1.199719254218446718 ) ) ;
#64992 = CARTESIAN_POINT ( 'NONE',  ( 5.387385936583818591, 7.378645907471495846, -1.599625672291283607 ) ) ;
#64993 = CARTESIAN_POINT ( 'NONE',  ( 6.639320575229252341, 2.457876053485750223, 2.280608551775892501 ) ) ;
#64994 = CARTESIAN_POINT ( 'NONE',  ( -2.788906526875773208E-15, 9.187500000000001776, -1.499999999999998446 ) ) ;
#64995 = CARTESIAN_POINT ( 'NONE',  ( 4.753338833179075351, 6.783512570024928579, 1.242321799368527380 ) ) ;
#64996 = CARTESIAN_POINT ( 'NONE',  ( 8.541273586929342798, 11.94827437051752206, -1.082531754730543083 ) ) ;
#64997 = VERTEX_POINT ( 'NONE', #133316 ) ;
#64998 = CARTESIAN_POINT ( 'NONE',  ( 2.699463648093935575, -1.376791127151571592, -1.252357159445316670 ) ) ;
#64999 = CARTESIAN_POINT ( 'NONE',  ( 0.3685665480608457667, -0.2352240095614567816, -1.901051784579368187 ) ) ;
#65000 = CARTESIAN_POINT ( 'NONE',  ( 6.405299695295086693, 1.602013123205116019, 1.069544239394400797 ) ) ;
#65001 = CARTESIAN_POINT ( 'NONE',  ( -1.500000000000039524, 8.500000000000000000, -10.89724735885167739 ) ) ;
#65002 = CARTESIAN_POINT ( 'NONE',  ( -1.919948509414037163, 8.999999999999998224, 0.7750000000000013545 ) ) ;
#65003 = CIRCLE ( 'NONE', #186070, 11.69999999999999041 ) ;
#65004 = CARTESIAN_POINT ( 'NONE',  ( 4.693755526227673336, 8.251780594207492214, -0.6034641085399840010 ) ) ;
#65005 =( NAMED_UNIT ( * ) PLANE_ANGLE_UNIT ( ) SI_UNIT ( $, .RADIAN. ) );
#65006 = CARTESIAN_POINT ( 'NONE',  ( -4.148431816101615155, 3.942184661647709198, 0.7216878364870317197 ) ) ;
#65007 = CARTESIAN_POINT ( 'NONE',  ( 7.944714827928039291, 11.25228915168265864, 1.082531754730557072 ) ) ;
#65008 = CARTESIAN_POINT ( 'NONE',  ( 4.575031941739591268, 1.798972412501558260, 0.8019633677735745758 ) ) ;
#65009 = CARTESIAN_POINT ( 'NONE',  ( 1.295735140135088281, 1.957893036122235531, -0.8148005001323217478 ) ) ;
#65010 = CARTESIAN_POINT ( 'NONE',  ( -6.905180308061733996, 6.950465202360470052, 0.7998128361456341429 ) ) ;
#65011 = CARTESIAN_POINT ( 'NONE',  ( 4.000000000000012434, 4.999999999999997335, -1.214306433183764966E-14 ) ) ;
#65012 = DIRECTION ( 'NONE',  ( 0.000000000000000000, 1.000000000000000000, 0.000000000000000000 ) ) ;
#65013 = CARTESIAN_POINT ( 'NONE',  ( 6.105464321129510097, -2.175355461714892691, 0.2646407054325700670 ) ) ;
#65014 = CARTESIAN_POINT ( 'NONE',  ( 0.1021010164683408550, 6.360493866598974755, -3.113991822131910059 ) ) ;
#65015 = CARTESIAN_POINT ( 'NONE',  ( 4.665017848976360071, -1.720483299173672043, -0.8667214970639931515 ) ) ;
#65016 = CARTESIAN_POINT ( 'NONE',  ( -6.073162743917628781, 9.172774736957510555, -1.199719254218440723 ) ) ;
#65017 = CARTESIAN_POINT ( 'NONE',  ( -1.225000000000040057, 2.333333334016199245, 0.7072540797572636206 ) ) ;
#65018 = CARTESIAN_POINT ( 'NONE',  ( 0.5927436934281339331, -2.190715567557582677, -0.2661302102612560505 ) ) ;
#65019 = CARTESIAN_POINT ( 'NONE',  ( 4.934241560730721510, 4.721313007132757811, 0.000000000000000000 ) ) ;
#65020 = EDGE_LOOP ( 'NONE', ( #196952, #101812, #128124, #179062, #40783 ) ) ;
#65021 = ORIENTED_EDGE ( 'NONE', *, *, #141919, .T. ) ;
#65022 = CARTESIAN_POINT ( 'NONE',  ( 6.526221542235329132, 1.009325857860805087, 1.690966299934024031 ) ) ;
#65023 = CARTESIAN_POINT ( 'NONE',  ( 0.9603743489425471402, -1.756279846738018291, -0.8291483874790173125 ) ) ;
#65024 = CARTESIAN_POINT ( 'NONE',  ( 0.2103132415818432799, -1.556605082263945228, -1.280954711483893727 ) ) ;
#65026 = CARTESIAN_POINT ( 'NONE',  ( 5.875803118876519626, -1.815897848738392106, 0.4062362408630160737 ) ) ;
#65025 = CARTESIAN_POINT ( 'NONE',  ( -6.903036488013351679, 8.082572653217566128, -1.199719254218452047 ) ) ;
#65027 = CARTESIAN_POINT ( 'NONE',  ( 6.062430963966053632, 7.101866208495718702, -1.199719254218452047 ) ) ;
#65028 = DIRECTION ( 'NONE',  ( 1.000000000000000000, -8.673617379884035472E-16, 0.000000000000000000 ) ) ;
#65029 = CARTESIAN_POINT ( 'NONE',  ( 1.499999999999819034, 7.361486028692880268, -4.203520246202064214 ) ) ;
#65030 = CARTESIAN_POINT ( 'NONE',  ( -4.934277840369690971, 7.844075682818238526, -1.199719254218452047 ) ) ;
#65031 = CARTESIAN_POINT ( 'NONE',  ( -5.413448473606448985, 9.537716662508005427, 0.000000000000000000 ) ) ;
#65032 = CARTESIAN_POINT ( 'NONE',  ( 0.9256184737543894370, -1.394389637717853514, -1.690728713229103342 ) ) ;
#65033 = CARTESIAN_POINT ( 'NONE',  ( 4.690757960648224589, 6.495636925554817864, 1.443375672974062551 ) ) ;
#65034 = DIRECTION ( 'NONE',  ( -0.7613463080411786432, 0.000000000000000000, -0.6483454320283800199 ) ) ;
#65035 = SURFACE_STYLE_USAGE ( .BOTH. , #162572 ) ;
#65036 = CARTESIAN_POINT ( 'NONE',  ( 1.523764310407935030, -1.012771255265769943, -1.518815351243132383 ) ) ;
#65037 = CARTESIAN_POINT ( 'NONE',  ( -4.620631424159025613, 4.285158171140619032, -0.7998128361456221525 ) ) ;
#65038 = TOROIDAL_SURFACE ( 'NONE', #148094, 1.914481421317583587, 0.05000000000000000278 ) ;
#65039 =( BOUNDED_SURFACE ( )  B_SPLINE_SURFACE ( 3, 2, ( 
 ( #183996, #164560, #83290 ),
 ( #99561, #133160, #81178 ),
 ( #51884, #114805, #31372 ),
 ( #132101, #150460, #181852 ) ),
 .UNSPECIFIED., .F., .F., .T. ) 
 B_SPLINE_SURFACE_WITH_KNOTS ( ( 4, 4 ),
 ( 3, 3 ),
 ( 0.0002170249176783571197, 0.0009435326495461319064 ),
 ( 0.000000000000000000, 1.000000000000000000 ),
 .UNSPECIFIED. ) 
 GEOMETRIC_REPRESENTATION_ITEM ( )  RATIONAL_B_SPLINE_SURFACE ( (
 ( 1.000000000000000000, 0.6273451206645743738, 1.000000000000000000),
 ( 1.000000000000000000, 0.6198154398457538239, 1.000000000000000000),
 ( 1.000000000000000000, 0.6183696555398915384, 1.000000000000000000),
 ( 1.000000000000000000, 0.6222646319068302345, 1.000000000000000000) ) ) 
 REPRESENTATION_ITEM ( '' )  SURFACE ( )  );
#65040 = CARTESIAN_POINT ( 'NONE',  ( -6.175853536056814086, 7.055546168579414079, -1.074032317439767903 ) ) ;
#65041 = CARTESIAN_POINT ( 'NONE',  ( 8.540746701604824409, 12.05162268759261224, -1.199719254218446718 ) ) ;
#65042 = CARTESIAN_POINT ( 'NONE',  ( 0.2406815423939384080, 0.3279693432677989184, 1.898232506199586167 ) ) ;
#65043 = CARTESIAN_POINT ( 'NONE',  ( 4.662917994108885189, 1.519075486231920458, -1.241376779329693258 ) ) ;
#65044 = CARTESIAN_POINT ( 'NONE',  ( -7.666245793523398078, 11.03137162816423356, 1.199719254218453823 ) ) ;
#65045 = CARTESIAN_POINT ( 'NONE',  ( 5.717788096661236885, 7.693838750903348789, 1.599625672291267398 ) ) ;
#65046 = CARTESIAN_POINT ( 'NONE',  ( 4.282901435897610298, 1.957309562236182021, -0.9860176978964061423 ) ) ;
#65047 = CARTESIAN_POINT ( 'NONE',  ( 6.609000000000015973, 2.967897204652647059, 2.453190122791535366 ) ) ;
#65049 = EDGE_CURVE ( 'NONE', #36461, #145929, #86657, .T. ) ;
#65048 = CARTESIAN_POINT ( 'NONE',  ( 3.414952709633051864, -1.570776679111930640, 1.348709175982481856 ) ) ;
#65051 = CARTESIAN_POINT ( 'NONE',  ( -1.364683531250012516, 1.092708333674754506, 0.7879004041258379498 ) ) ;
#65050 = CARTESIAN_POINT ( 'NONE',  ( 2.492951620383182298, 8.266420250602603659, -2.456391984604371359 ) ) ;
#65052 = ORIENTED_EDGE ( 'NONE', *, *, #40506, .T. ) ;
#65053 = CARTESIAN_POINT ( 'NONE',  ( 3.059543388688467314, -1.367113599135186819, 1.847867383329027335 ) ) ;
#65054 = CARTESIAN_POINT ( 'NONE',  ( 7.293923454472077239, 10.49303254931736262, 1.082531754730558626 ) ) ;
#65056 = CARTESIAN_POINT ( 'NONE',  ( 1.642778471875000035, -0.5760416661887077794, -2.845375778867859751 ) ) ;
#65055 = CARTESIAN_POINT ( 'NONE',  ( 5.722950238744198614, 8.730506807626655430, 1.082531754730549967 ) ) ;
#65057 = CARTESIAN_POINT ( 'NONE',  ( 6.720655732516669367, 7.629137130509068498, 2.426260288887295058 ) ) ;
#65058 = CARTESIAN_POINT ( 'NONE',  ( -7.533490631048818109, 8.818102486758951031, -1.199719254218452047 ) ) ;
#65059 = CARTESIAN_POINT ( 'NONE',  ( 3.697155016903285407, -0.5626119583077812125, 1.858668453590556213 ) ) ;
#65060 = ORIENTED_EDGE ( 'NONE', *, *, #114249, .T. ) ;
#65061 = CARTESIAN_POINT ( 'NONE',  ( 10.18181017373857067, 11.94149529319227909, 1.082531754730548412 ) ) ;
#65062 = CARTESIAN_POINT ( 'NONE',  ( 3.709155072767254868, 1.612916391665040416, -1.027221078234448859 ) ) ;
#65063 = DIRECTION ( 'NONE',  ( 1.561251128379126077E-17, 1.301042606982605475E-17, 1.000000000000000000 ) ) ;
#65064 = CARTESIAN_POINT ( 'NONE',  ( 5.350533963330765808, 0.5041449683875122156, 1.649457517733200040 ) ) ;
#65065 = CARTESIAN_POINT ( 'NONE',  ( 3.661342437515973547, 1.897110692972364454, -0.6839366698164970337 ) ) ;
#65066 = CARTESIAN_POINT ( 'NONE',  ( 4.553568368667338717, -1.501836741657993191, 1.740358071397982265 ) ) ;
#65067 = DIRECTION ( 'NONE',  ( -0.6507913734559640506, -0.7592566023653004592, 0.000000000000000000 ) ) ;
#65068 = CARTESIAN_POINT ( 'NONE',  ( 0.8036966383840878914, 1.806304194667744500, 1.267646993260997723 ) ) ;
#65069 = CARTESIAN_POINT ( 'NONE',  ( -3.350273356352693188, 6.922752992471175482, 0.000000000000000000 ) ) ;
#65070 = CARTESIAN_POINT ( 'NONE',  ( 5.958207135543601041, 0.7187401461678426529, 1.617382982224302879 ) ) ;
#65071 = EDGE_CURVE ( 'NONE', #56380, #49964, #87561, .T. ) ;
#65073 = CARTESIAN_POINT ( 'NONE',  ( 2.449550052152906332, 0.6095859302821411418, -2.209661595554306412 ) ) ;
#65072 = CARTESIAN_POINT ( 'NONE',  ( 6.225128807330042591, 7.291680359087043151, -1.199719254218452047 ) ) ;
#65074 = CARTESIAN_POINT ( 'NONE',  ( 0.8315134001313486678, 1.713846476070936653, 0.3014184826048373900 ) ) ;
#65075 = CARTESIAN_POINT ( 'NONE',  ( 1.123270288250309834, 3.221052654332833054, -0.7749999999993620881 ) ) ;
#65076 = CARTESIAN_POINT ( 'NONE',  ( 0.8426186123336505407, -0.9696909581486823360, 1.437080622210512360 ) ) ;
#65077 = CARTESIAN_POINT ( 'NONE',  ( -1.953008978358306879E-14, 0.2343750003414031002, 1.570758158831794260 ) ) ;
#65078 = AXIS2_PLACEMENT_3D ( 'NONE', #168380, #170505, #70845 ) ;
#65079 = DIRECTION ( 'NONE',  ( 0.000000000000000000, 0.000000000000000000, 1.000000000000000000 ) ) ;
#65080 = CARTESIAN_POINT ( 'NONE',  ( 0.8015275938294207370, -1.862055209299150249, 1.116337150347948892 ) ) ;
#65081 = CARTESIAN_POINT ( 'NONE',  ( 2.712125330650519750, 1.116209241849321465, -1.679223868463100011 ) ) ;
#65082 = CARTESIAN_POINT ( 'NONE',  ( 1.499999999999987121, 0.3270833340161527492, -0.8660254037844323793 ) ) ;
#65083 = CARTESIAN_POINT ( 'NONE',  ( 5.584577364790731302, -1.880054400457907171, -0.4198111936028568469 ) ) ;
#65084 = CARTESIAN_POINT ( 'NONE',  ( 1.364683531249996529, 12.46354166700806054, 0.7879004041258405033 ) ) ;
#65085 = CARTESIAN_POINT ( 'NONE',  ( 2.215342456320268383, 1.781105875021117502, -1.327318755304232933 ) ) ;
#65086 = ORIENTED_EDGE ( 'NONE', *, *, #82056, .T. ) ;
#65087 = CARTESIAN_POINT ( 'NONE',  ( 6.496114076516082747, -8.169775483750532530, 6.932145363377579805 ) ) ;
#65088 =( NAMED_UNIT ( * ) PLANE_ANGLE_UNIT ( ) SI_UNIT ( $, .RADIAN. ) );
#65089 = CARTESIAN_POINT ( 'NONE',  ( 8.353795204314554468, 12.89784483834236184, -0.7998128361456352531 ) ) ;
#65090 = CARTESIAN_POINT ( 'NONE',  ( 8.122743427918724279, 8.649157885426255632, 0.7216878364870267237 ) ) ;
#65091 = CARTESIAN_POINT ( 'NONE',  ( 5.126372767375061201, 0.1352161506754517850, 1.735264446013358608 ) ) ;
#65092 = CARTESIAN_POINT ( 'NONE',  ( 3.789464544343919883, -1.813617537123424661, 0.7486148740368094856 ) ) ;
#65094 = CARTESIAN_POINT ( 'NONE',  ( -7.700668062882084719, 8.086460282891644979, -0.7216878364870278340 ) ) ;
#65093 = CARTESIAN_POINT ( 'NONE',  ( 4.090809663021327758, 5.795697244990093644, 1.599625672291267398 ) ) ;
#65095 = CARTESIAN_POINT ( 'NONE',  ( -1.392969482149210014, 4.158527933356495510, 0.5575990067801558370 ) ) ;
#65096 = CARTESIAN_POINT ( 'NONE',  ( 4.534621088391048715, 2.217606307645642261, 0.4472613530076152699 ) ) ;
#65097 = CARTESIAN_POINT ( 'NONE',  ( 1.100133984900531825, 0.8377775336174065890, -1.885062252648894265 ) ) ;
#65098 = CARTESIAN_POINT ( 'NONE',  ( -7.854251061018346469, 8.057714414143200443, -0.7998128361456291469 ) ) ;
#65099 = ADVANCED_FACE ( 'NONE', ( #153798, #50965 ), #167913, .T. ) ;
#65100 = CARTESIAN_POINT ( 'NONE',  ( -3.429849674132942727, 5.984946472254969230, -1.082531754730549078 ) ) ;
#65101 = CARTESIAN_POINT ( 'NONE',  ( 2.413256113406063275, 2.020865564879420262, 1.017551375885389131 ) ) ;
#65102 = VERTEX_POINT ( 'NONE', #117088 ) ;
#65103 = CARTESIAN_POINT ( 'NONE',  ( 1.499999999999987121, 1.827083334016151861, -0.8660254037844253849 ) ) ;
#65104 = CARTESIAN_POINT ( 'NONE',  ( 2.776451973220807279, -1.788819259240326698, -0.5467896145717602296 ) ) ;
#65105 = CARTESIAN_POINT ( 'NONE',  ( 1.265804362365889668, 1.602598504008081237, -0.6630416328189077113 ) ) ;
#65106 = CARTESIAN_POINT ( 'NONE',  ( 5.689076433642084041, 1.658752129386225516, 1.432425853890168188 ) ) ;
#65107 = CARTESIAN_POINT ( 'NONE',  ( 6.440458288041322810, 2.281167638128688946, 0.3475669597150666257 ) ) ;
#65108 = CARTESIAN_POINT ( 'NONE',  ( 4.416967121957662279, 1.975198431823081302, 0.8787980929093119897 ) ) ;
#65109 = CARTESIAN_POINT ( 'NONE',  ( 4.101460596356475641, -1.936652220471976937, 0.1442349196467233863 ) ) ;
#65110 = CARTESIAN_POINT ( 'NONE',  ( -4.582292731294565158, 4.448355729372827305, 1.214306433183764966E-14 ) ) ;
#65111 = DIRECTION ( 'NONE',  ( 1.000000000000000000, 0.000000000000000000, 8.638326563840826660E-31 ) ) ;
#65112 = CARTESIAN_POINT ( 'NONE',  ( 0.9687500000000008882, 0.7852924748299362490, -1.895863743164110327 ) ) ;
#65113 = CARTESIAN_POINT ( 'NONE',  ( 4.027228449831594226, 7.557535101434955216, 0.3677212997342318990 ) ) ;
#65114 = CARTESIAN_POINT ( 'NONE',  ( 6.116136693540529912, 10.14959355252369910, 1.530808498934192557E-16 ) ) ;
#65115 = CARTESIAN_POINT ( 'NONE',  ( 1.360316468749994012, 2.265625000341386919, -1.387778780781445676E-14 ) ) ;
#65116 = CARTESIAN_POINT ( 'NONE',  ( 5.186172726741035355, 1.650080556555008293, 1.158690440749516881 ) ) ;
#65117 = CARTESIAN_POINT ( 'NONE',  ( -3.917943204224928699, 4.633650495426258509, -1.082531754730548412 ) ) ;
#65118 = CARTESIAN_POINT ( 'NONE',  ( 6.988338112840064120, 10.24047933403371502, 1.199719254218460707 ) ) ;
#65119 = CARTESIAN_POINT ( 'NONE',  ( 3.542423274920540432, 7.354853930707762721, -1.734723475976807094E-15 ) ) ;
#65120 = CARTESIAN_POINT ( 'NONE',  ( 3.439906511156048285, 0.8199118703316324863, -1.631291955839441865 ) ) ;
#65121 = DIRECTION ( 'NONE',  ( 0.000000000000000000, 8.546850786086437571E-32, 1.000000000000000000 ) ) ;
#65122 = CARTESIAN_POINT ( 'NONE',  ( -1.807716826991530024, 2.517780620582464213, 2.499994708711103630 ) ) ;
#65123 = ORIENTED_EDGE ( 'NONE', *, *, #173439, .F. ) ;
#65124 = CARTESIAN_POINT ( 'NONE',  ( -4.272227801637618505, 7.998366511970260717, 0.7216878364870338292 ) ) ;
#65125 = CARTESIAN_POINT ( 'NONE',  ( -3.285556943750000514, -4.076041666188709556, -1.896917185911906500 ) ) ;
#65126 = CARTESIAN_POINT ( 'NONE',  ( -9.332089804907933939, 9.781859615347734405, 1.040834085586084257E-14 ) ) ;
#65127 = CARTESIAN_POINT ( 'NONE',  ( 6.410808175004245157, -0.5408338447881118061, -1.945826018873537455 ) ) ;
#65128 = CARTESIAN_POINT ( 'NONE',  ( 1.647299267346370444, 0.2110521635003380359, 2.109970702148834754 ) ) ;
#65129 = VERTEX_POINT ( 'NONE', #5371 ) ;
#65130 = CARTESIAN_POINT ( 'NONE',  ( -6.296835998904160014, 6.311006518335105397, 0.000000000000000000 ) ) ;
#65131 = CARTESIAN_POINT ( 'NONE',  ( 4.976006071415387311, 5.764094157194782575, 1.199719254218462483 ) ) ;
#65132 = CARTESIAN_POINT ( 'NONE',  ( 6.385628592921421820, 1.419324251362139133, 1.494494355598655622 ) ) ;
#65133 = CARTESIAN_POINT ( 'NONE',  ( 4.746720300533005421, 1.994071680685698400, -0.2986252114312442640 ) ) ;
#65134 = ORIENTED_EDGE ( 'NONE', *, *, #92482, .F. ) ;
#65135 = ORIENTED_EDGE ( 'NONE', *, *, #63108, .T. ) ;
#65136 = CARTESIAN_POINT ( 'NONE',  ( -10.08065090696061716, 11.71951313199760136, -1.199719254218441611 ) ) ;
#65137 = CARTESIAN_POINT ( 'NONE',  ( -1.225000000000022071, 0.2916666673494853756, -0.7072540797573118043 ) ) ;
#65138 = AXIS2_PLACEMENT_3D ( 'NONE', #202485, #50938, #134354 ) ;
#65140 = FACE_OUTER_BOUND ( 'NONE', #85732, .T. ) ;
#65139 = CARTESIAN_POINT ( 'NONE',  ( -6.469175572376043348, 7.576401584974034265, 1.199719254218452047 ) ) ;
#65141 = CARTESIAN_POINT ( 'NONE',  ( 6.582202237817778467, 6.781708767774706104, 0.2773405359152263383 ) ) ;
#65142 = CARTESIAN_POINT ( 'NONE',  ( 5.624374986212743011, 0.3960386850128463920, -1.976653645673176474 ) ) ;
#65143 = CARTESIAN_POINT ( 'NONE',  ( 5.156134521940135329, -1.331146486249596306, 1.272188372451001026 ) ) ;
#65144 = CARTESIAN_POINT ( 'NONE',  ( -0.02338929933905566777, 0.2563879980532010605, -1.746150209723141167 ) ) ;
#65145 = CARTESIAN_POINT ( 'NONE',  ( 3.633692980683305152, -2.132556294031516142, 0.8823059210255141949 ) ) ;
#65146 = CARTESIAN_POINT ( 'NONE',  ( 5.668190738965027897, 8.770583741171307679, -1.199719254218452047 ) ) ;
#65147 = CARTESIAN_POINT ( 'NONE',  ( 5.782550318682353918, -2.107506929020441788, -0.4798289361013233223 ) ) ;
#65148 = CARTESIAN_POINT ( 'NONE',  ( 6.877010230629674759, 9.046264573866535486, 1.599625672291281386 ) ) ;
#65149 = CARTESIAN_POINT ( 'NONE',  ( 1.013109794239855699, -1.894405189233986597, 0.4268842903399574507 ) ) ;
#65150 = CARTESIAN_POINT ( 'NONE',  ( -3.100010679019018500, 6.768429558830820980, 1.040834085586084257E-14 ) ) ;
#65151 = ORIENTED_EDGE ( 'NONE', *, *, #43730, .T. ) ;
#65152 = CARTESIAN_POINT ( 'NONE',  ( 2.651925681381814837, 0.4070128260628380068, -0.1420391113308220876 ) ) ;
#65153 = CARTESIAN_POINT ( 'NONE',  ( -3.630551273409382329, 7.457669928944732796, 0.7998128361456352531 ) ) ;
#65154 = CARTESIAN_POINT ( 'NONE',  ( 3.344469905398727239, 0.4532862802011444758, 1.814783984445811127 ) ) ;
#65155 = AXIS2_PLACEMENT_3D ( 'NONE', #76147, #190946, #55630 ) ;
#65156 = B_SPLINE_CURVE_WITH_KNOTS ( 'NONE', 3,
 ( #129374, #130431, #44857, #176969, #45921, #160716 ),
 .UNSPECIFIED., .F., .F.,
 ( 4, 2, 4 ),
 ( 0.000000000000000000, 0.0003845013059668469482, 0.0007690026119336938965 ),
 .UNSPECIFIED. ) ;
#65159 = CARTESIAN_POINT ( 'NONE',  ( -5.098748287191073203, 8.106234214101666780, 1.199719254218452935 ) ) ;
#65158 = CARTESIAN_POINT ( 'NONE',  ( 0.7499999999999867883, -0.4020833326505157679, -1.299038105676652899 ) ) ;
#65157 = CARTESIAN_POINT ( 'NONE',  ( 1.775505761281343631, 0.3235837346332003372, -1.884644527778083001 ) ) ;
#65160 = CARTESIAN_POINT ( 'NONE',  ( 2.666872310945223923, -1.521158656661812714, 1.599105504226288499 ) ) ;
#65161 = CARTESIAN_POINT ( 'NONE',  ( 6.983263157960407419, 1.286439435963281142, 1.962168536134776931 ) ) ;
#65162 = CARTESIAN_POINT ( 'NONE',  ( -3.618674974218159868, 7.443814246554973479, 0.3006916729143232492 ) ) ;
#65163 = CARTESIAN_POINT ( 'NONE',  ( 6.224601922005513543, 7.395028676162137771, -1.082531754730548412 ) ) ;
#65164 = CARTESIAN_POINT ( 'NONE',  ( -2.948008335967658322, 5.526761261015804116, 1.199719254218462483 ) ) ;
#65165 = CARTESIAN_POINT ( 'NONE',  ( -6.034787771414192648, 9.094317262408276648, 1.082531754730549967 ) ) ;
#65166 = CARTESIAN_POINT ( 'NONE',  ( 1.089067603693228525, 1.740485041285372958, -0.9256802945506740210 ) ) ;
#65167 = CARTESIAN_POINT ( 'NONE',  ( 0.8862589459083686227, 1.552251447166236975, 1.707653507296547968 ) ) ;
#65168 = CARTESIAN_POINT ( 'NONE',  ( 1.152704166800899932, -0.4732522875653189520, -1.903817266927515961 ) ) ;
#65169 = CARTESIAN_POINT ( 'NONE',  ( 5.506706524517535506, 0.5933582781832097419, 1.975413352875006856 ) ) ;
#65170 = CARTESIAN_POINT ( 'NONE',  ( 5.680503174445848735, 5.729601246382692636, 1.040834085586084257E-14 ) ) ;
#65171 = CARTESIAN_POINT ( 'NONE',  ( 4.532168488718122390, 8.509556680138327778, 0.7998128361456271485 ) ) ;
#65172 = EDGE_LOOP ( 'NONE', ( #202957, #52644, #59305, #7216 ) ) ;
#65173 = CARTESIAN_POINT ( 'NONE',  ( 0.6823417656249917140, 4.905208333674755394, 1.181850606188765695 ) ) ;
#65174 = CARTESIAN_POINT ( 'NONE',  ( 7.204675194429079505E-15, -1.487500000000000044, -3.475000000000000089 ) ) ;
#65175 = CARTESIAN_POINT ( 'NONE',  ( 3.348500752450937590, 5.890039396959305229, 1.082531754730558626 ) ) ;
#65176 = CARTESIAN_POINT ( 'NONE',  ( 1.147616990042895191, 1.915638116573715743, -1.021621585119661058 ) ) ;
#65178 = CARTESIAN_POINT ( 'NONE',  ( 6.356982874815331641, 0.3076174260261410054, -1.815216213958574132 ) ) ;
#65177 = CARTESIAN_POINT ( 'NONE',  ( -11.96217875511318240, 11.32854366578976624, 0.9561995067075053090 ) ) ;
#65179 = CARTESIAN_POINT ( 'NONE',  ( 11.49978884755361008, 11.24270821162803813, -3.429452816445331731 ) ) ;
#65180 = CARTESIAN_POINT ( 'NONE',  ( -2.744103632728948305, 3.021832644587346017, -2.500000000000000444 ) ) ;
#65181 = CARTESIAN_POINT ( 'NONE',  ( 1.370139650511486007, -1.190941340819328564, 1.442406204513801971 ) ) ;
#65182 = CARTESIAN_POINT ( 'NONE',  ( 5.149776166300943814, 0.6834882490109328579, -2.050742609271530181 ) ) ;
#65183 = CARTESIAN_POINT ( 'NONE',  ( -6.087928554039494067, 6.027116558704463500, 0.4103310871990673014 ) ) ;
#65184 = CARTESIAN_POINT ( 'NONE',  ( 0.07735805125223899070, 6.946777552644263665, -2.683974465663693021 ) ) ;
#65185 = CARTESIAN_POINT ( 'NONE',  ( -1.402160292154681736E-14, -0.05312499965857903073, -1.575800808251665908 ) ) ;
#65186 = CARTESIAN_POINT ( 'NONE',  ( 1.857924044808876074, 0.7306008629870773818, -1.767408594711167735 ) ) ;
#65187 = CARTESIAN_POINT ( 'NONE',  ( 3.133429157788733654, -1.187652617478820227, -1.312364946228376628 ) ) ;
#65188 = CARTESIAN_POINT ( 'NONE',  ( 0.4340482808194641162, -1.023182136338888659, -1.615339470012015166 ) ) ;
#65190 = CARTESIAN_POINT ( 'NONE',  ( 5.782812685692425347, 1.563071972524389786, -1.107110302061852236 ) ) ;
#65189 = CARTESIAN_POINT ( 'NONE',  ( 0.7335685072721549460, -3.146544515318441704, -3.295627537534667972 ) ) ;
#65191 = CARTESIAN_POINT ( 'NONE',  ( 6.865690646733241032, -0.4297541067138924697, 1.928966555396218752 ) ) ;
#65192 = CARTESIAN_POINT ( 'NONE',  ( 1.499999999999989120, 4.754166666666689522, 0.8660254037844524744 ) ) ;
#65194 = CARTESIAN_POINT ( 'NONE',  ( 1.195735321641926197, 1.957225868588155837, -0.8166992996602240318 ) ) ;
#65193 = VECTOR ( 'NONE', #182160, 1000.000000000000114 ) ;
#65195 = CARTESIAN_POINT ( 'NONE',  ( 5.495418255317095380, 6.026204583819558813, -0.7979391942483995415 ) ) ;
#65196 = CARTESIAN_POINT ( 'NONE',  ( 4.662891624058607576, -1.671085903211678270, -0.8408918736509605196 ) ) ;
#65198 = ORIENTED_EDGE ( 'NONE', *, *, #171659, .T. ) ;
#65197 = CARTESIAN_POINT ( 'NONE',  ( 1.049113529465800054, -1.437755431736492673, -1.125068434497819680 ) ) ;
#65200 = CARTESIAN_POINT ( 'NONE',  ( 4.794097012578165007, 8.135614534340449566, -0.8214339667521903809 ) ) ;
#65199 = CARTESIAN_POINT ( 'NONE',  ( 5.145248760827346501, -1.894204247122273088, 1.132176536499051700 ) ) ;
#65201 = EDGE_CURVE ( 'NONE', #28319, #75836, #34700, .T. ) ;
#65202 = CARTESIAN_POINT ( 'NONE',  ( -1.364683531249997417, 5.321875000341417916, 1.214306433183764966E-14 ) ) ;
#65203 = CARTESIAN_POINT ( 'NONE',  ( 1.732955346664406537, -1.957976925384408817, -0.6489628464096306448 ) ) ;
#65204 = CARTESIAN_POINT ( 'NONE',  ( 6.661133543015731462, 6.665743976473484267, -0.7998128361456281477 ) ) ;
#65205 = CARTESIAN_POINT ( 'NONE',  ( -9.040589502214116280, 9.441775928871617651, 0.7998128361456462443 ) ) ;
#65206 = DIRECTION ( 'NONE',  ( -1.000000000000000000, 0.000000000000000000, 3.491481338843133355E-15 ) ) ;
#65207 = DIRECTION ( 'NONE',  ( 0.000000000000000000, 0.000000000000000000, 1.000000000000000000 ) ) ;
#65208 = CARTESIAN_POINT ( 'NONE',  ( 7.991605200612358573, 8.288237253661408843, 0.7998128361456281477 ) ) ;
#65209 = VERTEX_POINT ( 'NONE', #152724 ) ;
#65210 = ADVANCED_FACE ( 'NONE', ( #185205, #4305 ), #200386, .T. ) ;
#65211 = CARTESIAN_POINT ( 'NONE',  ( 4.352052382902608763, -0.7952921280917917279, 1.911720769834825973 ) ) ;
#65212 = CARTESIAN_POINT ( 'NONE',  ( 0.6823417656249882723, -0.8447916663252494907, 1.181850606188755259 ) ) ;
#65213 = CARTESIAN_POINT ( 'NONE',  ( 1.353037089713942320, -1.704917477850418805, 1.328741451194020762 ) ) ;
#65214 = CARTESIAN_POINT ( 'NONE',  ( -5.575295409310188965, 7.417394932307940003, -1.244639187630245170 ) ) ;
#65215 = CARTESIAN_POINT ( 'NONE',  ( 1.735027068915934167, 1.885295237280168790, 0.7248928932378613244 ) ) ;
#65216 = CARTESIAN_POINT ( 'NONE',  ( -0.4500000000000232703, 4.000000000000003553, 0.8338124244295432863 ) ) ;
#65218 = CARTESIAN_POINT ( 'NONE',  ( 5.992340707560141588, 9.934888558888093968, 0.7216878364870438212 ) ) ;
#65217 = CARTESIAN_POINT ( 'NONE',  ( -3.475000000000000533, -2.800000000000000266, 0.000000000000000000 ) ) ;
#65219 = CARTESIAN_POINT ( 'NONE',  ( 6.883263157960366030, 0.5727201817382967519, 2.105997115537924902 ) ) ;
#65220 = CARTESIAN_POINT ( 'NONE',  ( 0.2160302486270138655, 1.032475520995678853, -1.731998313101141163 ) ) ;
#65221 = CARTESIAN_POINT ( 'NONE',  ( 4.915667883426772633, -1.172277214026868464, -1.851500752446763709 ) ) ;
#65222 =( BOUNDED_CURVE ( )  B_SPLINE_CURVE ( 3, ( #114665, #79956, #211012, #163359 ),
 .UNSPECIFIED., .F., .T. ) 
 B_SPLINE_CURVE_WITH_KNOTS ( ( 4, 4 ),
 ( 0.4999999999999939493, 1.000000000000000000 ),
 .UNSPECIFIED. ) 
 CURVE ( )  GEOMETRIC_REPRESENTATION_ITEM ( )  RATIONAL_B_SPLINE_CURVE ( ( 1.000000000000007994, 0.3333333333333333148, 0.3333333333333252657, 1.000000000000000000 ) ) 
 REPRESENTATION_ITEM ( '' )  );
#65223 = B_SPLINE_CURVE_WITH_KNOTS ( 'NONE', 3,
 ( #85254, #87405, #184876, #201116, #105824, #54900, #48783, #168641, #154539, #20243, #121053, #118892, #170778, #36502, #171850, #122122, #6120, #2911, #137235, #155606, #86329, #152400, #52757, #151342, #203257, #103660, #72188, #138297, #39716, #187019, #202180, #7190, #3979, #70048, #136162, #119968, #185945, #114899, #37578, #68984, #22367, #23445, #180897, #135102, #204312, #89555, #169709, #21299, #153470, #5043, #55969, #38652, #104731, #188086, #32519, #131155, #197145, #164656, #19179, #176134, #77544, #94890, #107989, #8273, #127463, #42945, #126385, #60226, #93828, #76475, #159869, #205398, #9349, #11473, #91698, #74356, #41878, #191278, #75421, #160942, #73263, #174017, #10402, #142586, #206472, #45078, #109053, #139367, #141533, #157751, #140460, #58101, #110122, #189165, #209660, #28805, #124260, #40804, #193434, #125319, #24513, #27734, #57037, #175071, #111187, #190219, #143666, #61301, #92761, #123204, #158805, #25587, #106911, #172936, #207541, #90623, #177190, #156681, #59161, #26658, #208594, #192345, #44003, #63437, #198733, #518, #99143, #95963, #164143, #34120, #129588, #210741, #79681, #145794, #196636, #47213, #62365, #182491, #195575, #100191, #113327, #12536, #179334, #211800, #30955, #97030, #163084, #128527, #14665, #178268, #115445, #194496, #81813, #48276, #80757, #162017, #46140, #15727, #114389, #146846, #147896, #180384, #64501, #212865, #112255, #78608, #130644, #197683, #29879, #181436, #16786, #13606, #32008, #98090, #213912, #65535, #131681, #49328, #33065, #165192, #144730, #82869, #148947, #66586, #132729, #50379, #116501, #121858, #17846, #118638, #199806, #83931, #5857, #2657, #200858, #68731, #150020, #184623, #117571, #54638, #1590, #67651, #167332, #38389, #138039, #134852, #183566, #35172, #52505, #22099, #53573, #3717, #19988, #133797, #187829, #36240, #136971, #101249, #120787, #170517, #18918, #85002, #168392, #102318, #151094, #103393, #153209, #86073, #51451, #152148, #169454, #69793, #135902, #39455, #166257, #201920, #119706, #71928, #186764, #185689, #104470, #88212, #21040, #154283, #37318, #87138, #204052, #4779, #70857, #202999, #55703, #107731, #127205, #105551, #56777, #173757, #142332, #172673, #8008, #11211, #193172, #25334, #189969, #106645, #40542, #208343, #6928, #27470, #61044, #24250, #73006, #159613, #157496, #122943, #171585, #125067, #59974, #23179, #209400, #90353, #143404, #191025, #89294, #42692, #156422, #155345, #139106, #91435, #205134, #77292, #188899, #74099, #140191, #141276, #9090, #93568, #206212, #41618, #57839, #92512, #76222, #108797, #124001, #75167, #207285, #58912, #174824, #26400, #158550, #10147, #126128, #192088, #43754, #109868, #175880, #178007, #66339, #195321, #65284, #63178, #194240, #129343, #179075, #146594, #131431, #45885, #145546, #196385, #48026, #29624, #16533, #162829, #44822, #113069, #46952, #112006, #95708, #81557, #160682, #181187, #269, #210481, #78353, #197433, #163897, #144476, #147640, #132485, #96778, #98888, #161762, #213659, #32813, #64252, #110927, #130394, #13353, #176931, #28549, #30696, #94638, #12277, #79428, #49074, #211543, #180134, #14406, #115194, #80497, #82615, #164940, #148700, #128279, #114142, #62119, #212612, #31761, #97832, #15473, #168144, #18677, #4534, #202747, #104220, #119456, #52261, #71680 ),
 .UNSPECIFIED., .F., .F.,
 ( 4, 1, 1, 1, 1, 1, 1, 1, 1, 1, 1, 1, 1, 1, 1, 1, 1, 1, 1, 1, 1, 1, 1, 1, 1, 1, 1, 1, 1, 1, 1, 1, 1, 1, 1, 1, 1, 1, 1, 1, 1, 1, 1, 1, 1, 1, 1, 1, 1, 1, 1, 1, 1, 1, 1, 1, 1, 1, 1, 1, 1, 1, 1, 1, 1, 1, 1, 1, 1, 1, 1, 1, 1, 1, 1, 1, 1, 1, 1, 1, 1, 1, 1, 1, 1, 1, 1, 1, 1, 1, 1, 1, 1, 1, 1, 1, 1, 1, 1, 1, 1, 1, 1, 1, 1, 1, 1, 1, 1, 1, 1, 1, 1, 1, 1, 1, 1, 1, 1, 1, 1, 1, 1, 1, 1, 1, 1, 1, 1, 1, 1, 1, 1, 1, 1, 1, 1, 1, 1, 1, 1, 1, 1, 1, 1, 1, 1, 1, 1, 1, 1, 1, 1, 1, 1, 1, 1, 1, 1, 1, 1, 1, 1, 1, 1, 1, 1, 1, 1, 1, 1, 1, 1, 1, 1, 1, 1, 1, 1, 1, 1, 1, 1, 1, 1, 1, 1, 1, 1, 1, 1, 1, 1, 1, 1, 1, 1, 1, 1, 1, 1, 1, 1, 1, 1, 1, 1, 1, 1, 1, 1, 1, 1, 1, 1, 1, 1, 1, 1, 1, 1, 1, 1, 1, 1, 1, 1, 1, 1, 1, 1, 1, 1, 1, 1, 1, 1, 1, 1, 1, 1, 1, 1, 1, 1, 1, 1, 1, 1, 1, 1, 1, 1, 1, 1, 1, 1, 1, 1, 1, 1, 1, 1, 1, 1, 1, 1, 1, 1, 1, 1, 1, 1, 1, 1, 1, 1, 1, 1, 1, 1, 1, 1, 1, 1, 1, 1, 1, 1, 1, 1, 1, 1, 1, 1, 1, 1, 1, 1, 1, 1, 1, 1, 1, 1, 1, 1, 1, 1, 1, 1, 1, 1, 1, 1, 1, 1, 1, 1, 1, 1, 1, 1, 1, 1, 1, 1, 1, 1, 1, 1, 1, 1, 1, 1, 1, 1, 1, 1, 1, 1, 1, 1, 1, 1, 1, 1, 1, 1, 1, 1, 1, 1, 1, 1, 1, 1, 1, 1, 1, 1, 1, 1, 1, 1, 1, 1, 1, 1, 1, 1, 1, 1, 1, 1, 1, 1, 1, 1, 1, 1, 1, 1, 1, 4 ),
 ( 0.000000000000000000, 0.002599974731368114196, 0.005208790931971673047, 0.007813145979665977320, 0.01041652777592116073, 0.01302061325022423749, 0.01562498222773845216, 0.01822909327250534645, 0.02083329118620782031, 0.02343750764584028035, 0.02604160881127103033, 0.02864587273906003470, 0.03124992668191499748, 0.03385418289307650513, 0.03645825757725845717, 0.03906249379052053466, 0.04166666320740203266, 0.04427081823557592333, 0.04687506849204003262, 0.04947913642841410276, 0.05208339700068515682, 0.05468745344639398126, 0.05729170333903113588, 0.05989581325979084075, 0.06250002080062810883, 0.06510424464624173235, 0.06770834408375023261, 0.07031260355790951155, 0.07291665769283758869, 0.07552091454841564078, 0.07812498837240108851, 0.08072922377910608793, 0.08333339284475561881, 0.08593754734057650058, 0.08854179710653446722, 0.09114586450482109470, 0.09375012458370637902, 0.09635418052565795921, 0.09895842987840544613, 0.1015625393267825388, 0.1041667463075427041, 0.1067709697059155277, 0.1093750686050062593, 0.1119793276133541904, 0.1145833812402851093, 0.1171876375884709082, 0.1197917109360151500, 0.1223959458003068407, 0.1250001144218755300, 0.1276042683764700425, 0.1302085177025434359, 0.1328125845892443313, 0.1354168441945610146, 0.1380208996559441903, 0.1406251484930516882, 0.1432292574929059925, 0.1458334639374244401, 0.1484376869122458475, 0.1510417852965526830, 0.1536460438630466996, 0.1562500970055218374, 0.1588543528702505148, 0.1614584257649260002, 0.1640626601106844606, 0.1666668283118819260, 0.1692709817489688462, 0.1718752306590244638, 0.1744792970577103974, 0.1770835562133957763, 0.1796876112177483997, 0.1822918595631332073, 0.1848959681380851483, 0.1875001740701665309, 0.1901043966452301559, 0.1927084945383780445, 0.1953127526869259389, 0.1979168053684795814, 0.2005210607736844508, 0.2031251332390507092, 0.2057293670901427229, 0.2083335348946688259, 0.2109376878379560227, 0.2135419363558502259, 0.2161460022900811573, 0.2187502610200618980, 0.2213543155909112325, 0.2239585634684796434, 0.2265626716421396125, 0.2291668770855771753, 0.2317710992846666596, 0.2343751967102698508, 0.2369794544647692847, 0.2395835067089256143, 0.2421877616785296505, 0.2447918337381362330, 0.2473960671184182170, 0.2500002345499632850, 0.2526043870231480248, 0.2552086351727278490, 0.2578127006660536624, 0.2604169589942467167, 0.2630210131551104502, 0.2656252605887587936, 0.2682293683847277177, 0.2708335733633049913, 0.2734377952101950116, 0.2760418921918580404, 0.2786461495761977103, 0.2812502014064713896, 0.2838544559643880194, 0.2864585276417753179, 0.2890627605750938911, 0.2916669276573394809, 0.2942710796841097043, 0.2968753274892133587, 0.2994793925651746958, 0.3020836505154881335, 0.3046877042898750165, 0.3072919513034905736, 0.3098960587453611915, 0.3125002632828523530, 0.3151044848013095923, 0.3177085813626279731, 0.3203128384006882490, 0.3229168898405855304, 0.3255211440107198539, 0.3281252153294201834, 0.3307294478396133885, 0.3333336145962333963, 0.3359377662002681064, 0.3385420136847264727, 0.3411460783668558427, 0.3437503359631899347, 0.3463543893746011126, 0.3489586359920627823, 0.3515627431034201722, 0.3541669472235909888, 0.3567711684373747749, 0.3593752646019360286, 0.3619795213175900916, 0.3645835723906095116, 0.3671878261968588575, 0.3697918971803975663, 0.3723961292912953969, 0.3750002957459567798, 0.3776044469509276524, 0.3802086941385645069, 0.3828127584503868142, 0.3854170157166348365, 0.3880210687885642384, 0.3906253150337437030, 0.3932294218381663375, 0.3958336255647753599, 0.3984378464976386924, 0.4010419422890235119, 0.4036461987061379930, 0.4062502494357712601, 0.4088545029020263510, 0.4114585735739221262, 0.4140628053093475813, 0.4166669714857112461, 0.4192711223152827404, 0.4218753692299160307, 0.4244794331949501842, 0.4270836901549991405, 0.4296877429109347002, 0.4322919888076972583, 0.4348960953287579478, 0.4375002986855570652, 0.4401045193612476147, 0.4427086148030301427, 0.4453128709454660106, 0.4479169213551993378, 0.4505211745053449013, 0.4531252448891109341, 0.4557294762728811288, 0.4583336421946030970, 0.4609377926724337327, 0.4635420393378766879, 0.4661461029796354349, 0.4687503596573671660, 0.4713544121207915438, 0.4739586576929967765, 0.4765627639542633909, 0.4791669669649988861, 0.4817711874072597711, 0.4843752825230089321, 0.4869795384146229367, 0.4895835885279371524, 0.4921878413858530310, 0.4947919115049980165, 0.4973961425609249032, 0.5000003082516567554, 0.5026044584014001115, 0.5052087048414615200, 0.5078127681834534446, 0.5104170246027455171, 0.5130210767971369323, 0.5156253220686399796, 0.5182294280936764475, 0.5208336307820899957, 0.5234378510146604491, 0.5260419458279406157, 0.5286462014925853437, 0.5312502513329574461, 0.5338545039225196520, 0.5364585738005485105, 0.5390628045524396006, 0.5416669700358295314, 0.5442711198811350792, 0.5468753661196208427, 0.5494794291853500878, 0.5520836853700766822, 0.5546877373189100791, 0.5572919823135623618, 0.5598960881259297251, 0.5625002905157588939, 0.5651045105623757614, 0.5677086050967478092, 0.5703128605582734600, 0.5729169101491768945, 0.5755211624942581095, 0.5781252321546730411, 0.5807294626263322934, 0.5833336279260263879, 0.5859377774905402125, 0.5885420235512536236, 0.5911460863642216124, 0.5937503423382545220, 0.5963543940650019026, 0.5989586388066517886, 0.6015627444299086468, 0.6041669465448881171, 0.6067711664292861906, 0.6093752607083083861, 0.6119795159905627724, 0.6145835653554690969, 0.6171878174799397820, 0.6197918869462408775, 0.6223961171614702526, 0.6250002823011129305, 0.6276044316084782304, 0.6302086775152213605, 0.6328127400989277396, 0.6354169958861367595, 0.6380210474142689048, 0.6406252919267632073, 0.6432293973844667168, 0.6458335992483292820, 0.6484378189942425763, 0.6510419130414711875, 0.6536461681683013447, 0.6562502173306804520, 0.6588544692584096252, 0.6614585385540960871, 0.6640627685366956579, 0.6666669335399304508, 0.6692710826137896474, 0.6718753283903641238, 0.6744793907683068745, 0.6770836463925611337, 0.6796876977455479363, 0.6822919420527318035, 0.6848960473684391204, 0.6875002490049163528, 0.6901044686360783276, 0.6927085624750688453, 0.6953128174703216979, 0.6979168664536427036, 0.7005211182084990496, 0.7031251873570698585, 0.7057294171308388098, 0.7083335820213095824, 0.7109377308853042088, 0.7135419765555117699, 0.7161460387511890957, 0.7187502942363581671, 0.7213543454376690756, 0.7239585895633880996, 0.7265626947606567132, 0.7291668961934797411, 0.7317711157336249661, 0.7343752093879328813, 0.7369794642754557978, 0.7395835131031885945, 0.7421877647090413532, 0.7447918337339959338, 0.7473960633227341166, 0.7500002281240860658, 0.7526043768018576552, 0.7552086223895014827, 0.7578126844264116979, 0.7604169397963658206, 0.7630209908694718379, 0.7656252348375721661, 0.7682293399399604539, 0.7708335411928610714, 0.7734377606657260040, 0.7760418541589074737, 0.7786461089625497101, 0.7812501576581653007, 0.7838544091388848223, 0.7864584780637244865, 0.7890627074912324179, 0.7916668722271122949, 0.7942710207423038238, 0.7968752662711893198, 0.7994793281728324041, 0.8020835834514440377, 0.8046876344198176101, 0.8072918782541467220, 0.8098959832852158369, 0.8125001843819276148, 0.8151044038112509327, 0.8177084971668638902, 0.8203127519104773668, 0.8229168004974481976, 0.8255210518769072747, 0.8281251207251358881, 0.8307293500152160837, 0.8333335147092740813, 0.8359376630855301915, 0.8385419085794658667, 0.8411459703693440204, 0.8437502255804886220, 0.8463542764676049712, 0.8489585201920134550, 0.8515626251753276588, 0.8541668261395859441, 0.8567710455491102106, 0.8593751387907155870, 0.8619793934981552219, 0.8645834419999574028, 0.8671876933020320477, 0.8697917620971562513, 0.8723959912736143352, 0.8750001559495040881, 0.8776043042104727521, 0.8802085496932706699, 0.8828126113948897569, 0.8854168665624462253, 0.8880209173917842369, 0.8906251610301256783, 0.8932292659892527853, 0.8958334668447968108, 0.8984376862582688084, 0.9010417794094305322, 0.9036460341045560174, 0.9062500825446693220, 0.9088543337932389887, 0.9114584025587700866, 0.9140626316454156797, 0.9166667963267953745, 0.9192709444961273402, 0.9218751899916067805, 0.9244792516284782158, 0.9270835067763207871, 0.9296875575713596795, 0.9322918011475309630, 0.9348959061060417852, 0.9375001068764983181, 0.9401043263176916964, 0.9427084194022110619, 0.9453126741091559815, 0.9479167225106870376, 0.9505209737258253355, 0.9531250424882484751, 0.9557292715345466760, 0.9583334362123939743, 0.9609375841976093291, 0.9635418299546441023, 0.9661458919105455623, 0.9687501459642621215, 0.9713541960184646218, 0.9739584433044384815, 0.9765625494917742344, 0.9791667425299969141, 0.9817709508269629737, 0.9843750450459556323, 0.9869794226472197174, 0.9895834977571079660, 0.9921868632736227100, 0.9947912224625704569, 0.9974000159472320437, 1.000000000000000000 ),
 .UNSPECIFIED. ) ;
#65224 = CARTESIAN_POINT ( 'NONE',  ( -0.7499999999999972244, 5.139583334016151639, -1.299038105676652899 ) ) ;
#65225 = CARTESIAN_POINT ( 'NONE',  ( 4.007995338699683607, -0.7271224857151190601, 1.768968726348684406 ) ) ;
#65226 = CARTESIAN_POINT ( 'NONE',  ( -3.242371291962510504, 6.934516940598226320, 1.040834085586084257E-14 ) ) ;
#65227 = CARTESIAN_POINT ( 'NONE',  ( 6.765155463094761679, 6.995028916473103209, 0.7216878364870317197 ) ) ;
#65229 = CARTESIAN_POINT ( 'NONE',  ( 1.915638884950950027, -1.319244919589783516, -1.525031147761625405 ) ) ;
#65228 = CARTESIAN_POINT ( 'NONE',  ( -8.785320351530977234, 13.19336481018743079, 1.040834085586084257E-14 ) ) ;
#65230 = CARTESIAN_POINT ( 'NONE',  ( 1.364683531250000303, 12.81770833367473372, -0.7879004041258355073 ) ) ;
#65231 = VECTOR ( 'NONE', #68391, 1000.000000000000000 ) ;
#65233 = CARTESIAN_POINT ( 'NONE',  ( -3.305155586681401303, 7.078041627762083898, 0.7998128361456352531 ) ) ;
#65232 = CARTESIAN_POINT ( 'NONE',  ( 1.013678699313476095, -2.235087565253154107, 0.5086484811528817485 ) ) ;
#65234 = CARTESIAN_POINT ( 'NONE',  ( 4.225434206992398245, -1.650187577572001629, 0.5017251585606904429 ) ) ;
#65235 = CARTESIAN_POINT ( 'NONE',  ( -0.1394461523060883668, 1.988389203256015536, -2.694605331112149393 ) ) ;
#65236 = CARTESIAN_POINT ( 'NONE',  ( 4.708759422647839976, 4.387974169377582001, -0.7998128361456211532 ) ) ;
#65237 = CARTESIAN_POINT ( 'NONE',  ( -6.776323679501130570, -7.189645481333919896, -6.777910281175996587 ) ) ;
#65238 = CARTESIAN_POINT ( 'NONE',  ( 0.1755611466353811378, 5.720003923744535257, -2.838048273117784959 ) ) ;
#65239 = ORIENTED_EDGE ( 'NONE', *, *, #202346, .T. ) ;
#65240 = VERTEX_POINT ( 'NONE', #149532 ) ;
#65241 = CARTESIAN_POINT ( 'NONE',  ( 5.303285216261115487, 1.594816061929973827, -0.8590795265051922591 ) ) ;
#65242 = ORIENTED_EDGE ( 'NONE', *, *, #201642, .F. ) ;
#65243 = CARTESIAN_POINT ( 'NONE',  ( 5.987861119090863049, 7.014868056141362551, 1.199719254218452047 ) ) ;
#65245 = EDGE_CURVE ( 'NONE', #174590, #149924, #83977, .T. ) ;
#65244 = CARTESIAN_POINT ( 'NONE',  ( 5.553597010146855695, 5.912075037831448832, 0.6282849591137803502 ) ) ;
#65246 = CARTESIAN_POINT ( 'NONE',  ( 5.830666647502705580, 1.211628268937942066, -1.346810592849301047 ) ) ;
#65247 = CARTESIAN_POINT ( 'NONE',  ( 5.302647476276220573, 8.240153584747313076, -1.082531754730548412 ) ) ;
#65248 = TOROIDAL_SURFACE ( 'NONE', #106763, 11.92000000000000171, 0.08000000000000000167 ) ;
#65249 = CARTESIAN_POINT ( 'NONE',  ( -11.84104725192624130, 9.990164625485826733, -1.443823348526935169 ) ) ;
#65250 = CARTESIAN_POINT ( 'NONE',  ( 2.589988673929614738, -2.185656584452956075, -0.1600571409424780822 ) ) ;
#65252 = CARTESIAN_POINT ( 'NONE',  ( 9.511208455186636712, 11.05516360492796935, 1.199719254218453823 ) ) ;
#65251 = CARTESIAN_POINT ( 'NONE',  ( 6.320743865583476229, -1.315316497155760489, 1.316877014833318649 ) ) ;
#65253 = CARTESIAN_POINT ( 'NONE',  ( 4.095261013068919098, -0.3237038700398958690, 1.887879439767611744 ) ) ;
#65254 = CARTESIAN_POINT ( 'NONE',  ( -2.324999999999998845, 0.000000000000000000, -0.5000000000000004441 ) ) ;
#65255 = EDGE_CURVE ( 'NONE', #40132, #172181, #32782, .T. ) ;
#65256 = SURFACE_STYLE_FILL_AREA ( #147612 ) ;
#65257 = CARTESIAN_POINT ( 'NONE',  ( 1.364683531249986537, -0.09479166632524321789, -0.7879004041258309554 ) ) ;
#65258 = CARTESIAN_POINT ( 'NONE',  ( 5.124618876285529367, 7.962177208099690873, -1.082531754730549078 ) ) ;
#65260 = CARTESIAN_POINT ( 'NONE',  ( 5.964083501069187498, -1.130735325014235793, 1.789944102876602328 ) ) ;
#65259 = CARTESIAN_POINT ( 'NONE',  ( -9.978437869977959451, 10.74385839117019614, -0.7216878364870267237 ) ) ;
#65261 = CARTESIAN_POINT ( 'NONE',  ( 1.270647086845246188, -1.370953960119488668, 1.671340013135722335 ) ) ;
#65262 = EDGE_CURVE ( 'NONE', #201912, #62417, #84569, .T. ) ;
#65263 = CARTESIAN_POINT ( 'NONE',  ( -4.447956913735107598, 7.346977611736363656, 1.199719254218452935 ) ) ;
#65264 = CARTESIAN_POINT ( 'NONE',  ( 5.401997860402196316, 5.267028690082820930, 0.000000000000000000 ) ) ;
#65265 = CARTESIAN_POINT ( 'NONE',  ( 1.113953379265147925, -0.8168401028521531382, -1.632710947565917170 ) ) ;
#65266 = CARTESIAN_POINT ( 'NONE',  ( -3.846762897975357198, 5.510976019103107859, -1.599625672291256295 ) ) ;
#65267 = CARTESIAN_POINT ( 'NONE',  ( 4.032112419961201510, 0.9767663869549062516, -1.542106374223570553 ) ) ;
#65268 = CARTESIAN_POINT ( 'NONE',  ( 9.781847885788174324, 12.99548848723393490, -8.037988007782987054 ) ) ;
#65269 = VERTEX_POINT ( 'NONE', #93083 ) ;
#65270 = CARTESIAN_POINT ( 'NONE',  ( 2.875404442980381781, -0.1956706474990059230, 1.959820717905029097 ) ) ;
#65271 = VERTEX_POINT ( 'NONE', #9667 ) ;
#65272 = CARTESIAN_POINT ( 'NONE',  ( 4.528815305949091652, -1.774144813887452266, 0.7903587577767021699 ) ) ;
#65273 = CARTESIAN_POINT ( 'NONE',  ( -3.169574050544739841, 6.919863168935977527, -0.7998128361456481317 ) ) ;
#65275 = CARTESIAN_POINT ( 'NONE',  ( 5.537388447972660721, -0.05000006065614125139, 2.120159173171487055 ) ) ;
#65274 = CARTESIAN_POINT ( 'NONE',  ( 5.494797395288433250, 9.632623737803665875, 0.000000000000000000 ) ) ;
#65276 = FACE_OUTER_BOUND ( 'NONE', #107686, .T. ) ;
#65277 = CARTESIAN_POINT ( 'NONE',  ( 2.754443878939544454, 1.898071056134968959, 0.2320119769325945103 ) ) ;
#65278 = CARTESIAN_POINT ( 'NONE',  ( 5.539635733611046220, 6.394625955944754914, -1.222580188273769908 ) ) ;
#65279 = CARTESIAN_POINT ( 'NONE',  ( -1.217323170181705771, 3.094494316908636744, -0.7749999999999918066 ) ) ;
#65280 = CARTESIAN_POINT ( 'NONE',  ( 4.848976215542928792, 5.686169002002086970, 1.199719254218452047 ) ) ;
#65281 = CARTESIAN_POINT ( 'NONE',  ( 4.125643262898153196, -0.3419791877451948681, 1.983678759314363438 ) ) ;
#65282 = CARTESIAN_POINT ( 'NONE',  ( -5.210200771661759767, 6.624310050620605850, -1.450205880198666364 ) ) ;
#65283 = CARTESIAN_POINT ( 'NONE',  ( 4.881388680972560401, 1.702354803207173584, -0.6601141376258444771 ) ) ;
#65284 = CARTESIAN_POINT ( 'NONE',  ( 1.311079954825690619, -1.633285661836245906, 1.272233187909928454 ) ) ;
#65285 = CARTESIAN_POINT ( 'NONE',  ( -9.219181267612684749, 10.81842823604534765, 1.082531754730558626 ) ) ;
#65286 = CARTESIAN_POINT ( 'NONE',  ( -6.564228937702958788, 6.791309396811020527, 0.4070866938790471679 ) ) ;
#65287 = CARTESIAN_POINT ( 'NONE',  ( -0.3282377607281391496, 1.613835450998152288, 1.224999999999981881 ) ) ;
#65288 = CARTESIAN_POINT ( 'NONE',  ( 5.981297838379462384, 1.727768277425823396, -0.7175292643646775659 ) ) ;
#65289 = CARTESIAN_POINT ( 'NONE',  ( 7.949158136313996259, 8.168439335321471262, 1.040834085586084257E-14 ) ) ;
#65290 = CARTESIAN_POINT ( 'NONE',  ( -5.623934791570304625, 5.455678766453782913, 0.7998128361456341429 ) ) ;
#65291 = CARTESIAN_POINT ( 'NONE',  ( 1.364683531250000303, 10.81770833367473195, -0.7879004041258355073 ) ) ;
#65292 = CARTESIAN_POINT ( 'NONE',  ( -5.005985031943793295, 6.863401842066301661, -1.599625672291256295 ) ) ;
#65294 = CARTESIAN_POINT ( 'NONE',  ( -7.095713291905736853, 9.371694488680407886, 1.599625672291269396 ) ) ;
#65293 = CARTESIAN_POINT ( 'NONE',  ( 2.672928840188529609, 6.270167413528593414, 0.000000000000000000 ) ) ;
#65295 = CARTESIAN_POINT ( 'NONE',  ( -7.930593509350902792, 8.217056947189661287, -0.7998128361456362523 ) ) ;
#65296 = CARTESIAN_POINT ( 'NONE',  ( -4.381256195510448315, 8.263215994737505454, 1.040834085586084257E-14 ) ) ;
#65297 = AXIS2_PLACEMENT_3D ( 'NONE', #48322, #198777, #115487 ) ;
#65298 = CARTESIAN_POINT ( 'NONE',  ( 1.516557075436252733, 0.8353943144701718726, 1.894387172633307692 ) ) ;
#65299 = CARTESIAN_POINT ( 'NONE',  ( 2.372804174479496986, -0.3651721903723912921, -2.085361659519912259 ) ) ;
#65300 = CARTESIAN_POINT ( 'NONE',  ( 7.879259827836241570, 12.34422023245099176, 1.040834085586084257E-14 ) ) ;
#65301 = CARTESIAN_POINT ( 'NONE',  ( 1.147236149642312242, 1.739494102415694243, -0.9234435978164361458 ) ) ;
#65302 = CARTESIAN_POINT ( 'NONE',  ( 4.114373074986557910, 7.676947195153840831, 0.7202382532921544067 ) ) ;
#65303 = CARTESIAN_POINT ( 'NONE',  ( 5.097502569058200983, 6.970172302033127210, -1.443375672974051449 ) ) ;
#65305 = DIRECTION ( 'NONE',  ( 0.6507913734559658270, -0.7592566023652989049, 0.000000000000000000 ) ) ;
#65304 = CARTESIAN_POINT ( 'NONE',  ( 0.000000000000000000, -3.937499999999998224, -4.012584370867899430 ) ) ;
#65306 = CARTESIAN_POINT ( 'NONE',  ( 2.256202855815407915, 0.9821592622454662358, 2.071323110799852873 ) ) ;
#65307 = CARTESIAN_POINT ( 'NONE',  ( -3.809456170543987330, 8.470288933811271903, 2.500000000000000444 ) ) ;
#65308 = CARTESIAN_POINT ( 'NONE',  ( 2.425908952446104827, -1.891012092455180760, 0.2844710172774585488 ) ) ;
#65309 = ORIENTED_EDGE ( 'NONE', *, *, #190382, .T. ) ;
#65310 = CARTESIAN_POINT ( 'NONE',  ( 8.242994206984347372, 8.719174117677642499, 1.040834085586084257E-14 ) ) ;
#65311 = CARTESIAN_POINT ( 'NONE',  ( 0.8791531640492165067, -1.821740142837099174, -0.8571184184497283587 ) ) ;
#65312 = CARTESIAN_POINT ( 'NONE',  ( 1.323018481131872370, -1.771187822987334570, -0.8437873667686208723 ) ) ;
#65313 = CARTESIAN_POINT ( 'NONE',  ( -10.47097470845587175, 11.11055866948701443, 1.040834085586084257E-14 ) ) ;
#65314 = CARTESIAN_POINT ( 'NONE',  ( -6.364663046611467756, 9.512858423433634414, 1.199719254218452047 ) ) ;
#65315 = CARTESIAN_POINT ( 'NONE',  ( -11.94594309014493483, 8.080894294948576473, -0.5280401589721170907 ) ) ;
#65317 = CARTESIAN_POINT ( 'NONE',  ( 2.764225215535959457, -1.222102382295175760, 1.280393980213704763 ) ) ;
#65316 = CARTESIAN_POINT ( 'NONE',  ( 4.136730066327800159, -1.819077861029708032, 1.030257495502053589 ) ) ;
#65318 = CARTESIAN_POINT ( 'NONE',  ( 0.000000000000000000, 0.000000000000000000, 11.92000000000000171 ) ) ;
#65319 = EDGE_CURVE ( 'NONE', #71815, #164855, #39003, .T. ) ;
#65321 = CARTESIAN_POINT ( 'NONE',  ( 5.068466688948791266, -2.157128183272677191, -0.7757897288535390290 ) ) ;
#65320 = CARTESIAN_POINT ( 'NONE',  ( -1.162044386198238837E-16, 2.062499999999991562, 1.224999999999974332 ) ) ;
#65322 = CARTESIAN_POINT ( 'NONE',  ( 4.698987106650459822, -0.4602053158732459237, 1.678299975232977026 ) ) ;
#65323 = CARTESIAN_POINT ( 'NONE',  ( 8.594979316059474073, 12.11489407112305372, 1.199719254218450271 ) ) ;
#65324 = PRESENTATION_LAYER_ASSIGNMENT (  '', '', ( #23748 ) ) ;
#65325 = DIRECTION ( 'NONE',  ( 0.000000000000000000, 0.000000000000000000, 1.000000000000000000 ) ) ;
#65326 = CARTESIAN_POINT ( 'NONE',  ( 4.411323335215872277, 0.4626541248624673752, 1.670896574705359461 ) ) ;
#65327 = CARTESIAN_POINT ( 'NONE',  ( 4.914598841593178946, 0.8265366316180179362, 2.007889688367751724 ) ) ;
#65328 = CARTESIAN_POINT ( 'NONE',  ( 4.196412238629597447, 4.854568018944682706, -1.199719254218452047 ) ) ;
#65329 = CARTESIAN_POINT ( 'NONE',  ( 5.647672796105281279, 1.985869605424210649, -0.3494789899042491932 ) ) ;
#65330 = CARTESIAN_POINT ( 'NONE',  ( 0.3124999997796079620, 1.451031294483781764, 1.451031289061110341 ) ) ;
#65331 = CARTESIAN_POINT ( 'NONE',  ( 1.499999999999990896, 3.556250000682818602, 1.214306433183764966E-14 ) ) ;
#65332 = CARTESIAN_POINT ( 'NONE',  ( 2.643477790179576292, -1.426271481392614948, -1.295054687222449541 ) ) ;
#65333 = CARTESIAN_POINT ( 'NONE',  ( 1.499999999999997113, 9.927083334016131744, -0.8660254037844378194 ) ) ;
#65334 = CARTESIAN_POINT ( 'NONE',  ( 5.291355414077095531, -0.05489642510923819357, -2.220905102120291019 ) ) ;
#65335 = ORIENTED_EDGE ( 'NONE', *, *, #4201, .T. ) ;
#65336 = CARTESIAN_POINT ( 'NONE',  ( 6.983263157960404754, 0.5693283498368858497, 2.097578288773850552 ) ) ;
#65337 = CARTESIAN_POINT ( 'NONE',  ( 1.499999999999989120, 2.775000000000020339, 1.214306433183764966E-14 ) ) ;
#65338 = CARTESIAN_POINT ( 'NONE',  ( 7.800018446563675489, 7.994443030612759848, -0.7998128361456281477 ) ) ;
#65339 = CARTESIAN_POINT ( 'NONE',  ( 2.034109888970101920, -2.153751770765993001, 0.5431444268512666262 ) ) ;
#65340 = CARTESIAN_POINT ( 'NONE',  ( -3.197123283245616676, -0.9841229182759280159, 1.361626862150112860 ) ) ;
#65341 = CARTESIAN_POINT ( 'NONE',  ( 8.934460041725669655, 9.525884258209195821, 1.040834085586084257E-14 ) ) ;
#65342 = AXIS2_PLACEMENT_3D ( 'NONE', #97491, #132142, #200274 ) ;
#65343 = CARTESIAN_POINT ( 'NONE',  ( -9.531018800282611281, 12.14260790512831889, 1.443375672974076540 ) ) ;
#65344 = CARTESIAN_POINT ( 'NONE',  ( 8.000720045840086669, 8.506797273001177828, 0.7216878364870267237 ) ) ;
#65345 = CARTESIAN_POINT ( 'NONE',  ( -0.05211191391743182078, -1.802403943428915412, -0.9041556775107384425 ) ) ;
#65347 = CARTESIAN_POINT ( 'NONE',  ( 4.896965771356657449, 0.3494220250804170314, 2.032713711554866354 ) ) ;
#65346 = CARTESIAN_POINT ( 'NONE',  ( 10.70146331988817323, 11.37946204949139251, 0.7998128361456341429 ) ) ;
#65348 = CARTESIAN_POINT ( 'NONE',  ( -4.952806187693842510, 4.672695395264567786, 0.7998128361456341429 ) ) ;
#65349 = CARTESIAN_POINT ( 'NONE',  ( -1.499999999999997780, 5.431250000682820378, 1.214306433183764966E-14 ) ) ;
#65350 = CARTESIAN_POINT ( 'NONE',  ( -1.364683531250014514, -0.2197916663252438285, 0.7879004041258379498 ) ) ;
#65351 = CARTESIAN_POINT ( 'NONE',  ( 6.274654046616443992, -1.776150972019393093, -0.5868208112121618969 ) ) ;
#65352 = CARTESIAN_POINT ( 'NONE',  ( 5.080564943346563389, -0.6172752100359213401, 1.620779670503540659 ) ) ;
#65353 = CARTESIAN_POINT ( 'NONE',  ( 4.862738897425579410, 0.1637244223539826016, -1.732714468228998994 ) ) ;
#65354 = CARTESIAN_POINT ( 'NONE',  ( 3.161022370280501814, 6.839609865302569425, 0.000000000000000000 ) ) ;
#65355 = CARTESIAN_POINT ( 'NONE',  ( 2.296762559223310074, 1.838876890742843884, -1.368561501106011713 ) ) ;
#65356 = CARTESIAN_POINT ( 'NONE',  ( 1.364683531249988535, 4.717708333674756283, -0.7879004041258300672 ) ) ;
#65358 = CARTESIAN_POINT ( 'NONE',  ( 5.302318524065624317, 1.582279558761565452, -1.366676729786527211 ) ) ;
#65357 = B_SPLINE_CURVE_WITH_KNOTS ( 'NONE', 3,
 ( #177038, #128380, #161866, #132582, #168243, #18771, #84855, #2508 ),
 .UNSPECIFIED., .F., .F.,
 ( 4, 2, 2, 4 ),
 ( -5.999999997803333335E-08, 0.001024127516013730770, 0.001536221274020587195, 0.002048315032027443836 ),
 .UNSPECIFIED. ) ;
#65359 = CARTESIAN_POINT ( 'NONE',  ( 1.359045109759978498, 1.814150759811587355, -0.3131490413979670651 ) ) ;
#65360 = CARTESIAN_POINT ( 'NONE',  ( 1.355808955840427734E-16, 1.500000000000001332, 2.025000000000007905 ) ) ;
#65361 = CARTESIAN_POINT ( 'NONE',  ( 2.303361484738715159, 1.314996338066702242, -1.528741580717301263 ) ) ;
#65362 = CARTESIAN_POINT ( 'NONE',  ( 1.008081207548201741, -0.9882381260516819310, -1.956047874660173047 ) ) ;
#65363 = CARTESIAN_POINT ( 'NONE',  ( 7.459519926035591553, 16.00000000000000000, -10.25508784514941318 ) ) ;
#65364 = CARTESIAN_POINT ( 'NONE',  ( -5.540478329478883524, 9.615641817700700145, 0.000000000000000000 ) ) ;
#65365 = CARTESIAN_POINT ( 'NONE',  ( 1.574760213118006735, 1.391939136705011348, -1.532762857463897843 ) ) ;
#65366 = CARTESIAN_POINT ( 'NONE',  ( 6.328958779480917229, 6.278206752349526631, 0.7998128361456341429 ) ) ;
#65367 = CARTESIAN_POINT ( 'NONE',  ( -0.6801582343750265380, -0.2864583329919220822, 1.178068619123820771 ) ) ;
#65368 = CARTESIAN_POINT ( 'NONE',  ( 3.510498622083501719, -2.118129049236017192, -0.1023006277712720374 ) ) ;
#65369 = CARTESIAN_POINT ( 'NONE',  ( -1.364683531250014514, 0.4885416670080875434, -0.7879004041258289570 ) ) ;
#65370 = CARTESIAN_POINT ( 'NONE',  ( -0.005450286198350333053, -0.4226363183827580583, -1.886779976948229853 ) ) ;
#65371 = ORIENTED_EDGE ( 'NONE', *, *, #126509, .T. ) ;
#65372 = CARTESIAN_POINT ( 'NONE',  ( -5.143339171537843590, 7.093924681584509173, 1.599625672291263179 ) ) ;
#65373 = CARTESIAN_POINT ( 'NONE',  ( 8.886479618753304166, 12.45497775759917758, -1.199719254218446718 ) ) ;
#65374 = CARTESIAN_POINT ( 'NONE',  ( 6.495764994278797388, 8.671754808115688107, 1.443375672974063439 ) ) ;
#65375 = CARTESIAN_POINT ( 'NONE',  ( 1.737500000000001155, -2.989583332377417690, 3.009438278150922130 ) ) ;
#65376 = TOROIDAL_SURFACE ( 'NONE', #189869, 10.92000000000000348, 0.08000000000000000167 ) ;
#65377 = CARTESIAN_POINT ( 'NONE',  ( -5.045605722580076780, 9.038290442985410067, -0.7998128361456231517 ) ) ;
#65378 = CARTESIAN_POINT ( 'NONE',  ( 3.164323975240455944, 2.019972749466778073, -0.004219792236043878007 ) ) ;
#65379 = CARTESIAN_POINT ( 'NONE',  ( 0.5695303461548965052, 0.2060630844733425115, -2.095861547610248454 ) ) ;
#65380 = CARTESIAN_POINT ( 'NONE',  ( -5.271087860662956537, 9.371629280740593870, 0.000000000000000000 ) ) ;
#65381 = CARTESIAN_POINT ( 'NONE',  ( 7.703003830858588863, 12.13858823597705872, -0.7998128361456291469 ) ) ;
#65382 = CARTESIAN_POINT ( 'NONE',  ( 5.418752549068918789, -1.349321427123598038, 1.281850857350794959 ) ) ;
#65383 = CARTESIAN_POINT ( 'NONE',  ( 9.562578416340237197, 10.05076299535211781, 0.7998128361456462443 ) ) ;
#65384 = DIRECTION ( 'NONE',  ( 0.000000000000000000, 0.000000000000000000, -1.000000000000000000 ) ) ;
#65385 = CARTESIAN_POINT ( 'NONE',  ( -3.066115294984855133, 6.728884944124295053, 0.7998128361456341429 ) ) ;
#65386 = CARTESIAN_POINT ( 'NONE',  ( -7.043624497499477499, 8.176315654292865887, 1.199719254218450271 ) ) ;
#65387 = CARTESIAN_POINT ( 'NONE',  ( 6.280161615599199720, -1.104627599893250434, 1.739653883609869833 ) ) ;
#65389 = CARTESIAN_POINT ( 'NONE',  ( -4.331906098249381110, 7.414796467324478613, 1.153063172049747065 ) ) ;
#65388 = CARTESIAN_POINT ( 'NONE',  ( -5.773793314573309132, 7.829454515125894964, 1.599625672291263179 ) ) ;
#65390 = CARTESIAN_POINT ( 'NONE',  ( 1.364683531249988757, 0.1343750003414204142, 0.000000000000000000 ) ) ;
#65391 = CARTESIAN_POINT ( 'NONE',  ( 2.284178307277694664, -1.682821195468919395, 0.4169209145809901762 ) ) ;
#65392 = CARTESIAN_POINT ( 'NONE',  ( 1.253398004092287854, 0.7024035357156286352, 1.592479786115083229 ) ) ;
#65393 = AXIS2_PLACEMENT_3D ( 'NONE', #6634, #142028, #190723 ) ;
#65395 = CARTESIAN_POINT ( 'NONE',  ( 6.304178240674458422, 10.29869901418813782, 1.040834085586084257E-14 ) ) ;
#65394 = CARTESIAN_POINT ( 'NONE',  ( 6.428381082836107652, 1.334599446741807638, -1.882477381066828936 ) ) ;
#65396 = CARTESIAN_POINT ( 'NONE',  ( -11.04433755984576848, 5.142917986253679352, 4.203129294766247526 ) ) ;
#65397 = CARTESIAN_POINT ( 'NONE',  ( 2.477870184918748997, 1.265364588504451548, 1.626488340418334566 ) ) ;
#65398 = CARTESIAN_POINT ( 'NONE',  ( 4.385172619016207918, 7.203452924572514959, 1.199719254218462483 ) ) ;
#65399 = CARTESIAN_POINT ( 'NONE',  ( 1.370470000664014254, -0.4925687793003556969, 1.954872606163795989 ) ) ;
#65400 = CARTESIAN_POINT ( 'NONE',  ( -7.285838599102589797E-14, 7.078193277237590841, -2.121339347286493648 ) ) ;
#65401 = CARTESIAN_POINT ( 'NONE',  ( -4.613517410400161722, 8.604463755433990002, -0.7998128361456362523 ) ) ;
#65402 = CARTESIAN_POINT ( 'NONE',  ( 1.094530253197498526, -0.4767503703589200392, -1.912843428949811075 ) ) ;
#65404 = CARTESIAN_POINT ( 'NONE',  ( -6.211043768836215229, 8.339580045099285854, 1.443375672974064550 ) ) ;
#65403 = CARTESIAN_POINT ( 'NONE',  ( 4.412309042748480792, -1.912102599942141268, -0.04143165621695726192 ) ) ;
#65405 = CARTESIAN_POINT ( 'NONE',  ( 5.725267921653402148, -0.05769419298589681389, 2.206291853148376170 ) ) ;
#65406 = CARTESIAN_POINT ( 'NONE',  ( -7.227905289416814760, 7.605180057173966723, -0.7216878364870338292 ) ) ;
#65407 = CARTESIAN_POINT ( 'NONE',  ( 5.854088466050551887, 10.05179665369283981, 0.7998128361456341429 ) ) ;
#65408 = CARTESIAN_POINT ( 'NONE',  ( -4.624739795592943459, 6.488892076315448065, -1.443375672974066548 ) ) ;
#65409 = CARTESIAN_POINT ( 'NONE',  ( 0.1354234094306828728, -0.09670520914860020190, 2.017474364592846570 ) ) ;
#65410 = CARTESIAN_POINT ( 'NONE',  ( 4.764381983412778688E-15, 12.71875000068279782, -1.499999999999998446 ) ) ;
#65411 = CARTESIAN_POINT ( 'NONE',  ( 4.137936126805092485, -1.588447180316322260, -1.674080592224574504 ) ) ;
#65412 = CARTESIAN_POINT ( 'NONE',  ( 4.738696794244872557, -1.902450960283699199, -0.4786090228221794307 ) ) ;
#65413 = CARTESIAN_POINT ( 'NONE',  ( 1.955835763735654487, -0.6658547638305843952, 1.845409454533278648 ) ) ;
#65414 = CARTESIAN_POINT ( 'NONE',  ( 10.01963921569910632, 11.64833282552586091, 1.199719254218450271 ) ) ;
#65415 = CARTESIAN_POINT ( 'NONE',  ( 1.596166908135342233, 1.206333752204394871, 1.472837400516055606 ) ) ;
#65416 = ORIENTED_EDGE ( 'NONE', *, *, #105983, .T. ) ;
#65417 = CARTESIAN_POINT ( 'NONE',  ( 0.3568547849697421004, -1.996003273109921983, -0.7069239421778094057 ) ) ;
#65419 = CARTESIAN_POINT ( 'NONE',  ( -8.179646747746328828, 8.437342715325849341, -0.7998128361456291469 ) ) ;
#65418 = CARTESIAN_POINT ( 'NONE',  ( -5.786632634934295361, 5.645492917045106473, 0.7998128361456341429 ) ) ;
#65420 = CARTESIAN_POINT ( 'NONE',  ( 0.5679803739370090643, -1.732728882149033645, -0.6228371021387222317 ) ) ;
#65421 = ORIENTED_EDGE ( 'NONE', *, *, #71349, .T. ) ;
#65422 = CARTESIAN_POINT ( 'NONE',  ( 3.784171691162826701, -1.288926714175726129, -1.746948845794197958 ) ) ;
#65423 = CARTESIAN_POINT ( 'NONE',  ( 1.474414414893375769, 7.826756755319755676, -10.64843978026286386 ) ) ;
#65424 = CARTESIAN_POINT ( 'NONE',  ( 2.057031522680652369, 0.4693188842763912905, 2.067847215655476134 ) ) ;
#65425 = CARTESIAN_POINT ( 'NONE',  ( -0.7500000000000006661, 2.639583334016156080, -1.299038105676652011 ) ) ;
#65426 = CARTESIAN_POINT ( 'NONE',  ( 9.264299036839600987, 9.702770385934682551, -0.7998128361456281477 ) ) ;
#65427 = CARTESIAN_POINT ( 'NONE',  ( 6.548892101489681927, 6.803534504848940401, 0.4251794856353352525 ) ) ;
#65428 = CARTESIAN_POINT ( 'NONE',  ( 2.161468745749118625, 0.3553341821136410950, -2.029755476197503850 ) ) ;
#65430 = CARTESIAN_POINT ( 'NONE',  ( 1.464175926609780964E-14, -2.537500000000001865, -3.475000000000000533 ) ) ;
#65429 = CARTESIAN_POINT ( 'NONE',  ( -8.259941899223614215, 10.65968485389279508, -1.599625672291263179 ) ) ;
#65431 = CARTESIAN_POINT ( 'NONE',  ( -0.6823417656250212460, 2.801041667008084879, 1.181850606188767472 ) ) ;
#65432 = CARTESIAN_POINT ( 'NONE',  ( -0.02244404828157658613, 0.6916080914694566761, -2.270927585766496559 ) ) ;
#65433 = CARTESIAN_POINT ( 'NONE',  ( 5.233030847706650057, 1.768443763404730307, 0.7281017474275592871 ) ) ;
#65434 = CARTESIAN_POINT ( 'NONE',  ( -3.728129053633564283, 7.293308295973763400, 0.7216878364870122908 ) ) ;
#65435 = CARTESIAN_POINT ( 'NONE',  ( 1.599281762659544137, 1.849886183345637258, -1.302228464298058830 ) ) ;
#65436 = CARTESIAN_POINT ( 'NONE',  ( -9.869972641068651242, 11.57768483841065787, 1.082531754730558626 ) ) ;
#65437 = CARTESIAN_POINT ( 'NONE',  ( 1.722643027415799999, 1.340613184126436597, -1.218586174478804907 ) ) ;
#65438 = EDGE_CURVE ( 'NONE', #163559, #194999, #169723, .T. ) ;
#65439 = CARTESIAN_POINT ( 'NONE',  ( 1.674859764755828095, 1.664904793830531027, -0.9475745862929999541 ) ) ;
#65440 = CARTESIAN_POINT ( 'NONE',  ( 3.104029480343179603, 0.7476448069429382226, -1.930825944200013966 ) ) ;
#65441 = CARTESIAN_POINT ( 'NONE',  ( -0.6823417656250212460, 1.363541667008083547, 1.181850606188755259 ) ) ;
#65442 = CARTESIAN_POINT ( 'NONE',  ( 1.112115884188523918, -0.8845927946041342027, -1.761928416731074476 ) ) ;
#65443 = CARTESIAN_POINT ( 'NONE',  ( 5.830678075864223153, 1.857343136638961445, 0.5113247108688694365 ) ) ;
#65445 = CARTESIAN_POINT ( 'NONE',  ( 6.053075614097062740, 7.042710966267798689, -1.019147762646470001 ) ) ;
#65444 = CARTESIAN_POINT ( 'NONE',  ( 0.6457025891282016650, -1.976290545051001768, 1.191322501153786906 ) ) ;
#65446 = EDGE_CURVE ( 'NONE', #103667, #1071, #4492, .T. ) ;
#65447 = CARTESIAN_POINT ( 'NONE',  ( 1.364683531249986537, 1.405208333674755838, -0.7879004041258239610 ) ) ;
#65448 = CARTESIAN_POINT ( 'NONE',  ( 5.670399732568969675, -0.9243551164253935859, -1.844019960785907797 ) ) ;
#65449 = CARTESIAN_POINT ( 'NONE',  ( -6.033542053281340856, 6.997886136038390603, -1.199719254218446718 ) ) ;
#65450 = CARTESIAN_POINT ( 'NONE',  ( 6.252281394196331554, 10.44607872653774372, 1.040834085586084257E-14 ) ) ;
#65451 = CARTESIAN_POINT ( 'NONE',  ( -1.000000000000017097, 8.600000000000013856, 0.4000000000000026867 ) ) ;
#65453 = CARTESIAN_POINT ( 'NONE',  ( 0.7499999999999920064, 5.733333333333353821, 1.299038105676669330 ) ) ;
#65452 = CARTESIAN_POINT ( 'NONE',  ( 6.405314555823123257, 1.748765893162683271, 1.173091541056320297 ) ) ;
#65454 = CARTESIAN_POINT ( 'NONE',  ( 1.364683531249986537, 2.217708333674751398, -0.7879004041258239610 ) ) ;
#65455 = CARTESIAN_POINT ( 'NONE',  ( 4.640002929648442631, 0.9288797265196678810, -1.951996720969489951 ) ) ;
#65456 = CARTESIAN_POINT ( 'NONE',  ( 5.408855464265644564, -0.4929012147626107843, -1.958461550952787844 ) ) ;
#65457 = FACE_OUTER_BOUND ( 'NONE', #146408, .T. ) ;
#65458 = CARTESIAN_POINT ( 'NONE',  ( -6.236387472606166327, 6.378132927569716060, -0.7216878364870278340 ) ) ;
#65459 = EDGE_CURVE ( 'NONE', #163739, #49626, #191276, .T. ) ;
#65462 = CARTESIAN_POINT ( 'NONE',  ( 4.744990575102895569, 5.598539094783909320, -1.082531754730548412 ) ) ;
#65461 = CARTESIAN_POINT ( 'NONE',  ( -3.285556943750000070, -1.509374999522042238, 0.000000000000000000 ) ) ;
#65460 = CARTESIAN_POINT ( 'NONE',  ( 7.686546744304875389, 7.932335721302671949, 0.7998128361456291469 ) ) ;
#65463 = CARTESIAN_POINT ( 'NONE',  ( -4.685224601974262271, 7.623789914682047808, -1.199719254218453823 ) ) ;
#65464 = CARTESIAN_POINT ( 'NONE',  ( 3.731657894805060938, 0.6748485617756972976, -1.900415309456899182 ) ) ;
#65465 = CARTESIAN_POINT ( 'NONE',  ( -8.474009703741204547, 9.845098394908269768, -1.199719254218446718 ) ) ;
#65467 = CARTESIAN_POINT ( 'NONE',  ( -6.238160075619175515, 10.29195416494877513, 0.000000000000000000 ) ) ;
#65466 = CARTESIAN_POINT ( 'NONE',  ( -4.223528545856940042, 4.886203710709899006, -1.199719254218446718 ) ) ;
#65468 = CARTESIAN_POINT ( 'NONE',  ( -0.6823417656249969321, 4.967708333674755394, -1.181850606188749264 ) ) ;
#65470 = CARTESIAN_POINT ( 'NONE',  ( 0.6823417656249934904, 9.942708333674735499, 1.181850606188764807 ) ) ;
#65469 = CARTESIAN_POINT ( 'NONE',  ( 4.663041391408608405, -1.929494027986548454, -0.9748474430888448561 ) ) ;
#65471 = SURFACE_STYLE_FILL_AREA ( #16725 ) ;
#65473 = CARTESIAN_POINT ( 'NONE',  ( -11.51744110290411882, 7.078546551862022085, -3.212469843298280114 ) ) ;
#65472 = B_SPLINE_CURVE_WITH_KNOTS ( 'NONE', 3,
 ( #67368, #99912, #96742, #200578, #212577, #162790, #49037, #134578, #66304, #64216 ),
 .UNSPECIFIED., .F., .F.,
 ( 4, 2, 2, 2, 4 ),
 ( 0.000000000000000000, 0.0002503535593264579048, 0.0005007071186529158096, 0.0007510606779793737144, 0.001001414237305831619 ),
 .UNSPECIFIED. ) ;
#65475 = CARTESIAN_POINT ( 'NONE',  ( 6.011342256177334420, -1.897693555989588887, 0.6820111564242032909 ) ) ;
#65474 = CARTESIAN_POINT ( 'NONE',  ( -7.497295758232724872, 9.769931022736756177, -1.443375672974058777 ) ) ;
#65476 = CARTESIAN_POINT ( 'NONE',  ( -1.499999999999997780, 5.900000000000023448, 1.214306433183764966E-14 ) ) ;
#65477 = CARTESIAN_POINT ( 'NONE',  ( 0.6446037793155032780, -1.481899804082789984, 0.8824728545121940382 ) ) ;
#65478 = CARTESIAN_POINT ( 'NONE',  ( 3.250922972226694352, 7.014770244231638863, 0.7998128361456281477 ) ) ;
#65480 = CARTESIAN_POINT ( 'NONE',  ( 5.722423353419669567, 8.833855124701747386, 1.199719254218451159 ) ) ;
#65479 = CARTESIAN_POINT ( 'NONE',  ( 6.941411460516762943, 11.04213777067082702, -0.7216878364870267237 ) ) ;
#65481 =( GEOMETRIC_REPRESENTATION_CONTEXT ( 3 ) GLOBAL_UNCERTAINTY_ASSIGNED_CONTEXT ( ( #12623 ) ) GLOBAL_UNIT_ASSIGNED_CONTEXT ( ( #103543, #197829, #100337 ) ) REPRESENTATION_CONTEXT ( 'NONE', 'WORKASPACE' ) );
#65482 = FACE_OUTER_BOUND ( 'NONE', #212336, .T. ) ;
#65483 = CARTESIAN_POINT ( 'NONE',  ( 6.626239551081194001, 1.076695052409048614, -1.529385127534782951 ) ) ;
#65484 = CARTESIAN_POINT ( 'NONE',  ( 0.8736902326584498057, 0.3905749221770152269, -1.974679160882378826 ) ) ;
#65485 =( NAMED_UNIT ( * ) SI_UNIT ( $, .STERADIAN. ) SOLID_ANGLE_UNIT ( ) );
#65486 = CARTESIAN_POINT ( 'NONE',  ( 4.324687812634897988, 4.147816657603229373, 0.7216878364870317197 ) ) ;
#65487 = CARTESIAN_POINT ( 'NONE',  ( 3.452368941479638131, 2.206952907609287973, 0.002057427529567057434 ) ) ;
#65488 = CARTESIAN_POINT ( 'NONE',  ( -5.709392084686210289, 8.714688961225625974, 1.082531754730550855 ) ) ;
#65489 = VERTEX_POINT ( 'NONE', #40054 ) ;
#65490 = CARTESIAN_POINT ( 'NONE',  ( 8.053180056393003383, 12.33920113252646367, 1.040834085586084257E-14 ) ) ;
#65492 = CARTESIAN_POINT ( 'NONE',  ( 2.179314750421776026, 1.560514648525725745, 1.277027416600539533 ) ) ;
#65491 = CARTESIAN_POINT ( 'NONE',  ( 2.069135417989849568, -1.637292086295978111, 1.347470637625711731 ) ) ;
#65494 = VERTEX_POINT ( 'NONE', #171105 ) ;
#65493 = CARTESIAN_POINT ( 'NONE',  ( 2.390610142633019741, -1.734584137932100312, -0.5226098844451251280 ) ) ;
#65495 = CARTESIAN_POINT ( 'NONE',  ( 7.014364370223726830, 9.276787413384745662, -1.599625672291269396 ) ) ;
#65496 = CARTESIAN_POINT ( 'NONE',  ( 5.262536180398716290, 9.291375977107183104, -0.7998128361456291469 ) ) ;
#65498 = CARTESIAN_POINT ( 'NONE',  ( 0.4971116367980681350, -0.2779505141972256066, 1.895288638825567862 ) ) ;
#65497 = CARTESIAN_POINT ( 'NONE',  ( -5.590039407536138150, 5.416134151747256986, 0.000000000000000000 ) ) ;
#65499 = CARTESIAN_POINT ( 'NONE',  ( 1.843739406749204335, 8.920000000000001705, 0.7750000000000004663 ) ) ;
#65500 = CARTESIAN_POINT ( 'NONE',  ( 1.500000000000007105, 10.64264068711930733, 1.214306433183764966E-14 ) ) ;
#65501 = CARTESIAN_POINT ( 'NONE',  ( 4.975479186090847605, 7.788180902872553268, 1.082531754730558626 ) ) ;
#65502 = EDGE_CURVE ( 'NONE', #114534, #25627, #167039, .T. ) ;
#65503 = CARTESIAN_POINT ( 'NONE',  ( -1.402160292154681736E-14, -0.2406249996585799189, -1.575800808251665908 ) ) ;
#65504 = CARTESIAN_POINT ( 'NONE',  ( 3.469446951953614189E-15, 8.900000000000019895, 1.214306433183764966E-14 ) ) ;
#65505 = CARTESIAN_POINT ( 'NONE',  ( -8.676328237741483207, 12.20980114641871062, -1.199719254218446718 ) ) ;
#65506 = CARTESIAN_POINT ( 'NONE',  ( 3.608425205800522839, -0.8741791752944136906, -1.977237025433141504 ) ) ;
#65507 = EDGE_CURVE ( 'NONE', #82527, #74942, #208592, .T. ) ;
#65508 = CARTESIAN_POINT ( 'NONE',  ( -4.665414256878287702, 8.457084043084382330, -0.7216878364870338292 ) ) ;
#65509 = CARTESIAN_POINT ( 'NONE',  ( 5.777182853198898904, 6.873039762554409293, -1.082531754730548412 ) ) ;
#65510 = CARTESIAN_POINT ( 'NONE',  ( 2.426173717206762781, -2.096881089210366422, 0.3156149858808757203 ) ) ;
#65511 = CARTESIAN_POINT ( 'NONE',  ( 6.510779352739587189, 1.350450193652263930, -1.228632259304612839 ) ) ;
#65512 = CARTESIAN_POINT ( 'NONE',  ( 3.145733524295030836, 0.7127697582950813793, -1.838151395584181058 ) ) ;
#65513 = CARTESIAN_POINT ( 'NONE',  ( 5.941656858135131891, -1.798430535887390658, 0.6506349336675710804 ) ) ;
#65514 = EDGE_LOOP ( 'NONE', ( #77859, #119841, #103014, #33019, #179984, #114772, #126425, #25568 ) ) ;
#65515 = B_SPLINE_CURVE_WITH_KNOTS ( 'NONE', 3,
 ( #30775, #28629, #126207, #96854, #13429, #145624 ),
 .UNSPECIFIED., .F., .F.,
 ( 4, 2, 4 ),
 ( 0.000000000000000000, 0.5000000000000000000, 1.000000000000000000 ),
 .UNSPECIFIED. ) ;
#65516 = CARTESIAN_POINT ( 'NONE',  ( -1.115562610750309283E-14, 9.343750000682799595, 1.500000000000001554 ) ) ;
#65517 = CARTESIAN_POINT ( 'NONE',  ( 6.496546994228061145, 1.947915994809066076, 0.2903317952503216559 ) ) ;
#65518 = CARTESIAN_POINT ( 'NONE',  ( 1.658044662407763381, -1.373417096361102097, 1.373162012216273320 ) ) ;
#65519 = ORIENTED_EDGE ( 'NONE', *, *, #90049, .T. ) ;
#65520 = CARTESIAN_POINT ( 'NONE',  ( -5.008811405605897882, 4.808311159487113073, 0.7998128361456281477 ) ) ;
#65522 = CARTESIAN_POINT ( 'NONE',  ( 1.834945990282811579, 2.515477056191848249, -2.498594247320889306 ) ) ;
#65521 = CARTESIAN_POINT ( 'NONE',  ( -6.617788377246196951, 7.853746207276256719, -1.082531754730549967 ) ) ;
#65524 = CARTESIAN_POINT ( 'NONE',  ( 7.983053520348166288, 8.207983950027992748, -0.7998128361456281477 ) ) ;
#65523 = CARTESIAN_POINT ( 'NONE',  ( 2.589882131170073709, -2.085102945988726031, -0.1528390284690275547 ) ) ;
#65526 = CARTESIAN_POINT ( 'NONE',  ( 4.190878879955609371, 7.903459436674603822, -0.7216878364870338292 ) ) ;
#65525 = CARTESIAN_POINT ( 'NONE',  ( 5.947222937888848371, 10.09017719417900416, 1.040834085586084257E-14 ) ) ;
#65528 = ORIENTED_EDGE ( 'NONE', *, *, #2128, .T. ) ;
#65527 = CARTESIAN_POINT ( 'NONE',  ( 5.619756671179353624, -0.4603523440993940175, 1.855926886426212175 ) ) ;
#65529 = CARTESIAN_POINT ( 'NONE',  ( 4.248781725523794073, 0.5872999373685274804, 2.127227798101683387 ) ) ;
#65530 = CARTESIAN_POINT ( 'NONE',  ( 1.536444635327537833, 1.086998388645914027, -1.920427013416255768 ) ) ;
#65531 = FACE_OUTER_BOUND ( 'NONE', #2985, .T. ) ;
#65532 = CARTESIAN_POINT ( 'NONE',  ( 0.06490398442321809735, -1.535895564731554863, 1.139000086266952483 ) ) ;
#65533 = CARTESIAN_POINT ( 'NONE',  ( -10.56536251450128994, 12.34038937450521800, 3.404319718479181578 ) ) ;
#65534 = CARTESIAN_POINT ( 'NONE',  ( 11.55950211276791784, 13.80000000000000071, -3.221476510067116550 ) ) ;
#65535 = CARTESIAN_POINT ( 'NONE',  ( 3.824723168590526523, -1.392635068473629500, 1.532133406949770960 ) ) ;
#65537 = CARTESIAN_POINT ( 'NONE',  ( 2.290102563249151402, -0.9248296759884739870, 1.954025333243500917 ) ) ;
#65536 = CARTESIAN_POINT ( 'NONE',  ( -2.981903720001798597, 5.566305875722335372, -1.199719254218446718 ) ) ;
#65538 = CARTESIAN_POINT ( 'NONE',  ( 3.175498511859841333, 1.392037702009111033, 1.692654053968026151 ) ) ;
#65539 = CARTESIAN_POINT ( 'NONE',  ( -5.886439722289627419, 6.118937485343679761, -0.7679415244158314113 ) ) ;
#65540 = SURFACE_STYLE_FILL_AREA ( #15733 ) ;
#65541 = AXIS2_PLACEMENT_3D ( 'NONE', #31946, #212802, #195510 ) ;
#65542 = CARTESIAN_POINT ( 'NONE',  ( -8.012344526598182026E-15, 14.60937500034139980, -1.575800808251669460 ) ) ;
#65543 = CARTESIAN_POINT ( 'NONE',  ( -5.276058054373441664, 6.184431147304315424, -1.199719254218453823 ) ) ;
#65544 = UNCERTAINTY_MEASURE_WITH_UNIT (LENGTH_MEASURE( 1.000000000000000082E-05 ), #116330, 'distance_accuracy_value', 'NONE');
#65545 = CARTESIAN_POINT ( 'NONE',  ( 6.592404480832670721, -0.3601991968599608795, 1.702173051257379832 ) ) ;
#65546 = CARTESIAN_POINT ( 'NONE',  ( -9.246297574839990929, 11.81043314211192019, 1.443375672974076540 ) ) ;
#65547 = CARTESIAN_POINT ( 'NONE',  ( 4.926661076633905623, -1.356332079400805135, 1.564123780295342492 ) ) ;
#65548 = CARTESIAN_POINT ( 'NONE',  ( 6.028941913163482269, -1.788401068206580957, 1.133005349186385402 ) ) ;
#65549 = CARTESIAN_POINT ( 'NONE',  ( 4.788000803920411386, 8.737751371215816576, 1.040834085586084257E-14 ) ) ;
#65550 = CARTESIAN_POINT ( 'NONE',  ( 9.518502046417468776, 4.418053365869078597, 7.307953274077197747 ) ) ;
#65551 = CARTESIAN_POINT ( 'NONE',  ( 3.643367292660666390, 1.782436080146361013, -0.8378801856493125477 ) ) ;
#65552 = CARTESIAN_POINT ( 'NONE',  ( 5.841781729209135854, 2.289337533263948288, 0.1180171966539828449 ) ) ;
#65553 = CARTESIAN_POINT ( 'NONE',  ( 3.299243935302543118, 1.439784963707075649, 1.122460502641378755 ) ) ;
#65554 = CARTESIAN_POINT ( 'NONE',  ( 8.014278199453778839, 8.522615118883788199, 0.000000000000000000 ) ) ;
#65555 = CARTESIAN_POINT ( 'NONE',  ( 4.568734577680873876, 6.353276312092901890, -1.443375672974051449 ) ) ;
#65556 = CARTESIAN_POINT ( 'NONE',  ( -7.867809214632013770, 8.073532260025807261, 1.040834085586084257E-14 ) ) ;
#65557 = CARTESIAN_POINT ( 'NONE',  ( 4.844006021832467646, 8.873367135438366304, 0.000000000000000000 ) ) ;
#65558 = ORIENTED_EDGE ( 'NONE', *, *, #139460, .T. ) ;
#65559 = CARTESIAN_POINT ( 'NONE',  ( 3.849861664782163739, -1.391318219759619002, -1.455273641467175860 ) ) ;
#65560 = CARTESIAN_POINT ( 'NONE',  ( 0.1932713599902321500, -1.417659354009516148, -1.810318517150938389 ) ) ;
#65561 = CARTESIAN_POINT ( 'NONE',  ( 4.944172655442597986, -0.9282843415348587257, 1.728263438747809078 ) ) ;
#65562 = CARTESIAN_POINT ( 'NONE',  ( -6.555530967407501741, 7.606873202518897870, 1.199719254218450271 ) ) ;
#65563 = CARTESIAN_POINT ( 'NONE',  ( -3.086452525405351643, 6.752611712948207057, 0.7998128361456341429 ) ) ;
#65564 = CARTESIAN_POINT ( 'NONE',  ( -7.787098537122150610, -5.543994141378503215, 7.698131257602418565 ) ) ;
#65565 = CARTESIAN_POINT ( 'NONE',  ( -6.123442655227560927, 7.173046514967467147, 1.199719254218452047 ) ) ;
#65567 = CARTESIAN_POINT ( 'NONE',  ( 6.016413156365523207, 1.185731173915012038, -1.314077388775713784 ) ) ;
#65566 = CARTESIAN_POINT ( 'NONE',  ( 0.5387614761330473678, -1.791220285616751173, 1.078087367808887365 ) ) ;
#65568 = CARTESIAN_POINT ( 'NONE',  ( 1.400751299550835549, 7.315968950352074174, -4.333496285527503211 ) ) ;
#65569 = CARTESIAN_POINT ( 'NONE',  ( 1.447511513890851864, 0.6336015447323711802, -2.097855558553712196 ) ) ;
#65570 = CARTESIAN_POINT ( 'NONE',  ( 0.9600616587607477825, -1.572830678042375974, -0.7454570610717390355 ) ) ;
#65571 = CARTESIAN_POINT ( 'NONE',  ( 5.937581207780954884, 9.014596278131406848, -1.199719254218440723 ) ) ;
#65572 = CARTESIAN_POINT ( 'NONE',  ( -3.314994193297896796, 6.393354490853021765, -0.7784788408506218005 ) ) ;
#65573 = CARTESIAN_POINT ( 'NONE',  ( 1.435739417030171605, 0.8527202394775310612, -1.499263083578871836 ) ) ;
#65574 = CARTESIAN_POINT ( 'NONE',  ( 1.628746693258641853, 0.2190750365392846177, 2.180598679842937759 ) ) ;
#65575 = CARTESIAN_POINT ( 'NONE',  ( 4.073040751519330094, -2.058760688187323495, -0.7953439701907027981 ) ) ;
#65576 = CARTESIAN_POINT ( 'NONE',  ( 1.920994505713587541, -1.537477318048833475, 1.533119463567463203 ) ) ;
#65577 = LINE ( 'NONE', #64549, #200122 ) ;
#65578 = CARTESIAN_POINT ( 'NONE',  ( 2.097004163592118164, 1.893647498693065589, 0.9473067498170744116 ) ) ;
#65579 = CARTESIAN_POINT ( 'NONE',  ( 6.722000117219828930, -7.189371949512757709, -6.713552092916842184 ) ) ;
#65580 = ORIENTED_EDGE ( 'NONE', *, *, #143009, .F. ) ;
#65582 = CARTESIAN_POINT ( 'NONE',  ( 1.364683531249986537, 0.4260416670080872659, 0.7879004041258500513 ) ) ;
#65581 = CARTESIAN_POINT ( 'NONE',  ( 2.314399336204819857, 1.494381390340574489, -1.738437040929841082 ) ) ;
#65583 = CARTESIAN_POINT ( 'NONE',  ( -11.80247861663003484, 12.30000000000000071, -1.695431928471868632 ) ) ;
#65584 = CARTESIAN_POINT ( 'NONE',  ( 6.003563092752934871, 5.898578451166879510, 0.7998128361456341429 ) ) ;
#65585 = CARTESIAN_POINT ( 'NONE',  ( 4.477308758892056595, -1.984000869926884736, -0.9990560778978144763 ) ) ;
#65586 = CARTESIAN_POINT ( 'NONE',  ( -6.060131475628484310, 10.01397778830115470, 0.000000000000000000 ) ) ;
#65587 = CARTESIAN_POINT ( 'NONE',  ( 0.03969736035583037309, -7.921780080556623638, -11.00000000000012967 ) ) ;
#65588 = CARTESIAN_POINT ( 'NONE',  ( 5.666945020832181434, 5.713783400500082266, 0.7216878364870317197 ) ) ;
#65589 = CARTESIAN_POINT ( 'NONE',  ( -8.310784975052689205, 8.798263347090697906, -0.7216878364870267237 ) ) ;
#65590 = CARTESIAN_POINT ( 'NONE',  ( 4.421367491832270957, 6.251624388594711590, 1.443375672974058777 ) ) ;
#65591 = ORIENTED_EDGE ( 'NONE', *, *, #17510, .F. ) ;
#65592 = CARTESIAN_POINT ( 'NONE',  ( 3.199842427594956185, 1.824118962040650604, 0.8596310190432245868 ) ) ;
#65594 = CARTESIAN_POINT ( 'NONE',  ( 0.7079710255328255375, 0.6504495457556063176, -1.957355765043818696 ) ) ;
#65593 = CARTESIAN_POINT ( 'NONE',  ( 6.938021921891177612, 9.117444880338284818, -1.599625672291262513 ) ) ;
#65595 = CARTESIAN_POINT ( 'NONE',  ( -11.92051736251533534, 13.65180243792676862, 1.381800029228856808 ) ) ;
#65596 = CARTESIAN_POINT ( 'NONE',  ( 5.858531774436539052, 6.007577623030311287, 0.000000000000000000 ) ) ;
#65597 = CARTESIAN_POINT ( 'NONE',  ( 0.4019237886466816012, 8.707585450998170273, -1.499999999999998668 ) ) ;
#65598 = CARTESIAN_POINT ( 'NONE',  ( 1.364683531249988535, 3.363541667008084879, 0.7879004041258500513 ) ) ;
#65599 = CARTESIAN_POINT ( 'NONE',  ( 4.189532503254236318, -0.8396404696654431454, 2.024412170900617092 ) ) ;
#65600 = CARTESIAN_POINT ( 'NONE',  ( 1.740861508391436274, 2.010826320759526720, -0.1511413081683593562 ) ) ;
#65601 = CARTESIAN_POINT ( 'NONE',  ( 0.8898994657863326108, -0.4472179738511591895, -1.785967584704901912 ) ) ;
#65602 = CARTESIAN_POINT ( 'NONE',  ( 6.598014311344812199, 10.84943379654430906, 1.040834085586084257E-14 ) ) ;
#65603 = CARTESIAN_POINT ( 'NONE',  ( 5.614214418409627427, -0.8227427255552112184, -1.629729119005427496 ) ) ;
#65604 = CARTESIAN_POINT ( 'NONE',  ( 5.766250055133458119, 1.862018000461727052, -0.7743128548072516493 ) ) ;
#65605 = CARTESIAN_POINT ( 'NONE',  ( -7.121056995675673740, 9.330985799753529264, -1.599625672291263179 ) ) ;
#65607 = CARTESIAN_POINT ( 'NONE',  ( -5.281783360975562225, 8.319775133516907673, 1.199719254218452935 ) ) ;
#65606 = CARTESIAN_POINT ( 'NONE',  ( 4.118261297349164352, -1.160217402330826042, -1.942256231939092137 ) ) ;
#65608 = CARTESIAN_POINT ( 'NONE',  ( 0.6980488080095709202, -0.7561646473010454894, 1.965825473679798652 ) ) ;
#65609 = CARTESIAN_POINT ( 'NONE',  ( -6.720001414228860881, 7.869031733802326123, -1.199719254218452047 ) ) ;
#65610 = CARTESIAN_POINT ( 'NONE',  ( 5.143061708805018561, -0.2499388813127951525, -2.055141626981969338 ) ) ;
#65611 = CARTESIAN_POINT ( 'NONE',  ( 10.22692794340986921, 10.82583744360002243, 0.000000000000000000 ) ) ;
#65612 = PRESENTATION_STYLE_ASSIGNMENT (( #16872 ) ) ;
#65613 = B_SPLINE_CURVE_WITH_KNOTS ( 'NONE', 3,
 ( #33388, #1931, #200141, #35516, #137317, #188171, #102670, #56052 ),
 .UNSPECIFIED., .F., .F.,
 ( 4, 2, 2, 4 ),
 ( 4.051276326462483916E-18, 0.0002224730689913823186, 0.0004449461379827605715, 0.0008898922759655192999 ),
 .UNSPECIFIED. ) ;
#65614 = SHAPE_DEFINITION_REPRESENTATION ( #206145, #149737 ) ;
#65615 = CARTESIAN_POINT ( 'NONE',  ( -7.018317073368468328, 11.33978701890523233, -0.7998128361456291469 ) ) ;
#65616 = CARTESIAN_POINT ( 'NONE',  ( 11.07790593930098311, 11.29999999999999893, 0.6999999999999992895 ) ) ;
#65617 = CARTESIAN_POINT ( 'NONE',  ( 5.840530312436913007, 10.03597880781023299, 0.000000000000000000 ) ) ;
#65618 = CARTESIAN_POINT ( 'NONE',  ( 4.439983357641082762, 7.074277023141499754, -1.114066652139956926 ) ) ;
#65619 = CARTESIAN_POINT ( 'NONE',  ( 2.589077643123653072, 1.706113014995232380, 1.074661422923957055 ) ) ;
#65620 = CARTESIAN_POINT ( 'NONE',  ( -9.978437869977950569, 11.70422760547153906, -1.082531754730539753 ) ) ;
#65622 = CARTESIAN_POINT ( 'NONE',  ( 2.215342456320268383, 1.781105875021117502, -1.327318755304232933 ) ) ;
#65621 = CARTESIAN_POINT ( 'NONE',  ( 0.3344391967911933272, -1.139684030083350841, -1.788147294700337397 ) ) ;
#65623 = CARTESIAN_POINT ( 'NONE',  ( -5.608135385276092677, 5.599224824533729716, 0.4022279080854191391 ) ) ;
#65625 = COLOUR_RGB ( '', 0.66274510, 0.83137255, 0.94901961) ;
#65624 = CARTESIAN_POINT ( 'NONE',  ( -6.994027139803241866, 9.253060644560830994, -1.599625672291271394 ) ) ;
#65626 = CARTESIAN_POINT ( 'NONE',  ( 5.799137018343234473, 7.788745826199009237, -1.599625672291262513 ) ) ;
#65627 = CARTESIAN_POINT ( 'NONE',  ( 3.279693232472491893, -1.891448704997201302, 0.5207070127687256633 ) ) ;
#65628 = CARTESIAN_POINT ( 'NONE',  ( 4.638861114170084399, 8.563755066507100722, 0.7998128361456462443 ) ) ;
#65630 =( BOUNDED_CURVE ( )  B_SPLINE_CURVE ( 2, ( #66737, #55597, #31103, #64647, #116651, #33209, #83016 ),
 .UNSPECIFIED., .F., .T. ) 
 B_SPLINE_CURVE_WITH_KNOTS ( ( 3, 2, 2, 3 ),
 ( 0.3500000000000000888, 0.3583333333333333925, 0.3666666666666665853, 0.3749999999999998890 ),
 .UNSPECIFIED. ) 
 CURVE ( )  GEOMETRIC_REPRESENTATION_ITEM ( )  RATIONAL_B_SPLINE_CURVE ( ( 0.9999999999999982236, 0.8660254037844404840, 1.000000000000000000, 0.8660254037844387076, 1.000000000000000000, 0.8660254037844404840, 0.9999999999999982236 ) ) 
 REPRESENTATION_ITEM ( '' )  );
#65629 = CARTESIAN_POINT ( 'NONE',  ( -4.014146127519945928, 7.627013291057631150, 0.008764090477326666462 ) ) ;
#65631 = CARTESIAN_POINT ( 'NONE',  ( 3.684065054611349144, 5.321161868511784299, -1.599625672291262513 ) ) ;
#65632 = CARTESIAN_POINT ( 'NONE',  ( -6.305950844131887223, 6.529566537674873494, 0.000000000000000000 ) ) ;
#65633 = CARTESIAN_POINT ( 'NONE',  ( -8.053180056837398126, 8.497724275839514618, 0.7216878364870578100 ) ) ;
#65634 = CARTESIAN_POINT ( 'NONE',  ( 1.828540510153942922, -1.004066958311781832, -1.867862179375394005 ) ) ;
#65635 = CARTESIAN_POINT ( 'NONE',  ( -5.529746549527323474, 7.544733289238903851, -1.599625672291271394 ) ) ;
#65636 = CARTESIAN_POINT ( 'NONE',  ( 6.004347769543215030, 1.959566550440184907, 0.09775035808561728656 ) ) ;
#65637 = CARTESIAN_POINT ( 'NONE',  ( 2.887745953747706373, 1.527789104365802286, 1.529575784674996886 ) ) ;
#65638 = CARTESIAN_POINT ( 'NONE',  ( 2.419273308677453826, -1.061688697878185206, -1.504126257600538974 ) ) ;
#65639 = CARTESIAN_POINT ( 'NONE',  ( -4.029167574269930441, 7.605081013511371779, 0.2528308249854539502 ) ) ;
#65640 = CARTESIAN_POINT ( 'NONE',  ( 1.364683531249986981, -1.053124999658580752, 0.000000000000000000 ) ) ;
#65641 = CARTESIAN_POINT ( 'NONE',  ( 5.015436155323918399, -0.9350583589616268121, -1.467585299639478702 ) ) ;
#65642 = CYLINDRICAL_SURFACE ( 'NONE', #70352, 0.08000000000000020983 ) ;
#65643 = CARTESIAN_POINT ( 'NONE',  ( 5.178851490740205676, 6.104710163027444736, 1.082531754730558626 ) ) ;
#65644 = DIRECTION ( 'NONE',  ( 0.000000000000000000, 1.000000000000000000, 0.000000000000000000 ) ) ;
#65645 = CARTESIAN_POINT ( 'NONE',  ( 2.026462046419864826, 1.244889377058140845, -1.767065586814352773 ) ) ;
#65647 = EDGE_CURVE ( 'NONE', #107270, #6713, #68797, .T. ) ;
#65646 = VECTOR ( 'NONE', #61125, 1000.000000000000000 ) ;
#65648 = CARTESIAN_POINT ( 'NONE',  ( 4.306017418194902469, -1.755500069608874281, 0.9912479507018998603 ) ) ;
#65649 = CARTESIAN_POINT ( 'NONE',  ( -7.809133291347029271, 12.05447990663947877, 0.000000000000000000 ) ) ;
#65650 = CARTESIAN_POINT ( 'NONE',  ( 1.042116488573753497, 0.8753402851892390091, -1.976733581976031218 ) ) ;
#65651 = CARTESIAN_POINT ( 'NONE',  ( 2.495336804025758859, 1.521579944813663099, 1.253379492226768477 ) ) ;
#65652 = CARTESIAN_POINT ( 'NONE',  ( -6.504227504688391726, 6.823496289112537916, 0.6761912409562121917 ) ) ;
#65653 = CARTESIAN_POINT ( 'NONE',  ( 3.122533544175498221, 0.05045625456868290531, 1.941573572215535393 ) ) ;
#65656 = ORIENTED_EDGE ( 'NONE', *, *, #211661, .F. ) ;
#65655 = CARTESIAN_POINT ( 'NONE',  ( -5.329763783947941036, 5.390681634126922361, 0.000000000000000000 ) ) ;
#65654 = CARTESIAN_POINT ( 'NONE',  ( -2.580963302752292243, 0.4788041664876945269, 0.000000000000000000 ) ) ;
#65657 = CARTESIAN_POINT ( 'NONE',  ( -4.136646265500970365, 5.919449624541475607, -1.443375672974066548 ) ) ;
#65658 = CARTESIAN_POINT ( 'NONE',  ( 3.573456005653643519, 6.326726552307992080, -1.199719254218453823 ) ) ;
#65660 = ORIENTED_EDGE ( 'NONE', *, *, #199073, .T. ) ;
#65659 = CARTESIAN_POINT ( 'NONE',  ( -6.818824913030298696, 6.919993584815607335, 0.7998128361456341429 ) ) ;
#65661 = CARTESIAN_POINT ( 'NONE',  ( -9.991996023147281747, 11.72004545083573568, 1.082531754730558626 ) ) ;
#65662 = CARTESIAN_POINT ( 'NONE',  ( 1.237671066534186792, -1.994493743981802680, 0.9446329514863486265 ) ) ;
#65663 = CARTESIAN_POINT ( 'NONE',  ( -1.642778471875000035, -2.967708332855374831, -2.845375778867859751 ) ) ;
#65664 = CARTESIAN_POINT ( 'NONE',  ( 5.278158119090741174, -1.046208158741080529, -1.659298866772864534 ) ) ;
#65665 = ORIENTED_EDGE ( 'NONE', *, *, #156299, .F. ) ;
#65666 = CARTESIAN_POINT ( 'NONE',  ( 3.626253288856711610, 2.107507776945900524, 0.2035006255925037866 ) ) ;
#65667 = CARTESIAN_POINT ( 'NONE',  ( -1.500000000000011324, 3.452083334016151639, 0.8660254037844403729 ) ) ;
#65668 = CARTESIAN_POINT ( 'NONE',  ( 0.1745949693968328886, 2.059235863126197774, -2.173049245862024303 ) ) ;
#65669 = CARTESIAN_POINT ( 'NONE',  ( 4.294743845541324490, 1.480121740587354573, 1.094796260939827404 ) ) ;
#65670 = ORIENTED_EDGE ( 'NONE', *, *, #126069, .T. ) ;
#65671 = UNCERTAINTY_MEASURE_WITH_UNIT (LENGTH_MEASURE( 1.000000000000000082E-05 ), #151307, 'distance_accuracy_value', 'NONE');
#65672 = CARTESIAN_POINT ( 'NONE',  ( -7.472515219426274946, 11.86968485597268064, 0.000000000000000000 ) ) ;
#65673 = SURFACE_STYLE_FILL_AREA ( #51601 ) ;
#65674 = CARTESIAN_POINT ( 'NONE',  ( 5.625269520628737752, 1.871107552910089122, 0.9978724776121964402 ) ) ;
#65675 = DIRECTION ( 'NONE',  ( 0.000000000000000000, 0.000000000000000000, -1.000000000000000000 ) ) ;
#65676 = CARTESIAN_POINT ( 'NONE',  ( 5.612185521052973414, 8.634967976948757951, -1.199719254218440723 ) ) ;
#65677 = EDGE_CURVE ( 'NONE', #116404, #182073, #81879, .T. ) ;
#65678 = CARTESIAN_POINT ( 'NONE',  ( 5.641890011675567251, 0.8391073529228080252, -1.882412581722334943 ) ) ;
#65681 = CARTESIAN_POINT ( 'NONE',  ( 3.667381569930192597, 1.025862638139760419, 1.528780434079744843 ) ) ;
#65680 = CARTESIAN_POINT ( 'NONE',  ( 0.7130641938532373825, -1.569203791704287809, -1.000260708767531481 ) ) ;
#65679 = DIRECTION ( 'NONE',  ( 0.000000000000000000, -1.000000000000000000, -0.000000000000000000 ) ) ;
#65682 = CARTESIAN_POINT ( 'NONE',  ( 7.934546212495622086, 10.28005655271014795, -1.599625672291262513 ) ) ;
#65683 = PRESENTATION_STYLE_ASSIGNMENT (( #145941 ) ) ;
#65684 = CARTESIAN_POINT ( 'NONE',  ( -0.08000000000000714873, -6.134628647623513231, 10.91970695577494865 ) ) ;
#65685 = CARTESIAN_POINT ( 'NONE',  ( -0.1421055763938854355, -7.985988503423670615, -9.537847510268186113 ) ) ;
#65686 = CARTESIAN_POINT ( 'NONE',  ( 3.510573375967055654, -0.8941257848905452832, -2.017821460644920073 ) ) ;
#65687 = CARTESIAN_POINT ( 'NONE',  ( 4.692800188189328203, -0.4894541170284586462, -2.208696565397149314 ) ) ;
#65688 = CARTESIAN_POINT ( 'NONE',  ( -7.565086526745425033, 7.928281824065535055, 0.7216878364870317197 ) ) ;
#65689 = CARTESIAN_POINT ( 'NONE',  ( 4.711091175174894730, 1.502108783192051877, -1.012348896329213765 ) ) ;
#65690 = CARTESIAN_POINT ( 'NONE',  ( 5.577321932364699641, 1.455147452656019524, 1.246156846922679584 ) ) ;
#65691 = FACE_OUTER_BOUND ( 'NONE', #34476, .T. ) ;
#65692 = CARTESIAN_POINT ( 'NONE',  ( 6.666881909320486521, -1.711340306973156977, -0.7558587634414122292 ) ) ;
#65693 = CARTESIAN_POINT ( 'NONE',  ( 5.406657457964442415, 0.5403815791694633885, 1.780887135367102303 ) ) ;
#65694 = CARTESIAN_POINT ( 'NONE',  ( 2.535011536075336913, 5.133042487381361596, 0.9999999999999991118 ) ) ;
#65695 = CARTESIAN_POINT ( 'NONE',  ( 6.192257685097896314, -1.761771181780842577, -0.1690057029742654260 ) ) ;
#65696 = CARTESIAN_POINT ( 'NONE',  ( 0.1984543448181053105, 1.387095780679182377, -1.463931301963219855 ) ) ;
#65698 = CARTESIAN_POINT ( 'NONE',  ( 2.824945763694948653, 1.983238121251710950, 0.7091105908984902673 ) ) ;
#65697 = CARTESIAN_POINT ( 'NONE',  ( -2.928197990427299668, 6.360055388899728435, 1.040834085586084257E-14 ) ) ;
#65699 = CARTESIAN_POINT ( 'NONE',  ( 2.358755538653318773, 5.695705861830088423, 1.040834085586084257E-14 ) ) ;
#65701 = CARTESIAN_POINT ( 'NONE',  ( -8.642432853707342488, 12.17025653171218558, 1.199719254218462483 ) ) ;
#65700 = CARTESIAN_POINT ( 'NONE',  ( -3.197123283245616676, -0.9841229182759280159, 1.361626862150112860 ) ) ;
#65702 = CARTESIAN_POINT ( 'NONE',  ( -0.5000000000000386358, 3.949999999999988187, -0.4500000000000284883 ) ) ;
#65703 = CARTESIAN_POINT ( 'NONE',  ( 1.670181813679386007, 2.014099715005359670, -0.1526998803580876252 ) ) ;
#65704 = CARTESIAN_POINT ( 'NONE',  ( -1.201851678989727383E-14, 2.321875000341416584, 1.575800808251672791 ) ) ;
#65705 = CARTESIAN_POINT ( 'NONE',  ( 2.849184837166184536, 6.475799410002530898, 0.7998128361456362523 ) ) ;
#65706 = ADVANCED_FACE ( 'NONE', ( #205727 ), #57364, .F. ) ;
#65707 = CARTESIAN_POINT ( 'NONE',  ( 2.794378387653595475, -2.155598273342887339, -0.1620501260681943834 ) ) ;
#65708 = CARTESIAN_POINT ( 'NONE',  ( 6.620655732516647518, 0.007553340620044743381, 1.826407896915738238 ) ) ;
#65711 = CARTESIAN_POINT ( 'NONE',  ( -4.207966135563095733, 7.175396087857926375, 7.500000000000000000 ) ) ;
#65710 = CARTESIAN_POINT ( 'NONE',  ( 11.94105721237523277, 10.19999999999999929, -1.187919463087248939 ) ) ;
#65709 = CARTESIAN_POINT ( 'NONE',  ( 3.953084306836263995, 6.769626237021087789, 1.199719254218452047 ) ) ;
#65712 = CARTESIAN_POINT ( 'NONE',  ( 9.205623113554624481, 10.80261038964432707, 1.082531754730549967 ) ) ;
#65713 = CARTESIAN_POINT ( 'NONE',  ( -0.7500000000000215383, 3.972916667349481123, 1.299038105676671107 ) ) ;
#65714 = CARTESIAN_POINT ( 'NONE',  ( -8.202319746587722449, 8.671720580548228696, 1.040834085586084257E-14 ) ) ;
#65715 = CARTESIAN_POINT ( 'NONE',  ( -1.402160292154681736E-14, 0.9468750003414176941, -1.575800808251659024 ) ) ;
#65716 = CARTESIAN_POINT ( 'NONE',  ( 0.9256184737543894370, -1.394389637717853514, -1.690728713229103342 ) ) ;
#65717 = CARTESIAN_POINT ( 'NONE',  ( 0.1616376092238826501, 8.277406474726792140, 1.999409923707613945 ) ) ;
#65718 = CARTESIAN_POINT ( 'NONE',  ( 1.499281897245376527, 1.848817473390499844, -1.303928773892924609 ) ) ;
#65719 = CARTESIAN_POINT ( 'NONE',  ( -8.369460898337653276, 8.658792557682392754, 0.7998128361456462443 ) ) ;
#65720 = CARTESIAN_POINT ( 'NONE',  ( -4.731432421044883263, 5.582721248382882528, -1.082531754730543971 ) ) ;
#65721 = CARTESIAN_POINT ( 'NONE',  ( 0.6823417656249899377, 3.238541667008085323, -1.181850606188754593 ) ) ;
#65722 = CARTESIAN_POINT ( 'NONE',  ( 4.614363445337835934, 8.349151705029461468, -0.2795175495247017583 ) ) ;
#65723 = CARTESIAN_POINT ( 'NONE',  ( 0.7500000000000006661, 10.66666666666666430, -1.299038105676657340 ) ) ;
#65724 = CARTESIAN_POINT ( 'NONE',  ( 4.065465959251388206, 5.836405933916976707, -1.599625672291269396 ) ) ;
#65725 = ADVANCED_FACE ( 'NONE', ( #213967 ), #100246, .F. ) ;
#65726 = CARTESIAN_POINT ( 'NONE',  ( 3.356489944714312834, -1.342140201951192102, 1.153657164820639958 ) ) ;
#65727 = AXIS2_PLACEMENT_3D ( 'NONE', #123026, #91514, #70935 ) ;
#65728 = CARTESIAN_POINT ( 'NONE',  ( 6.370183515248876382, 1.128980158350336049, 1.895982279999992359 ) ) ;
#65729 = CARTESIAN_POINT ( 'NONE',  ( -1.402160292154681736E-14, 8.921875000341405126, 1.575800808251682339 ) ) ;
#65730 = ORIENTED_EDGE ( 'NONE', *, *, #197971, .F. ) ;
#65731 = CARTESIAN_POINT ( 'NONE',  ( -6.771371375382467583, 6.864631124226471037, -0.7998128361456362523 ) ) ;
#65732 = CARTESIAN_POINT ( 'NONE',  ( 5.290638740200858336, 1.525033539048275655, -1.319242139327673202 ) ) ;
#65733 = ORIENTED_EDGE ( 'NONE', *, *, #114579, .T. ) ;
#65734 = CARTESIAN_POINT ( 'NONE',  ( 2.395189659270926086, 1.444574673180216706, 1.188490415850687487 ) ) ;
#65735 = CARTESIAN_POINT ( 'NONE',  ( 3.063400401570901543, 1.746483293306470674, 1.111379191485066364 ) ) ;
#65736 = CARTESIAN_POINT ( 'NONE',  ( -8.041394506236766659, 8.554250810130591631, -0.7216878364870338292 ) ) ;
#65737 = CARTESIAN_POINT ( 'NONE',  ( 2.373185085050379506, -1.665764800640230803, -0.9392108107411781814 ) ) ;
#65738 = CARTESIAN_POINT ( 'NONE',  ( -0.4842345852037238663, 3.595399794601802146, 0.4350569428522566007 ) ) ;
#65739 = CARTESIAN_POINT ( 'NONE',  ( -9.348526197514022584, 4.999985930147239799, -7.001887667968696327 ) ) ;
#65740 = CARTESIAN_POINT ( 'NONE',  ( 9.681502918193430673, 4.134753598976697475, 7.090028296829109067 ) ) ;
#65741 = EDGE_CURVE ( 'NONE', #62417, #66472, #74225, .T. ) ;
#65742 = CARTESIAN_POINT ( 'NONE',  ( 1.364683531249988535, 4.717708333674756283, -0.7879004041258300672 ) ) ;
#65743 = CARTESIAN_POINT ( 'NONE',  ( 1.511816067030671729, -0.6413169068853613597, 1.801808535584384252 ) ) ;
#65744 = CARTESIAN_POINT ( 'NONE',  ( 3.121486724888074882, 0.2905151309811822569, -1.940125473959073421 ) ) ;
#65745 = EDGE_CURVE ( 'NONE', #40807, #198442, #19718, .T. ) ;
#65746 = CARTESIAN_POINT ( 'NONE',  ( -2.609770642201835855, 0.3830433331901538785, 0.000000000000000000 ) ) ;
#65747 = CARTESIAN_POINT ( 'NONE',  ( -5.147255595043616516, 6.034161611419515125, 1.199719254218452935 ) ) ;
#65749 = CARTESIAN_POINT ( 'NONE',  ( -2.279776052174470546, 5.602663296202901932, -0.04407265314621480051 ) ) ;
#65748 = CARTESIAN_POINT ( 'NONE',  ( 7.886038904643079661, 12.35212915539230139, -0.7998128361456352531 ) ) ;
#65750 = CARTESIAN_POINT ( 'NONE',  ( 6.344996225704436554, -1.666636976361988154, 1.052594414163325220 ) ) ;
#65751 = CARTESIAN_POINT ( 'NONE',  ( -0.6823417656250003738, 1.967708333674753174, -1.181850606188749264 ) ) ;
#65752 = CARTESIAN_POINT ( 'NONE',  ( 2.197523118450269486, 1.838911438263282738, -0.8198142501213819822 ) ) ;
#65754 = CARTESIAN_POINT ( 'NONE',  ( 2.777094422528699535, 1.814377389300044330, -1.091000554854235638 ) ) ;
#65753 = CARTESIAN_POINT ( 'NONE',  ( -8.188761592974058701, 8.655902734665618325, -0.7216878364870278340 ) ) ;
#65755 = CARTESIAN_POINT ( 'NONE',  ( 1.436717785781294943, 7.422226822640119792, 4.237127798884887220 ) ) ;
#65756 = CARTESIAN_POINT ( 'NONE',  ( 3.561042923925850978, 1.633862107263984065, -1.271492733312264090 ) ) ;
#65757 = CARTESIAN_POINT ( 'NONE',  ( 5.520104819419390907, 6.469152373191302985, 1.199719254218452935 ) ) ;
#65759 = CARTESIAN_POINT ( 'NONE',  ( 5.515469562660962666, 5.329135999392899947, 0.7998128361456341429 ) ) ;
#65758 = CARTESIAN_POINT ( 'NONE',  ( 6.369093512601681439, 2.000948562089053695, -0.6057377149290378293 ) ) ;
#65761 = ORIENTED_EDGE ( 'NONE', *, *, #85738, .F. ) ;
#65760 = CARTESIAN_POINT ( 'NONE',  ( 3.856323340278215106, 0.6566615474184741563, 1.703573633380930152 ) ) ;
#65762 = CARTESIAN_POINT ( 'NONE',  ( 9.836604141914616406, 11.43479190611061647, 1.199719254218452047 ) ) ;
#65763 = FACE_OUTER_BOUND ( 'NONE', #203462, .T. ) ;
#65764 = CARTESIAN_POINT ( 'NONE',  ( 9.553701449168967130, 11.68847306586624768, 6.138592618161210268 ) ) ;
#65765 = CARTESIAN_POINT ( 'NONE',  ( 5.262800499965147871, -1.601618428465928057, 1.518362080380669221 ) ) ;
#65766 = CARTESIAN_POINT ( 'NONE',  ( -8.012344526598182026E-15, 10.10937500034140335, -1.575800808251669460 ) ) ;
#65767 = CARTESIAN_POINT ( 'NONE',  ( 3.457576163436149486, -1.449788379102138869, -1.247086912153513749 ) ) ;
#65768 = CARTESIAN_POINT ( 'NONE',  ( -10.64723070543352712, 11.31619066596094392, 0.7998128361456462443 ) ) ;
#65769 = CARTESIAN_POINT ( 'NONE',  ( 6.877010230629674759, 9.046264573866535486, 1.599625672291281386 ) ) ;
#65770 = CARTESIAN_POINT ( 'NONE',  ( -3.755786496842899057E-14, 2.109375000341444206, -1.570758158831810247 ) ) ;
#65771 = CARTESIAN_POINT ( 'NONE',  ( 5.477130869796502211, 5.492333557625114437, 1.040834085586084257E-14 ) ) ;
#65772 = DIRECTION ( 'NONE',  ( 5.057645237790724994E-47, 9.066213480720158442E-32, -1.000000000000000000 ) ) ;
#65773 = DIRECTION ( 'NONE',  ( 0.000000000000000000, 0.000000000000000000, 1.000000000000000000 ) ) ;
#65774 = CARTESIAN_POINT ( 'NONE',  ( 0.5910386730991653570, -0.6632029860377097741, 1.717849102829023922 ) ) ;
#65775 = ORIENTED_EDGE ( 'NONE', *, *, #33554, .F. ) ;
#65776 = LINE ( 'NONE', #78851, #210192 ) ;
#65777 = CARTESIAN_POINT ( 'NONE',  ( 5.202362286721474050, -0.6290170809866748591, -1.761763226176292996 ) ) ;
#65778 = CARTESIAN_POINT ( 'NONE',  ( 11.80247861663003484, 11.30000000000000249, -1.695431928471867966 ) ) ;
#65779 = CARTESIAN_POINT ( 'NONE',  ( -1.499999999999997335, 7.809254910130847271, -3.635752117226044522 ) ) ;
#65780 = CARTESIAN_POINT ( 'NONE',  ( -5.910991785878158211, 9.839981483592442402, -0.7216878364870278340 ) ) ;
#65781 = CARTESIAN_POINT ( 'NONE',  ( 6.159481859310094620, 6.080483678816896109, 1.040834085586084257E-14 ) ) ;
#65782 = CARTESIAN_POINT ( 'NONE',  ( 1.533974946755271240, 1.168952700103634390, 1.584878304665905180 ) ) ;
#65783 = CARTESIAN_POINT ( 'NONE',  ( 2.566029989117986077, -1.034146858587611906, 1.730878619409223163 ) ) ;
#65784 = CARTESIAN_POINT ( 'NONE',  ( -8.941766003412679353, 10.39081407785832845, -1.199719254218446718 ) ) ;
#65785 = CARTESIAN_POINT ( 'NONE',  ( 6.343235766347262938, 8.493804042195527870, -1.599625672291281386 ) ) ;
#65786 = CARTESIAN_POINT ( 'NONE',  ( 3.719872605471106208, 6.605953636083950364, 7.500000000000000000 ) ) ;
#65787 = CARTESIAN_POINT ( 'NONE',  ( 2.625153213768507854, -2.044362554934661791, 0.7897752707372793779 ) ) ;
#65788 = CARTESIAN_POINT ( 'NONE',  ( 9.476364758792197307, 3.602180318966379247, -7.289720839516039774 ) ) ;
#65789 = CARTESIAN_POINT ( 'NONE',  ( -7.960608749518247151, 12.43912730774665576, 0.000000000000000000 ) ) ;
#65790 = CYLINDRICAL_SURFACE ( 'NONE', #179843, 1.500000000000000222 ) ;
#65792 = CARTESIAN_POINT ( 'NONE',  ( 9.579698345292687378, -7.154544010627095219, 0.07602376731354922035 ) ) ;
#65791 = B_SPLINE_SURFACE_WITH_KNOTS ( 'NONE', 1, 3, ( 
 ( #107176, #142848, #123464, #41069, #43206, #72462, #93020, #208852, #173202, #58366, #124519, #158016, #56234, #138562, #190477, #42136, #108251, #174272, #25847, #91955, #17848, #79929, #194750, #29062, #2660, #178515, #94087, #83933, #163331, #144979, #167334, #128772, #127722, #150022, #134854, #177449, #51453, #44258, #13853, #160127, #193681, #95146, #30126, #162266, #176385, #161197, #68733, #35174, #209918, #110381, #210983, #96215, #146035, #101251, #1592, #46386, #62611, #27991, #112504, #11726, #129843, #212048, #12784, #78857, #63687, #77802, #18920, #45324, #61556, #67653, #133799, #111444, #199809, #195825, #47464, #113579, #143922, #179581, #31203, #117573, #183568, #97277, #85005, #151096, #69795, #89296, #74101, #119709, #205136, #200860, #170519, #102321, #135904, #185691, #186766, #104472, #118640, #103395, #156424, #188902, #152150, #52507, #87140, #38392, #22101, #40544, #23181, #203001, #4781, #184625, #153211, #36242, #71931, #88214, #37321, #169456, #54641, #19991, #106648, #201922, #3720, #6930, #171588, #56779, #154285, #21043, #53575, #70859, #122945, #136974, #5859, #105553, #55706, #24252, #90356, #168394, #139108, #120789, #138041, #155347, #86075, #172675, #204054, #121860, #187831, #39458, #73009, #8010, #126130, #142335, #158553, #178009, #57841, #109870, #91437, #62121, #25336, #206215, #107734, #93571, #94640, #92514, #58914, #124004, #110929, #209402, #29626, #128281, #144478, #157498, #159616, #193175, #189971, #175883, #42694, #61047, #41620, #9093, #10149, #194243, #208345, #45887, #75169, #141279, #12279, #161764, #112008, #95711, #207287, #26403, #191027, #44824, #125070, #13356, #108800, #210484, #140193, #11213, #173759, #76224, #174826, #192090, #59976, #43757, #27473, #77294, #143406, #127207, #176934, #28551, #160684, #78357, #100999, #64254, #99948, #33870, #130397, #63181 ),
 ( #181189, #198489, #148702, #117323, #183321, #195323, #17598, #180136, #131433, #50134, #211545, #51201, #31764, #129345, #81559, #146596, #271, #82617, #65286, #147643, #97834, #34925, #46954, #49076, #30699, #1346, #179077, #145548, #113072, #32816, #166012, #163899, #212614, #96780, #116256, #66342, #167088, #67408, #83682, #162831, #98890, #132487, #14409, #115196, #196387, #182245, #80499, #48030, #15475, #133549, #213661, #199557, #114144, #197435, #149771, #79430, #164943, #16535, #85826, #119458, #69546, #71683, #118390, #72765, #35997, #89048, #188659, #137796, #121615, #102078, #203815, #54402, #169208, #3479, #40288, #152962, #68486, #55460, #187584, #185445, #138864, #103147, #168146, #39210, #106398, #151905, #22932, #18679, #202749, #134613, #19746, #135656, #4536, #136725, #150845, #201679, #84758, #6690, #184378, #2409, #105301, #171338, #53325, #155105, #120541, #20799, #37066, #200616, #70610, #52263, #204882, #56534, #86895, #122696, #186520, #38150, #104222, #170269, #21854, #87961, #154035, #5601, #73847, #107484, #91184, #158313, #75980, #90113, #74917, #128030, #160429, #123759, #172422, #58664, #9904, #142083, #12034, #209155, #174576, #190778, #156180, #124815, #24012, #43506, #208098, #8838, #157245, #26153, #205968, #78106, #41373, #189721, #192912, #143161, #176682, #59726, #207034, #173509, #25082, #28294, #141027, #125885, #77033, #27218, #210227, #61865, #139941, #110684, #42441, #191843, #60794, #7759, #144233, #108545, #57600, #92267, #109627, #93324, #175632, #159360, #10958, #126953, #193984, #44568, #94390, #45632, #33620, #211297, #177755, #79175, #65040, #66086, #63995, #30443, #95466, #82364, #180935, #149510, #99691, #116000, #129089, #131195, #164692, #161514, #81313, #14150, #32556, #29370, #62921, #196137, #165761, #113890, #17346, #46699, #112816, #198238, #133291, #83428 ) ),
 .UNSPECIFIED., .F., .T., .F.,
 ( 2, 2 ),
 ( 4, 2, 2, 2, 2, 2, 2, 2, 2, 2, 2, 2, 2, 2, 2, 2, 2, 2, 2, 2, 2, 2, 2, 2, 2, 2, 2, 2, 2, 2, 2, 2, 2, 2, 2, 2, 2, 2, 2, 2, 2, 2, 2, 2, 2, 2, 2, 2, 2, 2, 2, 2, 2, 2, 2, 2, 2, 2, 2, 2, 2, 2, 2, 2, 2, 2, 2, 2, 2, 2, 2, 2, 2, 2, 2, 2, 2, 2, 2, 2, 2, 2, 2, 2, 2, 2, 2, 2, 2, 2, 2, 2, 2, 2, 2, 2, 2, 2, 2, 2, 2, 2, 2, 2, 2, 2, 2, 2, 4 ),
 ( 0.000000000000000000, 1.000000000000000000 ),
 ( -5.017377349295429334E-06, 6.045441312669188748E-05, 0.0001259262036026792043, 0.0002568697845546538379, 0.0003878133655066284716, 0.0004205492607446221706, 0.0004532851559826158155, 0.0005187569464586031052, 0.0005842287369345903949, 0.0006497005274105776846, 0.0007806441083625523724, 0.0008461158988385397706, 0.0009115876893145270603, 0.0009770594797905143500, 0.001042531270266501640, 0.001173474851218476219, 0.001238946641694463509, 0.001304418432170450799, 0.001369890222646438088, 0.001435362013122425378, 0.001500833803598412668, 0.001566305594074400174, 0.001631777384550387681, 0.001697249175026374970, 0.001762720965502362260, 0.001828192755978349550, 0.001893664546454336840, 0.001959136336930324129, 0.002090079917882298709, 0.002155551708358285998, 0.002221023498834273288, 0.002286495289310260578, 0.002351967079786247868, 0.002482910660738222447, 0.002548382451214209737, 0.002613854241690197026, 0.002679326032166184316, 0.002744797822642171606, 0.002810269613118158896, 0.002875741403594146185, 0.003006684984546120765, 0.003072156775022108488, 0.003137628565498095778, 0.003203100355974083067, 0.003268572146450070791, 0.003399515727402045370, 0.003530459308354019950, 0.003563195203592013811, 0.003595931098830007239, 0.003661402889305994529, 0.003726874679781981819, 0.003792346470257969109, 0.003923290051209943688, 0.003988761841685931411, 0.004054233632161918267, 0.004119705422637905123, 0.004185177213113892847, 0.004250649003589880570, 0.004316120794065867426, 0.004381592584541854282, 0.004447064375017842006, 0.004578007955969816585, 0.004643479746445803441, 0.004708951536921791164, 0.004774423327397778888, 0.004839895117873765744, 0.004970838698825740323, 0.005101782279777714903, 0.005232725860729689482, 0.005363669441681664062, 0.005494613022633638641, 0.005625556603585613220, 0.005691028394061600076, 0.005756500184537587800, 0.005821971975013575523, 0.005887443765489562379, 0.006018387346441536959, 0.006083859136917524682, 0.006149330927393512405, 0.006214802717869500129, 0.006280274508345486985, 0.006411218089297461564, 0.006476689879773449288, 0.006542161670249437011, 0.006607633460725424734, 0.006673105251201411590, 0.006738577041677398446, 0.006804048832153386170, 0.006869520622629373893, 0.006934992413105360749, 0.007000464203581347605, 0.007065935994057335329, 0.007131407784533323052, 0.007196879575009309908, 0.007327823155961284488, 0.007393294946437272211, 0.007458766736913259067, 0.007491502632151252061, 0.007524238527389245923, 0.007589710317865233646, 0.007720653898817208226, 0.007786125689293195082, 0.007851597479769182805, 0.007917069270245168794, 0.007982541060721156517, 0.008113484641673131964, 0.008244428222625107411, 0.008309900013101095134, 0.008375371803577081123 ),
 .UNSPECIFIED. ) ;
#65793 = CARTESIAN_POINT ( 'NONE',  ( 4.231553341240963384, 7.950912974840849579, -0.7216878364870357165 ) ) ;
#65794 = CARTESIAN_POINT ( 'NONE',  ( 8.259941899223605333, 10.65968485389279508, -1.599625672291268286 ) ) ;
#65795 =( BOUNDED_CURVE ( )  B_SPLINE_CURVE ( 2, ( #189730, #120553, #89060 ),
 .UNSPECIFIED., .F., .T. ) 
 B_SPLINE_CURVE_WITH_KNOTS ( ( 3, 3 ),
 ( 0.1249999999999998751, 0.1276624645066402886 ),
 .UNSPECIFIED. ) 
 CURVE ( )  GEOMETRIC_REPRESENTATION_ITEM ( )  RATIONAL_B_SPLINE_CURVE ( ( 1.000000000000003997, 0.9143913742683040802, 0.9381891137235958134 ) ) 
 REPRESENTATION_ITEM ( '' )  );
#65796 = DIRECTION ( 'NONE',  ( 0.000000000000000000, 0.000000000000000000, 1.000000000000000000 ) ) ;
#65797 = CARTESIAN_POINT ( 'NONE',  ( 5.994113311017540191, 9.046863725278862844, -1.082531754730548412 ) ) ;
#65798 = ORIENTED_EDGE ( 'NONE', *, *, #10571, .T. ) ;
#65799 = VERTEX_POINT ( 'NONE', #166314 ) ;
#65801 = CARTESIAN_POINT ( 'NONE',  ( 1.383448652483735941, 0.1460618955802815977, -2.007835497447094664 ) ) ;
#65800 = CARTESIAN_POINT ( 'NONE',  ( 5.056134578334451568, -1.329838508726857382, 1.273713382018211382 ) ) ;
#65802 = CARTESIAN_POINT ( 'NONE',  ( 3.321888608656462072, -1.742702400767569992, 1.498638621658739511 ) ) ;
#65804 = CARTESIAN_POINT ( 'NONE',  ( 1.322862136463611504, -1.679459703857703268, -0.8019484745323454122 ) ) ;
#65803 = CARTESIAN_POINT ( 'NONE',  ( -1.249999999999963807, 8.500000000000000000, 10.85702537530424827 ) ) ;
#65805 = CARTESIAN_POINT ( 'NONE',  ( -3.285556943749998737, -3.580208332855374653, 1.896917185911908499 ) ) ;
#65806 = DIRECTION ( 'NONE',  ( -0.6507913734559559460, 0.7592566023653074536, 0.000000000000000000 ) ) ;
#65807 = CARTESIAN_POINT ( 'NONE',  ( 6.064708884584704585, 0.6063723501847050334, 1.813766235492550560 ) ) ;
#65808 = CARTESIAN_POINT ( 'NONE',  ( -9.267161690140662600, 10.77044237904097734, -1.199719254218441611 ) ) ;
#65809 = CARTESIAN_POINT ( 'NONE',  ( -7.593975437430151132, 8.032261896522864930, -0.7216878364870338292 ) ) ;
#65811 = CARTESIAN_POINT ( 'NONE',  ( 2.272138710904994863, -1.152746988206950096, 1.473173409640892162 ) ) ;
#65810 = CARTESIAN_POINT ( 'NONE',  ( 3.913685052542864362, -1.076426932671892711, -1.792217407939109552 ) ) ;
#65812 = CARTESIAN_POINT ( 'NONE',  ( 7.836249599018724865, 9.205007956019091608, -1.082531754730537976 ) ) ;
#65813 = CARTESIAN_POINT ( 'NONE',  ( -1.001543065824772872E-14, 5.384375000341413475, 1.575800808251672791 ) ) ;
#65814 = CARTESIAN_POINT ( 'NONE',  ( 6.251489360189885325, 1.835807759842246423, -0.1425652098738516838 ) ) ;
#65815 = CARTESIAN_POINT ( 'NONE',  ( 2.659370686574860976, 6.254349567645977714, -0.7998128361456291469 ) ) ;
#65816 = CARTESIAN_POINT ( 'NONE',  ( -6.604641253243921817, -6.414086731524404783, -7.221001870987140414 ) ) ;
#65817 = CARTESIAN_POINT ( 'NONE',  ( 4.617633504863215776, -1.690751803285206245, 0.3404669814689939011 ) ) ;
#65818 = CARTESIAN_POINT ( 'NONE',  ( -6.632963465583701534, 8.761543347979550589, -1.599625672291263179 ) ) ;
#65819 = CARTESIAN_POINT ( 'NONE',  ( 0.5099215751255279372, -1.647279052675547861, 0.5420907402255652485 ) ) ;
#65820 = CARTESIAN_POINT ( 'NONE',  ( -1.620863580070950327, 0.4000000000000010214, 1.903365770102947385 ) ) ;
#65821 = SURFACE_SIDE_STYLE ('',( #82100 ) ) ;
#65822 = ADVANCED_FACE ( 'NONE', ( #18977 ), #181492, .T. ) ;
#65823 = CARTESIAN_POINT ( 'NONE',  ( 9.578206935422338475, -9.907361015872668375, -0.1671882239541239157 ) ) ;
#65824 = CARTESIAN_POINT ( 'NONE',  ( 4.258752264053907055, -0.6753675163390076008, -2.063452119831588494 ) ) ;
#65825 = CARTESIAN_POINT ( 'NONE',  ( 3.281694405262673087, 1.158851912627656189, 1.410738560442346801 ) ) ;
#65826 = CARTESIAN_POINT ( 'NONE',  ( 1.551531708069888937, 1.481957716508151668, 1.285475804911541120 ) ) ;
#65827 = CARTESIAN_POINT ( 'NONE',  ( 5.524650688480493343, 0.4156912398748518478, 2.075975271109116171 ) ) ;
#65828 = B_SPLINE_CURVE_WITH_KNOTS ( 'NONE', 3,
 ( #97242, #115657, #147061, #213081, #164358, #15942 ),
 .UNSPECIFIED., .F., .F.,
 ( 4, 2, 4 ),
 ( 0.000000000000000000, 0.0001030949158708163878, 0.0002061898317416328299 ),
 .UNSPECIFIED. ) ;
#65830 = CARTESIAN_POINT ( 'NONE',  ( 0.6823417656249917140, 3.905208333674754950, 1.181850606188765695 ) ) ;
#65829 = CARTESIAN_POINT ( 'NONE',  ( 6.005493137707444973, -2.275576565988911337, 0.2767016799969032603 ) ) ;
#65831 = CARTESIAN_POINT ( 'NONE',  ( 5.314433026432511475, 5.302519407033794430, 1.040834085586084257E-14 ) ) ;
#65832 = CARTESIAN_POINT ( 'NONE',  ( 9.348510611822643313, 10.86534945433664134, 1.199719254218453823 ) ) ;
#65833 = VECTOR ( 'NONE', #167338, 1000.000000000000000 ) ;
#65834 = CARTESIAN_POINT ( 'NONE',  ( 1.823052125313682215, 1.569171740784220281, -1.426411057285102979 ) ) ;
#65835 = CARTESIAN_POINT ( 'NONE',  ( -4.039966587192274083, 5.736380323189513852, 1.443375672974064550 ) ) ;
#65836 = CARTESIAN_POINT ( 'NONE',  ( 4.190878879955592495, 7.903459436674620697, -0.7216878364870198403 ) ) ;
#65837 = CARTESIAN_POINT ( 'NONE',  ( -4.568734577680887199, 6.353276312092901890, -1.443375672974051449 ) ) ;
#65838 = CARTESIAN_POINT ( 'NONE',  ( 5.963789030284865511, -0.5350816163755196531, 2.103975319158644552 ) ) ;
#65840 = CARTESIAN_POINT ( 'NONE',  ( -1.402160292154681736E-14, 12.84375000068279959, 1.732050807568881190 ) ) ;
#65839 = CARTESIAN_POINT ( 'NONE',  ( 1.843739406749228538, 9.999999999999998224, -0.7749999999999996891 ) ) ;
#65842 = ORIENTED_EDGE ( 'NONE', *, *, #163961, .T. ) ;
#65841 = CARTESIAN_POINT ( 'NONE',  ( 2.543850053281167423, -2.071606161961367043, 0.8020612402455605805 ) ) ;
#65843 = CARTESIAN_POINT ( 'NONE',  ( 6.152970239395502361, 1.038990588714868490, 1.728003889287746286 ) ) ;
#65845 = CARTESIAN_POINT ( 'NONE',  ( 4.153227615898272163, 1.745077553047107433, -1.099210343703932669 ) ) ;
#65844 = CARTESIAN_POINT ( 'NONE',  ( 3.659811400685081040, 6.357198169852855685, -1.199719254218446718 ) ) ;
#65847 = CARTESIAN_POINT ( 'NONE',  ( 3.130865642711470276, -4.000192543527539613, -1.507748429708645199 ) ) ;
#65846 = CARTESIAN_POINT ( 'NONE',  ( 4.583538449871731757, 7.505156070562471804, 1.199719254218451159 ) ) ;
#65848 = CARTESIAN_POINT ( 'NONE',  ( 5.550083779947807550, 7.568460058062819407, -1.599625672291283607 ) ) ;
#65849 = CARTESIAN_POINT ( 'NONE',  ( 0.000000000000000000, -3.084374999522042859, -3.793834371823813001 ) ) ;
#65850 = CYLINDRICAL_SURFACE ( 'NONE', #2590, 0.3999999999999997446 ) ;
#65851 = CARTESIAN_POINT ( 'NONE',  ( 4.458453498679889826, -1.646799808365447149, -0.8236825204945982248 ) ) ;
#65852 = CARTESIAN_POINT ( 'NONE',  ( 4.143988507271280319, 7.986403691791820414, -0.7998128361456221525 ) ) ;
#65853 = CARTESIAN_POINT ( 'NONE',  ( 1.342334339533798104, 0.3310447913058271463, 1.692513552724637771 ) ) ;
#65854 = CARTESIAN_POINT ( 'NONE',  ( -0.1531117392989979065, -1.803405091603600185, -0.9023890051431044945 ) ) ;
#65855 = CARTESIAN_POINT ( 'NONE',  ( 2.250986472945924355, 2.253575863342609065, -0.4525425749238082829 ) ) ;
#65856 = CARTESIAN_POINT ( 'NONE',  ( 1.364683531249990311, 3.446875000341416584, 1.214306433183764966E-14 ) ) ;
#65857 = CARTESIAN_POINT ( 'NONE',  ( 1.335668079023267119, -2.045225487398461883, 0.9674528744543411385 ) ) ;
#65858 = CARTESIAN_POINT ( 'NONE',  ( 3.809285178775764447, 1.806332912941556623, 1.082654235687771749 ) ) ;
#65859 = CARTESIAN_POINT ( 'NONE',  ( -4.821859908315634158, 5.654533310236863564, 1.199719254218452935 ) ) ;
#65860 = CARTESIAN_POINT ( 'NONE',  ( 1.967667936517076166, 0.9046490693802499150, 1.520878277628298303 ) ) ;
#65861 = CARTESIAN_POINT ( 'NONE',  ( 5.615048174354031474, 9.702639970055050966, 0.7998128361456462443 ) ) ;
#65862 = CARTESIAN_POINT ( 'NONE',  ( 5.844973620822844218, 5.991759777147701804, 0.7216878364870328300 ) ) ;
#65863 = CARTESIAN_POINT ( 'NONE',  ( -4.889686956022917919, 8.856385215335397021, 1.214306433183764966E-14 ) ) ;
#65864 = CARTESIAN_POINT ( 'NONE',  ( 5.870317324592803310, 7.871789516823500144, -1.443375672974057666 ) ) ;
#65865 = CARTESIAN_POINT ( 'NONE',  ( -1.500000000000013101, 1.629166666666691077, -0.8660254037844313801 ) ) ;
#65866 = ADVANCED_FACE ( 'NONE', ( #117633 ), #575, .T. ) ;
#65867 = CARTESIAN_POINT ( 'NONE',  ( -3.761497552787613330, 6.475832013972435242, 1.199719254218464037 ) ) ;
#65868 = CARTESIAN_POINT ( 'NONE',  ( 4.588250468535750137, 1.280153277506433707, 1.815263839992816042 ) ) ;
#65869 = CARTESIAN_POINT ( 'NONE',  ( 3.240350661220792183, 0.5327334615983710941, 2.125583950146384904 ) ) ;
#65870 = CARTESIAN_POINT ( 'NONE',  ( -4.924636110261798372, 6.768494766770632332, 1.599625672291267398 ) ) ;
#65871 = CARTESIAN_POINT ( 'NONE',  ( -5.469788628470539926, 5.346117919495872783, -0.7998128361456362523 ) ) ;
#65872 = DIRECTION ( 'NONE',  ( 0.000000000000000000, -7.228014483236694583E-17, 1.000000000000000000 ) ) ;
#65873 = AXIS2_PLACEMENT_3D ( 'NONE', #7278, #22461, #206561 ) ;
#65874 = CARTESIAN_POINT ( 'NONE',  ( 1.364683531249988535, 3.655208333674750509, -0.7879004041258239610 ) ) ;
#65875 = CARTESIAN_POINT ( 'NONE',  ( 6.610000000000021636, 3.695490760540712127, 2.514297579034238783 ) ) ;
#65876 = CARTESIAN_POINT ( 'NONE',  ( -4.067082894419624672, 6.728385229256075739, 1.082531754730560403 ) ) ;
#65877 = CARTESIAN_POINT ( 'NONE',  ( 5.431924468521282634, -2.068440459917933794, 0.4666711972392265650 ) ) ;
#65878 = CARTESIAN_POINT ( 'NONE',  ( -7.756673280794142755, 8.222076047114187602, -0.7216878364870338292 ) ) ;
#65879 = ORIENTED_EDGE ( 'NONE', *, *, #120622, .T. ) ;
#65881 = CARTESIAN_POINT ( 'NONE',  ( 1.220146605508150803E-14, 11.21875000068279249, -1.499999999999998446 ) ) ;
#65880 = CARTESIAN_POINT ( 'NONE',  ( -4.326460416536637155, 8.061637896019123062, 0.000000000000000000 ) ) ;
#65882 = CARTESIAN_POINT ( 'NONE',  ( 4.385172619016207918, 7.203452924572514959, 1.199719254218462483 ) ) ;
#65883 = CARTESIAN_POINT ( 'NONE',  ( 6.550350952284553330, -1.418464805562440922, 1.173678288350611609 ) ) ;
#65884 = UNCERTAINTY_MEASURE_WITH_UNIT (LENGTH_MEASURE( 1.000000000000000082E-05 ), #128836, 'distance_accuracy_value', 'NONE');
#65885 = CARTESIAN_POINT ( 'NONE',  ( 1.364683531249988535, 2.967708333674755394, -0.7879004041258239610 ) ) ;
#65886 = CARTESIAN_POINT ( 'NONE',  ( 1.452286687950472999, -1.492487064643189809, -0.8950295028009451759 ) ) ;
#65887 = CARTESIAN_POINT ( 'NONE',  ( 2.361091307074211887, 5.906356958228550447, 0.7998128361456462443 ) ) ;
#65889 = EDGE_CURVE ( 'NONE', #109006, #94442, #200786, .T. ) ;
#65888 = CARTESIAN_POINT ( 'NONE',  ( 0.1507198084474276056, -0.4258245693303016610, -1.922078969575198526 ) ) ;
#65890 = CARTESIAN_POINT ( 'NONE',  ( 1.364683531249988757, -0.5531249996585801965, 0.000000000000000000 ) ) ;
#65891 = CARTESIAN_POINT ( 'NONE',  ( 0.000000000000000000, 0.7999999999999951594, 0.000000000000000000 ) ) ;
#65892 = CARTESIAN_POINT ( 'NONE',  ( 4.873979933848565871, 1.241796773192262116, 1.769252301715443565 ) ) ;
#65893 = EDGE_CURVE ( 'NONE', #164262, #44, #98147, .T. ) ;
#65894 = CARTESIAN_POINT ( 'NONE',  ( -3.623053363349869382, 5.249981562040033189, 1.599625672291267398 ) ) ;
#65895 = CARTESIAN_POINT ( 'NONE',  ( -6.358410854684793279, 7.480862754296137673, -1.082531754730543083 ) ) ;
#65896 = CARTESIAN_POINT ( 'NONE',  ( 4.522454563201145028, 1.332364063043836033, -1.702191164408660251 ) ) ;
#65898 = ORIENTED_EDGE ( 'NONE', *, *, #36376, .F. ) ;
#65897 = CYLINDRICAL_SURFACE ( 'NONE', #8340, 1.500000000000000222 ) ;
#65899 = CARTESIAN_POINT ( 'NONE',  ( -1.201851678989727383E-14, 3.446875000341421469, -1.575800808251660134 ) ) ;
#65900 = CARTESIAN_POINT ( 'NONE',  ( 5.553970887368382847, 1.969207887765548559, -0.09415503477229987539 ) ) ;
#65901 = CARTESIAN_POINT ( 'NONE',  ( 5.518767629808705166, 1.731759826824400106, -0.08707812323833011292 ) ) ;
#65903 = CARTESIAN_POINT ( 'NONE',  ( 2.085717061910817183, -0.9337068281064246911, 1.982830571388309204 ) ) ;
#65902 = CARTESIAN_POINT ( 'NONE',  ( -0.6801582343750213200, -0.4010416663252705516, -1.178068619123886718 ) ) ;
#65904 = CARTESIAN_POINT ( 'NONE',  ( 3.364621831457567769, 1.035725732715401470, 2.062151656813861145 ) ) ;
#65905 = CARTESIAN_POINT ( 'NONE',  ( 4.270816029187285423, -1.921422972303673093, -0.7454010919232464394 ) ) ;
#65906 = CARTESIAN_POINT ( 'NONE',  ( 0.6033350840282033500, -1.932664299774440098, 0.1897328419256556487 ) ) ;
#65907 = CARTESIAN_POINT ( 'NONE',  ( -6.439759776366783761, 8.536139043893143707, 1.443375672974078761 ) ) ;
#65908 = CARTESIAN_POINT ( 'NONE',  ( -3.980200614063634568, 6.801261928786307642, 1.199719254218452935 ) ) ;
#65909 = DIRECTION ( 'NONE',  ( 0.000000000000000000, 0.000000000000000000, -1.000000000000000000 ) ) ;
#65910 = CARTESIAN_POINT ( 'NONE',  ( 4.148766697842418694, 2.080301416381886703, 0.4105806053946169376 ) ) ;
#65911 = DIRECTION ( 'NONE',  ( 1.000000000000000000, -0.000000000000000000, 1.779758311459929752E-16 ) ) ;
#65912 = CARTESIAN_POINT ( 'NONE',  ( 1.582657950916711131, -0.6767122143778031562, 1.899619169727875700 ) ) ;
#65913 = CARTESIAN_POINT ( 'NONE',  ( -4.555176424067209240, 8.258196894812975586, 1.040834085586084257E-14 ) ) ;
#65914 = CARTESIAN_POINT ( 'NONE',  ( 4.348781676370103710, 0.5853419563807431558, 2.127667884090424621 ) ) ;
#65915 = CARTESIAN_POINT ( 'NONE',  ( -3.285556943750000070, -0.5468749995220407722, 0.000000000000000000 ) ) ;
#65916 = CARTESIAN_POINT ( 'NONE',  ( 1.364067407192349757, 4.011924485828274101, -0.6250643920678818910 ) ) ;
#65917 = DIRECTION ( 'NONE',  ( 0.000000000000000000, -1.000000000000000000, 0.000000000000000000 ) ) ;
#65918 = CARTESIAN_POINT ( 'NONE',  ( 3.633153978699183995, 3.497932562452356731, -2.447764766412549697 ) ) ;
#65920 = CARTESIAN_POINT ( 'NONE',  ( -9.818302567231157241, -8.862962251182134210, 0.6073963244357452052 ) ) ;
#65919 = CARTESIAN_POINT ( 'NONE',  ( -4.620524454801235414, 8.454239455966142458, -0.3877863265914320845 ) ) ;
#65921 = FACE_OUTER_BOUND ( 'NONE', #65172, .T. ) ;
#65922 = EDGE_LOOP ( 'NONE', ( #6460, #112769, #199085, #70004, #90614 ) ) ;
#65923 = CARTESIAN_POINT ( 'NONE',  ( 4.627839754413318296, -1.266395719900258232, -1.625807017514354191 ) ) ;
#65924 = CARTESIAN_POINT ( 'NONE',  ( -5.157946788997579689E-14, 1.203125000341463746, 1.570758158831762286 ) ) ;
#65925 = CARTESIAN_POINT ( 'NONE',  ( -4.229253852459088137, 7.021547696922494808, 1.199719254218464037 ) ) ;
#65926 = CARTESIAN_POINT ( 'NONE',  ( 3.334632977657724151, 1.279679970181834436, -1.562544408365494686 ) ) ;
#65927 = CARTESIAN_POINT ( 'NONE',  ( 0.7499999999999885647, -0.5166666666666444030, 1.299038105676657340 ) ) ;
#65928 = CARTESIAN_POINT ( 'NONE',  ( 3.358669367883368118, 4.941533567329135401, -1.599625672291262513 ) ) ;
#65929 = CARTESIAN_POINT ( 'NONE',  ( 2.606383665309390363, -0.7875068868475536554, -1.904698518741376079 ) ) ;
#65930 = CARTESIAN_POINT ( 'NONE',  ( 3.912411256987575303, 4.016135269252925077, 0.7252027155559813698 ) ) ;
#65931 = CARTESIAN_POINT ( 'NONE',  ( 4.306686350635271054, 8.176217842383143974, -0.7998128361456221525 ) ) ;
#65932 = CARTESIAN_POINT ( 'NONE',  ( -0.2409995289980037536, -0.004801160710915518791, -2.000252362011435192 ) ) ;
#65933 = CARTESIAN_POINT ( 'NONE',  ( 1.218424693763892730, -0.04700249260505655335, 1.840701667592301138 ) ) ;
#65934 = CARTESIAN_POINT ( 'NONE',  ( 6.375609195709820654, 2.113139023092651225, -0.6363509056886568205 ) ) ;
#65935 = CARTESIAN_POINT ( 'NONE',  ( 5.040599249230596435, 9.102725900736217568, 0.7998128361456341429 ) ) ;
#65936 = CARTESIAN_POINT ( 'NONE',  ( 1.687033600898584895, -0.3153356727807927196, -2.138329785107299319 ) ) ;
#65937 = CARTESIAN_POINT ( 'NONE',  ( -4.636525346193588248, 4.511627113421689650, 0.7216878364870317197 ) ) ;
#65938 = CARTESIAN_POINT ( 'NONE',  ( 1.745327705122714956, 0.3399549603602426417, -1.987498286102694411 ) ) ;
#65939 = CARTESIAN_POINT ( 'NONE',  ( 1.355808955840422310E-16, 3.400000000000000355, 2.024999999999999911 ) ) ;
#65940 = CARTESIAN_POINT ( 'NONE',  ( 0.2681426532152464959, -1.225442487749365483, 1.413462724991432218 ) ) ;
#65941 = DIRECTION ( 'NONE',  ( 0.000000000000000000, 0.000000000000000000, -1.000000000000000000 ) ) ;
#65942 = TOROIDAL_SURFACE ( 'NONE', #38314, 10.92000000000000171, 0.08000000000000000167 ) ;
#65943 = CARTESIAN_POINT ( 'NONE',  ( 4.522318884118472049, 1.213545612936163032, -1.553610194691892765 ) ) ;
#65944 = CARTESIAN_POINT ( 'NONE',  ( 4.891814693739657827, -2.006371927678828104, 0.2024599332275459629 ) ) ;
#65946 = CARTESIAN_POINT ( 'NONE',  ( 10.68346185744421462, 11.56638637654751989, 0.000000000000000000 ) ) ;
#65945 = CARTESIAN_POINT ( 'NONE',  ( 0.6823417656249899377, 2.092708333674753174, 1.181850606188767472 ) ) ;
#65948 = CARTESIAN_POINT ( 'NONE',  ( -0.004863692847738298151, -0.4900785244342681368, -2.159743284330918112 ) ) ;
#65947 = CARTESIAN_POINT ( 'NONE',  ( -6.744291347794091784, 9.955758108146730123, -1.199719254218440723 ) ) ;
#65949 = CARTESIAN_POINT ( 'NONE',  ( 5.828598057497599960, -1.316348130051235410, 1.597988563933512074 ) ) ;
#65950 = CARTESIAN_POINT ( 'NONE',  ( 7.091078035147269532, 8.231678114882006625, 1.199719254218462483 ) ) ;
#65951 = CARTESIAN_POINT ( 'NONE',  ( -7.172426956829277778, 8.326585190177668849, -1.199719254218452935 ) ) ;
#65952 = CARTESIAN_POINT ( 'NONE',  ( 7.041790712887754822, 6.002124920821316323, 2.446252293856579829 ) ) ;
#65953 = CARTESIAN_POINT ( 'NONE',  ( 5.519787823685118333, -0.4868164491665989413, 1.960129884169951708 ) ) ;
#65954 = CARTESIAN_POINT ( 'NONE',  ( -0.7500000000000249800, -1.277083332650516656, 1.299038105676659116 ) ) ;
#65955 = CARTESIAN_POINT ( 'NONE',  ( 3.686388391042205726, -1.138424198849327107, 2.007274438705310970 ) ) ;
#65956 = CARTESIAN_POINT ( 'NONE',  ( 1.112259789790952746, 2.060362754584772471, -0.09740899567091049205 ) ) ;
#65957 = CARTESIAN_POINT ( 'NONE',  ( 7.782016984564049444, 11.06247500109133064, 1.082531754730557072 ) ) ;
#65958 = EDGE_CURVE ( 'NONE', #56116, #192556, #79189, .T. ) ;
#65959 = CARTESIAN_POINT ( 'NONE',  ( 6.099189001301251523, 8.209082816308541197, 1.599625672291268286 ) ) ;
#65960 = CARTESIAN_POINT ( 'NONE',  ( 6.886615681098613884, 6.999082814228660077, 0.000000000000000000 ) ) ;
#65961 = CARTESIAN_POINT ( 'NONE',  ( 0.6823417656249882723, 0.4885416670080827695, -1.181850606188749264 ) ) ;
#65962 = CARTESIAN_POINT ( 'NONE',  ( 3.718679271898170491, 7.560485927181699317, 0.7998128361456271485 ) ) ;
#65963 = CARTESIAN_POINT ( 'NONE',  ( 7.754900676892376055, 8.149731665903665601, 1.040834085586084257E-14 ) ) ;
#65964 = CARTESIAN_POINT ( 'NONE',  ( 4.492743645254620333, 2.128474237214292852, 0.4277247895240059994 ) ) ;
#65966 = CARTESIAN_POINT ( 'NONE',  ( 3.175182228840720988, 1.170341537027960843, 1.421418621496411516 ) ) ;
#65965 = CARTESIAN_POINT ( 'NONE',  ( -5.585596099150199834, 5.618876325204420930, -0.7216878364870207285 ) ) ;
#65967 = CARTESIAN_POINT ( 'NONE',  ( 0.6823417656249917140, 4.842708333674755394, 1.181850606188765695 ) ) ;
#65968 = CARTESIAN_POINT ( 'NONE',  ( 4.739868811304373430, 2.185674081084403753, 0.1610935195608814985 ) ) ;
#65969 = LINE ( 'NONE', #130032, #201853 ) ;
#65970 = CARTESIAN_POINT ( 'NONE',  ( 5.313438862022389131, -0.3376633510823018880, 2.237075724153537504 ) ) ;
#65971 = CARTESIAN_POINT ( 'NONE',  ( -5.194998520284300980, 6.641152480062820551, -1.419077516013200313 ) ) ;
#65972 = CARTESIAN_POINT ( 'NONE',  ( 4.639288533706844575, 8.435234533841581950, -0.4270733708018232822 ) ) ;
#65973 = AXIS2_PLACEMENT_3D ( 'NONE', #66800, #34332, #83077 ) ;
#65974 = CARTESIAN_POINT ( 'NONE',  ( -6.739811759324840779, 7.035737605399991601, -0.7216878364870338292 ) ) ;
#65975 = CARTESIAN_POINT ( 'NONE',  ( 4.909461021924254709, 5.860697626067345567, 1.082531754730549078 ) ) ;
#65976 = CARTESIAN_POINT ( 'NONE',  ( 6.169200886764430791, 0.1279487620423936933, -1.765195888111121159 ) ) ;
#65977 = CARTESIAN_POINT ( 'NONE',  ( 4.600248117428091810, -0.9470982757478171310, 1.776368884175743235 ) ) ;
#65978 = CARTESIAN_POINT ( 'NONE',  ( 7.796102023057898123, 9.054206100777749455, -1.199719254218441611 ) ) ;
#65979 = CARTESIAN_POINT ( 'NONE',  ( 3.135867587238525100, -1.413284743790550468, -1.561492743641406999 ) ) ;
#65980 = CARTESIAN_POINT ( 'NONE',  ( 2.407709352951839854, -1.104968261951447595, -1.564578956373291696 ) ) ;
#65981 = CARTESIAN_POINT ( 'NONE',  ( 4.521807925357579805, 5.234196320127330715, -1.199719254218452047 ) ) ;
#65982 = CARTESIAN_POINT ( 'NONE',  ( 3.156658437648862225, -0.5693117071641734528, -1.885488911330883255 ) ) ;
#65983 = CARTESIAN_POINT ( 'NONE',  ( 4.763928514684708126, 0.6297656808758389513, -1.919195086291412888 ) ) ;
#65984 = CARTESIAN_POINT ( 'NONE',  ( 0.9713206009373563932, 1.803875226702996049, -0.4951341686536685494 ) ) ;
#65985 = CARTESIAN_POINT ( 'NONE',  ( 1.310910670669521272, -1.548711629584406113, 1.204245502051364936 ) ) ;
#65987 = ORIENTED_EDGE ( 'NONE', *, *, #125678, .T. ) ;
#65986 = CARTESIAN_POINT ( 'NONE',  ( 0.7207899753199145110, 1.446443371814851941, -1.251069288267861346 ) ) ;
#65988 = CARTESIAN_POINT ( 'NONE',  ( 5.829642864196168617, 6.863966765392747860, 1.082531754730558626 ) ) ;
#65989 = TOROIDAL_SURFACE ( 'NONE', #173197, 10.92000000000000348, 0.08000000000000000167 ) ;
#65990 = CARTESIAN_POINT ( 'NONE',  ( -0.6823417656250003738, 1.280208333674752508, -1.181850606188749264 ) ) ;
#65991 = CARTESIAN_POINT ( 'NONE',  ( 5.946149726614578412, 1.868617323842229894, 0.09011704611043556967 ) ) ;
#65992 = CARTESIAN_POINT ( 'NONE',  ( 2.191614386903386613, 5.708633884695917260, -0.7998128361456281477 ) ) ;
#65993 = CARTESIAN_POINT ( 'NONE',  ( 0.000000000000000000, -4.500000000000003553, 0.000000000000000000 ) ) ;
#65994 = CARTESIAN_POINT ( 'NONE',  ( 6.227406488038683463, 0.1581931229415085571, -2.064300627111631314 ) ) ;
#65995 = CARTESIAN_POINT ( 'NONE',  ( 10.00050683067331114, 3.975933801733724238, 5.773795310721800966 ) ) ;
#65996 = CARTESIAN_POINT ( 'NONE',  ( 1.451716722110554025, 1.566445173006292935, 1.353826630019476562 ) ) ;
#65997 = CARTESIAN_POINT ( 'NONE',  ( -0.7500000000000215383, 1.441666666666688190, 1.299038105676659116 ) ) ;
#65998 = CARTESIAN_POINT ( 'NONE',  ( 7.447506452608354088, 7.583179037664891098, 0.7998128361456341429 ) ) ;
#65999 = CARTESIAN_POINT ( 'NONE',  ( -7.720478407978036195, 11.09464301169468037, -1.199719254218446718 ) ) ;
#66000 = CARTESIAN_POINT ( 'NONE',  ( 4.583538449871731757, 7.505156070562471804, 1.199719254218451159 ) ) ;
#66001 = CARTESIAN_POINT ( 'NONE',  ( 6.006510593949522026, -2.110231943656666331, -0.2080817731764383061 ) ) ;
#66002 = CARTESIAN_POINT ( 'NONE',  ( 5.259637247458703868, 5.100941308315409373, 0.000000000000000000 ) ) ;
#66003 = ADVANCED_FACE ( 'NONE', ( #198788 ), #209982, .F. ) ;
#66004 = CARTESIAN_POINT ( 'NONE',  ( -0.6823417656250212460, 1.301041667008083547, 1.181850606188755259 ) ) ;
#66005 = CARTESIAN_POINT ( 'NONE',  ( -0.7500000000000215383, 2.941666666666689522, 1.299038105676671107 ) ) ;
#66007 = CARTESIAN_POINT ( 'NONE',  ( 5.359550796103802028, 5.147230771742885125, -0.7998128361456231517 ) ) ;
#66006 = CARTESIAN_POINT ( 'NONE',  ( 6.654749070045313353, -0.5220710138904552933, -1.891073168474053823 ) ) ;
#66008 = EDGE_CURVE ( 'NONE', #116455, #161726, #141400, .T. ) ;
#66009 = CARTESIAN_POINT ( 'NONE',  ( 3.356795910091507906, -0.8196482158769200499, 1.842165019812888049 ) ) ;
#66010 = CARTESIAN_POINT ( 'NONE',  ( 3.151485257178482158, 1.867856130240726387, -0.4247363484005464151 ) ) ;
#66011 = CARTESIAN_POINT ( 'NONE',  ( -0.7500000000000215383, 4.472916667349482012, 1.299038105676671107 ) ) ;
#66012 = CARTESIAN_POINT ( 'NONE',  ( 1.892365914234435120, -0.5883382831698009685, -2.111031122750434363 ) ) ;
#66013 = DIRECTION ( 'NONE',  ( 0.6507913734559775953, 0.7592566023652888019, 0.000000000000000000 ) ) ;
#66014 = CARTESIAN_POINT ( 'NONE',  ( 3.233525009082056201, -1.253693836546897700, -1.388425355430204622 ) ) ;
#66015 = CARTESIAN_POINT ( 'NONE',  ( -1.500000000000001332, -0.5687499993171779566, 0.000000000000000000 ) ) ;
#66016 = CARTESIAN_POINT ( 'NONE',  ( -7.507464373665155399, 9.781794407407920389, 1.599625672291295375 ) ) ;
#66018 = CARTESIAN_POINT ( 'NONE',  ( 5.273117041167244778, 1.866726688708058690, -0.9990383793265914525 ) ) ;
#66017 = CARTESIAN_POINT ( 'NONE',  ( -3.307826292054304673, 6.802955074131234348, -0.7216878364870267237 ) ) ;
#66019 = CARTESIAN_POINT ( 'NONE',  ( 1.364683531249997417, 8.546875000341403350, 2.602085213965210642E-15 ) ) ;
#66020 = CARTESIAN_POINT ( 'NONE',  ( 6.848098043024292814, -0.8888149443028300345, 1.868052569137634400 ) ) ;
#66022 = CARTESIAN_POINT ( 'NONE',  ( -4.195212134638190982, 7.860597793832757141, -0.3698817738262829558 ) ) ;
#66021 = CARTESIAN_POINT ( 'NONE',  ( 2.155913254374627552, 0.8966022695893551830, 1.888892756932699646 ) ) ;
#66024 = ORIENTED_EDGE ( 'NONE', *, *, #81633, .T. ) ;
#66023 = CARTESIAN_POINT ( 'NONE',  ( 0.5512174377280190107, 0.5480947683692177774, -1.635447244754190788 ) ) ;
#66025 = CARTESIAN_POINT ( 'NONE',  ( 6.262976894508937242, 9.394224579314053969, -1.199719254218440723 ) ) ;
#66026 = CARTESIAN_POINT ( 'NONE',  ( -1.500000000000015099, 12.01041666734946212, -0.8660254037844309360 ) ) ;
#66027 = CARTESIAN_POINT ( 'NONE',  ( -0.08367765422325271207, -9.912493506416723221, -9.499631469177289844 ) ) ;
#66028 = CARTESIAN_POINT ( 'NONE',  ( -9.348561386651960348, 4.000000000000000888, 7.001914024036569373 ) ) ;
#66029 = CARTESIAN_POINT ( 'NONE',  ( 9.720832950873944611, 10.44331931888218001, -0.7216878364870257245 ) ) ;
#66030 = CARTESIAN_POINT ( 'NONE',  ( 1.499999999999990896, 4.306250000682819490, 1.214306433183764966E-14 ) ) ;
#66031 = CARTESIAN_POINT ( 'NONE',  ( -6.338600509588822263, 7.353787668397130162, -1.199719254218446718 ) ) ;
#66033 = CARTESIAN_POINT ( 'NONE',  ( 1.541375357114631806, -1.705629342057282560, 0.6104535550692562484 ) ) ;
#66032 = CARTESIAN_POINT ( 'NONE',  ( 6.554440917563797875, 6.611545590104705994, -0.7998128361456481317 ) ) ;
#66034 = CARTESIAN_POINT ( 'NONE',  ( -6.938021921891187382, 9.117444880338284818, -1.599625672291263179 ) ) ;
#66035 = VECTOR ( 'NONE', #142742, 1000.000000000000000 ) ;
#66036 = CARTESIAN_POINT ( 'NONE',  ( 5.379888026524302980, 5.170957540566797128, -0.7998128361456211532 ) ) ;
#66037 = CARTESIAN_POINT ( 'NONE',  ( -6.497544600628390121, 6.760421010857692536, 0.1165534177344582784 ) ) ;
#66038 = CARTESIAN_POINT ( 'NONE',  ( 7.062871678076271920, 7.204714810702593120, -0.7998128361456341429 ) ) ;
#66039 = CARTESIAN_POINT ( 'NONE',  ( 6.639320575229240795, 2.471732717405307422, 2.181477732991484064 ) ) ;
#66040 = VECTOR ( 'NONE', #42219, 1000.000000000000000 ) ;
#66041 = DIRECTION ( 'NONE',  ( 0.000000000000000000, 8.546850786086437571E-32, 1.000000000000000000 ) ) ;
#66042 = DIRECTION ( 'NONE',  ( 0.000000000000000000, 0.000000000000000000, 1.000000000000000000 ) ) ;
#66043 = CARTESIAN_POINT ( 'NONE',  ( 9.951321562750607086, 11.67259191370631477, -1.082531754730537088 ) ) ;
#66044 = ORIENTED_EDGE ( 'NONE', *, *, #204596, .T. ) ;
#66045 = EDGE_CURVE ( 'NONE', #81487, #14615, #22384, .T. ) ;
#66046 = CARTESIAN_POINT ( 'NONE',  ( 2.822522581191502677, -1.285663882657582580, 1.345810825326615223 ) ) ;
#66047 = CARTESIAN_POINT ( 'NONE',  ( -0.03574161356561295771, -1.858227405880557015, -0.4649775414454700995 ) ) ;
#66048 = CARTESIAN_POINT ( 'NONE',  ( 6.598663746767657656, -0.5144617408539242653, -1.856373320315672037 ) ) ;
#66049 = EDGE_CURVE ( 'NONE', #78570, #22516, #38448, .T. ) ;
#66050 = CARTESIAN_POINT ( 'NONE',  ( 4.784634885068531851, 8.146353749921887655, 0.8039021629790907841 ) ) ;
#66051 = FACE_OUTER_BOUND ( 'NONE', #11529, .T. ) ;
#66052 = CARTESIAN_POINT ( 'NONE',  ( -2.806174608348664723, 6.217694776474651519, 1.040834085586084257E-14 ) ) ;
#66053 = CARTESIAN_POINT ( 'NONE',  ( 9.598809568795314107, 10.30095870645710754, -0.7216878364870257245 ) ) ;
#66054 = CARTESIAN_POINT ( 'NONE',  ( 4.082825143736307005, 1.868653194780546922, 0.6220825103698603975 ) ) ;
#66055 = CARTESIAN_POINT ( 'NONE',  ( 1.471502243059899850, -1.820439715282649251, -1.087164402369590555 ) ) ;
#66056 = CARTESIAN_POINT ( 'NONE',  ( -6.579784621333750749, 6.570836901177822931, 0.7998128361456341429 ) ) ;
#66057 = DIRECTION ( 'NONE',  ( -1.000000000000000000, 0.000000000000000000, 0.000000000000000000 ) ) ;
#66058 = CARTESIAN_POINT ( 'NONE',  ( 3.475000000000000533, -2.595833333333334103, -2.006292185433951047 ) ) ;
#66059 = CARTESIAN_POINT ( 'NONE',  ( 5.789076383285488347, 1.657349226701849476, 1.433863557930945332 ) ) ;
#66060 = CARTESIAN_POINT ( 'NONE',  ( 5.279289720117871454, 6.257118729668095902, 1.159094902893437196 ) ) ;
#66061 = CARTESIAN_POINT ( 'NONE',  ( 3.926716319054617266, 1.828954700887480245, 0.6050711068611572818 ) ) ;
#66062 = CARTESIAN_POINT ( 'NONE',  ( -6.235860587281615075, 9.362588887548838557, -1.199719254218440723 ) ) ;
#66063 = CARTESIAN_POINT ( 'NONE',  ( 0.6920833903016985200, -1.811158644599793810, -0.2285449354127722099 ) ) ;
#66064 = CARTESIAN_POINT ( 'NONE',  ( 1.594636444620714633, -2.196503929104542951, -0.2137616909994101699 ) ) ;
#66065 = CARTESIAN_POINT ( 'NONE',  ( -6.090138087829436664, 7.032093901976294248, 0.9931326435281346843 ) ) ;
#66066 = ORIENTED_EDGE ( 'NONE', *, *, #72448, .F. ) ;
#66067 = DIRECTION ( 'NONE',  ( -1.000000000000000000, 5.578564026256503701E-16, -1.972152263052529514E-31 ) ) ;
#66068 = VERTEX_POINT ( 'NONE', #168446 ) ;
#66069 = CARTESIAN_POINT ( 'NONE',  ( 6.157084851585769236, 1.612115889470520314, -1.131004145815546424 ) ) ;
#66070 = CARTESIAN_POINT ( 'NONE',  ( 1.101004982060274751, -0.4702163980460572490, 1.884172457509038834 ) ) ;
#66071 = CARTESIAN_POINT ( 'NONE',  ( 6.204520426337317929, -1.658329656736241553, -1.591615412813138564 ) ) ;
#66073 = CARTESIAN_POINT ( 'NONE',  ( 4.276097919418925031, -0.9535845961709583651, -1.597878833905818086 ) ) ;
#66072 = CARTESIAN_POINT ( 'NONE',  ( -5.447343857640614573, 9.577261277214532242, -0.7998128361456362523 ) ) ;
#66074 = CARTESIAN_POINT ( 'NONE',  ( 7.049313524462606395, 7.188896964819984525, 0.000000000000000000 ) ) ;
#66075 = CARTESIAN_POINT ( 'NONE',  ( 11.97929049433705373, 12.22000000000000064, -0.7046979865771834106 ) ) ;
#66076 = PRESENTATION_STYLE_ASSIGNMENT (( #16267 ) ) ;
#66077 = CARTESIAN_POINT ( 'NONE',  ( -6.728924311084075960, 6.744833205886536120, 1.040834085586084257E-14 ) ) ;
#66078 = CARTESIAN_POINT ( 'NONE',  ( -4.841670253855968831, 4.821239182352949904, 0.000000000000000000 ) ) ;
#66079 = CARTESIAN_POINT ( 'NONE',  ( 0.3807642395799659130, -0.2741851280289032688, -2.174293136291181483 ) ) ;
#66080 = CARTESIAN_POINT ( 'NONE',  ( 3.877268743828266029, 6.506935386899531437, 1.082531754730558626 ) ) ;
#66081 = CARTESIAN_POINT ( 'NONE',  ( 3.294945724223604877, 7.655198976062517424, 2.499999999999998668 ) ) ;
#66082 = CARTESIAN_POINT ( 'NONE',  ( -0.4000000000000496492, 3.372708439410135206, 0.4999999999999483746 ) ) ;
#66083 = CARTESIAN_POINT ( 'NONE',  ( 1.822601884235462766, 1.703052241681313861, 0.6583118566880485911 ) ) ;
#66084 = CARTESIAN_POINT ( 'NONE',  ( -4.355193658487827690, 6.104145239700998538, -1.599625672291256295 ) ) ;
#66085 = CARTESIAN_POINT ( 'NONE',  ( 3.480872026922664286, -1.732388960670039113, -0.08070120533314528721 ) ) ;
#66086 = CARTESIAN_POINT ( 'NONE',  ( -6.204128743306504212, 7.035606015609114472, -1.046755002246579469 ) ) ;
#66087 = CARTESIAN_POINT ( 'NONE',  ( 6.509000000000039421, 2.968845098214093703, 2.453284407971462411 ) ) ;
#66088 = EDGE_CURVE ( 'NONE', #64464, #6407, #21809, .T. ) ;
#66089 = CARTESIAN_POINT ( 'NONE',  ( 10.71502147350184231, 11.39527989537399755, 0.000000000000000000 ) ) ;
#66090 = CARTESIAN_POINT ( 'NONE',  ( 6.393173274427864428, 1.585754722747900969, -0.9045919592586546543 ) ) ;
#66091 = CARTESIAN_POINT ( 'NONE',  ( 4.416819765676714304, -1.456490764316048292, 1.314424223973278183 ) ) ;
#66092 = CARTESIAN_POINT ( 'NONE',  ( -9.013473194986783454, 9.410140237106395134, -0.7998128361456291469 ) ) ;
#66093 = CARTESIAN_POINT ( 'NONE',  ( 5.452350330990040739, 9.512825819463730070, 0.7998128361456462443 ) ) ;
#66094 = CARTESIAN_POINT ( 'NONE',  ( 4.266349992362879817, 2.119992548681798095, -0.05317809935000831351 ) ) ;
#66095 = CARTESIAN_POINT ( 'NONE',  ( -8.076906825439122528, 10.44614393447756129, -1.599625672291263179 ) ) ;
#66096 = CIRCLE ( 'NONE', #45434, 0.07999999999999998779 ) ;
#66097 = CARTESIAN_POINT ( 'NONE',  ( 4.660252114795294887, 6.460046772059735432, -1.599625672291256517 ) ) ;
#66098 = CARTESIAN_POINT ( 'NONE',  ( 2.518496159030516601, 0.8812310945605882351, 1.873447404777649261 ) ) ;
#66100 = CARTESIAN_POINT ( 'NONE',  ( 0.6823417656249899377, 0.6552083336747518416, 1.181850606188755259 ) ) ;
#66099 = FACE_OUTER_BOUND ( 'NONE', #27170, .T. ) ;
#66101 = ORIENTED_EDGE ( 'NONE', *, *, #188521, .F. ) ;
#66102 = CARTESIAN_POINT ( 'NONE',  ( 2.497091698460200071, -2.273154071007321697, 0.3411551791231131059 ) ) ;
#66103 = CARTESIAN_POINT ( 'NONE',  ( 8.920901888111997025, 10.47043562662792304, 1.082531754730549967 ) ) ;
#66105 = CARTESIAN_POINT ( 'NONE',  ( 3.285556943749998737, -2.355208332855375453, -1.896917185911906500 ) ) ;
#66104 = CARTESIAN_POINT ( 'NONE',  ( 6.211043768836173484, 8.339580045099285854, 1.443375672974065660 ) ) ;
#66106 = CARTESIAN_POINT ( 'NONE',  ( -2.905110965495596944E-15, 1.687500000000013101, -1.225000000000019851 ) ) ;
#66107 = DIRECTION ( 'NONE',  ( 0.000000000000000000, 0.000000000000000000, -1.000000000000000000 ) ) ;
#66108 = ORIENTED_EDGE ( 'NONE', *, *, #89116, .F. ) ;
#66109 = CARTESIAN_POINT ( 'NONE',  ( 9.856414487010587422, 11.56186699200962487, 1.082531754730548412 ) ) ;
#66110 = CARTESIAN_POINT ( 'NONE',  ( 3.955252344019274169, -1.661368509396843995, 0.9470704235666274062 ) ) ;
#66111 = CARTESIAN_POINT ( 'NONE',  ( 4.911038474854160896, 1.501934305467259145, 0.8478258478515336982 ) ) ;
#66112 = CARTESIAN_POINT ( 'NONE',  ( 3.854704076794239764, -1.883312302057647880, -0.7212934815618715634 ) ) ;
#66113 = CARTESIAN_POINT ( 'NONE',  ( 4.922631952865072158, -1.624392127635465144, -1.626674183726722678 ) ) ;
#66114 = LINE ( 'NONE', #166857, #104816 ) ;
#66115 = CARTESIAN_POINT ( 'NONE',  ( 1.102499568101540817, -2.207063161980229005, 0.003256074490760872773 ) ) ;
#66116 = CARTESIAN_POINT ( 'NONE',  ( -3.526529353330350336, 7.128384988945109413, -0.7216878364870458196 ) ) ;
#66117 = CARTESIAN_POINT ( 'NONE',  ( 5.536323748068817885, 1.743679661707888018, 0.3015777700523143978 ) ) ;
#66119 = CARTESIAN_POINT ( 'NONE',  ( 1.693750089093534861, -0.7690282282955845927, 2.159540072747981654 ) ) ;
#66118 = CARTESIAN_POINT ( 'NONE',  ( 5.417364897112183719, 8.477953592343014932, 1.199719254218451159 ) ) ;
#66120 = CARTESIAN_POINT ( 'NONE',  ( 6.298766309436587996, 1.533505995929709487, 1.018591839899836371 ) ) ;
#66121 = CARTESIAN_POINT ( 'NONE',  ( -5.908321080505254841, 10.11506803722328129, 0.7998128361456291469 ) ) ;
#66122 = CARTESIAN_POINT ( 'NONE',  ( 6.615165563918417924, -2.126712762998611783, 0.5283135293715838232 ) ) ;
#66123 = CARTESIAN_POINT ( 'NONE',  ( -4.462568837553487100, 5.235360394347691404, -1.199719254218453823 ) ) ;
#66124 = CARTESIAN_POINT ( 'NONE',  ( 0.6801582343749726922, -0.9947916663252467373, 1.178068619123801675 ) ) ;
#66125 = CARTESIAN_POINT ( 'NONE',  ( 1.854512760316388897, 9.001999999999998892, 2.484105960264901825 ) ) ;
#66126 = CARTESIAN_POINT ( 'NONE',  ( 6.566853775770633561, 1.536883091774071453, -1.387433097640700774 ) ) ;
#66127 = CARTESIAN_POINT ( 'NONE',  ( 1.815639016007553730, -1.320828798922760949, -1.523793687088881299 ) ) ;
#66128 = CARTESIAN_POINT ( 'NONE',  ( 1.499999999999989120, 0.3062500006828158816, 0.000000000000000000 ) ) ;
#66129 = CARTESIAN_POINT ( 'NONE',  ( 5.443948574151852959, 0.7788650187186187956, -1.762213160536057144 ) ) ;
#66130 = CARTESIAN_POINT ( 'NONE',  ( 1.364683531250000303, 11.50520833367472839, -0.7879004041258355073 ) ) ;
#66131 = CARTESIAN_POINT ( 'NONE',  ( 1.881385292706035051, -2.033259550720186049, -0.8950972351880029931 ) ) ;
#66132 = ORIENTED_EDGE ( 'NONE', *, *, #15332, .F. ) ;
#66133 = CARTESIAN_POINT ( 'NONE',  ( -9.578446392664467623, -9.953004327042588528, 0.1519871474491493735 ) ) ;
#66134 = CARTESIAN_POINT ( 'NONE',  ( 9.378489572351044856, 11.96465713920816043, -1.599625672291262513 ) ) ;
#66135 = CARTESIAN_POINT ( 'NONE',  ( 0.000000000000000000, -13.99999999999999822, 0.000000000000000000 ) ) ;
#66136 = CARTESIAN_POINT ( 'NONE',  ( 5.003314770209169815, -1.731378854590956307, 0.1774945436790342501 ) ) ;
#66139 = ADVANCED_FACE ( 'NONE', ( #106706 ), #77186, .T. ) ;
#66138 = CARTESIAN_POINT ( 'NONE',  ( 3.191801227909254912, -1.315628469008291557, -1.455533501494077342 ) ) ;
#66137 = VECTOR ( 'NONE', #41577, 1000.000000000000000 ) ;
#66141 = CARTESIAN_POINT ( 'NONE',  ( -6.968527767744110868, 9.153035033833367251, 1.443375672974078761 ) ) ;
#66140 = CARTESIAN_POINT ( 'NONE',  ( 5.345992642490140057, 5.131412925860272090, 1.040834085586084257E-14 ) ) ;
#66142 = CARTESIAN_POINT ( 'NONE',  ( -5.752954180755987856, 6.096397935365156506, 0.6526304460669953844 ) ) ;
#66143 = CARTESIAN_POINT ( 'NONE',  ( 4.517028817706403743, 2.066010597640522750, 0.9224273224419097250 ) ) ;
#66144 = CARTESIAN_POINT ( 'NONE',  ( 0.6782753517312088976, -1.101985112813896883, -1.743456004656674718 ) ) ;
#66145 = CARTESIAN_POINT ( 'NONE',  ( -8.843996274815957293, 9.212417163573759282, 1.040834085586084257E-14 ) ) ;
#66146 = CARTESIAN_POINT ( 'NONE',  ( -8.631737353394710155, 13.22211067893587533, 1.040834085586084257E-14 ) ) ;
#66147 = CARTESIAN_POINT ( 'NONE',  ( 2.624197652063056996, -1.302182479666073700, -1.850046142848650321 ) ) ;
#66148 = ORIENTED_EDGE ( 'NONE', *, *, #179634, .F. ) ;
#66149 = CARTESIAN_POINT ( 'NONE',  ( 1.499999999999985123, -0.6729166659838520248, -0.8660254037844323793 ) ) ;
#66150 = CARTESIAN_POINT ( 'NONE',  ( 2.952262541859524969, 0.6266372353985818489, 1.762611677789377440 ) ) ;
#66151 = CARTESIAN_POINT ( 'NONE',  ( 1.213026639236804316, 1.670944716536880259, 0.4636423645143650241 ) ) ;
#66152 = CARTESIAN_POINT ( 'NONE',  ( 5.478137895480934105, -2.137967713159651506, -0.4810252310911074525 ) ) ;
#66153 = CARTESIAN_POINT ( 'NONE',  ( 6.651428954171766605, -1.847749378774863560, -1.382155756676258784 ) ) ;
#66154 = CARTESIAN_POINT ( 'NONE',  ( 1.498976495884283056, 1.685333290510768744, -1.185852821821014702 ) ) ;
#66155 = CARTESIAN_POINT ( 'NONE',  ( 4.611236491138351212, -1.904185011576609465, 0.3803074441277309314 ) ) ;
#66156 = CARTESIAN_POINT ( 'NONE',  ( -5.395781948114519722, 5.397426482329451325, 0.000000000000000000 ) ) ;
#66157 = CARTESIAN_POINT ( 'NONE',  ( 6.907498162232361238, -0.4094499450241483318, 1.831839262316947270 ) ) ;
#66158 = CARTESIAN_POINT ( 'NONE',  ( 0.9062500000000004441, 1.895863743164069470, -0.7852924748300356139 ) ) ;
#66159 = CARTESIAN_POINT ( 'NONE',  ( 4.055251984284337752, 7.519160923078652026, -0.4935718261673445184 ) ) ;
#66160 = CARTESIAN_POINT ( 'NONE',  ( 6.292342264464226176, -1.899326897351862664, 0.6766127494588560776 ) ) ;
#66162 = ADVANCED_FACE ( 'NONE', ( #201973 ), #156839, .T. ) ;
#66161 = CARTESIAN_POINT ( 'NONE',  ( 4.773879485787624333, 4.742149952939897162, -0.7216878364870357165 ) ) ;
#66163 = CARTESIAN_POINT ( 'NONE',  ( 0.6801582343749865700, 1.307291667008089853, -1.178068619123883165 ) ) ;
#66164 = CARTESIAN_POINT ( 'NONE',  ( 5.010388774477189777, -1.913804350592800629, 0.6351971752796632398 ) ) ;
#66165 = CARTESIAN_POINT ( 'NONE',  ( -10.50487009249003378, 11.15010328419353947, 0.7998128361456462443 ) ) ;
#66166 = CARTESIAN_POINT ( 'NONE',  ( 7.151035956204054855, 10.43029348462504124, 1.199719254218460707 ) ) ;
#66167 = CARTESIAN_POINT ( 'NONE',  ( 3.528865121306874464, 7.339036084825155015, -0.7998128361456362523 ) ) ;
#66169 = DIRECTION ( 'NONE',  ( -1.000000000000000000, 0.000000000000000000, 0.000000000000000000 ) ) ;
#66168 = CARTESIAN_POINT ( 'NONE',  ( 2.226930044512597906, -0.0006860120723567450030, 1.825872481329051222 ) ) ;
#66170 = CARTESIAN_POINT ( 'NONE',  ( 0.000000000000000000, 12.31951671548121219, 0.000000000000000000 ) ) ;
#66171 = CARTESIAN_POINT ( 'NONE',  ( 11.86145016429273191, 13.40000000000000036, 1.099999999999996758 ) ) ;
#66172 = ORIENTED_EDGE ( 'NONE', *, *, #66555, .F. ) ;
#66173 = CARTESIAN_POINT ( 'NONE',  ( -5.438229012412890917, 8.398332043573416783, -1.082531754730549967 ) ) ;
#66174 = UNCERTAINTY_MEASURE_WITH_UNIT (LENGTH_MEASURE( 1.000000000000000082E-05 ), #132509, 'distance_accuracy_value', 'NONE');
#66175 = DIRECTION ( 'NONE',  ( 0.000000000000000000, 1.000000000000000000, 0.000000000000000000 ) ) ;
#66176 = CARTESIAN_POINT ( 'NONE',  ( -8.320953590485107298, 10.73086516036454618, 1.599625672291269396 ) ) ;
#66177 = CARTESIAN_POINT ( 'NONE',  ( 0.1936255187755825669, 1.883021768735486434, -0.7310382463305180600 ) ) ;
#66178 = CARTESIAN_POINT ( 'NONE',  ( 6.498696386931579028, -2.177790866848747342, -0.4366942510913833231 ) ) ;
#66179 = VERTEX_POINT ( 'NONE', #169511 ) ;
#66180 = CARTESIAN_POINT ( 'NONE',  ( -5.074494633264801990, 9.142270515442742607, 0.7998128361456291469 ) ) ;
#66181 = CARTESIAN_POINT ( 'NONE',  ( 4.333802657862601215, 8.207853534148366492, 0.7998128361456462443 ) ) ;
#66182 = CARTESIAN_POINT ( 'NONE',  ( 6.051650376505027573, 0.6007964193008934473, -1.971360088487213780 ) ) ;
#66183 = CARTESIAN_POINT ( 'NONE',  ( 5.485000066852382616, -2.016597020608828839, 0.002808655738886777897 ) ) ;
#66184 = VERTEX_POINT ( 'NONE', #87197 ) ;
#66185 = ORIENTED_EDGE ( 'NONE', *, *, #150826, .T. ) ;
#66186 = ORIENTED_EDGE ( 'NONE', *, *, #32339, .F. ) ;
#66187 = DIRECTION ( 'NONE',  ( 0.000000000000000000, -1.496258514059622730E-16, 1.000000000000000000 ) ) ;
#66188 = CARTESIAN_POINT ( 'NONE',  ( 1.737499999999999378, -1.122916665710751882, -3.009438278150925683 ) ) ;
#66189 = VECTOR ( 'NONE', #18916, 1000.000000000000000 ) ;
#66191 = CARTESIAN_POINT ( 'NONE',  ( -1.244150428499003036, 3.178773246564667421, -0.7749999999999918066 ) ) ;
#66190 = CARTESIAN_POINT ( 'NONE',  ( -4.932134020321308654, 8.976183133675331050, 0.7998128361456291469 ) ) ;
#66192 = CARTESIAN_POINT ( 'NONE',  ( 6.592372495380235620, 6.775069446727209233, 0.2122460957004346782 ) ) ;
#66193 = CARTESIAN_POINT ( 'NONE',  ( 5.641953822799152363, -0.04667112846407085042, -2.015725140939367943 ) ) ;
#66194 = CARTESIAN_POINT ( 'NONE',  ( 5.015489797737916255, -0.9877249803392706973, -1.553577481828890106 ) ) ;
#66195 = CIRCLE ( 'NONE', #121671, 0.07999999999999993228 ) ;
#66196 = CARTESIAN_POINT ( 'NONE',  ( -3.741289556128929661, 7.428763123923387113, 2.448390356388095768 ) ) ;
#66197 = CARTESIAN_POINT ( 'NONE',  ( 3.299772510450727836, 1.819142665603549425, 1.419829399881943566 ) ) ;
#66198 = CARTESIAN_POINT ( 'NONE',  ( 7.693325821111733021, 7.940244644243982464, -0.7998128361456341429 ) ) ;
#66199 = CARTESIAN_POINT ( 'NONE',  ( 4.780646861661003832, -2.095393720161139228, -0.5303334973314683953 ) ) ;
#66200 = CARTESIAN_POINT ( 'NONE',  ( 8.457588896826466751, 8.761608555919362828, 1.040834085586084257E-14 ) ) ;
#66201 = CARTESIAN_POINT ( 'NONE',  ( 0.9779546479521743496, -1.895077795344397575, -0.4239509559331255395 ) ) ;
#66202 = CARTESIAN_POINT ( 'NONE',  ( -3.262708522383007903, 6.958243709422141876, 1.040834085586084257E-14 ) ) ;
#66203 = CARTESIAN_POINT ( 'NONE',  ( 0.6823417656249882723, 2.926041667008084879, -1.181850606188754593 ) ) ;
#66204 = CARTESIAN_POINT ( 'NONE',  ( -4.305596300791617814, 7.180890229968955651, 1.199719254218452935 ) ) ;
#66205 = CARTESIAN_POINT ( 'NONE',  ( 3.485083742438867649, 1.691615344724434200, -0.7988839237506044633 ) ) ;
#66206 =( BOUNDED_SURFACE ( )  B_SPLINE_SURFACE ( 3, 2, ( 
 ( #157564, #40611, #75233 ),
 ( #106716, #141343, #142401 ),
 ( #207357, #190036, #58978 ),
 ( #191091, #126198, #109937 ) ),
 .UNSPECIFIED., .F., .F., .T. ) 
 B_SPLINE_SURFACE_WITH_KNOTS ( ( 4, 4 ),
 ( 3, 3 ),
 ( 0.004991389062828482590, 0.008017777006561210146 ),
 ( 0.000000000000000000, 1.000000000000000000 ),
 .UNSPECIFIED. ) 
 GEOMETRIC_REPRESENTATION_ITEM ( )  RATIONAL_B_SPLINE_SURFACE ( (
 ( 1.000000000000000000, 0.7184380228464046780, 1.000000000000000000),
 ( 1.000000000000000000, 0.7185467277397590280, 1.000000000000000000),
 ( 1.000000000000000000, 0.7186585579880989672, 1.000000000000000000),
 ( 1.000000000000000000, 0.7187737999613676987, 1.000000000000000000) ) ) 
 REPRESENTATION_ITEM ( '' )  SURFACE ( )  );
#66209 = CARTESIAN_POINT ( 'NONE',  ( -6.180537922983287302, 8.303989891604203422, -1.599625672291271394 ) ) ;
#66208 = CARTESIAN_POINT ( 'NONE',  ( 1.499999999999987121, -1.214583332650518432, 0.8660254037844524744 ) ) ;
#66207 = CARTESIAN_POINT ( 'NONE',  ( 1.546972149855216472, 0.1906517044060058730, 1.902890584052991940 ) ) ;
#66210 = CARTESIAN_POINT ( 'NONE',  ( 2.543839704335303153, -1.636039663378138886, -1.481301067789652537 ) ) ;
#66211 = CARTESIAN_POINT ( 'NONE',  ( 1.250000000000037526, 8.500000000000000000, 12.00100000000000122 ) ) ;
#66212 = DIRECTION ( 'NONE',  ( -0.6507913734559640506, -0.7592566023653004592, 0.000000000000000000 ) ) ;
#66213 = CARTESIAN_POINT ( 'NONE',  ( 6.577113915960825175, 8.766661883411348555, -1.443375672974078761 ) ) ;
#66214 = CARTESIAN_POINT ( 'NONE',  ( -4.647747731386360215, 4.316793862905830892, 0.7998128361456341429 ) ) ;
#66215 = CARTESIAN_POINT ( 'NONE',  ( -7.580417283372126391, 8.016444050121833698, 0.7216878364870317197 ) ) ;
#66216 = CARTESIAN_POINT ( 'NONE',  ( 0.9132762689940625567, -0.2936195204277583515, 1.949272377766637643 ) ) ;
#66217 = CARTESIAN_POINT ( 'NONE',  ( 0.1832606990049808204, -2.239562280805599492, -0.5557475372391910140 ) ) ;
#66218 = CARTESIAN_POINT ( 'NONE',  ( 1.609737659951641309, 0.5726723138891121057, -1.876404140693301414 ) ) ;
#66219 = CARTESIAN_POINT ( 'NONE',  ( 4.873915701820059176, -2.023805994998853830, 0.3972042427494940076 ) ) ;
#66220 = CARTESIAN_POINT ( 'NONE',  ( 3.877268743828258479, 7.467304601200877023, 0.7216878364870298324 ) ) ;
#66221 = EDGE_CURVE ( 'NONE', #161998, #127879, #190438, .T. ) ;
#66222 = CARTESIAN_POINT ( 'NONE',  ( 6.879836604291781121, 6.991173891287354003, -0.7998128361456341429 ) ) ;
#66223 = VERTEX_POINT ( 'NONE', #40600 ) ;
#66224 = CARTESIAN_POINT ( 'NONE',  ( 0.6823417656249917140, 4.655208333674755394, 1.181850606188765695 ) ) ;
#66225 = CARTESIAN_POINT ( 'NONE',  ( -6.773376349083140013, 7.849261790823902629, -6.661184041420947111 ) ) ;
#66226 = CARTESIAN_POINT ( 'NONE',  ( 3.836594282542909795, 6.459481848733281240, 1.082531754730558626 ) ) ;
#66227 = CARTESIAN_POINT ( 'NONE',  ( 1.428853742479018862, -1.379120938454091227, 1.676725645940212894 ) ) ;
#66229 = CARTESIAN_POINT ( 'NONE',  ( 6.110883706712432861, -0.2185277653131960651, 1.828168259763853776 ) ) ;
#66228 = CARTESIAN_POINT ( 'NONE',  ( 9.486277548414619787, -9.200719317737716452, -0.5196196971346837001 ) ) ;
#66230 = DIRECTION ( 'NONE',  ( -1.000000000000000000, 0.000000000000000000, 0.000000000000000000 ) ) ;
#66231 = CARTESIAN_POINT ( 'NONE',  ( -11.78331023100045627, 12.30000000000000071, -1.800000000000001155 ) ) ;
#66232 = CARTESIAN_POINT ( 'NONE',  ( 1.669004442688322154, 0.1428430569143137041, -1.865171992484420338 ) ) ;
#66233 = CARTESIAN_POINT ( 'NONE',  ( 5.290363030411685763, -2.144575937485785566, -0.2703735795691122323 ) ) ;
#66234 = CARTESIAN_POINT ( 'NONE',  ( -6.110283559904478246, 6.013173453705326743, 0.3066926896367061506 ) ) ;
#66235 = CARTESIAN_POINT ( 'NONE',  ( 0.000000000000000000, -0.6185895741317448682, 6.264285714285709794 ) ) ;
#66236 = CARTESIAN_POINT ( 'NONE',  ( 6.435676556713933572, 6.878741676577107889, -0.7109887800627444632 ) ) ;
#66237 = CARTESIAN_POINT ( 'NONE',  ( 0.6823417656249917140, 5.405208333674749177, 1.181850606188765695 ) ) ;
#66238 = CARTESIAN_POINT ( 'NONE',  ( 1.084454188491505988, -1.212558158303608913, 1.478703618145213783 ) ) ;
#66239 = CARTESIAN_POINT ( 'NONE',  ( 3.186155166506371650, -1.743393047566743181, -0.3038327287053984027 ) ) ;
#66240 = CARTESIAN_POINT ( 'NONE',  ( 0.7680391878876170475, 1.910087531778673187, -0.09433495293535018589 ) ) ;
#66242 = CARTESIAN_POINT ( 'NONE',  ( 5.132410944242819184, 0.5605724621733051416, 1.831730044279370029 ) ) ;
#66241 = CARTESIAN_POINT ( 'NONE',  ( 2.953507107040155066, -3.210470589277563569, 1.499658823967387145 ) ) ;
#66243 = B_SPLINE_CURVE_WITH_KNOTS ( 'NONE', 3,
 ( #137832, #105339, #86931, #123796, #172458, #135693 ),
 .UNSPECIFIED., .F., .F.,
 ( 4, 2, 4 ),
 ( 0.000000000000000000, 0.0003258677429877278493, 0.0006517354859754556987 ),
 .UNSPECIFIED. ) ;
#66244 = CARTESIAN_POINT ( 'NONE',  ( 6.039503384146654774, 1.820429283694004141, -0.7522724601281975954 ) ) ;
#66245 = CARTESIAN_POINT ( 'NONE',  ( -0.7500000000000215383, 4.441666666666691299, 1.299038105676671107 ) ) ;
#66246 = CARTESIAN_POINT ( 'NONE',  ( 0.6684183810189650021, 2.117893379942568988, -0.1100008709709817956 ) ) ;
#66247 = LINE ( 'NONE', #84664, #65231 ) ;
#66248 = CARTESIAN_POINT ( 'NONE',  ( 4.311305935566238645, -0.3199438451688824125, 1.842931056080451935 ) ) ;
#66250 = VERTEX_POINT ( 'NONE', #10209 ) ;
#66249 = CARTESIAN_POINT ( 'NONE',  ( 0.8557438351849018243, 1.823752217391808372, -0.08689656109241167270 ) ) ;
#66252 = FACE_OUTER_BOUND ( 'NONE', #17327, .T. ) ;
#66251 = CARTESIAN_POINT ( 'NONE',  ( 4.354274438496381627, 2.206422198305586058, -0.05263853172451230661 ) ) ;
#66253 = CARTESIAN_POINT ( 'NONE',  ( 0.6823417656249917140, 5.155208333674749177, 1.181850606188765695 ) ) ;
#66254 = CARTESIAN_POINT ( 'NONE',  ( 2.084505489600170680, 1.189443612574309084, -1.685003561244757364 ) ) ;
#66255 = CARTESIAN_POINT ( 'NONE',  ( 7.135668919494039031, 7.219368582364847242, 1.040834085586084257E-14 ) ) ;
#66256 = CARTESIAN_POINT ( 'NONE',  ( -9.154780037725563702, 11.70366268214508487, 1.599625672291281386 ) ) ;
#66257 = CARTESIAN_POINT ( 'NONE',  ( 0.4499999999999712563, 3.949999999999981526, -6.938893903907228378E-15 ) ) ;
#66258 = DIRECTION ( 'NONE',  ( 0.000000000000000000, 0.000000000000000000, -1.000000000000000000 ) ) ;
#66259 = PRESENTATION_LAYER_ASSIGNMENT (  '', '', ( #73224 ) ) ;
#66260 = CARTESIAN_POINT ( 'NONE',  ( 6.504189997394580480, -0.8109953713257547214, 1.730197269205424160 ) ) ;
#66261 = VERTEX_POINT ( 'NONE', #12334 ) ;
#66262 = CARTESIAN_POINT ( 'NONE',  ( 3.895033709675084221, 0.3008086390649654662, 2.048262060622765279 ) ) ;
#66263 = CARTESIAN_POINT ( 'NONE',  ( -0.7499999999999972244, 5.858333333333353821, -1.299038105676652011 ) ) ;
#66264 = CARTESIAN_POINT ( 'NONE',  ( 1.950665695202157046, 0.6760947502928333908, 2.053231632317173538 ) ) ;
#66265 = CARTESIAN_POINT ( 'NONE',  ( -6.074251926901598431, 7.043194046877760961, -1.007762736454496988 ) ) ;
#66266 = CARTESIAN_POINT ( 'NONE',  ( 1.858075313305072473, 0.7708903827231723405, -1.866970155298973921 ) ) ;
#66267 = CARTESIAN_POINT ( 'NONE',  ( 4.812781342726857758, 6.637997537979888563, 1.443375672974062551 ) ) ;
#66268 = EDGE_CURVE ( 'NONE', #72818, #154255, #127263, .T. ) ;
#66269 = EDGE_LOOP ( 'NONE', ( #11860, #102884, #135565, #7699 ) ) ;
#66271 = CARTESIAN_POINT ( 'NONE',  ( 8.595506201384013778, 10.09080732544527592, 1.082531754730558626 ) ) ;
#66270 = CARTESIAN_POINT ( 'NONE',  ( -3.475000000000000533, -3.849999999999999201, 0.000000000000000000 ) ) ;
#66272 = CARTESIAN_POINT ( 'NONE',  ( 0.01853512708399032358, 14.54363643945355555, 11.97163374478178710 ) ) ;
#66273 = CARTESIAN_POINT ( 'NONE',  ( -0.2351498743046881446, -0.1506043639611966134, -1.983733596389973597 ) ) ;
#66274 = CARTESIAN_POINT ( 'NONE',  ( 6.539320575229276677, 6.035451701470580410, 2.698157228745074576 ) ) ;
#66275 = CARTESIAN_POINT ( 'NONE',  ( 4.405938146338868933, -0.9375679901368579872, -1.981035393479456008 ) ) ;
#66276 = CARTESIAN_POINT ( 'NONE',  ( 0.7499999999999902300, 3.597916667349487785, -1.299038105676658228 ) ) ;
#66277 = CARTESIAN_POINT ( 'NONE',  ( 4.043146078444789460, 0.09904687726844901841, 1.909973672635330910 ) ) ;
#66278 = CARTESIAN_POINT ( 'NONE',  ( -4.928552533767591726, 5.708731696605642725, 1.199719254218462483 ) ) ;
#66279 = ADVANCED_FACE ( 'NONE', ( #141335, #42749 ), #192149, .F. ) ;
#66280 = CARTESIAN_POINT ( 'NONE',  ( 5.327991180046175224, 5.318337252916401248, -0.7216878364870207285 ) ) ;
#66282 = CARTESIAN_POINT ( 'NONE',  ( 2.548454031204652637, -1.388473193742698619, 1.462459214312331168 ) ) ;
#66281 = CARTESIAN_POINT ( 'NONE',  ( -10.10046125205658463, 11.84658821789661509, -1.082531754730537976 ) ) ;
#66283 = CARTESIAN_POINT ( 'NONE',  ( -1.402160292154681736E-14, 12.23437500034140335, 1.575800808251682339 ) ) ;
#66285 = CARTESIAN_POINT ( 'NONE',  ( -6.154475385960665790, 6.144919136567696505, 0.000000000000000000 ) ) ;
#66284 = CARTESIAN_POINT ( 'NONE',  ( 0.8379086502938500880, 0.9226890658239239595, -2.098657079483890353 ) ) ;
#66286 = CARTESIAN_POINT ( 'NONE',  ( 4.489066604428880503, 1.540008836363685241, -0.7767696631951895858 ) ) ;
#66287 = CARTESIAN_POINT ( 'NONE',  ( -0.1394461523061196473, 5.719344608737997326, -2.874279450258274249 ) ) ;
#66288 = CARTESIAN_POINT ( 'NONE',  ( 3.551346171775753735, 6.230655402791975384, 1.199719254218462483 ) ) ;
#66289 = CIRCLE ( 'NONE', #94027, 1.872309607372811158 ) ;
#66290 = CARTESIAN_POINT ( 'NONE',  ( -1.257539916218605169, 2.922412844624491246, -0.7749999999999988010 ) ) ;
#66291 = CARTESIAN_POINT ( 'NONE',  ( 0.7659737006216191801, -1.952758744216346765, 0.1886366088557633325 ) ) ;
#66292 = CARTESIAN_POINT ( 'NONE',  ( 0.7779422811538607707, -1.042605501850740080, 1.552959968518424771 ) ) ;
#66293 = CARTESIAN_POINT ( 'NONE',  ( 3.354752944377597856, 6.001296637494123232, -1.199719254218446718 ) ) ;
#66294 = CARTESIAN_POINT ( 'NONE',  ( 0.1755611466353291517, 7.629137130509040077, -2.844001552353003781 ) ) ;
#66295 = ORIENTED_EDGE ( 'NONE', *, *, #78986, .T. ) ;
#66296 =( BOUNDED_CURVE ( )  B_SPLINE_CURVE ( 2, ( #134795, #116440, #37265, #20983, #167276 ),
 .UNSPECIFIED., .F., .T. ) 
 B_SPLINE_CURVE_WITH_KNOTS ( ( 3, 2, 3 ),
 ( 0.3228721300350675949, 0.3273809523809523836, 0.3303571428571428492 ),
 .UNSPECIFIED. ) 
 CURVE ( )  GEOMETRIC_REPRESENTATION_ITEM ( )  RATIONAL_B_SPLINE_CURVE ( ( 0.9507769454952199606, 0.8985166342628003733, 1.000000000000000000, 0.9330127018922194093, 0.9330127018922194093 ) ) 
 REPRESENTATION_ITEM ( '' )  );
#66297 = EDGE_LOOP ( 'NONE', ( #49320, #209911, #21703, #110114 ) ) ;
#66298 = CARTESIAN_POINT ( 'NONE',  ( 4.828658830049068484, 1.245459390374216380, -1.315641719143684885 ) ) ;
#66299 = ORIENTED_EDGE ( 'NONE', *, *, #192938, .F. ) ;
#66300 = CARTESIAN_POINT ( 'NONE',  ( 4.518610335104485287, 8.493738834255713854, 0.000000000000000000 ) ) ;
#66301 = CARTESIAN_POINT ( 'NONE',  ( 7.487360338304382523, -6.465328379374282619, -7.487360338304409169 ) ) ;
#66302 = CARTESIAN_POINT ( 'NONE',  ( 5.496671973222438723, -1.768653292081886708, -0.3907654940887676509 ) ) ;
#66303 = CARTESIAN_POINT ( 'NONE',  ( 5.844973620822830895, 8.872867420051733234, 1.082531754730549967 ) ) ;
#66304 = CARTESIAN_POINT ( 'NONE',  ( 7.720982897393566802, -5.823938088759704534, -7.834948825496931057 ) ) ;
#66305 = CARTESIAN_POINT ( 'NONE',  ( 5.394965581569445057, 6.295244270701876310, -1.058425382943289028 ) ) ;
#66306 = ORIENTED_EDGE ( 'NONE', *, *, #97869, .F. ) ;
#66307 = VECTOR ( 'NONE', #49329, 1000.000000000000000 ) ;
#66309 = CARTESIAN_POINT ( 'NONE',  ( 9.215791728987056786, 11.77484298861683598, -1.599625672291262513 ) ) ;
#66308 = CARTESIAN_POINT ( 'NONE',  ( 6.144940932578938586, -0.2738450275633330100, -1.840644705263774217 ) ) ;
#66310 = CARTESIAN_POINT ( 'NONE',  ( 3.339363673285804079, 0.4624358396413058570, -1.858828564233159675 ) ) ;
#66311 = CARTESIAN_POINT ( 'NONE',  ( 3.906157654512973920, 7.571284673658210451, -0.7216878364870253915 ) ) ;
#66312 = ADVANCED_FACE ( 'NONE', ( #157553 ), #190027, .F. ) ;
#66313 = CARTESIAN_POINT ( 'NONE',  ( 3.019342412789784547, 6.452475500722323787, 0.1501914610189964416 ) ) ;
#66314 = FILL_AREA_STYLE ('',( #103119 ) ) ;
#66315 = CARTESIAN_POINT ( 'NONE',  ( 6.643132081016124069, 7.813037518349371879, 1.082531754730558626 ) ) ;
#66317 = CARTESIAN_POINT ( 'NONE',  ( 5.524650688480493343, 0.4156912398748518478, 2.075975271109116171 ) ) ;
#66316 = CARTESIAN_POINT ( 'NONE',  ( -10.03267048443264109, 11.76749898900197877, 1.082531754730558626 ) ) ;
#66318 = CARTESIAN_POINT ( 'NONE',  ( 0.2335756976950612018, -1.975703151049061024, 0.8776370805363906680 ) ) ;
#66319 = CARTESIAN_POINT ( 'NONE',  ( -5.957882158562513908, 5.915560371269843465, -0.7998128361456362523 ) ) ;
#66320 = CARTESIAN_POINT ( 'NONE',  ( 4.686278372178935392, 5.496354851410763409, 1.199719254218452047 ) ) ;
#66321 = CARTESIAN_POINT ( 'NONE',  ( 0.6041866639863550104, -0.6101368697832668664, -1.720745249832649870 ) ) ;
#66322 = CARTESIAN_POINT ( 'NONE',  ( -3.469997250093771246, 6.135748327496311383, -1.199719254218452935 ) ) ;
#66323 = CARTESIAN_POINT ( 'NONE',  ( 3.610199614654508338, -0.7391254383575728282, -1.669438027971142047 ) ) ;
#66324 = CARTESIAN_POINT ( 'NONE',  ( 9.545480790392691262, 12.19169623295751315, -8.744449518525772902 ) ) ;
#66325 = VERTEX_POINT ( 'NONE', #44882 ) ;
#66326 = CARTESIAN_POINT ( 'NONE',  ( 3.033609518001907368, 1.871031307821906964, -0.6153852250644732402 ) ) ;
#66327 = CARTESIAN_POINT ( 'NONE',  ( 5.126486101458046285, 0.1468865524030492364, 1.936578770319798748 ) ) ;
#66328 = CARTESIAN_POINT ( 'NONE',  ( -5.340986169140711226, 5.195848383611072485, 0.000000000000000000 ) ) ;
#66329 = CARTESIAN_POINT ( 'NONE',  ( 7.126746022638799971, 8.343567110280638133, 1.199719254218452047 ) ) ;
#66330 = CARTESIAN_POINT ( 'NONE',  ( -6.343417644159658586, 6.506394916542938667, -2.500000000000000444 ) ) ;
#66331 = CARTESIAN_POINT ( 'NONE',  ( 2.420441844550869526, -0.7335502799032425081, -1.766186906296034698 ) ) ;
#66332 = B_SPLINE_CURVE_WITH_KNOTS ( 'NONE', 3,
 ( #140216, #107755, #75188, #158575, #89315, #125090 ),
 .UNSPECIFIED., .F., .F.,
 ( 4, 2, 4 ),
 ( 0.000000000000000000, 0.0003779448103413554443, 0.0007558896206827108886 ),
 .UNSPECIFIED. ) ;
#66333 = CARTESIAN_POINT ( 'NONE',  ( 6.021928883684827483, 6.074059740061504620, -0.5497475987105825412 ) ) ;
#66334 = CARTESIAN_POINT ( 'NONE',  ( -4.080641063585716211, 5.783833847506671511, -1.249999999999999334 ) ) ;
#66335 = CARTESIAN_POINT ( 'NONE',  ( 5.713835393516482952, 5.630839145382857680, 0.7998128361456352531 ) ) ;
#66336 = CARTESIAN_POINT ( 'NONE',  ( 5.508690485854129903, 5.321227076451600091, 1.040834085586084257E-14 ) ) ;
#66337 = CARTESIAN_POINT ( 'NONE',  ( -15.75000000000000000, 9.799999999999998934, -0.7000000000000009548 ) ) ;
#66338 = CARTESIAN_POINT ( 'NONE',  ( 4.863791234866603475, 1.805334366393744450, -0.2710410529033688842 ) ) ;
#66339 = CARTESIAN_POINT ( 'NONE',  ( 1.346235217667652417, -0.9325981557438846048, 1.848514419461377845 ) ) ;
#66340 = CARTESIAN_POINT ( 'NONE',  ( -7.673551755654729689, 11.89630144833179060, 0.7216878364870458196 ) ) ;
#66341 = COLOUR_RGB ( '', 0.72549020, 0.75294118, 0.79215686) ;
#66342 = CARTESIAN_POINT ( 'NONE',  ( -6.253183873137761140, 7.001293123865100831, 0.9949814792902436089 ) ) ;
#66343 = CARTESIAN_POINT ( 'NONE',  ( 11.48243876534946217, 11.29999999999999893, -3.200000000000001510 ) ) ;
#66344 = EDGE_CURVE ( 'NONE', #155158, #77611, #102601, .T. ) ;
#66345 = CARTESIAN_POINT ( 'NONE',  ( 5.471519871388384360, 1.802534880541529994, -0.5000026934619330454 ) ) ;
#66346 = CARTESIAN_POINT ( 'NONE',  ( 6.564118927310645724, 10.80988918183778225, -0.7998128361456291469 ) ) ;
#66347 = AXIS2_PLACEMENT_3D ( 'NONE', #176648, #144196, #95425 ) ;
#66348 = CARTESIAN_POINT ( 'NONE',  ( -5.382750679825375251, 6.238629533673094585, -1.199719254218446718 ) ) ;
#66349 = CARTESIAN_POINT ( 'NONE',  ( 2.530568227245037605, 6.104080031761181857, 0.000000000000000000 ) ) ;
#66350 = CARTESIAN_POINT ( 'NONE',  ( 1.364683531249997417, 10.29687500034139802, 2.602085213965210642E-15 ) ) ;
#66351 = CARTESIAN_POINT ( 'NONE',  ( -5.087333953625788219, 6.958308917361963886, 1.599625672291267398 ) ) ;
#66352 = CARTESIAN_POINT ( 'NONE',  ( 3.979481780810941949, 4.601482484822914998, 1.199719254218464037 ) ) ;
#66353 = CARTESIAN_POINT ( 'NONE',  ( -5.935437387732586778, 10.14670372898850381, -0.7998128361456362523 ) ) ;
#66354 = CARTESIAN_POINT ( 'NONE',  ( -6.878064000834399394, 6.918829510595249310, -0.7998128361456291469 ) ) ;
#66355 = CARTESIAN_POINT ( 'NONE',  ( 6.596539238361469160, 2.146192635953731553, 0.3271905807876190897 ) ) ;
#66356 = CARTESIAN_POINT ( 'NONE',  ( 2.021262997689095897, -1.889599275135231071, 0.9552078933684378104 ) ) ;
#66357 = CARTESIAN_POINT ( 'NONE',  ( 9.576136569953906275, 10.06658084123472641, 0.000000000000000000 ) ) ;
#66358 = CARTESIAN_POINT ( 'NONE',  ( 0.5159288176862960595, 6.781431689740628599, 3.543831299045886229 ) ) ;
#66359 = CARTESIAN_POINT ( 'NONE',  ( 5.823117640241993520, -1.869163851432435575, -0.8903994044791310181 ) ) ;
#66360 = CARTESIAN_POINT ( 'NONE',  ( 4.026354976812863917, 7.791716866330316904, -0.3671166487079768892 ) ) ;
#66361 = CARTESIAN_POINT ( 'NONE',  ( 5.721177635286841756, 6.737423998331861341, -1.082531754730543083 ) ) ;
#66362 = CARTESIAN_POINT ( 'NONE',  ( -4.524619481383255426, 4.928362264877893750, 0.8618174646245332360 ) ) ;
#66363 = CARTESIAN_POINT ( 'NONE',  ( 2.941680396524527286, 0.8243158943622121981, -2.139088555740241038 ) ) ;
#66365 = CARTESIAN_POINT ( 'NONE',  ( 0.000000000000000000, 13.79999999999999893, 0.000000000000000000 ) ) ;
#66364 = CARTESIAN_POINT ( 'NONE',  ( -4.161989969715274462, 4.726297878971393196, -2.420000000000000373 ) ) ;
#66366 = CARTESIAN_POINT ( 'NONE',  ( 2.513799616133075343, -0.5961229146635020903, 1.817204401178821760 ) ) ;
#66367 = EDGE_LOOP ( 'NONE', ( #60187, #196410, #79026, #51512 ) ) ;
#66368 = CARTESIAN_POINT ( 'NONE',  ( 6.588899466117086767, 10.63087377720454363, 1.040834085586084257E-14 ) ) ;
#66369 = CARTESIAN_POINT ( 'NONE',  ( 0.4396980093101590659, -1.910362728465137439, 0.6353400594101745735 ) ) ;
#66370 = CARTESIAN_POINT ( 'NONE',  ( 0.8659734994756922433, -1.952832785578303199, 0.1866259229855102009 ) ) ;
#66371 = CARTESIAN_POINT ( 'NONE',  ( 3.763657168278617959, 3.180244510940670288, -2.446973152615704361 ) ) ;
#66372 = CARTESIAN_POINT ( 'NONE',  ( -6.367525699912501835, 10.58053041653993098, -0.7998128361456291469 ) ) ;
#66373 = CARTESIAN_POINT ( 'NONE',  ( -1.642778471875000035, -0.6052083328553746755, -2.845375778867859751 ) ) ;
#66375 = CARTESIAN_POINT ( 'NONE',  ( 2.412676795855304590, 1.579722209848779313, 0.7981720169879211735 ) ) ;
#66374 = CARTESIAN_POINT ( 'NONE',  ( 3.380887635974954453, 1.889918501611790536, -0.8941524261326051493 ) ) ;
#66376 = CARTESIAN_POINT ( 'NONE',  ( 3.985733972293228344, 7.593847367743336463, 1.040834085586084257E-14 ) ) ;
#66378 = CARTESIAN_POINT ( 'NONE',  ( 5.490252784120214002, -0.5523235152877626897, -2.224609438220140234 ) ) ;
#66377 = CARTESIAN_POINT ( 'NONE',  ( 0.07999999999999327094, -8.407420853759283830, 10.91970695577496286 ) ) ;
#66379 = CARTESIAN_POINT ( 'NONE',  ( 3.239928156850964580, 0.4239778953066320466, 1.687749859276384878 ) ) ;
#66380 = CARTESIAN_POINT ( 'NONE',  ( 2.920892028740289081, 5.495125569250587816, 1.199719254218452047 ) ) ;
#66381 = AXIS2_PLACEMENT_3D ( 'NONE', #40785, #154522, #138279 ) ;
#66382 = CARTESIAN_POINT ( 'NONE',  ( 5.411639590510088027, 6.342609606130419131, -1.199719254218452047 ) ) ;
#66383 = CARTESIAN_POINT ( 'NONE',  ( 2.917049273830461864, 0.5812832248327322038, 1.633648419047509792 ) ) ;
#66384 = CARTESIAN_POINT ( 'NONE',  ( 3.508415132820621007, 2.171350060761201295, 0.003086831990101178078 ) ) ;
#66385 = CARTESIAN_POINT ( 'NONE',  ( 2.846322183865124700, 5.408127416896231665, -1.199719254218446718 ) ) ;
#66386 = CARTESIAN_POINT ( 'NONE',  ( 5.577361344084559747, 1.530155114678043660, 1.313547687611632764 ) ) ;
#66387 = CARTESIAN_POINT ( 'NONE',  ( 0.1249994045006353610, -2.052053476427470269, 7.016016019767730053E-15 ) ) ;
#66388 = CARTESIAN_POINT ( 'NONE',  ( -1.499999999999997780, 3.681250000682819046, 1.214306433183764966E-14 ) ) ;
#66389 = CARTESIAN_POINT ( 'NONE',  ( 2.538006180297863068, 0.9099634639774205613, -1.697936525022441190 ) ) ;
#66390 = CARTESIAN_POINT ( 'NONE',  ( -1.500000000000008216, 9.281250000682799595, 3.469446951953614189E-15 ) ) ;
#66391 = CARTESIAN_POINT ( 'NONE',  ( 5.168325547630102434, 2.218848025724213802, -0.1096118590232265239 ) ) ;
#66392 = ORIENTED_EDGE ( 'NONE', *, *, #55251, .F. ) ;
#66393 = CARTESIAN_POINT ( 'NONE',  ( 6.983263157960366563, 2.056882910316945701, 2.252511522010155698 ) ) ;
#66394 = CARTESIAN_POINT ( 'NONE',  ( 1.499999999999989120, 1.525000000000019451, 0.000000000000000000 ) ) ;
#66395 = CARTESIAN_POINT ( 'NONE',  ( 7.461064606222022277, 7.598996883547496139, 1.040834085586084257E-14 ) ) ;
#66396 = CARTESIAN_POINT ( 'NONE',  ( 5.165293336682183600, 5.128523102325077687, -0.7216878364870197293 ) ) ;
#66397 = CARTESIAN_POINT ( 'NONE',  ( 1.471644961476214597, -1.907451222982279093, -1.138109381883713578 ) ) ;
#66399 = EDGE_CURVE ( 'NONE', #150774, #111149, #7052, .T. ) ;
#66398 = CARTESIAN_POINT ( 'NONE',  ( 6.725062055625550705, -1.793239977796506457, -0.7961783947641184467 ) ) ;
#66400 = CARTESIAN_POINT ( 'NONE',  ( 8.432808358020025707, 9.900993174853955026, 1.082531754730558626 ) ) ;
#66401 = DIRECTION ( 'NONE',  ( 0.000000000000000000, -0.000000000000000000, 1.000000000000000000 ) ) ;
#66402 = CIRCLE ( 'NONE', #156436, 0.08000000000000020983 ) ;
#66403 = CARTESIAN_POINT ( 'NONE',  ( 6.039231080244466199, 6.010467446565510130, 0.7998128361456352531 ) ) ;
#66404 = CARTESIAN_POINT ( 'NONE',  ( -4.855228407469635243, 4.837057028235559386, 0.7216878364870257245 ) ) ;
#66405 = CARTESIAN_POINT ( 'NONE',  ( 4.193840287544727374, -1.420164769765386303, -1.496150262111215934 ) ) ;
#66406 = CARTESIAN_POINT ( 'NONE',  ( -3.079673448598517549, 6.744702790006905424, 1.040834085586084257E-14 ) ) ;
#66407 = CARTESIAN_POINT ( 'NONE',  ( 0.7499999999999902300, 4.097916667349481123, -1.299038105676658228 ) ) ;
#66408 = CARTESIAN_POINT ( 'NONE',  ( -0.6823417656250246877, 0.3010416670080895418, 1.181850606188755259 ) ) ;
#66409 = CARTESIAN_POINT ( 'NONE',  ( 5.993391575003322203, 1.416176893967495687, 1.222094818194748189 ) ) ;
#66410 = CARTESIAN_POINT ( 'NONE',  ( 4.447759528527571504, -1.551977624003277212, -0.7738437340010505539 ) ) ;
#66411 = CARTESIAN_POINT ( 'NONE',  ( 4.265022598847971302, 1.686782405526715545, -0.4282675217706712889 ) ) ;
#66412 = CARTESIAN_POINT ( 'NONE',  ( 2.998324526916512411, 6.649795714711241423, 0.000000000000000000 ) ) ;
#66413 = CARTESIAN_POINT ( 'NONE',  ( 1.822231264363738834, 1.315867814366477484, -1.876927872033665956 ) ) ;
#66414 = CARTESIAN_POINT ( 'NONE',  ( -1.001543065824772872E-14, 5.634375000341415252, 1.575800808251672791 ) ) ;
#66415 = CARTESIAN_POINT ( 'NONE',  ( 5.583562150179168349, -0.9389753047652232842, 1.868084059271076347 ) ) ;
#66416 = CARTESIAN_POINT ( 'NONE',  ( 1.534833434108737515, -1.332603482217321389, -1.270662175854364362 ) ) ;
#66417 = FACE_OUTER_BOUND ( 'NONE', #141091, .T. ) ;
#66418 = SURFACE_STYLE_FILL_AREA ( #199633 ) ;
#66419 = CARTESIAN_POINT ( 'NONE',  ( 1.899064777474347654, -0.9530127170578571727, -1.777010740487514173 ) ) ;
#66420 = CARTESIAN_POINT ( 'NONE',  ( -0.02321191073820921824, -0.1601477211686137825, -2.156400265872604471 ) ) ;
#66421 = CARTESIAN_POINT ( 'NONE',  ( 10.12759493444457171, 13.73870611316562851, -7.322964122302763279 ) ) ;
#66422 = CARTESIAN_POINT ( 'NONE',  ( -7.497822643557261024, 8.706213491360317747, -1.199719254218446718 ) ) ;
#66423 = CARTESIAN_POINT ( 'NONE',  ( 4.171104814498611368, 8.018039383557042044, 0.7998128361456321445 ) ) ;
#66424 = CARTESIAN_POINT ( 'NONE',  ( -1.360316468750052854, 2.661458333674782573, 0.7853790794158580502 ) ) ;
#66425 = CARTESIAN_POINT ( 'NONE',  ( 3.457788318579996467, -1.606868461378293755, -1.383752881913953292 ) ) ;
#66426 = CARTESIAN_POINT ( 'NONE',  ( -0.6823417656250003738, -0.7822916663252423852, -1.181850606188749264 ) ) ;
#66427 = CARTESIAN_POINT ( 'NONE',  ( 5.584540971669589737, -1.782103179330214449, -0.3958202769075992444 ) ) ;
#66428 = ORIENTED_EDGE ( 'NONE', *, *, #32460, .T. ) ;
#66429 = CARTESIAN_POINT ( 'NONE',  ( -5.281783360975562225, 8.319775133516907673, 1.199719254218452935 ) ) ;
#66430 = CARTESIAN_POINT ( 'NONE',  ( 6.577113915960825175, 8.766661883411348555, -1.443375672974078761 ) ) ;
#66431 = CARTESIAN_POINT ( 'NONE',  ( 3.475000000000000533, -3.660416665710751971, 2.006292185433948827 ) ) ;
#66432 = CARTESIAN_POINT ( 'NONE',  ( -5.693534442735004752, 8.729875052244421951, 1.199719254218452047 ) ) ;
#66433 = CARTESIAN_POINT ( 'NONE',  ( 3.656514325482379757, 2.010451960178538222, 0.1936393378089220907 ) ) ;
#66434 = CARTESIAN_POINT ( 'NONE',  ( 0.3410288278610376089, 0.3603064943271740428, 2.074735154451929020 ) ) ;
#66436 = CARTESIAN_POINT ( 'NONE',  ( -5.824109505522200081, 8.952488968821326054, -1.199719254218452047 ) ) ;
#66435 = PRESENTATION_LAYER_ASSIGNMENT (  '', '', ( #25028 ) ) ;
#66437 = CARTESIAN_POINT ( 'NONE',  ( -2.823841133396259639, 6.516508098929413961, -0.7998128361456481317 ) ) ;
#66438 = CARTESIAN_POINT ( 'NONE',  ( 4.680409711739222267, 1.147293496411544433, -1.465074471950976953 ) ) ;
#66439 = CARTESIAN_POINT ( 'NONE',  ( 9.101601193475611140, 9.512956235343358102, -0.7998128361456221525 ) ) ;
#66440 = CARTESIAN_POINT ( 'NONE',  ( 0.000000000000000000, 4.500000000000003553, 0.000000000000000000 ) ) ;
#66441 = ORIENTED_EDGE ( 'NONE', *, *, #81363, .F. ) ;
#66442 = CARTESIAN_POINT ( 'NONE',  ( -2.740719608256871442, 6.349256642941639051, 0.7998128361456341429 ) ) ;
#66443 = CARTESIAN_POINT ( 'NONE',  ( -7.344766530301162000, 9.591980256816594164, 1.599625672291295375 ) ) ;
#66444 = CARTESIAN_POINT ( 'NONE',  ( 6.684453628662900826, -2.020573120193806638, -0.4047117086388977714 ) ) ;
#66446 = CARTESIAN_POINT ( 'NONE',  ( -4.357679483485834560, 7.387146062586773532, 1.181458644690215998 ) ) ;
#66445 = CARTESIAN_POINT ( 'NONE',  ( -5.586841817283045408, 8.675676665875643678, 1.199719254218454489 ) ) ;
#66447 = CARTESIAN_POINT ( 'NONE',  ( -1.402160292154681736E-14, 0.3218750003414227456, 1.575800808251672791 ) ) ;
#66448 = CARTESIAN_POINT ( 'NONE',  ( 1.246934265006810927, -1.689945720101847293, -0.3868003843893202953 ) ) ;
#66449 = CARTESIAN_POINT ( 'NONE',  ( 0.7611566575390321665, 0.8540426286860869354, 1.516288903859766890 ) ) ;
#66451 = CARTESIAN_POINT ( 'NONE',  ( 8.595506201384020883, 9.130438111143927671, 0.7216878364870438212 ) ) ;
#66450 = CARTESIAN_POINT ( 'NONE',  ( 0.3238087740765641653, -0.1086241252120211664, 2.305164108462977701 ) ) ;
#66452 = CARTESIAN_POINT ( 'NONE',  ( 6.076298462418691315, 7.128931413452940014, -1.143247356662546732 ) ) ;
#66453 = CARTESIAN_POINT ( 'NONE',  ( 3.005207323352117488, 1.739114039596071803, 1.105284290502930089 ) ) ;
#66454 = CARTESIAN_POINT ( 'NONE',  ( 3.981290663907289140, 7.796589541200495965, -0.7998128361456221525 ) ) ;
#66455 = CARTESIAN_POINT ( 'NONE',  ( 1.282577132041575529, -1.967586879516727061, 0.4389604359977539172 ) ) ;
#66456 = DIRECTION ( 'NONE',  ( 0.000000000000000000, 1.000000000000000000, 0.000000000000000000 ) ) ;
#66457 = CARTESIAN_POINT ( 'NONE',  ( -4.111865726694519552, 8.019203457777400956, 0.000000000000000000 ) ) ;
#66458 = CARTESIAN_POINT ( 'NONE',  ( 6.403191318657627029, 1.556466930477506505, 1.037356966126230517 ) ) ;
#66460 = CARTESIAN_POINT ( 'NONE',  ( -6.943184063974175757, 9.193743722760251202, -1.443375672974066548 ) ) ;
#66459 = CARTESIAN_POINT ( 'NONE',  ( 4.957238921819991262, -1.637161358497842389, 0.9882132959125531357 ) ) ;
#66461 = CARTESIAN_POINT ( 'NONE',  ( 6.024089167411393220, -1.222679950896175205, -1.837027303407394507 ) ) ;
#66462 = CARTESIAN_POINT ( 'NONE',  ( -5.546694241322218666, 8.524874810634301525, 1.082531754730550855 ) ) ;
#66463 = CARTESIAN_POINT ( 'NONE',  ( 5.826972158823246595, 10.02016096192762085, -0.7998128361456481317 ) ) ;
#66464 = CARTESIAN_POINT ( 'NONE',  ( -3.485854892044998543, 6.120562236477518070, -1.082531754730546636 ) ) ;
#66465 = CARTESIAN_POINT ( 'NONE',  ( 6.621762855810419346, -0.4656160214656123175, 2.076383538966434017 ) ) ;
#66466 = DIRECTION ( 'NONE',  ( 0.000000000000000000, 0.000000000000000000, 1.000000000000000000 ) ) ;
#66467 = CARTESIAN_POINT ( 'NONE',  ( 3.048224541365350593, 0.8318171267079670361, -2.152611968481593419 ) ) ;
#66468 = CARTESIAN_POINT ( 'NONE',  ( 4.615648854252428102, 0.4318217149890530848, -1.913582009320368371 ) ) ;
#66469 = CARTESIAN_POINT ( 'NONE',  ( 1.674581101246939374, 1.321464807213859505, -1.450045219730737633 ) ) ;
#66470 = CARTESIAN_POINT ( 'NONE',  ( 10.18233705906309972, 11.83814697611718714, 1.199719254218450271 ) ) ;
#66471 = CARTESIAN_POINT ( 'NONE',  ( 1.436838838544731267, 7.449283400311756509, 4.203727439823562229 ) ) ;
#66472 = VERTEX_POINT ( 'NONE', #93628 ) ;
#66473 = CARTESIAN_POINT ( 'NONE',  ( 0.05801502780489272565, 1.224741999009547833, 1.726997829920233540 ) ) ;
#66474 =( BOUNDED_CURVE ( )  B_SPLINE_CURVE ( 2, ( #112844, #210258, #46732, #32587, #178860, #98664, #176710, #212385, #64027 ),
 .UNSPECIFIED., .F., .T. ) 
 B_SPLINE_CURVE_WITH_KNOTS ( ( 3, 2, 2, 2, 3 ),
 ( 0.8125000000000000000, 0.8154761904761904656, 0.8214285714285713969, 0.8273809523809523281, 0.8303571428571429047 ),
 .UNSPECIFIED. ) 
 CURVE ( )  GEOMETRIC_REPRESENTATION_ITEM ( )  RATIONAL_B_SPLINE_CURVE ( ( 0.9330127018922194093, 0.9330127018922194093, 1.000000000000000000, 0.8660254037844387076, 1.000000000000000000, 0.8660254037844387076, 1.000000000000000000, 0.9330127018922180770, 0.9330127018922194093 ) ) 
 REPRESENTATION_ITEM ( '' )  );
#66476 = CARTESIAN_POINT ( 'NONE',  ( -8.779068160048691283, 10.20099992726700933, -1.199719254218446718 ) ) ;
#66475 = CARTESIAN_POINT ( 'NONE',  ( -4.948889764188092677, 5.732458465429559169, 1.199719254218462483 ) ) ;
#66477 = CARTESIAN_POINT ( 'NONE',  ( 0.4273693582952375891, 0.9489586001507933632, -1.577591209259328275 ) ) ;
#66478 = CARTESIAN_POINT ( 'NONE',  ( 4.329095027809041873, -2.023602029403932079, -0.7869089946421561343 ) ) ;
#66479 = CARTESIAN_POINT ( 'NONE',  ( -0.3857294007042892936, 3.105957228677906024, 1.963430320088064063 ) ) ;
#66480 = CARTESIAN_POINT ( 'NONE',  ( 1.353939357992512305, -1.539690173578952770, -1.458446627980537480 ) ) ;
#66481 = CARTESIAN_POINT ( 'NONE',  ( -0.7500000000000215383, 2.472916667349486897, 1.299038105676671107 ) ) ;
#66482 = CARTESIAN_POINT ( 'NONE',  ( 9.562578416340237197, 10.05076299535211781, 0.7998128361456462443 ) ) ;
#66483 = CARTESIAN_POINT ( 'NONE',  ( -1.225000000000056044, 2.541666667349471886, -0.7072540797572937077 ) ) ;
#66484 = CARTESIAN_POINT ( 'NONE',  ( 6.569431593124095414, 6.790062804044275424, 0.3413723397009699734 ) ) ;
#66485 = CARTESIAN_POINT ( 'NONE',  ( 2.600915689618611193, 1.657045147975671817, -1.224973224035642794 ) ) ;
#66487 = CARTESIAN_POINT ( 'NONE',  ( 1.252085211431714251, 3.300000000000025135, 0.7750000000000100142 ) ) ;
#66486 = CARTESIAN_POINT ( 'NONE',  ( -9.840520565420403543, 10.37502883594562597, 1.040834085586084257E-14 ) ) ;
#66488 = CARTESIAN_POINT ( 'NONE',  ( 1.364683531249986537, 2.155208333674751398, -0.7879004041258239610 ) ) ;
#66489 = CARTESIAN_POINT ( 'NONE',  ( -0.02244404828157658613, 7.629137130509074716, -2.789100637983293662 ) ) ;
#66490 = CARTESIAN_POINT ( 'NONE',  ( 5.607153537668954968, 7.478697956109829903, -1.381574923128374044 ) ) ;
#66491 = CARTESIAN_POINT ( 'NONE',  ( 4.529883686416775745, -1.874680353417649492, 0.3764776581506729114 ) ) ;
#66492 = AXIS2_PLACEMENT_3D ( 'NONE', #8195, #122042, #190145 ) ;
#66493 = CARTESIAN_POINT ( 'NONE',  ( 11.78331023100045627, 12.30000000000000071, -1.800000000000001155 ) ) ;
#66494 = CARTESIAN_POINT ( 'NONE',  ( 1.581717252844972998, 2.090516975186909487, -0.8654489506779092789 ) ) ;
#66495 = AXIS2_PLACEMENT_3D ( 'NONE', #108486, #28231, #78042 ) ;
#66496 = CARTESIAN_POINT ( 'NONE',  ( -3.521367211247373508, 5.131347717920458962, -1.599625672291256295 ) ) ;
#66497 = CARTESIAN_POINT ( 'NONE',  ( 1.195247182365884564, 1.673216051897677747, -0.6948750315247439469 ) ) ;
#66498 = CARTESIAN_POINT ( 'NONE',  ( 2.167068266397979670, 1.749796802513942318, -0.7803250849751103280 ) ) ;
#66499 = CARTESIAN_POINT ( 'NONE',  ( 2.998552181135270001, 2.054425100943928051, 0.2560010573490826835 ) ) ;
#66500 = CARTESIAN_POINT ( 'NONE',  ( 0.6823417656249899377, 2.155208333674753174, 1.181850606188767472 ) ) ;
#66501 = CARTESIAN_POINT ( 'NONE',  ( 0.7253841367629434433, -1.872807053274931244, 0.6160819575430801498 ) ) ;
#66502 = CARTESIAN_POINT ( 'NONE',  ( 5.725206259757900540, -0.04501307181254722567, 1.926136320475122288 ) ) ;
#66504 = CARTESIAN_POINT ( 'NONE',  ( 5.599868899865946936, 7.382462344760764239, -1.240035354157904779 ) ) ;
#66503 = CARTESIAN_POINT ( 'NONE',  ( 1.296046498377702472, 1.750325484892759409, 1.504033841696296836 ) ) ;
#66505 = CARTESIAN_POINT ( 'NONE',  ( 1.364683531249986537, 1.655208333674748955, -0.7879004041258239610 ) ) ;
#66506 = CARTESIAN_POINT ( 'NONE',  ( 5.600070422683368854, 0.8392489243487236683, -1.884408887491027196 ) ) ;
#66507 = CARTESIAN_POINT ( 'NONE',  ( -5.005985031943793295, 6.863401842066301661, -1.599625672291256295 ) ) ;
#66508 = CARTESIAN_POINT ( 'NONE',  ( -0.9999999999999988898, 6.468705557303653819, -4.925226524755048629 ) ) ;
#66510 = CARTESIAN_POINT ( 'NONE',  ( -0.7500000000000215383, 3.691666666666690411, 1.299038105676671107 ) ) ;
#66509 = CARTESIAN_POINT ( 'NONE',  ( 5.754936497916005145, -1.662164095216655202, 1.293063917272518015 ) ) ;
#66511 = CARTESIAN_POINT ( 'NONE',  ( 1.364683531249988757, 2.196875000341415252, 1.214306433183764966E-14 ) ) ;
#66512 = CARTESIAN_POINT ( 'NONE',  ( 4.393933622532245842, -0.8317529007547799225, 1.995363109761492337 ) ) ;
#66513 = CARTESIAN_POINT ( 'NONE',  ( 5.479167871109219767, -1.826835719847461847, -0.8615247647300682265 ) ) ;
#66514 = CARTESIAN_POINT ( 'NONE',  ( -0.1399997263889611598, 2.874570648431204578, -2.488748559936367233 ) ) ;
#66515 = CARTESIAN_POINT ( 'NONE',  ( -5.422898255786203769, 6.389431388914436738, -1.082531754730544860 ) ) ;
#66518 = CARTESIAN_POINT ( 'NONE',  ( 6.046573322014824114, 7.117052299514516456, -1.082531754730543083 ) ) ;
#66517 = CARTESIAN_POINT ( 'NONE',  ( -3.285556943750000514, -2.238541666188709200, -1.896917185911906500 ) ) ;
#66516 = CARTESIAN_POINT ( 'NONE',  ( 6.013923656113508542, 9.173938811177871244, -1.199719254218452047 ) ) ;
#66519 = CARTESIAN_POINT ( 'NONE',  ( -5.276058054373441664, 6.184431147304315424, -1.199719254218453823 ) ) ;
#66520 = CARTESIAN_POINT ( 'NONE',  ( 3.239470508323912146, 0.4852670486454255250, -1.957170429962351577 ) ) ;
#66521 = CARTESIAN_POINT ( 'NONE',  ( -9.124801077197171040, 10.60435499727357289, -1.199719254218441611 ) ) ;
#66523 = CARTESIAN_POINT ( 'NONE',  ( -11.00038526257045568, -5.601932402265104471, 0.008494835128522478310 ) ) ;
#66522 = CARTESIAN_POINT ( 'NONE',  ( -9.002250809793991948, 12.48608113052627289, -1.082531754730543971 ) ) ;
#66524 = CARTESIAN_POINT ( 'NONE',  ( -0.6823417656250212460, 5.551041667008087543, 1.181850606188767472 ) ) ;
#66526 = CARTESIAN_POINT ( 'NONE',  ( -11.86145017031081217, 12.59418046486151077, -1.100000000000000533 ) ) ;
#66525 = CARTESIAN_POINT ( 'NONE',  ( 4.715790015261832835, -2.120648752638915724, 0.4184459369844309440 ) ) ;
#66527 = SURFACE_SIDE_STYLE ('',( #65471 ) ) ;
#66528 = CARTESIAN_POINT ( 'NONE',  ( -11.45615580362692221, 6.921991398061194900, -3.423271987478961886 ) ) ;
#66529 = EDGE_CURVE ( 'NONE', #83476, #122390, #66786, .T. ) ;
#66531 = CARTESIAN_POINT ( 'NONE',  ( 5.431267612114304200, -1.591330327768199382, -1.238307421737715019 ) ) ;
#66530 = CARTESIAN_POINT ( 'NONE',  ( -6.846504384776758378, 9.010674420371453053, -1.443375672974058777 ) ) ;
#66532 = CARTESIAN_POINT ( 'NONE',  ( -1.364683531250014514, -0.6989583329919100141, -0.7879004041258359514 ) ) ;
#66533 = CARTESIAN_POINT ( 'NONE',  ( 1.101696929656799995, -1.725068445828933594, -0.003817819714259720019 ) ) ;
#66534 = CARTESIAN_POINT ( 'NONE',  ( 5.435893244436359240, 5.306573304789342416, -0.7998128361456481317 ) ) ;
#66535 = VECTOR ( 'NONE', #500, 1000.000000000000000 ) ;
#66537 = CARTESIAN_POINT ( 'NONE',  ( 5.806634928402749196, 9.996434193103704402, -0.7998128361456481317 ) ) ;
#66536 = CARTESIAN_POINT ( 'NONE',  ( 8.324343129110697959, 9.774450407793066731, -1.082531754730543083 ) ) ;
#66538 = CARTESIAN_POINT ( 'NONE',  ( -11.59482873632621036, 8.292847044363275799, 2.925048987524553556 ) ) ;
#66539 = CARTESIAN_POINT ( 'NONE',  ( 6.327412175546781370, -1.761338861328298089, 0.6302073946208713862 ) ) ;
#66540 = CARTESIAN_POINT ( 'NONE',  ( 1.031890287230966985, -1.963566467742537069, 0.4430998199175004704 ) ) ;
#66541 = CARTESIAN_POINT ( 'NONE',  ( -6.739811759324828344, 8.956476034002674780, -1.443375672974066548 ) ) ;
#66542 = EDGE_LOOP ( 'NONE', ( #129616, #62762, #54359, #139000 ) ) ;
#66544 = CARTESIAN_POINT ( 'NONE',  ( 2.267204043252795120, 1.842440753109304330, -0.8197907266209792931 ) ) ;
#66543 = CARTESIAN_POINT ( 'NONE',  ( 2.086737175084628859, -1.302296122868449535, 1.673399772156684895 ) ) ;
#66545 = CARTESIAN_POINT ( 'NONE',  ( 2.671877653990344381, 1.802496804585513868, -0.1814095246875074008 ) ) ;
#66546 = CARTESIAN_POINT ( 'NONE',  ( 7.364013710877980401, 8.620379413226322285, -1.199719254218452047 ) ) ;
#66547 = CARTESIAN_POINT ( 'NONE',  ( 6.789893189004300389, -0.9291300992274166282, 1.949920244826188309 ) ) ;
#66548 = ORIENTED_EDGE ( 'NONE', *, *, #124471, .F. ) ;
#66549 = CARTESIAN_POINT ( 'NONE',  ( 5.449487677688982679, 8.445153826357429949, -1.199719254218446718 ) ) ;
#66550 = TOROIDAL_SURFACE ( 'NONE', #25147, 11.70000000000000107, 0.2000000000000000111 ) ;
#66552 = CARTESIAN_POINT ( 'NONE',  ( 0.4795166263942132745, -0.6867406401212177158, 1.788596380544268616 ) ) ;
#66551 = CARTESIAN_POINT ( 'NONE',  ( -3.893162665418476109, 7.693773542963529444, 1.040834085586084257E-14 ) ) ;
#66553 = AXIS2_PLACEMENT_3D ( 'NONE', #52151, #2295, #85708 ) ;
#66554 = CARTESIAN_POINT ( 'NONE',  ( -11.94105721237523099, 10.19999999999999929, -1.187919463087249827 ) ) ;
#66555 = EDGE_CURVE ( 'NONE', #203057, #38441, #187870, .T. ) ;
#66556 = CARTESIAN_POINT ( 'NONE',  ( 5.544921637864819175, 7.492161215640853023, -1.443375672974057666 ) ) ;
#66557 = CARTESIAN_POINT ( 'NONE',  ( -1.402160292154681736E-14, 0.3843750003414230232, 1.575800808251672791 ) ) ;
#66558 = CARTESIAN_POINT ( 'NONE',  ( 2.724825686666657809, 6.122787701178987518, 0.000000000000000000 ) ) ;
#66559 = CARTESIAN_POINT ( 'NONE',  ( -8.947491310014823895, 12.52615806407091803, 1.199719254218462483 ) ) ;
#66560 = CARTESIAN_POINT ( 'NONE',  ( 3.907220446582274853, 1.852832235905249370, 1.113321777468062823 ) ) ;
#66561 = CARTESIAN_POINT ( 'NONE',  ( -6.807602527837528505, 7.114826835331461652, 0.7216878364870317197 ) ) ;
#66562 = CARTESIAN_POINT ( 'NONE',  ( 5.560252395380215873, 6.619954228432645138, 1.082531754730549078 ) ) ;
#66563 = CARTESIAN_POINT ( 'NONE',  ( 1.863691559860299884, -1.706161385809309650, -1.259181899442491037 ) ) ;
#66564 = CARTESIAN_POINT ( 'NONE',  ( -1.225000000000042277, 2.479166666666715368, -0.7072540797573197979 ) ) ;
#66565 = CARTESIAN_POINT ( 'NONE',  ( 3.514874812717229347, 1.780701125067783108, 0.8461077801947043397 ) ) ;
#66566 = CARTESIAN_POINT ( 'NONE',  ( 5.906500813101932756, -1.903809282439900219, -0.1807861040028224398 ) ) ;
#66567 = ORIENTED_EDGE ( 'NONE', *, *, #112110, .F. ) ;
#66568 = CARTESIAN_POINT ( 'NONE',  ( 9.605899910213576476, -6.890735599539920209, -0.05097232478520941079 ) ) ;
#66569 = CARTESIAN_POINT ( 'NONE',  ( 5.898876253247024692, 0.3825491175142159417, 1.931855958600266154 ) ) ;
#66570 = CARTESIAN_POINT ( 'NONE',  ( 1.060374178334378303, -1.755330386401842802, -0.8309217204432550741 ) ) ;
#66571 = EDGE_LOOP ( 'NONE', ( #189406, #162792, #38521, #212928 ) ) ;
#66572 = CARTESIAN_POINT ( 'NONE',  ( -5.171509248969888617, 4.998125310078441075, 0.7998128361456281477 ) ) ;
#66574 = CARTESIAN_POINT ( 'NONE',  ( 7.472478939787284169, 8.746922180287201698, 1.199719254218452935 ) ) ;
#66573 = CARTESIAN_POINT ( 'NONE',  ( -6.780486220610186798, 8.043560357867583832, -1.082531754730549967 ) ) ;
#66575 = CARTESIAN_POINT ( 'NONE',  ( 8.145751363712157911, 8.397798100619326078, -0.7998128361456281477 ) ) ;
#66577 = CARTESIAN_POINT ( 'NONE',  ( 6.170369307550831017, 6.371388078330353366, 0.7216878364870328300 ) ) ;
#66576 = CARTESIAN_POINT ( 'NONE',  ( 6.388916700537700777, 8.476822122092563916, 1.599625672291281386 ) ) ;
#66579 = ORIENTED_EDGE ( 'NONE', *, *, #18291, .F. ) ;
#66578 = CARTESIAN_POINT ( 'NONE',  ( 6.270165159132718991, 1.906809857242173445, -0.1455798257045255728 ) ) ;
#66580 = CARTESIAN_POINT ( 'NONE',  ( 4.828867971087246858, 2.111205472107956282, 0.6427781511747706622 ) ) ;
#66581 = CARTESIAN_POINT ( 'NONE',  ( 2.151677955860908487, -1.772288797910109404, -1.314638326115322053 ) ) ;
#66582 = DIRECTION ( 'NONE',  ( 1.000000000000000000, -0.000000000000000000, -0.000000000000000000 ) ) ;
#66583 = CARTESIAN_POINT ( 'NONE',  ( 0.8383554657987003500, 1.138622818284718008, -1.536203910471350298 ) ) ;
#66584 = CARTESIAN_POINT ( 'NONE',  ( 0.3641668253325698879, -9.063144096568546360, -9.630238394150364201 ) ) ;
#66585 = CARTESIAN_POINT ( 'NONE',  ( 8.387690588348714726, 12.93738945304888333, 1.040834085586084257E-14 ) ) ;
#66586 = CARTESIAN_POINT ( 'NONE',  ( 3.684089399883890614, -1.230936008959164996, -1.664559344884769088 ) ) ;
#66587 = CARTESIAN_POINT ( 'NONE',  ( -6.247609857798938293, 6.183299677053865295, -0.7998128361456291469 ) ) ;
#66589 = CARTESIAN_POINT ( 'NONE',  ( 2.237400686453533183, -1.931180590798301955, 0.9714560045831142077 ) ) ;
#66588 = CARTESIAN_POINT ( 'NONE',  ( 1.499999999999990896, 3.775000000000021227, 1.214306433183764966E-14 ) ) ;
#66590 = CARTESIAN_POINT ( 'NONE',  ( 3.702820756938397295, 1.880440254450808757, 1.125299312022425280 ) ) ;
#66591 = CARTESIAN_POINT ( 'NONE',  ( 2.000000000000000000, -2.856854249492364328, 2.449293598294706414E-16 ) ) ;
#66592 = CARTESIAN_POINT ( 'NONE',  ( 2.943528747942701695, 6.448217615992859919, 0.000000000000000000 ) ) ;
#66593 = CARTESIAN_POINT ( 'NONE',  ( -1.626862140677534470E-15, 1.125000000682806034, 1.224999999999975886 ) ) ;
#66594 = CARTESIAN_POINT ( 'NONE',  ( -0.6823417656250003738, 13.96354166700806942, 1.181850606188754593 ) ) ;
#66595 = CARTESIAN_POINT ( 'NONE',  ( -4.950662367645459305, 5.804802846121667415, -1.199719254218453823 ) ) ;
#66596 = CARTESIAN_POINT ( 'NONE',  ( 6.346334349054894908, 0.2861236430486256421, -1.710204530248355059 ) ) ;
#66597 = CARTESIAN_POINT ( 'NONE',  ( -10.49364770729726359, 11.34493653470939023, 0.7216878364870438212 ) ) ;
#66598 = CARTESIAN_POINT ( 'NONE',  ( 3.362232293424003426, -2.068089847843882279, 0.09686330349460009481 ) ) ;
#66599 = CARTESIAN_POINT ( 'NONE',  ( 5.290659027526918301, 1.602671996148979483, -1.383575156158120878 ) ) ;
#66600 = CARTESIAN_POINT ( 'NONE',  ( 5.829115978871627135, 8.888053511070525659, 1.199719254218462483 ) ) ;
#66601 = CARTESIAN_POINT ( 'NONE',  ( 0.6823417656249917140, 5.342708333674749177, 1.181850606188765695 ) ) ;
#66602 = CARTESIAN_POINT ( 'NONE',  ( 2.676555125969529048, 1.290216341703333436, -1.488019019629209572 ) ) ;
#66603 = CARTESIAN_POINT ( 'NONE',  ( 5.437530556340149701, 0.9332327497303912756, -2.093863557220442484 ) ) ;
#66604 = CARTESIAN_POINT ( 'NONE',  ( 2.473051018021198200, 0.08991741065280876855, -1.823594477012622006 ) ) ;
#66605 = CARTESIAN_POINT ( 'NONE',  ( 5.090160327287878594, 4.903218234782778850, -0.7998128361456481317 ) ) ;
#66606 = CARTESIAN_POINT ( 'NONE',  ( 4.161989969270895706, 5.878740935614591656, 1.443375672974062551 ) ) ;
#66607 = CARTESIAN_POINT ( 'NONE',  ( -5.669280788808708671, 9.765911353585494226, 0.7998128361456481317 ) ) ;
#66608 = ORIENTED_EDGE ( 'NONE', *, *, #68459, .F. ) ;
#66609 = CARTESIAN_POINT ( 'NONE',  ( 4.429943789601535009, -1.973532241649661678, 0.3969061482532297291 ) ) ;
#66610 = CARTESIAN_POINT ( 'NONE',  ( 4.662917994108885189, 1.519075486231920458, -1.241376779329693258 ) ) ;
#66611 = CARTESIAN_POINT ( 'NONE',  ( -7.344766530301162000, 9.591980256816594164, 1.599625672291295375 ) ) ;
#66612 = CARTESIAN_POINT ( 'NONE',  ( -3.653032323878261600, 6.349289246911547835, -1.199719254218452047 ) ) ;
#66613 = CARTESIAN_POINT ( 'NONE',  ( 0.07536363704235481131, 0.6997989235110781969, -2.226667633679416447 ) ) ;
#66615 = CARTESIAN_POINT ( 'NONE',  ( 5.752768645092715794, -1.392961553103783112, 1.091694246300749738 ) ) ;
#66614 = CARTESIAN_POINT ( 'NONE',  ( -0.04130929284668418550, -1.869521504948624235, -0.9361258523304989421 ) ) ;
#66616 = CARTESIAN_POINT ( 'NONE',  ( 10.99683038201373719, -5.197079954928569556, -0.2726351642629408212 ) ) ;
#66617 = CARTESIAN_POINT ( 'NONE',  ( 1.886939110189549185, 1.905679594745551819, -1.081921739459410059 ) ) ;
#66618 = CARTESIAN_POINT ( 'NONE',  ( 0.6084659026615606425, -0.2575236531317924293, 1.721126145854386946 ) ) ;
#66619 = CARTESIAN_POINT ( 'NONE',  ( 5.113396490648394632, 9.117379672398465473, 1.040834085586084257E-14 ) ) ;
#66620 = CARTESIAN_POINT ( 'NONE',  ( 0.1335669894368343991, 0.2365985627143319114, -2.188050374159770772 ) ) ;
#66621 = CARTESIAN_POINT ( 'NONE',  ( 0.7324925891301607983, 0.1221277223508714788, 1.720630200619164496 ) ) ;
#66622 = CARTESIAN_POINT ( 'NONE',  ( 0.7908558668072614983, -2.181831595417762504, 0.7228866375666581634 ) ) ;
#66623 = CARTESIAN_POINT ( 'NONE',  ( 0.7322823680011962821, 2.160084099745246178, 0.3691886501416344335 ) ) ;
#66624 = CARTESIAN_POINT ( 'NONE',  ( 6.257189190585941141, -1.725921076436988111, -0.1656679613657590366 ) ) ;
#66625 = CARTESIAN_POINT ( 'NONE',  ( 3.317197348578094562, 1.995112415077514356, 0.9436014139095407760 ) ) ;
#66626 = AXIS2_PLACEMENT_3D ( 'NONE', #167388, #44324, #94153 ) ;
#66627 = CARTESIAN_POINT ( 'NONE',  ( 0.9015274132509668581, -1.862984440646279438, 1.114554472006025865 ) ) ;
#66628 = CARTESIAN_POINT ( 'NONE',  ( -0.005637892868452093476, -0.3948761927005627337, -1.788892068844874395 ) ) ;
#66629 = CARTESIAN_POINT ( 'NONE',  ( 2.589187231636483233, 1.791351791295469731, 1.128514814827277002 ) ) ;
#66630 = VECTOR ( 'NONE', #68411, 1000.000000000000000 ) ;
#66631 = CARTESIAN_POINT ( 'NONE',  ( 6.620655732516668834, 6.034240673559561507, 2.768629221164942145 ) ) ;
#66632 = CARTESIAN_POINT ( 'NONE',  ( 5.772470297455748245, -1.221717764600898981, 1.489408783192472052 ) ) ;
#66633 = ORIENTED_EDGE ( 'NONE', *, *, #142863, .T. ) ;
#66635 = CARTESIAN_POINT ( 'NONE',  ( -0.6823417656250003738, 0.2802083336747515641, -1.181850606188749264 ) ) ;
#66634 = CARTESIAN_POINT ( 'NONE',  ( 2.912002956782848262, -1.132189443809348273, -1.993217883792548495 ) ) ;
#66636 = CARTESIAN_POINT ( 'NONE',  ( 2.659370686574860976, 6.254349567645977714, -0.7998128361456291469 ) ) ;
#66637 = CARTESIAN_POINT ( 'NONE',  ( 5.168682875307768931, 7.053215992657626110, -1.599625672291256295 ) ) ;
#66638 = CARTESIAN_POINT ( 'NONE',  ( 5.285853969472154468, 2.141190784740894415, -0.5908706489107099502 ) ) ;
#66639 = CARTESIAN_POINT ( 'NONE',  ( -7.131225611108100715, 9.342849184424693476, 1.443375672974078761 ) ) ;
#66641 = EDGE_CURVE ( 'NONE', #27240, #135098, #11272, .T. ) ;
#66640 = CARTESIAN_POINT ( 'NONE',  ( -1.608462485350604876, 8.735270501766756013, -2.463594439587629914 ) ) ;
#66642 = CARTESIAN_POINT ( 'NONE',  ( 6.819388077993785657, 7.058300300521964665, 1.040834085586084257E-14 ) ) ;
#66643 = CARTESIAN_POINT ( 'NONE',  ( -6.792271770322117597, 9.907772251142352715, 1.082531754730549967 ) ) ;
#66644 = CARTESIAN_POINT ( 'NONE',  ( 5.722950238744211937, 5.849399164722627553, 0.7216878364870328300 ) ) ;
#66645 = ORIENTED_EDGE ( 'NONE', *, *, #146400, .F. ) ;
#66646 = CARTESIAN_POINT ( 'NONE',  ( 2.654922836763852878, 1.081066371885472277, 1.701947380796410059 ) ) ;
#66648 = CARTESIAN_POINT ( 'NONE',  ( 1.164971494057164492, 1.564520514315300481, -1.344193796132137964 ) ) ;
#66647 = CARTESIAN_POINT ( 'NONE',  ( 5.940443861082012944, 10.08226827123770697, 0.7998128361456462443 ) ) ;
#66649 = CARTESIAN_POINT ( 'NONE',  ( 6.883263157960391787, -0.001104538646235289417, 1.946037152736757925 ) ) ;
#66650 = CARTESIAN_POINT ( 'NONE',  ( 6.672020991256494504, 6.956648375986938859, 0.000000000000000000 ) ) ;
#66651 = FACE_OUTER_BOUND ( 'NONE', #185287, .T. ) ;
#66652 = CARTESIAN_POINT ( 'NONE',  ( -0.6823417656249969321, 3.967708333674754950, -1.181850606188749264 ) ) ;
#66653 = CARTESIAN_POINT ( 'NONE',  ( 3.750093249908572623, 0.7883579158753216687, 2.044908353623323016 ) ) ;
#66654 = CARTESIAN_POINT ( 'NONE',  ( 1.037732671793228700, -1.587836052788630603, 1.242728777923551409 ) ) ;
#66655 = CARTESIAN_POINT ( 'NONE',  ( 0.7140992756325339474, 1.701125707204936166, 0.7050099338341904165 ) ) ;
#66656 = CARTESIAN_POINT ( 'NONE',  ( 4.734224819668921391, 0.3176365174208677367, 1.813369535050498360 ) ) ;
#66657 = ADVANCED_FACE ( 'NONE', ( #94699 ), #96834, .T. ) ;
#66658 = CARTESIAN_POINT ( 'NONE',  ( 7.259501185113382604, 10.55683625168592243, -1.199719254218441611 ) ) ;
#66659 = CARTESIAN_POINT ( 'NONE',  ( 5.825187583072056974, -0.04236064406601056098, 1.825263316621673848 ) ) ;
#66660 = CARTESIAN_POINT ( 'NONE',  ( 6.223279759862190730, 1.994869330463379331, 0.2930738960792296233 ) ) ;
#66661 = CARTESIAN_POINT ( 'NONE',  ( -7.018317073368468328, 11.33978701890523233, -0.7998128361456291469 ) ) ;
#66663 = CARTESIAN_POINT ( 'NONE',  ( -7.293360289508603600, 7.473618190706972086, 0.000000000000000000 ) ) ;
#66662 = CARTESIAN_POINT ( 'NONE',  ( 4.047957556655322087, 0.7652766760943878754, -2.129282649148962925 ) ) ;
#66664 = CARTESIAN_POINT ( 'NONE',  ( 6.581095821095639842, -0.09928302661296910248, -2.103742297734310984 ) ) ;
#66665 = FILL_AREA_STYLE_COLOUR ( '', #91814 ) ;
#66666 = CARTESIAN_POINT ( 'NONE',  ( 4.334477209444560053, -1.194628513295314942, 1.690740121169509447 ) ) ;
#66667 = CARTESIAN_POINT ( 'NONE',  ( 8.432281472695482449, 11.92507992053172572, 1.199719254218450271 ) ) ;
#66668 = APPLICATION_PROTOCOL_DEFINITION ( 'draft international standard', 'automotive_design', 1998, #195850 ) ;
#66670 = CARTESIAN_POINT ( 'NONE',  ( 2.613793455771874719, -1.905494007693061098, 0.2829725131217008527 ) ) ;
#66669 = CARTESIAN_POINT ( 'NONE',  ( -8.178592977541617515, 10.56477777859713463, 1.599625672291295375 ) ) ;
#66671 = UNCERTAINTY_MEASURE_WITH_UNIT (LENGTH_MEASURE( 1.000000000000000082E-05 ), #76426, 'distance_accuracy_value', 'NONE');
#66672 = CARTESIAN_POINT ( 'NONE',  ( 5.342823980928582905, 4.390142039796938178, -2.499999999999995115 ) ) ;
#66673 = CARTESIAN_POINT ( 'NONE',  ( 7.095713291905693332, 9.371694488680407886, 1.599625672291268286 ) ) ;
#66674 = CARTESIAN_POINT ( 'NONE',  ( 5.096651299933133039, 6.508523278119453082, -1.213691435513279293 ) ) ;
#66675 = CARTESIAN_POINT ( 'NONE',  ( -2.428882075142555497, 5.985446187641602300, 1.040834085586084257E-14 ) ) ;
#66677 = CARTESIAN_POINT ( 'NONE',  ( 1.195894564581518660, 2.049875489592466238, -0.8564406981130603391 ) ) ;
#66676 = CARTESIAN_POINT ( 'NONE',  ( 1.072698285844303934, 0.8645715524648779349, 1.936551149067309741 ) ) ;
#66678 = AXIS2_PLACEMENT_3D ( 'NONE', #35116, #120731, #5793 ) ;
#66679 = CARTESIAN_POINT ( 'NONE',  ( 3.874133602078254413, 1.168181435743149921, 1.752046721337781054 ) ) ;
#66680 = CARTESIAN_POINT ( 'NONE',  ( -7.273023059088104425, 7.449891421883056530, 0.000000000000000000 ) ) ;
#66681 = CARTESIAN_POINT ( 'NONE',  ( 7.474622759835693131, 7.614814729430110951, -0.7998128361456281477 ) ) ;
#66682 = CARTESIAN_POINT ( 'NONE',  ( 2.769914238037580745, -1.940913097850523128, 0.2850433363836765155 ) ) ;
#66683 = CARTESIAN_POINT ( 'NONE',  ( 6.647575389402066826, 6.649926130590872120, 1.040834085586084257E-14 ) ) ;
#66684 = CARTESIAN_POINT ( 'NONE',  ( -4.322081814030608982, 7.236479734952984799, 0.9908985150933833363 ) ) ;
#66685 = CARTESIAN_POINT ( 'NONE',  ( 5.671388329218120639, 5.511041227042920099, 1.040834085586084257E-14 ) ) ;
#66686 = CARTESIAN_POINT ( 'NONE',  ( -6.292392690518214593, 7.474117906093608710, -1.082531754730549967 ) ) ;
#66687 = CARTESIAN_POINT ( 'NONE',  ( -6.385527162356466668, 10.39360608948380182, 0.000000000000000000 ) ) ;
#66688 = CARTESIAN_POINT ( 'NONE',  ( 2.021885665735908333, -0.4598567139443253682, 2.069992740399699382 ) ) ;
#66689 = CARTESIAN_POINT ( 'NONE',  ( -4.776215253764153346, 8.794277906025310898, -0.7998128361456362523 ) ) ;
#66690 = CARTESIAN_POINT ( 'NONE',  ( 4.932062528313536198, 1.127988425013145779, 1.604980062286972542 ) ) ;
#66691 = CARTESIAN_POINT ( 'NONE',  ( 3.168983506954273999, -1.996715753333128118, -0.8287754370841573515 ) ) ;
#66692 = CARTESIAN_POINT ( 'NONE',  ( 2.700538275128167687, 1.556679782967337999, 0.9830204120172959525 ) ) ;
#66693 = CARTESIAN_POINT ( 'NONE',  ( -4.014161209245137307, 7.626991082632122776, -0.01188119308113272377 ) ) ;
#66694 = EDGE_CURVE ( 'NONE', #54700, #153986, #56486, .T. ) ;
#66695 = DIRECTION ( 'NONE',  ( 1.214306433183764966E-17, 1.000000000000000000, 5.200010849845536803E-32 ) ) ;
#66696 = CARTESIAN_POINT ( 'NONE',  ( 4.347407756490777153, 1.739891706657967552, -0.04609750694275702165 ) ) ;
#66697 = CARTESIAN_POINT ( 'NONE',  ( 4.039966587192257208, 6.696749537490852333, 1.082531754730558626 ) ) ;
#66698 = CARTESIAN_POINT ( 'NONE',  ( -10.85768919388902809, 5.702095803505641491, 6.451939001899068771 ) ) ;
#66699 = CARTESIAN_POINT ( 'NONE',  ( 1.868271315571629509, 1.111147431007172726, 1.854118885846419262 ) ) ;
#66700 = CARTESIAN_POINT ( 'NONE',  ( 4.147814418418220406, -0.1948115906579734602, -2.006652602119996853 ) ) ;
#66701 = CARTESIAN_POINT ( 'NONE',  ( -8.798878505144648088, 12.24881344176869469, -1.082531754730543083 ) ) ;
#66702 = CARTESIAN_POINT ( 'NONE',  ( 1.710078970767275885, -2.145365142986368934, 0.2646356489638818088 ) ) ;
#66703 = CARTESIAN_POINT ( 'NONE',  ( 2.993000350225515138, 1.691612214138412007, -1.012252976823005968 ) ) ;
#66704 = CARTESIAN_POINT ( 'NONE',  ( 3.110573765929941725, 1.430363465515383625, -1.356829130874689815 ) ) ;
#66705 = EDGE_CURVE ( 'NONE', #10073, #23962, #147281, .T. ) ;
#66706 = CARTESIAN_POINT ( 'NONE',  ( 1.464175926609780964E-14, -2.843749999044085541, -3.475000000000000533 ) ) ;
#66707 = CARTESIAN_POINT ( 'NONE',  ( 3.825673241664818036, 1.036335792742661299, -1.642260645495984495 ) ) ;
#66710 = ORIENTED_EDGE ( 'NONE', *, *, #175830, .T. ) ;
#66709 = CARTESIAN_POINT ( 'NONE',  ( 11.55950211276791251, 13.88000000000000078, -3.221476510067114329 ) ) ;
#66708 = CARTESIAN_POINT ( 'NONE',  ( -8.798878505144648088, 12.24881344176869469, -1.082531754730543083 ) ) ;
#66712 = EDGE_CURVE ( 'NONE', #161735, #73749, #118002, .T. ) ;
#66711 = CARTESIAN_POINT ( 'NONE',  ( -6.474900878978163021, 9.711745571186627402, -1.199719254218452047 ) ) ;
#66713 = CARTESIAN_POINT ( 'NONE',  ( 2.911969131885072670, 6.619324097166378706, 0.000000000000000000 ) ) ;
#66715 = ORIENTED_EDGE ( 'NONE', *, *, #47373, .T. ) ;
#66714 = CARTESIAN_POINT ( 'NONE',  ( -5.010620288702242853, 8.003418215864698482, -1.199719254218453823 ) ) ;
#66716 = CARTESIAN_POINT ( 'NONE',  ( -8.744645890690007306, 12.18554205823825498, 1.082531754730558626 ) ) ;
#66717 = CARTESIAN_POINT ( 'NONE',  ( 0.7630613749609324037, -1.597064910551798667, 1.523150255686569254 ) ) ;
#66718 = CARTESIAN_POINT ( 'NONE',  ( 1.001543065824772753E-15, -3.871874999522043836, 3.793834371823811669 ) ) ;
#66719 = AXIS2_PLACEMENT_3D ( 'NONE', #185844, #166412, #183725 ) ;
#66720 = CARTESIAN_POINT ( 'NONE',  ( 4.926587646396720643, -1.284401507782207963, 1.482881906352449874 ) ) ;
#66721 = CARTESIAN_POINT ( 'NONE',  ( 2.830704105008190030, 0.7231396562890277657, -1.882474209725725434 ) ) ;
#66722 = ORIENTED_EDGE ( 'NONE', *, *, #99349, .F. ) ;
#66723 = CARTESIAN_POINT ( 'NONE',  ( 3.257133915093980203, 0.04755548373316278304, -2.116953498886654295 ) ) ;
#66724 = CARTESIAN_POINT ( 'NONE',  ( 0.7499999999999885647, 2.347916667349486453, -1.299038105676652899 ) ) ;
#66726 = CARTESIAN_POINT ( 'NONE',  ( -4.717347382551060342, 7.590990148696470818, 1.199719254218464037 ) ) ;
#66725 = CARTESIAN_POINT ( 'NONE',  ( 0.07479286986303290696, 5.725009232006174287, -2.449550298930736059 ) ) ;
#66727 = CARTESIAN_POINT ( 'NONE',  ( 4.628748294741646951, -1.682209325509572473, 0.7487199040775436298 ) ) ;
#66728 = ORIENTED_EDGE ( 'NONE', *, *, #146061, .F. ) ;
#66729 = CARTESIAN_POINT ( 'NONE',  ( -9.318531651294266638, 9.766041769465124034, -0.7998128361456291469 ) ) ;
#66730 = CARTESIAN_POINT ( 'NONE',  ( -3.147653791585727667, 8.920000000000001705, -2.499999999999998668 ) ) ;
#66731 = CARTESIAN_POINT ( 'NONE',  ( 5.642871316567687145, 2.044259226470702462, 0.5637153772257290640 ) ) ;
#66732 = CARTESIAN_POINT ( 'NONE',  ( -5.538461698019560231, 5.946930065481515371, -0.9078598751902633435 ) ) ;
#66733 = CARTESIAN_POINT ( 'NONE',  ( 6.124532705071213279, 8.168374127381657246, -1.599625672291262513 ) ) ;
#66734 = AXIS2_PLACEMENT_3D ( 'NONE', #74414, #72245, #125370 ) ;
#66735 = ORIENTED_EDGE ( 'NONE', *, *, #214139, .T. ) ;
#66736 = CARTESIAN_POINT ( 'NONE',  ( 5.817669245088300300, -2.011504375995844196, 0.4472435552253516411 ) ) ;
#66739 = CARTESIAN_POINT ( 'NONE',  ( 3.016969003575611818, -1.773741936391802332, 0.4936923545346691977 ) ) ;
#66738 = CARTESIAN_POINT ( 'NONE',  ( 0.6075646283644918766, 0.5893627863808469369, -1.765331146162614662 ) ) ;
#66737 = CARTESIAN_POINT ( 'NONE',  ( 5.899206235721897507, 6.055031161196562373, 0.000000000000000000 ) ) ;
#66740 = CARTESIAN_POINT ( 'NONE',  ( 8.555358625423188812, 9.940005470203933768, 1.199719254218462483 ) ) ;
#66741 = CARTESIAN_POINT ( 'NONE',  ( -11.16489891154634861, 3.742896273583264932, 3.684481756086905424 ) ) ;
#66742 = CARTESIAN_POINT ( 'NONE',  ( -4.833902094211216749, 5.059593709313742416, -0.9115025817279830411 ) ) ;
#66743 = CARTESIAN_POINT ( 'NONE',  ( -1.040834085586084257E-14, -7.473374494045017968, -9.579665964948867796 ) ) ;
#66744 = CARTESIAN_POINT ( 'NONE',  ( 1.893488989520499377, 1.919108310403025985, -1.089527612406354873 ) ) ;
#66745 = CARTESIAN_POINT ( 'NONE',  ( 5.132209903004834928, 1.169260703421838743, -1.936728657785217411 ) ) ;
#66746 = CARTESIAN_POINT ( 'NONE',  ( 3.608611488583326032, 1.916353073142588403, 0.6279913346786819561 ) ) ;
#66747 = CARTESIAN_POINT ( 'NONE',  ( -6.805829924380121909, 8.963220883242035697, 1.443375672974078761 ) ) ;
#66748 = CARTESIAN_POINT ( 'NONE',  ( 4.271601952734533469, 0.3905692737867596520, -1.768816315278500584 ) ) ;
#66749 = CARTESIAN_POINT ( 'NONE',  ( 5.278507882932355955, -0.4720989235634742154, -1.856488224439522439 ) ) ;
#66750 = CARTESIAN_POINT ( 'NONE',  ( -1.201851678989727383E-14, 3.118750000682814161, -1.732050807568863648 ) ) ;
#66751 = CARTESIAN_POINT ( 'NONE',  ( 4.856247981345184428, 0.7163626499266174674, 1.728251504774950709 ) ) ;
#66752 = CARTESIAN_POINT ( 'NONE',  ( 4.650750022344506185, -0.4068995778509130190, -1.815856201304208550 ) ) ;
#66753 = CARTESIAN_POINT ( 'NONE',  ( -1.364683531250010295, 5.530208333674751842, 0.7879004041258379498 ) ) ;
#66754 = CARTESIAN_POINT ( 'NONE',  ( 6.526229032160782317, 1.014938005144504274, -1.449696215517197961 ) ) ;
#66755 = CARTESIAN_POINT ( 'NONE',  ( -0.1003747550864658999, -1.976661868047492998, 0.3981153667176607902 ) ) ;
#66757 = CARTESIAN_POINT ( 'NONE',  ( 2.350341522438728514, 2.105628791459000393, 0.05071553880554508648 ) ) ;
#66756 = CARTESIAN_POINT ( 'NONE',  ( -3.104453987404963478, 5.605318171072321221, -1.082531754730549078 ) ) ;
#66758 = CARTESIAN_POINT ( 'NONE',  ( 8.723781775389312543, 12.26516360700784958, -1.199719254218446718 ) ) ;
#66760 = CARTESIAN_POINT ( 'NONE',  ( -8.805130697071332335, 12.36007068230351358, 1.199719254218462483 ) ) ;
#66759 = CARTESIAN_POINT ( 'NONE',  ( 1.436838838544733044, 7.449283400311756509, -4.203727439823553347 ) ) ;
#66761 = CARTESIAN_POINT ( 'NONE',  ( 4.370663978927065152, 5.060324124126027279, 2.420000000000000373 ) ) ;
#66762 = CARTESIAN_POINT ( 'NONE',  ( 1.951431513787309724, -1.802353211750299167, 0.9118321038049399530 ) ) ;
#66763 = CARTESIAN_POINT ( 'NONE',  ( 1.364683531249988757, 2.384375000341422357, 1.214306433183764966E-14 ) ) ;
#66764 = CARTESIAN_POINT ( 'NONE',  ( 6.720655732516647163, 0.002698097948191854455, 1.926293798961113080 ) ) ;
#66765 = CARTESIAN_POINT ( 'NONE',  ( 5.183294799126148433, 4.941598775268944976, 1.040834085586084257E-14 ) ) ;
#66766 = ORIENTED_EDGE ( 'NONE', *, *, #96671, .F. ) ;
#66767 = CARTESIAN_POINT ( 'NONE',  ( 2.706508253401081809, -0.8245430293080566742, -1.998349536214229616 ) ) ;
#66768 = CARTESIAN_POINT ( 'NONE',  ( 6.610000000000021636, 3.695490760540712127, 2.514297579034238783 ) ) ;
#66771 = CARTESIAN_POINT ( 'NONE',  ( 10.91970695577495043, -6.134628647623513231, 5.204170427930421283E-15 ) ) ;
#66770 = CARTESIAN_POINT ( 'NONE',  ( -3.642287698956971020, 3.120124397464318022, -2.499999999999528821 ) ) ;
#66769 = CARTESIAN_POINT ( 'NONE',  ( 3.736153849017632922, 6.516540702899320081, -1.199719254218453823 ) ) ;
#66772 = CARTESIAN_POINT ( 'NONE',  ( 9.869972640624258275, 10.61731562359089587, 0.000000000000000000 ) ) ;
#66773 = CARTESIAN_POINT ( 'NONE',  ( 6.509000000000012776, 0.004788705324892602276, 2.000274819378269342 ) ) ;
#66774 = CARTESIAN_POINT ( 'NONE',  ( -7.876924059859742755, 8.292092279365579799, 1.040834085586084257E-14 ) ) ;
#66775 = CARTESIAN_POINT ( 'NONE',  ( 1.523247060345904291, -2.062048068855956373, 0.7425582295156886170 ) ) ;
#66776 = CARTESIAN_POINT ( 'NONE',  ( -4.313792511808268060, 5.583989749030219052, 1.358440613521926910 ) ) ;
#66777 = CARTESIAN_POINT ( 'NONE',  ( 1.007111469781604596, 1.711705730394815106, -1.479659443445595413 ) ) ;
#66778 = CARTESIAN_POINT ( 'NONE',  ( -7.049349804101573191, 10.31165964050546258, -1.199719254218440723 ) ) ;
#66779 = EDGE_CURVE ( 'NONE', #174327, #88062, #73895, .T. ) ;
#66780 = CARTESIAN_POINT ( 'NONE',  ( -4.731432421044877934, 6.543090462684225450, -1.443375672974051449 ) ) ;
#66781 = CARTESIAN_POINT ( 'NONE',  ( -1.364683531249997417, 3.321875000341423245, 1.214306433183764966E-14 ) ) ;
#66782 = CARTESIAN_POINT ( 'NONE',  ( 4.625518323863472503, 8.335144253906971556, 0.3473850511846506839 ) ) ;
#66783 = CARTESIAN_POINT ( 'NONE',  ( 1.500000000000001332, 10.87499999999999645, 0.000000000000000000 ) ) ;
#66784 = CARTESIAN_POINT ( 'NONE',  ( 5.388439706788500594, 5.251210844200210559, 0.7998128361456352531 ) ) ;
#66785 = CARTESIAN_POINT ( 'NONE',  ( 2.793947764029936831, -1.764715128225034180, -0.1343432132955291736 ) ) ;
#66786 = CIRCLE ( 'NONE', #149877, 2.080000000000000071 ) ;
#66787 = CARTESIAN_POINT ( 'NONE',  ( 0.1652458694026041341, -1.881425287724652673, -0.9463707761560661291 ) ) ;
#66788 = CIRCLE ( 'NONE', #94543, 10.25000000000000000 ) ;
#66789 = CARTESIAN_POINT ( 'NONE',  ( -0.6823417656250003738, 8.401041667008064096, 1.181850606188754593 ) ) ;
#66790 = ORIENTED_EDGE ( 'NONE', *, *, #137134, .F. ) ;
#66791 = CARTESIAN_POINT ( 'NONE',  ( -5.315678745009726924, 8.359319748223434487, -1.199719254218453823 ) ) ;
#66792 = CARTESIAN_POINT ( 'NONE',  ( 5.009388752257521560, -1.913799287717246500, 0.6352160319311253023 ) ) ;
#66793 = VERTEX_POINT ( 'NONE', #1403 ) ;
#66794 = CARTESIAN_POINT ( 'NONE',  ( 2.869827659178546764, 0.9992216309704025079, 1.581230272166146644 ) ) ;
#66795 = CARTESIAN_POINT ( 'NONE',  ( 2.360293207207576849, -2.069885933316969240, 0.04650197241463926989 ) ) ;
#66796 = CARTESIAN_POINT ( 'NONE',  ( -6.251718229232846369, 9.347402796530044355, -1.082531754730549967 ) ) ;
#66797 = CARTESIAN_POINT ( 'NONE',  ( 2.478646075381494285, -1.315928518397539548, 1.387899491812602859 ) ) ;
#66798 = CARTESIAN_POINT ( 'NONE',  ( -5.155907263950760822, 7.611285832944477470, 1.217474411562294190 ) ) ;
#66799 = CARTESIAN_POINT ( 'NONE',  ( -1.559074708514275542, 8.689926414953912825, 2.502785155726149569 ) ) ;
#66800 = CARTESIAN_POINT ( 'NONE',  ( 11.33772463945036790, 12.69999999999999929, -3.680000000000001048 ) ) ;
#66801 = CARTESIAN_POINT ( 'NONE',  ( 1.364683531249988535, 3.967708333674751842, -0.7879004041258239610 ) ) ;
#66802 = CARTESIAN_POINT ( 'NONE',  ( 1.617294888471169312, 1.591762500684265946, 1.059657513450793953 ) ) ;
#66803 = CARTESIAN_POINT ( 'NONE',  ( 5.668717624289557833, 8.667235424096215723, -1.082531754730548412 ) ) ;
#66804 = CARTESIAN_POINT ( 'NONE',  ( 2.506241959165692812, 1.961374882610424919, 0.05109738790698423877 ) ) ;
#66805 = CARTESIAN_POINT ( 'NONE',  ( -5.427887300360803913, 4.356806483369918048, -2.440341253675376798 ) ) ;
#66806 = CARTESIAN_POINT ( 'NONE',  ( -5.309953438407606363, 6.223975762010839574, 1.199719254218452935 ) ) ;
#66807 = CARTESIAN_POINT ( 'NONE',  ( 5.836213162209912930, -1.179542664122106510, -1.762073437084572314 ) ) ;
#66809 = DIRECTION ( 'NONE',  ( 1.224646799147353207E-16, 1.000000000000000000, -0.000000000000000000 ) ) ;
#66808 = CARTESIAN_POINT ( 'NONE',  ( 8.561083932025322696, 12.07534945641652158, -1.199719254218446718 ) ) ;
#66810 = CARTESIAN_POINT ( 'NONE',  ( 0.3681424317822541425, -1.226883886190757611, 1.412057460252094554 ) ) ;
#66811 = CARTESIAN_POINT ( 'NONE',  ( 1.364683531249988757, 1.884375000341421913, 0.000000000000000000 ) ) ;
#66812 = CARTESIAN_POINT ( 'NONE',  ( 1.828386956846822509, -0.9528715280972717139, -1.773455306963005462 ) ) ;
#66814 = CARTESIAN_POINT ( 'NONE',  ( 0.5974486649760869517, -0.3061723685214760016, 2.094854868064464970 ) ) ;
#66813 = CARTESIAN_POINT ( 'NONE',  ( -8.215877900201387973, 8.687538426430837291, 0.7216878364870578100 ) ) ;
#66815 = CARTESIAN_POINT ( 'NONE',  ( 10.35782045828010745, 9.182042646633135519, 6.014258400289742568 ) ) ;
#66816 = CARTESIAN_POINT ( 'NONE',  ( 2.207561477879273593, -1.661462528888792090, -1.235070534849058266 ) ) ;
#66817 = CARTESIAN_POINT ( 'NONE',  ( 4.095444919779759552, 6.935713618788495793, 1.199719254218451159 ) ) ;
#66818 = CARTESIAN_POINT ( 'NONE',  ( 4.923546060418115822, 5.773167154356443120, -1.199719254218452047 ) ) ;
#66819 = ORIENTED_EDGE ( 'NONE', *, *, #187111, .F. ) ;
#66821 = CARTESIAN_POINT ( 'NONE',  ( 4.878236342818665250, 4.585697242910212523, 1.040834085586084257E-14 ) ) ;
#66820 = CARTESIAN_POINT ( 'NONE',  ( 6.263634082940216175, 1.073540726731788908, 1.793809194602818735 ) ) ;
#66824 = ORIENTED_EDGE ( 'NONE', *, *, #119166, .F. ) ;
#66823 = CARTESIAN_POINT ( 'NONE',  ( 2.666445455534327102, 0.6121260541337695260, 1.705033028387469285 ) ) ;
#66822 = CARTESIAN_POINT ( 'NONE',  ( 3.944226942909400346, 1.816763600636053688, 0.1792749827478901103 ) ) ;
#66825 = CARTESIAN_POINT ( 'NONE',  ( 9.890836756369282057, 11.49806328964105617, -1.199719254218440723 ) ) ;
#66826 = DIRECTION ( 'NONE',  ( 0.000000000000000000, 0.000000000000000000, -1.000000000000000000 ) ) ;
#66827 = CARTESIAN_POINT ( 'NONE',  ( 11.15461176689735012, 7.620380504396416121, -0.7938402394984110932 ) ) ;
#66828 = CARTESIAN_POINT ( 'NONE',  ( 4.876106637443972325, 1.267215935518750669, 1.806476597341267087 ) ) ;
#66829 = CARTESIAN_POINT ( 'NONE',  ( -8.012344526598182026E-15, 10.85937500034139624, -1.575800808251669460 ) ) ;
#66830 = VERTEX_POINT ( 'NONE', #67464 ) ;
#66831 = CARTESIAN_POINT ( 'NONE',  ( 3.756429630051653312, 1.903336793139896788, 0.1845653119916731144 ) ) ;
#66832 = CARTESIAN_POINT ( 'NONE',  ( -2.785310492603665367, 5.336947110424484109, 1.199719254218462483 ) ) ;
#66833 = CARTESIAN_POINT ( 'NONE',  ( 5.947222937888848371, 10.09017719417900416, 1.040834085586084257E-14 ) ) ;
#66834 = CARTESIAN_POINT ( 'NONE',  ( -1.360316468750036645, 1.901041667008058988, -0.7853790794159222211 ) ) ;
#66835 = CARTESIAN_POINT ( 'NONE',  ( 4.487385655998878953, 6.258369236797239665, 1.443375672974062551 ) ) ;
#66836 = CARTESIAN_POINT ( 'NONE',  ( 10.99967557777141103, -6.699439830718304734, -0.09581361862938142515 ) ) ;
#66837 = CARTESIAN_POINT ( 'NONE',  ( 7.585545081070966589, 14.47801472900905395, -9.241967501645218519 ) ) ;
#66838 = CARTESIAN_POINT ( 'NONE',  ( 0.9074547957551477584, -0.8278116715597811925, -1.644758345054016191 ) ) ;
#66839 = CARTESIAN_POINT ( 'NONE',  ( 0.000000000000000000, -3.499999999999999556, 0.000000000000000000 ) ) ;
#66840 = EDGE_CURVE ( 'NONE', #105543, #144349, #177537, .T. ) ;
#66841 = CARTESIAN_POINT ( 'NONE',  ( 4.868341698904518289, -1.223052743625025141, 1.415352931214426846 ) ) ;
#66842 = CARTESIAN_POINT ( 'NONE',  ( 5.996449078994045223, 10.21788403546024782, 0.7998128361456331437 ) ) ;
#66843 = FACE_OUTER_BOUND ( 'NONE', #207187, .T. ) ;
#66844 = CIRCLE ( 'NONE', #94604, 0.08000000000000025147 ) ;
#66845 = CARTESIAN_POINT ( 'NONE',  ( -6.724481002698126098, 8.868313807946373473, -1.443375672974059665 ) ) ;
#66846 = CARTESIAN_POINT ( 'NONE',  ( 5.847644326195776010, 5.716673223516856694, -0.7998128361456281477 ) ) ;
#66847 = CARTESIAN_POINT ( 'NONE',  ( 1.762491902426995605, -0.7040454445105134296, -1.839503732180563844 ) ) ;
#66848 = CARTESIAN_POINT ( 'NONE',  ( 1.810172953844836341, 1.158670025852935437, -1.650096248209935945 ) ) ;
#66849 = CARTESIAN_POINT ( 'NONE',  ( -8.076906825439122528, 10.44614393447756129, -1.599625672291263179 ) ) ;
#66850 = CARTESIAN_POINT ( 'NONE',  ( 4.694866332082116678, 8.699370830729650450, 0.7998128361456341429 ) ) ;
#66851 = CARTESIAN_POINT ( 'NONE',  ( -0.4809368265653978236, 3.139971263792654899, 0.3999999999999597211 ) ) ;
#66852 = CARTESIAN_POINT ( 'NONE',  ( 2.537292984272555785, -1.624655320356691801, -1.470880813658273389 ) ) ;
#66853 = CARTESIAN_POINT ( 'NONE',  ( 6.129513044595951143, -1.717388127611047421, 0.6198453807191862674 ) ) ;
#66854 = CARTESIAN_POINT ( 'NONE',  ( -4.796887421136680985, 4.490790167614548523, 1.214306433183764966E-14 ) ) ;
#66855 = CARTESIAN_POINT ( 'NONE',  ( 6.825078400183544503, 2.075476428726834577, 2.163873318353096931 ) ) ;
#66856 = CARTESIAN_POINT ( 'NONE',  ( -15.75000000000000000, 13.39999999999998259, 3.599999999999999201 ) ) ;
#66857 = CARTESIAN_POINT ( 'NONE',  ( 5.424670859243587273, 5.501406555305196733, -0.7216878364870458196 ) ) ;
#66858 = CARTESIAN_POINT ( 'NONE',  ( 7.747594715205354809, 11.12627870345989756, -1.199719254218446718 ) ) ;
#66859 = VECTOR ( 'NONE', #171721, 1000.000000000000000 ) ;
#66860 = CARTESIAN_POINT ( 'NONE',  ( 3.408985558832261731, 6.064568021024562938, 1.199719254218462483 ) ) ;
#66861 = CARTESIAN_POINT ( 'NONE',  ( 6.211043768836170820, 9.299949259400630552, 1.082531754730549967 ) ) ;
#66862 = ORIENTED_EDGE ( 'NONE', *, *, #180960, .T. ) ;
#66864 = CARTESIAN_POINT ( 'NONE',  ( 1.207682405589046937, 1.525905122249699319, 1.313188400431253955 ) ) ;
#66863 = CARTESIAN_POINT ( 'NONE',  ( 3.649809678215182096, 0.6660801477775115664, 1.716721118343276453 ) ) ;
#66865 = CARTESIAN_POINT ( 'NONE',  ( 3.251609920728415037, -2.263897172838242877, -0.3959942320375854918 ) ) ;
#66867 = CARTESIAN_POINT ( 'NONE',  ( 0.7427237327431088776, -0.2200284318808701234, -1.847805914472876232 ) ) ;
#66866 = CARTESIAN_POINT ( 'NONE',  ( -0.4019237886466802689, 9.948664549684631098, -1.500000000000002887 ) ) ;
#66868 = CARTESIAN_POINT ( 'NONE',  ( 1.737499999999999378, -0.1166666666666676955, -3.009438278150925683 ) ) ;
#66869 = CARTESIAN_POINT ( 'NONE',  ( -4.115063316947640715, 4.759660943649018705, 1.199719254218462483 ) ) ;
#66870 = CARTESIAN_POINT ( 'NONE',  ( 7.334597915313080918, 9.580116872663850813, 1.040834085586084257E-14 ) ) ;
#66871 = CARTESIAN_POINT ( 'NONE',  ( 4.799029005866479736, -0.2398712174674077491, -1.897248949554980024 ) ) ;
#66872 = CARTESIAN_POINT ( 'NONE',  ( -8.507905087775398556, 9.884643009614800135, 1.199719254218462483 ) ) ;
#66873 = CARTESIAN_POINT ( 'NONE',  ( -6.970300371201519241, 7.304640985922785212, 0.7216878364870317197 ) ) ;
#66875 = CARTESIAN_POINT ( 'NONE',  ( 2.465516990510143280, 1.834972510290140191, -0.3627323784974947340 ) ) ;
#66874 = CARTESIAN_POINT ( 'NONE',  ( 3.650014318109519262, 0.7545864325827613683, 1.950000943494380135 ) ) ;
#66876 = CARTESIAN_POINT ( 'NONE',  ( 7.619319141200063150, 9.912291636198670375, 1.443375672974076540 ) ) ;
#66877 = CARTESIAN_POINT ( 'NONE',  ( 3.147653791585699690, 8.920000000000010587, 2.500000000000000444 ) ) ;
#66878 = EDGE_CURVE ( 'NONE', #21442, #202900, #12048, .T. ) ;
#66879 = CARTESIAN_POINT ( 'NONE',  ( 5.583513413114173041, -0.8223277247318347971, 1.647484189299788682 ) ) ;
#66880 = CARTESIAN_POINT ( 'NONE',  ( 4.532503425670185493, 4.182342172903648070, 1.214306433183764966E-14 ) ) ;
#66881 = CARTESIAN_POINT ( 'NONE',  ( 5.998049851660174348, 5.987234766784138351, -0.01316317710055334329 ) ) ;
#66882 = CARTESIAN_POINT ( 'NONE',  ( 5.039546052477672511, -1.223360384887246743, -1.216254805912063919 ) ) ;
#66883 = CARTESIAN_POINT ( 'NONE',  ( -7.901704598666176693, 8.113076874732334076, 0.7998128361456602331 ) ) ;
#66884 =( BOUNDED_CURVE ( )  B_SPLINE_CURVE ( 2, ( #52925, #205565, #23617, #204484, #22539, #36665, #189329, #187188, #40970 ),
 .UNSPECIFIED., .F., .T. ) 
 B_SPLINE_CURVE_WITH_KNOTS ( ( 3, 2, 2, 2, 3 ),
 ( 0.4375000000000000000, 0.4404761904761904656, 0.4464285714285714524, 0.4523809523809523836, 0.4553571428571427937 ),
 .UNSPECIFIED. ) 
 CURVE ( )  GEOMETRIC_REPRESENTATION_ITEM ( )  RATIONAL_B_SPLINE_CURVE ( ( 0.9330127018922194093, 0.9330127018922194093, 1.000000000000000000, 0.8660254037844387076, 1.000000000000000000, 0.8660254037844387076, 1.000000000000000000, 0.9330127018922206306, 0.9330127018922194093 ) ) 
 REPRESENTATION_ITEM ( '' )  );
#66885 = CARTESIAN_POINT ( 'NONE',  ( 0.2461560209003906818, 1.715711078377361032, -0.2512605247984560086 ) ) ;
#66886 = CARTESIAN_POINT ( 'NONE',  ( 6.305322857734435793, 1.832379230283949667, 1.229636283518860118 ) ) ;
#66887 =( NAMED_UNIT ( * ) SI_UNIT ( $, .STERADIAN. ) SOLID_ANGLE_UNIT ( ) );
#66888 = CARTESIAN_POINT ( 'NONE',  ( -0.3282377607281410370, 0.7611645503674365765, -1.225000000000029399 ) ) ;
#66890 = CARTESIAN_POINT ( 'NONE',  ( 5.120078768083678789, 2.148437930330206136, -0.3118015998682179823 ) ) ;
#66889 = B_SPLINE_CURVE_WITH_KNOTS ( 'NONE', 3,
 ( #70056, #149199, #53843, #167586, #67912, #18109 ),
 .UNSPECIFIED., .F., .F.,
 ( 4, 2, 4 ),
 ( 0.000000000000000000, 0.0003778774010236167534, 0.0007557548020472335069 ),
 .UNSPECIFIED. ) ;
#66891 = CARTESIAN_POINT ( 'NONE',  ( 2.930095790256614485, 1.013914413367119627, -1.518051517300327502 ) ) ;
#66892 = CARTESIAN_POINT ( 'NONE',  ( 1.657006586592904673, 1.606862555911577006, -1.125131163738995577 ) ) ;
#66893 = CARTESIAN_POINT ( 'NONE',  ( 5.260995011843273339, -0.05493784808423751720, -2.116803055475650730 ) ) ;
#66894 = EDGE_CURVE ( 'NONE', #95692, #60619, #11826, .T. ) ;
#66895 = EDGE_LOOP ( 'NONE', ( #196862, #137191, #160667, #78121 ) ) ;
#66897 = CARTESIAN_POINT ( 'NONE',  ( -1.201851678989727383E-14, 3.509375000341421469, -1.575800808251660134 ) ) ;
#66896 = CARTESIAN_POINT ( 'NONE',  ( 6.251568577072929678, 2.286574220100371591, -0.1642174239346057829 ) ) ;
#66898 = CARTESIAN_POINT ( 'NONE',  ( 10.05067194643221207, 10.62020544712608938, 0.7998128361456462443 ) ) ;
#66899 = CARTESIAN_POINT ( 'NONE',  ( 1.647299267346370444, 0.2110521635003380359, 2.109970702148834754 ) ) ;
#66900 = CARTESIAN_POINT ( 'NONE',  ( -6.100805936469506641, 6.219954468743612352, 0.7216878364870317197 ) ) ;
#66901 = CARTESIAN_POINT ( 'NONE',  ( 4.380693030546913391, 7.164540064729805202, 1.082531754730549078 ) ) ;
#66902 = CARTESIAN_POINT ( 'NONE',  ( -4.243338890952904841, 5.973648010910253880, -1.443375672974051449 ) ) ;
#66903 = CARTESIAN_POINT ( 'NONE',  ( 6.139545750997863927, 2.009069680886385267, -0.8233997750264672177 ) ) ;
#66905 = CARTESIAN_POINT ( 'NONE',  ( 1.499999999999993117, 12.38541666734946212, 0.8660254037844409281 ) ) ;
#66904 = CARTESIAN_POINT ( 'NONE',  ( 6.983263157960387879, 4.689051080487334211, 2.716346346018564617 ) ) ;
#66907 = ORIENTED_EDGE ( 'NONE', *, *, #36152, .F. ) ;
#66906 = CARTESIAN_POINT ( 'NONE',  ( 2.754761814426693434, 2.204812966250285999, 0.2695357242936818332 ) ) ;
#66908 = CARTESIAN_POINT ( 'NONE',  ( 0.03630054827139220924, -1.841026678340401679, 1.376304820193236189 ) ) ;
#66910 = CARTESIAN_POINT ( 'NONE',  ( 4.750865691763131338, -0.4467450692671371959, -2.013472809446889666 ) ) ;
#66909 = CARTESIAN_POINT ( 'NONE',  ( 5.183294799126148433, 4.941598775268944976, 1.040834085586084257E-14 ) ) ;
#66912 = CARTESIAN_POINT ( 'NONE',  ( 1.737499999999999378, -3.266666666666667496, -3.009438278150925683 ) ) ;
#66911 = CARTESIAN_POINT ( 'NONE',  ( 7.517069824134078537, 7.734612647770044092, 0.000000000000000000 ) ) ;
#66913 = CARTESIAN_POINT ( 'NONE',  ( 6.384963997392946844, 6.413822516572072807, 0.7998128361456352531 ) ) ;
#66914 = CARTESIAN_POINT ( 'NONE',  ( -3.285556943749998737, -2.967708332855377051, 1.896917185911908499 ) ) ;
#66915 = CARTESIAN_POINT ( 'NONE',  ( 0.1329588055935396196, 2.886534925058126699, -2.334852352984605695 ) ) ;
#66916 = CARTESIAN_POINT ( 'NONE',  ( 0.7442207691023922100, 0.6088243375477386810, 2.000016368695969327 ) ) ;
#66917 = CARTESIAN_POINT ( 'NONE',  ( 4.606092368833686557, -0.09613688574180989654, 2.014232646917232916 ) ) ;
#66918 = CARTESIAN_POINT ( 'NONE',  ( 4.001369526190221571, -1.836035423186295201, 0.1395379388276704880 ) ) ;
#66919 = EDGE_CURVE ( 'NONE', #114519, #8253, #29622, .T. ) ;
#66920 = CARTESIAN_POINT ( 'NONE',  ( 4.385172619016207918, 7.203452924572514959, 1.199719254218462483 ) ) ;
#66921 = FILL_AREA_STYLE ('',( #186026 ) ) ;
#66922 = CARTESIAN_POINT ( 'NONE',  ( 2.203723468020501119, -1.724507683567375826, 0.03868650182545228799 ) ) ;
#66923 = CARTESIAN_POINT ( 'NONE',  ( -0.1179535434602772825, -2.016182236903838465, -0.04464881524945257807 ) ) ;
#66924 = CARTESIAN_POINT ( 'NONE',  ( 1.688534781859708067, 1.914194972067848832, 1.272504748915660899 ) ) ;
#66925 = CARTESIAN_POINT ( 'NONE',  ( -5.656776405399756236, 7.622658444431597680, -1.599625672291256295 ) ) ;
#66926 = CARTESIAN_POINT ( 'NONE',  ( 1.107111304455286049, 1.712943910497457756, -1.478075018494163118 ) ) ;
#66927 = CARTESIAN_POINT ( 'NONE',  ( 3.756553094297815143, 0.7580258897690328457, 1.965105124105433809 ) ) ;
#66928 = CARTESIAN_POINT ( 'NONE',  ( -4.767627293860968507, 5.591261926706423857, -1.199719254218453823 ) ) ;
#66929 = CARTESIAN_POINT ( 'NONE',  ( 5.601490020740366838, 9.686822124172440596, 1.040834085586084257E-14 ) ) ;
#66930 = CARTESIAN_POINT ( 'NONE',  ( 5.356880090730863131, 7.343055753976412525, 1.443375672974064550 ) ) ;
#66931 = CARTESIAN_POINT ( 'NONE',  ( 0.000000000000000000, 7.629137130509076492, -2.599999999999999201 ) ) ;
#66932 = CARTESIAN_POINT ( 'NONE',  ( -5.900823170445743671, 7.907379670318584353, 1.599625672291269396 ) ) ;
#66933 = UNCERTAINTY_MEASURE_WITH_UNIT (LENGTH_MEASURE( 1.000000000000000082E-05 ), #170220, 'distance_accuracy_value', 'NONE');
#66934 = CARTESIAN_POINT ( 'NONE',  ( -1.500000000000013101, 2.629166666666687746, -0.8660254037844313801 ) ) ;
#66935 = CARTESIAN_POINT ( 'NONE',  ( -3.436101866059630527, 6.096203712789787232, 1.199719254218462483 ) ) ;
#66936 = CARTESIAN_POINT ( 'NONE',  ( 5.203485844055394161, 1.958870149131001881, -1.047680120605886556 ) ) ;
#66937 = CARTESIAN_POINT ( 'NONE',  ( 3.925867417771063739, 1.172880473742785812, -1.850976771919823793 ) ) ;
#66938 = CARTESIAN_POINT ( 'NONE',  ( -6.112028321662274166, 6.025121218227761588, 0.7998128361456341429 ) ) ;
#66939 = CARTESIAN_POINT ( 'NONE',  ( -11.86145017354119879, 10.09514365543875769, 1.099999999999996980 ) ) ;
#66940 = CARTESIAN_POINT ( 'NONE',  ( 5.865915527372128402, 0.6157079936559419764, -2.029145397309819021 ) ) ;
#66941 = AXIS2_PLACEMENT_3D ( 'NONE', #121800, #187767, #7947 ) ;
#66942 = CARTESIAN_POINT ( 'NONE',  ( -0.6823417656249969321, 3.217708333674754062, -1.181850606188749264 ) ) ;
#66943 = CARTESIAN_POINT ( 'NONE',  ( 6.890000000000029878, 7.629137130509094256, 2.600000000000001421 ) ) ;
#66944 = CARTESIAN_POINT ( 'NONE',  ( -4.284013352238255301, 6.981470763377843447, -1.082531754730549967 ) ) ;
#66945 = CARTESIAN_POINT ( 'NONE',  ( 5.695592476053609410, 1.958610405324921588, -0.8133567297157192622 ) ) ;
#66946 = CARTESIAN_POINT ( 'NONE',  ( -6.238160076063538284, 9.331584951165851294, 1.082531754730549967 ) ) ;
#66947 = ORIENTED_EDGE ( 'NONE', *, *, #173047, .F. ) ;
#66950 = MECHANICAL_DESIGN_GEOMETRIC_PRESENTATION_REPRESENTATION (  '', ( #11631 ), #1249 ) ;
#66949 = CARTESIAN_POINT ( 'NONE',  ( 6.245025451202089073, -1.828886558906620774, 1.152162773130911644 ) ) ;
#66948 = CARTESIAN_POINT ( 'NONE',  ( -5.370438244788932280, 6.398504386076097283, 1.082531754730549078 ) ) ;
#66951 = CARTESIAN_POINT ( 'NONE',  ( 4.710568305744190276, 7.583081225755162968, 1.199719254218462483 ) ) ;
#66952 = CARTESIAN_POINT ( 'NONE',  ( 6.339398910184078417, 0.6979989802004606947, -1.704029730133400866 ) ) ;
#66953 = FACE_OUTER_BOUND ( 'NONE', #157997, .T. ) ;
#66954 = CARTESIAN_POINT ( 'NONE',  ( -1.201851678989727383E-14, 2.134375000341423689, 1.575800808251672791 ) ) ;
#66955 = CARTESIAN_POINT ( 'NONE',  ( 0.8545597497816240784, 0.3412253653619911065, -1.706464705969434670 ) ) ;
#66956 = CARTESIAN_POINT ( 'NONE',  ( 2.900554798319789906, 5.471398800426671372, 1.199719254218452047 ) ) ;
#66957 = CARTESIAN_POINT ( 'NONE',  ( 11.55950211276791251, 12.29999999999998472, 3.221476510067111665 ) ) ;
#66958 = CARTESIAN_POINT ( 'NONE',  ( -1.364683531250014514, -0.1572916663252435232, 0.7879004041258379498 ) ) ;
#66959 = CARTESIAN_POINT ( 'NONE',  ( -0.4205683736966969177, 3.129384673317391563, -0.4296503687815703687 ) ) ;
#66960 = CARTESIAN_POINT ( 'NONE',  ( 4.821240550277555492, -0.1094919189667045711, 2.159058991224649393 ) ) ;
#66961 = CARTESIAN_POINT ( 'NONE',  ( -4.647747731386360215, 4.316793862905830892, 0.7998128361456341429 ) ) ;
#66962 = AXIS2_PLACEMENT_3D ( 'NONE', #47335, #31078, #97152 ) ;
#66963 = CARTESIAN_POINT ( 'NONE',  ( -6.602457619730773608, 8.725953194484466380, 1.443375672974078761 ) ) ;
#66964 = CARTESIAN_POINT ( 'NONE',  ( 4.979442225389012933, 2.018306902694905425, -0.7746836383674888804 ) ) ;
#66965 = ORIENTED_EDGE ( 'NONE', *, *, #160465, .T. ) ;
#66966 = CARTESIAN_POINT ( 'NONE',  ( -1.364683531250012516, 3.030208333674755394, 0.7879004041258379498 ) ) ;
#66967 = CARTESIAN_POINT ( 'NONE',  ( 6.221945801152132027, -1.093087313283289230, -1.640361058829779228 ) ) ;
#66968 = CARTESIAN_POINT ( 'NONE',  ( 5.325445489366991580, -1.254443461812755789, 1.197174301038748334 ) ) ;
#66969 = EDGE_CURVE ( 'NONE', #28791, #56620, #179698, .T. ) ;
#66971 = CARTESIAN_POINT ( 'NONE',  ( 2.279091853667324141, 2.002311374866962979, -0.8913168663882904408 ) ) ;
#66970 = CARTESIAN_POINT ( 'NONE',  ( -10.62873463776380056, 11.29999999999999893, -3.200000000000001510 ) ) ;
#66972 = CARTESIAN_POINT ( 'NONE',  ( 2.608792587697115639, -0.8827421749361822334, -2.132256252471361524 ) ) ;
#66973 = CARTESIAN_POINT ( 'NONE',  ( 4.938775350723108026, 0.3481798140595788738, 2.030979325763365928 ) ) ;
#66974 = CARTESIAN_POINT ( 'NONE',  ( 0.5154417807694658960, -1.038215432012145056, -1.640949389817857984 ) ) ;
#66975 = CARTESIAN_POINT ( 'NONE',  ( -7.659993601596726265, 8.039006744725394782, -0.7216878364870267237 ) ) ;
#66977 = ADVANCED_FACE ( 'NONE', ( #179686 ), #133394, .T. ) ;
#66976 = CARTESIAN_POINT ( 'NONE',  ( -5.167592825464113915, 6.057888380243431570, 1.199719254218452935 ) ) ;
#66978 = CARTESIAN_POINT ( 'NONE',  ( 4.786522169170392971, 5.141580351323886688, 0.8077998227834035649 ) ) ;
#66979 = CARTESIAN_POINT ( 'NONE',  ( 3.269896953881154644, 0.5115095171020591636, -2.057881918134551125 ) ) ;
#66980 = CARTESIAN_POINT ( 'NONE',  ( 1.459611520199757706, -1.915600648959712382, -0.6298732728240025169 ) ) ;
#66981 = CARTESIAN_POINT ( 'NONE',  ( -6.019457014343129408, 9.966524250134902729, 0.000000000000000000 ) ) ;
#66982 = CARTESIAN_POINT ( 'NONE',  ( 4.559734661428293201, 0.4870809927834463537, -2.152189095746533720 ) ) ;
#66983 = CARTESIAN_POINT ( 'NONE',  ( 0.000000000000000000, -2.384374999522042238, -3.793834371823813001 ) ) ;
#66984 = CARTESIAN_POINT ( 'NONE',  ( 1.674410341579468442, 1.254762736130067502, -1.374450116433557856 ) ) ;
#66985 = CARTESIAN_POINT ( 'NONE',  ( -0.1290005225502675879, 5.719648796287211567, -2.768066027128403217 ) ) ;
#66986 = CYLINDRICAL_SURFACE ( 'NONE', #73160, 0.08000000000000020983 ) ;
#66987 = FACE_OUTER_BOUND ( 'NONE', #102304, .T. ) ;
#66989 = CARTESIAN_POINT ( 'NONE',  ( 6.825078400183582694, 6.033236438919748146, 2.839236806905225841 ) ) ;
#66988 = CARTESIAN_POINT ( 'NONE',  ( -5.679622069920094773, 7.427521650927588759, -1.335666627332438683 ) ) ;
#66990 =( NAMED_UNIT ( * ) PLANE_ANGLE_UNIT ( ) SI_UNIT ( $, .RADIAN. ) );
#66991 = EDGE_LOOP ( 'NONE', ( #55012, #129550, #168619, #106939 ) ) ;
#66992 = CARTESIAN_POINT ( 'NONE',  ( 2.957942382388091040, 2.051108442962752409, -0.2004023863233852509 ) ) ;
#66993 = CARTESIAN_POINT ( 'NONE',  ( 0.6801582343749952297, 1.807291667008069425, -1.178068619123869398 ) ) ;
#66994 = CARTESIAN_POINT ( 'NONE',  ( -5.717788096661253761, 7.693838750903348789, 1.599625672291269396 ) ) ;
#66995 = CARTESIAN_POINT ( 'NONE',  ( 3.861976953351463848, 0.6784905939434657807, -1.902444917487989606 ) ) ;
#66996 = CARTESIAN_POINT ( 'NONE',  ( -0.7500000000000006661, 0.1083333333333560966, -1.299038105676652011 ) ) ;
#66997 = CARTESIAN_POINT ( 'NONE',  ( 8.419250204406344196, 12.76628297187536809, 1.040834085586084257E-14 ) ) ;
#66998 = CARTESIAN_POINT ( 'NONE',  ( 2.307559741017367383, -0.4527674059561050401, 2.010364544233154138 ) ) ;
#67000 = CARTESIAN_POINT ( 'NONE',  ( -0.6823417656250003738, 13.65104166700806232, 1.181850606188754593 ) ) ;
#66999 = CARTESIAN_POINT ( 'NONE',  ( -1.225000000000012523, 2.906250000341427331, -4.336808689942017736E-14 ) ) ;
#67001 = ADVANCED_FACE ( 'NONE', ( #150391 ), #55019, .T. ) ;
#67002 = CARTESIAN_POINT ( 'NONE',  ( 4.171104814498611368, 8.018039383557042044, 0.7998128361456321445 ) ) ;
#67003 = CARTESIAN_POINT ( 'NONE',  ( -0.1409997244346088141, 1.357410162930408504, -2.254437325861287533 ) ) ;
#67004 = CARTESIAN_POINT ( 'NONE',  ( 1.517261703430743625, -1.021610662766696764, -1.531488883528262512 ) ) ;
#67005 = CARTESIAN_POINT ( 'NONE',  ( 6.182275136424624229, -1.184133725572718676, 1.862117674348878760 ) ) ;
#67006 = CARTESIAN_POINT ( 'NONE',  ( 7.225569521440261767, 7.394528961293920233, -0.7998128361456341429 ) ) ;
#67007 = CARTESIAN_POINT ( 'NONE',  ( 1.757319832705085627, -1.853012815387704570, -1.112828241397870066 ) ) ;
#67008 = CARTESIAN_POINT ( 'NONE',  ( -3.958617665510279160, 5.641473247893851628, -1.443375672974053447 ) ) ;
#67009 = CARTESIAN_POINT ( 'NONE',  ( 2.219935720625454412, 0.9462983093676997637, -1.780669029686342331 ) ) ;
#67010 = CARTESIAN_POINT ( 'NONE',  ( -4.257741265285667431, 3.982435197156672491, 0.4597581080974452727 ) ) ;
#67011 = CARTESIAN_POINT ( 'NONE',  ( -0.1841593485105972039, 7.053066371975295290, 4.037421829300336995 ) ) ;
#67012 = SURFACE_SIDE_STYLE ('',( #103823 ) ) ;
#67013 = AXIS2_PLACEMENT_3D ( 'NONE', #98911, #194264, #97855 ) ;
#67014 = CARTESIAN_POINT ( 'NONE',  ( 4.188322375386017704, -1.949839058108787437, -0.2904977467932718382 ) ) ;
#67015 = CARTESIAN_POINT ( 'NONE',  ( 2.993375309983861143, -0.3886322325962355273, 1.978555244300662874 ) ) ;
#67017 = CARTESIAN_POINT ( 'NONE',  ( 8.690413276235306128, 13.08263988900915109, -0.7216878364870267237 ) ) ;
#67016 = CARTESIAN_POINT ( 'NONE',  ( -1.364683531250014514, 1.988541667008086655, -0.7879004041258289570 ) ) ;
#67019 = CARTESIAN_POINT ( 'NONE',  ( 6.463511354401173747, 0.3618736704080193212, -2.074577690073164060 ) ) ;
#67018 = CARTESIAN_POINT ( 'NONE',  ( -7.823218330285243383, 9.085841792542966644, -1.199719254218446718 ) ) ;
#67020 = CIRCLE ( 'NONE', #25603, 3.432849766368862632 ) ;
#67021 = CARTESIAN_POINT ( 'NONE',  ( 5.055165704564410944, 1.723227314588217318, -1.147259442322377865 ) ) ;
#67022 = CARTESIAN_POINT ( 'NONE',  ( 6.551614543901692400, 8.666636272683888365, 1.599625672291281386 ) ) ;
#67023 = CARTESIAN_POINT ( 'NONE',  ( -6.581593504430098385, 9.765943957555402122, -1.199719254218440723 ) ) ;
#67024 = CARTESIAN_POINT ( 'NONE',  ( 6.539320575229276677, 2.966918982532817051, 2.456386401752636672 ) ) ;
#67025 = CARTESIAN_POINT ( 'NONE',  ( 4.834242814930416188, -1.083969679716361156, -1.704088710659272810 ) ) ;
#67026 = CARTESIAN_POINT ( 'NONE',  ( -1.500000000000015099, -0.5479166659838513587, 0.8660254037844403729 ) ) ;
#67027 = CARTESIAN_POINT ( 'NONE',  ( 0.4618802912403723870, -0.5535076142849646441, 1.986819116141485653 ) ) ;
#67028 = CARTESIAN_POINT ( 'NONE',  ( 8.324343129110697959, 9.774450407793066731, -1.082531754730543083 ) ) ;
#67029 = CARTESIAN_POINT ( 'NONE',  ( 6.424584688029230328, 8.588711117491191871, 1.599625672291268286 ) ) ;
#67030 = CARTESIAN_POINT ( 'NONE',  ( 4.603875680292229156, 7.528882839386387360, 1.199719254218452047 ) ) ;
#67031 = CARTESIAN_POINT ( 'NONE',  ( -1.364683531250014514, 1.301041667008083325, -0.7879004041258289570 ) ) ;
#67033 = CARTESIAN_POINT ( 'NONE',  ( 6.827182134110234557, 2.482032550715262964, 2.096239902261677113 ) ) ;
#67032 = CARTESIAN_POINT ( 'NONE',  ( 3.555981428534177091, 7.370671776590375757, 0.7998128361456271485 ) ) ;
#67034 = CARTESIAN_POINT ( 'NONE',  ( 6.982085920913413624, 8.208483664896217391, -1.082531754730543971 ) ) ;
#67036 = CARTESIAN_POINT ( 'NONE',  ( 0.08000000000000020983, -7.246166700194011767, -9.579665964948882007 ) ) ;
#67035 = CARTESIAN_POINT ( 'NONE',  ( 2.840461511066312728, -1.118188532415839598, 1.860977255340636516 ) ) ;
#67037 = LINE ( 'NONE', #165639, #124016 ) ;
#67039 = CARTESIAN_POINT ( 'NONE',  ( 2.577489280727011778, -0.9446877197298314544, 1.580272903027237774 ) ) ;
#67038 = CARTESIAN_POINT ( 'NONE',  ( -3.741687207691642314, 6.348756928073427730, 1.082531754730560403 ) ) ;
#67040 = CARTESIAN_POINT ( 'NONE',  ( 0.6823417656249899377, 5.176041667008086655, -1.181850606188754593 ) ) ;
#67041 = CARTESIAN_POINT ( 'NONE',  ( 4.845371438081495619, 0.6875289519675978900, -2.081009137124201658 ) ) ;
#67042 = DIRECTION ( 'NONE',  ( 0.000000000000000000, 0.000000000000000000, 1.000000000000000000 ) ) ;
#67043 = CARTESIAN_POINT ( 'NONE',  ( 4.575235619729528302, 0.004297453766812646056, -2.262689076577176106 ) ) ;
#67044 = CARTESIAN_POINT ( 'NONE',  ( -5.122186659821378996, 6.697499048860120041, -1.435703471572645551 ) ) ;
#67045 = CARTESIAN_POINT ( 'NONE',  ( 5.694759483343039719, 7.307619849039811655, -1.219011658351103478 ) ) ;
#67046 = CARTESIAN_POINT ( 'NONE',  ( -4.624739795592936353, 7.449261290616792763, -1.082531754730549967 ) ) ;
#67047 = CARTESIAN_POINT ( 'NONE',  ( 4.746763178560254204, 6.631252689777363152, 1.443375672974065660 ) ) ;
#67048 = CARTESIAN_POINT ( 'NONE',  ( 6.766889846978989986, -1.619426471845460069, -0.7142080874563813131 ) ) ;
#67049 = CARTESIAN_POINT ( 'NONE',  ( 4.020185130887462321, -2.007537125943322120, 0.1504822817294942383 ) ) ;
#67050 = CARTESIAN_POINT ( 'NONE',  ( 7.308008492965924141, 8.484763649003774333, -1.199719254218451159 ) ) ;
#67051 = CARTESIAN_POINT ( 'NONE',  ( 2.819468948711697287, -0.2076110458819386551, 2.095707187103168945 ) ) ;
#67052 = CARTESIAN_POINT ( 'NONE',  ( 0.4564612863584472380, -1.804040949374663194, -0.6446129174930875783 ) ) ;
#67054 = CARTESIAN_POINT ( 'NONE',  ( -1.201851678989727383E-14, 2.212500000000021672, 1.732050807568877637 ) ) ;
#67053 = CARTESIAN_POINT ( 'NONE',  ( -0.6823417656250003738, 12.40104166700806232, 1.181850606188754593 ) ) ;
#67055 = CARTESIAN_POINT ( 'NONE',  ( 1.592182281804704003, 0.9734619808988297374, -1.712098776470400763 ) ) ;
#67056 = CARTESIAN_POINT ( 'NONE',  ( 0.6021629784135495989, -0.6261829430146518272, -1.762877433595814614 ) ) ;
#67057 = CARTESIAN_POINT ( 'NONE',  ( 1.275752070009423367, -1.914805681740685106, 0.4264308320794732432 ) ) ;
#67059 = VERTEX_POINT ( 'NONE', #99500 ) ;
#67058 = CARTESIAN_POINT ( 'NONE',  ( -0.1229892814952095459, -1.709044814581164973, -0.8582256167319823881 ) ) ;
#67060 = CARTESIAN_POINT ( 'NONE',  ( 5.422898255786183341, 7.349800603215774331, -1.443375672974051449 ) ) ;
#67061 = CARTESIAN_POINT ( 'NONE',  ( -1.364683531250012516, 0.5927083336747520637, 0.7879004041258379498 ) ) ;
#67062 = CARTESIAN_POINT ( 'NONE',  ( 5.998880656844745474, 1.528293836345222312, -1.078463600801618405 ) ) ;
#67063 = CARTESIAN_POINT ( 'NONE',  ( 9.541187415715040032, 12.15447128979948310, -1.599625672291262513 ) ) ;
#67064 = DIRECTION ( 'NONE',  ( -0.4243160830846685605, 0.9055141421511231359, 0.000000000000000000 ) ) ;
#67065 = CARTESIAN_POINT ( 'NONE',  ( 6.403194803628889709, -1.752124481401344358, 1.102429006916323395 ) ) ;
#67066 = FACE_OUTER_BOUND ( 'NONE', #98656, .T. ) ;
#67067 = CARTESIAN_POINT ( 'NONE',  ( 0.7310241076574041097, -1.948878508384953356, -0.6990896207654460071 ) ) ;
#67068 = CARTESIAN_POINT ( 'NONE',  ( -1.500000000000015099, 0.6291666666666863028, -0.8660254037844313801 ) ) ;
#67069 = CARTESIAN_POINT ( 'NONE',  ( 8.125414133291656071, 8.374071331795406081, -0.7998128361456291469 ) ) ;
#67070 = CARTESIAN_POINT ( 'NONE',  ( -8.525379664894808585, 8.840697785332414682, -0.7998128361456291469 ) ) ;
#67071 = CARTESIAN_POINT ( 'NONE',  ( 3.854260808034858155, 7.718664386007802136, -0.7998128361456362523 ) ) ;
#67072 = CARTESIAN_POINT ( 'NONE',  ( 5.408776937209000657, 5.274937613024121674, 0.7998128361456352531 ) ) ;
#67073 = CARTESIAN_POINT ( 'NONE',  ( -0.6823417656250003738, 0.9677083336747521747, -1.181850606188749264 ) ) ;
#67074 = ORIENTED_EDGE ( 'NONE', *, *, #71139, .T. ) ;
#67075 = CARTESIAN_POINT ( 'NONE',  ( -0.7500000000000006661, 2.858333333333358706, -1.299038105676652011 ) ) ;
#67077 = CARTESIAN_POINT ( 'NONE',  ( 4.847203612085560387, 5.613824621309978724, -1.199719254218452047 ) ) ;
#67076 = CARTESIAN_POINT ( 'NONE',  ( 5.775826483351648832, -1.914393393812302113, 0.4282712878391075062 ) ) ;
#67078 = CARTESIAN_POINT ( 'NONE',  ( 2.723982329760873178, -1.752761823190003287, -0.9961495992579154635 ) ) ;
#67079 = CARTESIAN_POINT ( 'NONE',  ( 3.467908617337426502, -0.9394263201649171169, 1.669454279737823343 ) ) ;
#67080 = CARTESIAN_POINT ( 'NONE',  ( 11.88156762547253997, 9.720000084540316720, -1.686557021358706443 ) ) ;
#67081 = CARTESIAN_POINT ( 'NONE',  ( 1.822082775007987543, 1.258534617508931586, -1.793986466278547853 ) ) ;
#67082 =( BOUNDED_SURFACE ( )  B_SPLINE_SURFACE ( 3, 2, ( 
 ( #32774, #14368, #131398 ),
 ( #180097, #115157, #52225 ),
 ( #65249, #133512, #118353 ),
 ( #197395, #97796, #80459 ),
 ( #147603, #146557, #181152 ),
 ( #182206, #213621, #164904 ) ),
 .UNSPECIFIED., .F., .F., .T. ) 
 B_SPLINE_SURFACE_WITH_KNOTS ( ( 4, 2, 4 ),
 ( 3, 3 ),
 ( 0.000000000000000000, 0.0003766365702389428338, 0.0007532731404778856676 ),
 ( 0.000000000000000000, 1.000000000000000000 ),
 .UNSPECIFIED. ) 
 GEOMETRIC_REPRESENTATION_ITEM ( )  RATIONAL_B_SPLINE_SURFACE ( (
 ( 1.000000000000000000, 0.7452309222762957264, 1.000000000000000000),
 ( 1.000000000000000000, 0.7451892422672021787, 1.000000000000000000),
 ( 1.000000000000000000, 0.7429606254238220187, 1.000000000000000000),
 ( 1.000000000000000000, 0.7311462761266275256, 1.000000000000000000),
 ( 1.000000000000000000, 0.7212257702790848546, 1.000000000000000000),
 ( 1.000000000000000000, 0.7071067811865551223, 1.000000000000000000) ) ) 
 REPRESENTATION_ITEM ( '' )  SURFACE ( )  );
#67083 = CARTESIAN_POINT ( 'NONE',  ( 0.2333690889706925009, 5.722554199285137422, -2.647406232470352894 ) ) ;
#67084 = CARTESIAN_POINT ( 'NONE',  ( 3.760894150569486616, -1.648321677062795976, -0.8843367818652316803 ) ) ;
#67085 = CARTESIAN_POINT ( 'NONE',  ( 1.499999999999985123, -1.172916665983846363, -0.8660254037844323793 ) ) ;
#67086 = CARTESIAN_POINT ( 'NONE',  ( -6.496328159242330536, 10.73079995242472862, 0.000000000000000000 ) ) ;
#67088 = CARTESIAN_POINT ( 'NONE',  ( 4.605136521778616654, -0.1025035295275648906, 2.114849348554531883 ) ) ;
#67087 = CARTESIAN_POINT ( 'NONE',  ( -5.097502569058225852, 5.049433873430440478, -0.7216878364870207285 ) ) ;
#67089 = LINE ( 'NONE', #71360, #14606 ) ;
#67090 = CARTESIAN_POINT ( 'NONE',  ( 6.303194806757332458, -1.751150776259063457, 1.104182018118210262 ) ) ;
#67092 = CARTESIAN_POINT ( 'NONE',  ( 4.055646997469144033, 7.518606479810191701, -0.4957702256945207830 ) ) ;
#67091 = CARTESIAN_POINT ( 'NONE',  ( 2.525039811729863359, -1.949768895325499463, 0.7551890176837258162 ) ) ;
#67094 = VERTEX_POINT ( 'NONE', #1960 ) ;
#67093 = CARTESIAN_POINT ( 'NONE',  ( 1.078623681775535914, -0.03615993657634165859, -1.724571457899269911 ) ) ;
#67095 = CARTESIAN_POINT ( 'NONE',  ( 7.786460292950004636, 7.978625184730144149, 1.040834085586084257E-14 ) ) ;
#67096 = CARTESIAN_POINT ( 'NONE',  ( 8.737618474220361975, 14.93717167570155446, 8.231545548724737316 ) ) ;
#67097 = DIRECTION ( 'NONE',  ( 1.000000000000000000, 0.000000000000000000, 0.000000000000000000 ) ) ;
#67099 = CARTESIAN_POINT ( 'NONE',  ( 5.938108092661121162, 9.871617174839238729, 1.040834085586084257E-14 ) ) ;
#67098 = CARTESIAN_POINT ( 'NONE',  ( 6.337546739384100292, 9.481222731668410120, 1.199719254218460707 ) ) ;
#67100 = DIRECTION ( 'NONE',  ( 1.000000000000000000, -0.000000000000000000, -0.000000000000000000 ) ) ;
#67102 = CARTESIAN_POINT ( 'NONE',  ( 0.8030048707254822116, 1.598173448761495585, -0.8528199064772985505 ) ) ;
#67101 = CARTESIAN_POINT ( 'NONE',  ( 5.671053392266061977, 9.838255734277600695, 0.7998128361456331437 ) ) ;
#67103 = CARTESIAN_POINT ( 'NONE',  ( -6.669721502918952716, 9.868759955792373972, 1.199719254218452047 ) ) ;
#67104 = CARTESIAN_POINT ( 'NONE',  ( 3.571683402196252910, 6.254382171615883834, 1.199719254218462483 ) ) ;
#67105 = CARTESIAN_POINT ( 'NONE',  ( -5.773214272755326171, 7.262619621122762048, 1.194638459467006530 ) ) ;
#67106 = CARTESIAN_POINT ( 'NONE',  ( 7.700104897918568447, 7.948153567185284096, 0.000000000000000000 ) ) ;
#67107 = CARTESIAN_POINT ( 'NONE',  ( 6.639320575229276322, 3.701785489019034259, 2.411212692025939131 ) ) ;
#67108 = DIRECTION ( 'NONE',  ( -1.000000000000000000, 0.000000000000000000, 0.000000000000000000 ) ) ;
#67109 = DIRECTION ( 'NONE',  ( -0.7808688094430278337, 0.6246950475544273962, 5.663618661477066041E-32 ) ) ;
#67110 = CARTESIAN_POINT ( 'NONE',  ( 8.270110514656021650, 11.63191745286530576, 1.082531754730557072 ) ) ;
#67111 = ORIENTED_EDGE ( 'NONE', *, *, #98727, .T. ) ;
#67112 = EDGE_CURVE ( 'NONE', #47534, #116561, #154233, .T. ) ;
#67113 = ORIENTED_EDGE ( 'NONE', *, *, #152281, .T. ) ;
#67114 = CARTESIAN_POINT ( 'NONE',  ( 2.558860573628952473, 1.496680913221506870, -1.105902276818030217 ) ) ;
#67115 = EDGE_CURVE ( 'NONE', #21086, #1801, #49661, .T. ) ;
#67116 = CARTESIAN_POINT ( 'NONE',  ( 0.7377199025260212650, 1.913388251642001103, -0.09504988074141537679 ) ) ;
#67117 = CARTESIAN_POINT ( 'NONE',  ( 0.7859742890132662696, 2.042544534415400737, -0.5693509180391894686 ) ) ;
#67118 = CARTESIAN_POINT ( 'NONE',  ( -1.880823357903582460, 8.986349088233119176, 0.7750000000000013545 ) ) ;
#67119 = STYLED_ITEM ( 'NONE', ( #152830 ), #2404 ) ;
#67120 = CARTESIAN_POINT ( 'NONE',  ( 1.854512760316388897, 2.488359591189891251, 2.484105960264901825 ) ) ;
#67121 = CARTESIAN_POINT ( 'NONE',  ( -1.567286081490176786, 8.684911043814580012, -2.501016734198262981 ) ) ;
#67122 = CARTESIAN_POINT ( 'NONE',  ( -3.118012141462980669, 6.581505231774690046, 0.7216878364870317197 ) ) ;
#67123 = CARTESIAN_POINT ( 'NONE',  ( 7.443063144222396232, 11.62739806832741785, 1.040834085586084257E-14 ) ) ;
#67124 = CARTESIAN_POINT ( 'NONE',  ( 4.979337304519595442, -0.1005905848140927622, 1.967025916208066327 ) ) ;
#67125 = CARTESIAN_POINT ( 'NONE',  ( 1.893382502257603850, -0.1070854039621378373, -2.117916637519041689 ) ) ;
#67126 = CARTESIAN_POINT ( 'NONE',  ( -6.013204822860843457, 6.974159367214481264, -1.199719254218446718 ) ) ;
#67127 = CARTESIAN_POINT ( 'NONE',  ( -11.59427420681528709, 8.291911680476573565, -2.926947285362574203 ) ) ;
#67128 = LINE ( 'NONE', #159594, #177289 ) ;
#67129 = CARTESIAN_POINT ( 'NONE',  ( 5.490230790444213582, -0.5297859672059505032, -2.126319610106224278 ) ) ;
#67130 = CARTESIAN_POINT ( 'NONE',  ( 9.508009452561562824, 4.000000000000000888, -7.612500000000001599 ) ) ;
#67131 = CARTESIAN_POINT ( 'NONE',  ( 4.717753586115435382, -1.889304338648789106, 0.3753660715558500005 ) ) ;
#67132 = CARTESIAN_POINT ( 'NONE',  ( -8.667740277838301921, 9.006785167099828016, -0.7998128361456291469 ) ) ;
#67133 = CARTESIAN_POINT ( 'NONE',  ( -0.6125000000000158096, 2.270833334016133964, -1.060881119635972647 ) ) ;
#67134 = CARTESIAN_POINT ( 'NONE',  ( 1.471597369358583096, 0.1596246592955492538, -2.201166978212334424 ) ) ;
#67135 = CYLINDRICAL_SURFACE ( 'NONE', #183069, 1.500000000000000222 ) ;
#67136 = ORIENTED_EDGE ( 'NONE', *, *, #92074, .T. ) ;
#67137 = CARTESIAN_POINT ( 'NONE',  ( 1.499999999999993117, 10.63541666734946212, 0.8660254037844408170 ) ) ;
#67138 = ORIENTED_EDGE ( 'NONE', *, *, #104977, .T. ) ;
#67139 = CARTESIAN_POINT ( 'NONE',  ( 6.403175662787183420, -1.665661181276241853, 1.050507712364300072 ) ) ;
#67140 = CARTESIAN_POINT ( 'NONE',  ( 1.470153547685297823, -1.844723335029124112, -0.6073778784492619431 ) ) ;
#67141 = CARTESIAN_POINT ( 'NONE',  ( 6.749376085230743172, -2.252018642839793472, -0.4587488502729390460 ) ) ;
#67143 = CARTESIAN_POINT ( 'NONE',  ( 4.451900780290086956, -0.7152352812324501707, 1.718214207458491849 ) ) ;
#67142 = CARTESIAN_POINT ( 'NONE',  ( -5.607179047703544583, 8.699403434699558346, 1.199719254218454489 ) ) ;
#67144 = CARTESIAN_POINT ( 'NONE',  ( 7.713663051532233972, 7.963971413067895355, -0.7998128361456341429 ) ) ;
#67145 = SURFACE_STYLE_FILL_AREA ( #79163 ) ;
#67146 = CARTESIAN_POINT ( 'NONE',  ( -5.636439174979254396, 7.598931675607687453, -1.599625672291256295 ) ) ;
#67147 = CARTESIAN_POINT ( 'NONE',  ( -3.360593407046564618, -0.9395304069187625506, 0.08390535222174622110 ) ) ;
#67148 = CARTESIAN_POINT ( 'NONE',  ( 0.09952931447375359952, -0.5783855404800625211, 2.113812074898171023 ) ) ;
#67149 = CARTESIAN_POINT ( 'NONE',  ( 4.609409038966229666, 6.400729850259146758, -1.443375672974051449 ) ) ;
#67150 = DIRECTION ( 'NONE',  ( 0.000000000000000000, 1.000000000000000000, 0.000000000000000000 ) ) ;
#67151 = PLANE ( 'NONE',  #106804 ) ;
#67152 = CARTESIAN_POINT ( 'NONE',  ( 1.629252094361890890, -1.719607636260962025, 0.6136192449261099746 ) ) ;
#67153 = CARTESIAN_POINT ( 'NONE',  ( -3.436101866059630527, 6.096203712789787232, 1.199719254218462483 ) ) ;
#67154 = CARTESIAN_POINT ( 'NONE',  ( 3.779676010894826188, 1.462474260537292681, -0.9315460551484288088 ) ) ;
#67155 = CARTESIAN_POINT ( 'NONE',  ( 0.003603623020859416434, 2.503419261533966100, -2.003492231431212467 ) ) ;
#67156 = CARTESIAN_POINT ( 'NONE',  ( 6.509000000000014552, 2.444259026362519904, 2.383015625331697862 ) ) ;
#67157 = CARTESIAN_POINT ( 'NONE',  ( 0.1331565106231606399, 5.723858289613107608, -2.539976893513963052 ) ) ;
#67158 = CARTESIAN_POINT ( 'NONE',  ( 0.1527873662319845505, -1.548267161427993255, 1.146224303156289093 ) ) ;
#67159 = CARTESIAN_POINT ( 'NONE',  ( 4.082823661314609609, 1.861412734803047142, 0.6194944872321900275 ) ) ;
#67160 = CARTESIAN_POINT ( 'NONE',  ( -8.715193815486133033, 9.062147627688959872, 0.7998128361456462443 ) ) ;
#67161 = CARTESIAN_POINT ( 'NONE',  ( 5.880485940025228508, 7.883652901494672349, 1.599625672291267398 ) ) ;
#67162 = CARTESIAN_POINT ( 'NONE',  ( 4.512424090126602394, -2.120028616272570332, -0.05109941365945279423 ) ) ;
#67163 = CARTESIAN_POINT ( 'NONE',  ( 7.289443866002793371, 8.533381260871966134, 1.199719254218452047 ) ) ;
#67164 = B_SPLINE_CURVE_WITH_KNOTS ( 'NONE', 3,
 ( #86165, #85093, #151178, #133889, #39547, #102410 ),
 .UNSPECIFIED., .F., .F.,
 ( 4, 2, 4 ),
 ( 1.347205729526718589E-17, 9.978364048176284397E-05, 0.0001995672809635122167 ),
 .UNSPECIFIED. ) ;
#67165 = CIRCLE ( 'NONE', #18645, 11.09999999999999964 ) ;
#67166 = CARTESIAN_POINT ( 'NONE',  ( -8.239604668803112375, 10.63595808506888396, -1.599625672291263179 ) ) ;
#67167 = CARTESIAN_POINT ( 'NONE',  ( 5.281064527722868718, 6.119995689553514140, 1.199719254218462483 ) ) ;
#67168 = CARTESIAN_POINT ( 'NONE',  ( 3.186448005867897670, 1.153939711166888982, -1.718631068965512210 ) ) ;
#67170 = CARTESIAN_POINT ( 'NONE',  ( 0.6823417656249882723, 0.4885416670080827695, -1.181850606188749264 ) ) ;
#67169 =( LENGTH_UNIT ( ) NAMED_UNIT ( * ) SI_UNIT ( .MILLI., .METRE. ) );
#67171 = EDGE_LOOP ( 'NONE', ( #178781, #47894, #203844, #135507 ) ) ;
#67172 = CARTESIAN_POINT ( 'NONE',  ( 2.778317543532899947, 1.969881296151472894, -1.184559908770227432 ) ) ;
#67173 = CARTESIAN_POINT ( 'NONE',  ( 7.944714827928043732, 10.29191993738131927, 1.443375672974076540 ) ) ;
#67175 = CARTESIAN_POINT ( 'NONE',  ( -1.642778471874998480, -2.151041666188707957, 2.845375778867863303 ) ) ;
#67174 = CARTESIAN_POINT ( 'NONE',  ( 7.377044979611483200, 7.779176362401098999, -0.7216878364870317197 ) ) ;
#67176 = B_SPLINE_CURVE_WITH_KNOTS ( 'NONE', 3,
 ( #107494, #85840, #72777, #119472 ),
 .UNSPECIFIED., .F., .F.,
 ( 4, 4 ),
 ( 0.000000000000000000, 1.930757672285080358E-06 ),
 .UNSPECIFIED. ) ;
#67177 = FILL_AREA_STYLE ('',( #200384 ) ) ;
#67178 = DIRECTION ( 'NONE',  ( -0.000000000000000000, -1.000000000000000000, -0.000000000000000000 ) ) ;
#67179 = EDGE_LOOP ( 'NONE', ( #32515, #117241 ) ) ;
#67180 = CARTESIAN_POINT ( 'NONE',  ( 0.000000000000000000, 19.00000000000000000, -12.00000000000000178 ) ) ;
#67181 = EDGE_CURVE ( 'NONE', #158693, #119038, #200171, .T. ) ;
#67182 = CARTESIAN_POINT ( 'NONE',  ( 4.148624843374196125, 1.876505540506741010, 0.3678670841067502861 ) ) ;
#67183 = CARTESIAN_POINT ( 'NONE',  ( 5.174679765213248572, -1.625057609515182078, -0.5782863776828560676 ) ) ;
#67184 = CARTESIAN_POINT ( 'NONE',  ( 3.257046257486408969, 0.04465439498414420366, -2.016188763087948033 ) ) ;
#67185 = CARTESIAN_POINT ( 'NONE',  ( 5.362068906036296490, -0.05402111011005260310, -2.298215290733228500 ) ) ;
#67186 = CARTESIAN_POINT ( 'NONE',  ( -4.296393142825893463, 0.4330127018922214077, 4.470011852588161361 ) ) ;
#67187 = CARTESIAN_POINT ( 'NONE',  ( 1.172829962703396456, -1.397616723802884708, 1.707921395779465890 ) ) ;
#67188 = CARTESIAN_POINT ( 'NONE',  ( -4.340018570150309785, 7.117086527600392287, -1.082531754730551743 ) ) ;
#67189 = CARTESIAN_POINT ( 'NONE',  ( 6.134039733390581617, 0.8703851191177320867, -1.540848210998513990 ) ) ;
#67191 = CARTESIAN_POINT ( 'NONE',  ( 2.238584135424640298, 0.5043332063416061661, 2.235947581072089907 ) ) ;
#67190 = CARTESIAN_POINT ( 'NONE',  ( 5.631432701629774051, 7.663367133358481631, 1.599625672291269396 ) ) ;
#67192 = CARTESIAN_POINT ( 'NONE',  ( 6.703072984701052839, -0.3981723446819797063, 1.804146177254343009 ) ) ;
#67193 = CARTESIAN_POINT ( 'NONE',  ( -6.312203035614172286, 9.521931420595302953, -1.199719254218452047 ) ) ;
#67194 = DIRECTION ( 'NONE',  ( 0.000000000000000000, 0.000000000000000000, -1.000000000000000000 ) ) ;
#67195 = CARTESIAN_POINT ( 'NONE',  ( -4.573896719763875574, 6.429575154514868274, -1.599625672291271394 ) ) ;
#67196 = CARTESIAN_POINT ( 'NONE',  ( -1.360316468750016439, -0.07812499965861169349, -3.469446951953614189E-14 ) ) ;
#67197 = CARTESIAN_POINT ( 'NONE',  ( -0.02968770228140016343, 0.003472272166151618711, -1.826291111852257343 ) ) ;
#67198 = CARTESIAN_POINT ( 'NONE',  ( 6.496543107701719499, 2.047251205643263017, 0.3077783505985449142 ) ) ;
#67199 = CARTESIAN_POINT ( 'NONE',  ( 0.9015777671340443611, -1.966303774932298021, 0.4465067697373495403 ) ) ;
#67200 = CARTESIAN_POINT ( 'NONE',  ( 0.7499999999999885647, -0.2354166659838466402, 1.299038105676657340 ) ) ;
#67201 = CARTESIAN_POINT ( 'NONE',  ( 5.127533266204091333, -1.828772253489078237, 0.6060055780525953617 ) ) ;
#67202 = CARTESIAN_POINT ( 'NONE',  ( 1.364683531250000303, 12.25520833367473195, -0.7879004041258355073 ) ) ;
#67203 = CARTESIAN_POINT ( 'NONE',  ( 2.092296997076743548, 1.370790743785160970, 1.747926019109148799 ) ) ;
#67204 = ORIENTED_EDGE ( 'NONE', *, *, #130004, .T. ) ;
#67206 = CARTESIAN_POINT ( 'NONE',  ( -6.760415694342130179E-18, -5.633679745285109895E-18, -0.4330127018938150774 ) ) ;
#67205 = CARTESIAN_POINT ( 'NONE',  ( 0.000000000000000000, 2.817530495244580102, 1.214306433183764966E-14 ) ) ;
#67207 = CARTESIAN_POINT ( 'NONE',  ( 3.840479349152599919, 7.346192795665340114, 0.4818892653144311033 ) ) ;
#67208 = CARTESIAN_POINT ( 'NONE',  ( 10.06423010004587759, 10.63602329300870153, 0.000000000000000000 ) ) ;
#67209 = CARTESIAN_POINT ( 'NONE',  ( -9.579764304849156531, -9.919999999999998153, 0.06720017513374074158 ) ) ;
#67210 = FACE_OUTER_BOUND ( 'NONE', #16088, .T. ) ;
#67211 = CARTESIAN_POINT ( 'NONE',  ( 4.774825072940077852, 1.621577360410943802, -0.6326411939767513370 ) ) ;
#67212 = CARTESIAN_POINT ( 'NONE',  ( 2.699599903323801620, -1.451799986561516764, -1.319707477925702310 ) ) ;
#67214 = CARTESIAN_POINT ( 'NONE',  ( -7.714226216495749355, 8.102278128774251797, 1.040834085586084257E-14 ) ) ;
#67213 = CARTESIAN_POINT ( 'NONE',  ( 3.337278367258157630, 7.045241861776501580, 0.7998128361456341429 ) ) ;
#67215 = CARTESIAN_POINT ( 'NONE',  ( -5.903030530102264528, 6.005529115149156993, -0.1628943571830038795 ) ) ;
#67216 = CARTESIAN_POINT ( 'NONE',  ( -3.475000000000000533, -2.085416665710750905, -2.006292185433948827 ) ) ;
#67217 = CARTESIAN_POINT ( 'NONE',  ( 0.7310139678005268538, -1.941628062548940381, -0.6965263486069167564 ) ) ;
#67218 = CARTESIAN_POINT ( 'NONE',  ( -8.342344591110322227, 8.627156865917170236, -0.7998128361456291469 ) ) ;
#67219 = CARTESIAN_POINT ( 'NONE',  ( -4.433153041544240835, 4.274359424664112339, 0.7216878364870317197 ) ) ;
#67220 = VECTOR ( 'NONE', #186874, 1000.000000000000000 ) ;
#67221 = CARTESIAN_POINT ( 'NONE',  ( 1.745381597357411385, -1.910777759476259163, 1.211296049258607788 ) ) ;
#67222 = VERTEX_POINT ( 'NONE', #100558 ) ;
#67223 = CARTESIAN_POINT ( 'NONE',  ( -1.500000000000001332, -0.3187499993171846735, 0.000000000000000000 ) ) ;
#67224 = CARTESIAN_POINT ( 'NONE',  ( 2.424885678431305092, -0.004389691185376768875, 1.870726058193001196 ) ) ;
#67225 = CARTESIAN_POINT ( 'NONE',  ( 1.125167334363995852, 0.3372632679971860337, 1.700812921812058454 ) ) ;
#67226 = EDGE_CURVE ( 'NONE', #146583, #73220, #152512, .T. ) ;
#67227 = CARTESIAN_POINT ( 'NONE',  ( 5.548420995840112724, -1.728225626343689925, 1.347513067664840358 ) ) ;
#67228 = CARTESIAN_POINT ( 'NONE',  ( 5.737451576302465384, -2.089288847444936259, 0.9800045452074584995 ) ) ;
#67229 = CARTESIAN_POINT ( 'NONE',  ( 1.164996006578455923, -1.862832630767555120, -0.8818606138344189382 ) ) ;
#67230 = CARTESIAN_POINT ( 'NONE',  ( 3.240110121693033474, 0.4724093276110411521, 1.883494029347228871 ) ) ;
#67231 = CARTESIAN_POINT ( 'NONE',  ( -4.189106276498259618, 6.870745841681152655, 1.082531754730560403 ) ) ;
#67232 = MECHANICAL_DESIGN_GEOMETRIC_PRESENTATION_REPRESENTATION (  '', ( #174599 ), #75939 ) ;
#67233 = CARTESIAN_POINT ( 'NONE',  ( 6.028550586359523678, 1.802609027081774951, 0.4991829554215552744 ) ) ;
#67234 = CARTESIAN_POINT ( 'NONE',  ( 0.8437500000000005551, 1.895863743164106774, 0.7852924748299443536 ) ) ;
#67235 = EDGE_CURVE ( 'NONE', #53793, #34146, #86447, .T. ) ;
#67236 = CARTESIAN_POINT ( 'NONE',  ( 4.063008298707909027, 7.508743736771079647, -0.5217633019904341918 ) ) ;
#67237 = CARTESIAN_POINT ( 'NONE',  ( 6.222029796014385106, -1.727739227931901489, -1.038831587593692873 ) ) ;
#67238 = CARTESIAN_POINT ( 'NONE',  ( 0.6801582343749987825, 1.557291667008103841, -1.178068619123876282 ) ) ;
#67239 = CARTESIAN_POINT ( 'NONE',  ( 4.693982515131527755, 1.755768268644173791, 0.9914009648221073778 ) ) ;
#67240 = CARTESIAN_POINT ( 'NONE',  ( -5.219525951136862574, 5.191794485855519170, -0.7216878364870197293 ) ) ;
#67241 = CARTESIAN_POINT ( 'NONE',  ( 8.097244055859613709, 10.46987070330147063, -1.599625672291262513 ) ) ;
#67242 = CARTESIAN_POINT ( 'NONE',  ( 5.225741863424510747, 5.061396693608882558, 0.7998128361456352531 ) ) ;
#67243 = CARTESIAN_POINT ( 'NONE',  ( 2.103868193876055503, -1.825329726703457833, 0.04394198290156441783 ) ) ;
#67244 = CARTESIAN_POINT ( 'NONE',  ( -5.418418667316934112, 6.350518529071726981, -1.199719254218453823 ) ) ;
#67245 = CARTESIAN_POINT ( 'NONE',  ( -0.1296875068448125334, 2.048176110289974261, -2.243787855586779401 ) ) ;
#67246 = CARTESIAN_POINT ( 'NONE',  ( -0.3282377607281289911, 1.761164550367436021, -1.225000000000013634 ) ) ;
#67247 = ORIENTED_EDGE ( 'NONE', *, *, #103483, .T. ) ;
#67248 = CARTESIAN_POINT ( 'NONE',  ( -6.590672069574513792, 6.861741300691274859, 0.000000000000000000 ) ) ;
#67249 = CARTESIAN_POINT ( 'NONE',  ( -4.437596350374534815, 4.071617251725375475, -0.7998128361456221525 ) ) ;
#67250 = CARTESIAN_POINT ( 'NONE',  ( -8.188234707649510113, 11.64035869464474082, -1.199719254218446718 ) ) ;
#67251 = CARTESIAN_POINT ( 'NONE',  ( 0.3166733070498818359, -0.6846287639105748113, -1.900330225253379801 ) ) ;
#67252 = CARTESIAN_POINT ( 'NONE',  ( 6.586594613159782341, -1.369803613283290700, 1.749543456560544552 ) ) ;
#67253 = CARTESIAN_POINT ( 'NONE',  ( -7.747558435566414659, 8.003516027774422170, -0.7998128361456362523 ) ) ;
#67254 = CARTESIAN_POINT ( 'NONE',  ( 5.250031796989762967, 7.148123067953287446, 1.599625672291267398 ) ) ;
#67255 = CARTESIAN_POINT ( 'NONE',  ( 5.454002199308585652, 2.058645617578058751, -0.09870700237277732492 ) ) ;
#67256 = CARTESIAN_POINT ( 'NONE',  ( 5.010388774477188889, -1.913804350592800407, 0.6351971752796631288 ) ) ;
#67257 = VERTEX_POINT ( 'NONE', #69098 ) ;
#67258 = ORIENTED_EDGE ( 'NONE', *, *, #129790, .F. ) ;
#67259 = CARTESIAN_POINT ( 'NONE',  ( 2.888709804529736136, 6.440345301045965698, 0.3798094595594287415 ) ) ;
#67261 = DIRECTION ( 'NONE',  ( 0.000000000000000000, 0.000000000000000000, -1.000000000000000000 ) ) ;
#67260 = CARTESIAN_POINT ( 'NONE',  ( -5.281783360975562225, 8.319775133516907673, 1.199719254218452935 ) ) ;
#67262 = CARTESIAN_POINT ( 'NONE',  ( 4.655672573246532941, 8.415299432525721102, 0.4976263304441782553 ) ) ;
#67263 = CARTESIAN_POINT ( 'NONE',  ( 5.255232437486731634, -2.000551055875991580, -0.2495666058281582056 ) ) ;
#67264 = CARTESIAN_POINT ( 'NONE',  ( 4.611176429654996412, -1.805050139478355353, 0.3618648703537508671 ) ) ;
#67265 = DIRECTION ( 'NONE',  ( 0.000000000000000000, 0.000000000000000000, -1.000000000000000000 ) ) ;
#67266 = CARTESIAN_POINT ( 'NONE',  ( 3.791899867668945490, 1.670594791088287678, 1.592266751676748582 ) ) ;
#67267 = CARTESIAN_POINT ( 'NONE',  ( 5.318541398310776103, 9.426991741329731056, -0.7998128361456481317 ) ) ;
#67268 = CARTESIAN_POINT ( 'NONE',  ( 5.184929619776310616, -0.2588774643964042999, -2.145956309214678726 ) ) ;
#67270 = CARTESIAN_POINT ( 'NONE',  ( 6.446011968293428041, 9.607765498729298415, -1.199719254218440723 ) ) ;
#67269 = CARTESIAN_POINT ( 'NONE',  ( 3.467982673848205355, -0.9896861206786079501, 1.756853968756578066 ) ) ;
#67271 = CARTESIAN_POINT ( 'NONE',  ( 0.5560688330792910028, -1.405822068596472407, 1.340092691751965770 ) ) ;
#67272 = CARTESIAN_POINT ( 'NONE',  ( -3.490334480514268645, 6.159475096320226939, -1.199719254218452935 ) ) ;
#67273 = CARTESIAN_POINT ( 'NONE',  ( 3.989890550291860016, 2.181093686755405603, 0.7249921343481547931 ) ) ;
#67274 = CARTESIAN_POINT ( 'NONE',  ( -0.6823417656250003738, 2.967708333674754062, -1.181850606188749264 ) ) ;
#67275 = CARTESIAN_POINT ( 'NONE',  ( -4.492547798081878874, 6.334668079219206049, 1.599625672291263179 ) ) ;
#67276 = CARTESIAN_POINT ( 'NONE',  ( 3.379631771358857950, 1.185797501207178861, 1.446808710765794315 ) ) ;
#67279 = CARTESIAN_POINT ( 'NONE',  ( -5.237192476628793614, 9.332084666034067055, 0.7998128361456291469 ) ) ;
#67278 = CARTESIAN_POINT ( 'NONE',  ( 1.499999999999987566, -0.4437499993171847845, 0.000000000000000000 ) ) ;
#67277 = CARTESIAN_POINT ( 'NONE',  ( 0.9317291061951762376, -1.865162313430932750, 0.4216105838140621342 ) ) ;
#67280 = CARTESIAN_POINT ( 'NONE',  ( 2.877765823869771644, 2.095344539500657799, -0.6929138170133213315 ) ) ;
#67281 = CARTESIAN_POINT ( 'NONE',  ( 6.346625304528514810, 6.577020074804287297, 0.000000000000000000 ) ) ;
#67282 = CARTESIAN_POINT ( 'NONE',  ( 5.515469562660962666, 5.329135999392899947, 0.7998128361456341429 ) ) ;
#67283 = DIRECTION ( 'NONE',  ( 0.000000000000000000, -1.000000000000000000, 0.000000000000000000 ) ) ;
#67284 = CARTESIAN_POINT ( 'NONE',  ( -2.449219305563052895, 6.009172956465517856, 1.040834085586084257E-14 ) ) ;
#67285 = CARTESIAN_POINT ( 'NONE',  ( -7.892254816486440561, 8.380254505421877553, 0.000000000000000000 ) ) ;
#67286 = CARTESIAN_POINT ( 'NONE',  ( 0.2980362317399931626, -1.970818609879662953, -0.05296617050038961161 ) ) ;
#67287 = CARTESIAN_POINT ( 'NONE',  ( 6.586558022634583232, -2.261718397432868066, -0.4576183726279075548 ) ) ;
#67288 = CARTESIAN_POINT ( 'NONE',  ( 1.381223342121252085, -0.05156877537583307025, 1.961363007973878858 ) ) ;
#67289 = CARTESIAN_POINT ( 'NONE',  ( 4.452046733557501135, -0.7940950990443145230, 1.903769949380555770 ) ) ;
#67290 = CARTESIAN_POINT ( 'NONE',  ( 6.480434237652135998, 6.662854153456708950, 0.7216878364870317197 ) ) ;
#67291 = CARTESIAN_POINT ( 'NONE',  ( 6.852720297064418986, 6.959538199522133262, 0.7998128361456331437 ) ) ;
#67292 = ORIENTED_EDGE ( 'NONE', *, *, #179963, .T. ) ;
#67293 = CARTESIAN_POINT ( 'NONE',  ( 7.090551149822722721, 11.21613407486112379, 0.7216878364870438212 ) ) ;
#67294 = CARTESIAN_POINT ( 'NONE',  ( -1.364683531250012516, 4.801041667008083991, -0.7879004041258300672 ) ) ;
#67295 = CARTESIAN_POINT ( 'NONE',  ( 6.933263157960373846, 7.629137130509066722, 2.546189081643289942 ) ) ;
#67296 = CARTESIAN_POINT ( 'NONE',  ( 4.812781342726870193, 4.717259109377208048, 0.7216878364870317197 ) ) ;
#67297 = CARTESIAN_POINT ( 'NONE',  ( 0.3038947965873342039, -1.677446906807459337, -1.377854473705003580 ) ) ;
#67298 = CARTESIAN_POINT ( 'NONE',  ( 9.495512617570035729, -9.134774474195877403, -0.2994571439533144641 ) ) ;
#67299 = CARTESIAN_POINT ( 'NONE',  ( -5.100224957694119432, 6.410602811745620855, 1.321793204645645980 ) ) ;
#67300 = LINE ( 'NONE', #3373, #80816 ) ;
#67301 = CARTESIAN_POINT ( 'NONE',  ( 1.036156370570060270, 1.841834720703208639, 0.3256331921374157057 ) ) ;
#67302 = CARTESIAN_POINT ( 'NONE',  ( -6.112394247781385737, 6.011859825068855301, 0.2949881747824866229 ) ) ;
#67303 = CARTESIAN_POINT ( 'NONE',  ( -0.02264175331119500090, 1.349762599094967763, -2.344447671987642146 ) ) ;
#67304 = CARTESIAN_POINT ( 'NONE',  ( 5.253852870291571442, 7.792406146126436006, -1.285611862062207011 ) ) ;
#67305 = CARTESIAN_POINT ( 'NONE',  ( 1.364683531249990311, 4.946875000341417916, 1.214306433183764966E-14 ) ) ;
#67306 = CARTESIAN_POINT ( 'NONE',  ( 1.242663310189826564, 1.843194135250892707, 0.5091577964371831744 ) ) ;
#67307 = CARTESIAN_POINT ( 'NONE',  ( 2.975218959772182536, 1.681091501613757533, -0.5536541633112538330 ) ) ;
#67308 = CARTESIAN_POINT ( 'NONE',  ( 1.172351427048579531, 0.7757545017167380985, 1.748050575570128329 ) ) ;
#67310 = CARTESIAN_POINT ( 'NONE',  ( 4.218306492681688447, 1.879367783149912929, 0.3698934672397135581 ) ) ;
#67309 = CARTESIAN_POINT ( 'NONE',  ( 2.535847408461032609E-15, 11.09999999999999432, 0.2598076211376220135 ) ) ;
#67311 = CARTESIAN_POINT ( 'NONE',  ( 5.230891393285493685, -1.853837313009810028, -0.6654804215649990917 ) ) ;
#67312 = CARTESIAN_POINT ( 'NONE',  ( 1.019968326173793960, -0.5097545255977399270, 2.058319881341897695 ) ) ;
#67313 = CARTESIAN_POINT ( 'NONE',  ( 4.184706906422049677, 7.590773377626947038, -0.8858016570119742195 ) ) ;
#67314 = CARTESIAN_POINT ( 'NONE',  ( 3.432352559540859271, 1.824792983844251371, 0.4109263881779609551 ) ) ;
#67316 = EDGE_LOOP ( 'NONE', ( #95690, #86401 ) ) ;
#67315 = CARTESIAN_POINT ( 'NONE',  ( 0.3635304476994546952, 1.806310985241452949, -0.2645042207462811046 ) ) ;
#67318 = CARTESIAN_POINT ( 'NONE',  ( -4.570507181138272479, 7.385989907086349504, 1.082531754730549967 ) ) ;
#67317 = CARTESIAN_POINT ( 'NONE',  ( 3.967548030458594166, 0.2710504330169676845, -2.190103208553782821 ) ) ;
#67319 = CARTESIAN_POINT ( 'NONE',  ( -1.364683531250012516, 4.301041667008089320, -0.7879004041258300672 ) ) ;
#67320 = CARTESIAN_POINT ( 'NONE',  ( 2.348159106025033083, -0.8842165242596754515, 1.863692774951962727 ) ) ;
#67321 = CARTESIAN_POINT ( 'NONE',  ( 7.935599982700328958, 8.152621489438862667, 0.7998128361456481317 ) ) ;
#67323 = CARTESIAN_POINT ( 'NONE',  ( -7.804689982961090955, 12.25722208009664094, 0.7998128361456481317 ) ) ;
#67322 = VECTOR ( 'NONE', #143162, 1000.000000000000000 ) ;
#67324 = CARTESIAN_POINT ( 'NONE',  ( -0.8965429266985017742, 15.44733976321393953, -11.92417820654543448 ) ) ;
#67325 = CARTESIAN_POINT ( 'NONE',  ( 11.94105721237522921, 10.90000000000000036, -1.187919463087248939 ) ) ;
#67326 = CARTESIAN_POINT ( 'NONE',  ( 6.363533315466952445, -1.540175188624912428, -1.133462061071670579 ) ) ;
#67327 = ORIENTED_EDGE ( 'NONE', *, *, #130606, .T. ) ;
#67328 = CARTESIAN_POINT ( 'NONE',  ( 4.773920332862017446, -2.031068740936771366, 0.4005940302675218834 ) ) ;
#67330 = CARTESIAN_POINT ( 'NONE',  ( 1.499999999999987121, 4.295833333333352044, -0.8660254037844323793 ) ) ;
#67329 = CIRCLE ( 'NONE', #164306, 9.499999999999991118 ) ;
#67331 = CARTESIAN_POINT ( 'NONE',  ( 1.933122032479916985, 0.2097677157741582865, 2.151362962771664833 ) ) ;
#67332 = CARTESIAN_POINT ( 'NONE',  ( -5.826481282663010575, 7.222486169913409526, -1.172043233395845485 ) ) ;
#67333 = CARTESIAN_POINT ( 'NONE',  ( 1.559246255342447984, -1.705015668849844124, 1.082290385971399926 ) ) ;
#67334 = DIRECTION ( 'NONE',  ( -0.6743504407196689865, -1.104276606162287428E-12, -0.7384114592157872137 ) ) ;
#67336 = CARTESIAN_POINT ( 'NONE',  ( 7.131225611108079399, 11.26358761302737754, 0.7216878364870438212 ) ) ;
#67335 = CARTESIAN_POINT ( 'NONE',  ( 3.475000000000000533, -3.675000000000001155, 0.000000000000000000 ) ) ;
#67337 = CARTESIAN_POINT ( 'NONE',  ( 6.766953912288387940, -2.015720078709513086, 0.04667315333419658208 ) ) ;
#67338 = CARTESIAN_POINT ( 'NONE',  ( 0.5851731681005939434, 1.651346252830317551, 1.157095189655330314 ) ) ;
#67339 = CARTESIAN_POINT ( 'NONE',  ( 6.639320575229263888, 1.250520135805782251, 2.217830841512329787 ) ) ;
#67340 = CARTESIAN_POINT ( 'NONE',  ( 4.616832073239669043, -0.1072513232249286408, 2.189039617437993357 ) ) ;
#67341 = CARTESIAN_POINT ( 'NONE',  ( 1.499999999999989120, 3.285416667349486897, 0.8660254037844524744 ) ) ;
#67342 = CARTESIAN_POINT ( 'NONE',  ( 4.025576834063953946, -0.3218090080209669024, 1.884953445776993863 ) ) ;
#67343 = CARTESIAN_POINT ( 'NONE',  ( -3.418627288940168096, 7.140148937072163804, -0.7998128361456281477 ) ) ;
#67344 = CARTESIAN_POINT ( 'NONE',  ( 3.673896439178918172, 6.269667698141953238, 1.082531754730558626 ) ) ;
#67346 = CARTESIAN_POINT ( 'NONE',  ( 1.634388897023292486, 0.6352195160324504153, 1.913798142305182415 ) ) ;
#67345 = DIRECTION ( 'NONE',  ( -1.207943261119674327E-30, -2.168404344971008079E-15, 1.000000000000000000 ) ) ;
#67347 = CARTESIAN_POINT ( 'NONE',  ( -0.6823417656250003738, 12.46354166700806765, 1.181850606188754593 ) ) ;
#67349 = CARTESIAN_POINT ( 'NONE',  ( -3.955946960137363799, 7.837298230127379917, 0.7998128361456352531 ) ) ;
#67348 = CARTESIAN_POINT ( 'NONE',  ( 0.2579210422260198587, 2.266244506498811706, -0.3445303224042794432 ) ) ;
#67350 = CARTESIAN_POINT ( 'NONE',  ( 4.348488605181799471, 0.4613061074445113374, 1.661866727659202736 ) ) ;
#67351 = CARTESIAN_POINT ( 'NONE',  ( -0.1399997263889559695, 7.629137130509076492, -2.600276787041354343 ) ) ;
#67352 = CARTESIAN_POINT ( 'NONE',  ( 3.659811400685081040, 6.357198169852855685, -1.199719254218446718 ) ) ;
#67353 = CARTESIAN_POINT ( 'NONE',  ( -11.48243876534946040, 12.30000000000000071, -3.200000000000001510 ) ) ;
#67354 = CARTESIAN_POINT ( 'NONE',  ( 1.223018651738450480, -1.772137153356953432, -0.8420139538000551704 ) ) ;
#67355 = CARTESIAN_POINT ( 'NONE',  ( -1.499999999999997780, 4.681250000682819490, 1.214306433183764966E-14 ) ) ;
#67356 = CARTESIAN_POINT ( 'NONE',  ( 5.705283713252285338, 5.550585841749444249, -0.7998128361456211532 ) ) ;
#67357 = CARTESIAN_POINT ( 'NONE',  ( 0.07536363704233049743, 0.2309889609098912111, -2.177957698420322163 ) ) ;
#67358 = EDGE_LOOP ( 'NONE', ( #14644, #84808, #192965, #189629 ) ) ;
#67359 =( NAMED_UNIT ( * ) SI_UNIT ( $, .STERADIAN. ) SOLID_ANGLE_UNIT ( ) );
#67360 = VERTEX_POINT ( 'NONE', #121168 ) ;
#67361 = CARTESIAN_POINT ( 'NONE',  ( 4.441949062027584993, -1.118158961774197380, -1.425077651336349227 ) ) ;
#67362 =( GEOMETRIC_REPRESENTATION_CONTEXT ( 3 ) GLOBAL_UNCERTAINTY_ASSIGNED_CONTEXT ( ( #142675 ) ) GLOBAL_UNIT_ASSIGNED_CONTEXT ( ( #178473, #196841, #111402 ) ) REPRESENTATION_CONTEXT ( 'NONE', 'WORKASPACE' ) );
#67363 = EDGE_LOOP ( 'NONE', ( #178576, #104790, #17360, #101463 ) ) ;
#67364 = CARTESIAN_POINT ( 'NONE',  ( 6.424584688029230328, 8.588711117491191871, 1.599625672291268286 ) ) ;
#67365 = CARTESIAN_POINT ( 'NONE',  ( 6.781144757626058173, -7.161464053357574855, -6.776370306708051849 ) ) ;
#67366 = CARTESIAN_POINT ( 'NONE',  ( 4.389189793862141364, -0.004542125399705549196, -1.811656973097997447 ) ) ;
#67367 = CARTESIAN_POINT ( 'NONE',  ( 5.356880090730850696, 9.263794182579101033, 0.7216878364870317197 ) ) ;
#67368 = CARTESIAN_POINT ( 'NONE',  ( 8.081892667527529994, -5.166862915010145052, -7.462104991928515396 ) ) ;
#67369 = CARTESIAN_POINT ( 'NONE',  ( 5.833718835943604297, 6.012594516355426855, -0.4067158398524447493 ) ) ;
#67370 = EDGE_LOOP ( 'NONE', ( #101913, #169234, #107968, #38788 ) ) ;
#67371 = EDGE_CURVE ( 'NONE', #98728, #115710, #169328, .T. ) ;
#67373 = CARTESIAN_POINT ( 'NONE',  ( 8.516493047678546091, 13.08765898893368629, -0.7998128361456352531 ) ) ;
#67372 = CARTESIAN_POINT ( 'NONE',  ( 6.602007162813277041, 0.7109360278478898953, -1.720114357745919476 ) ) ;
#67374 = CARTESIAN_POINT ( 'NONE',  ( 4.288635103545942684, 1.478190772419993415, -1.218367487985058339 ) ) ;
#67375 = CARTESIAN_POINT ( 'NONE',  ( -6.381095703207997794, -8.233137084989849086, -7.037870247915931188 ) ) ;
#67376 = CARTESIAN_POINT ( 'NONE',  ( -11.78039045457385292, 4.728130269440308453, 4.968650233931813709 ) ) ;
#67377 =( GEOMETRIC_REPRESENTATION_CONTEXT ( 3 ) GLOBAL_UNCERTAINTY_ASSIGNED_CONTEXT ( ( #30210 ) ) GLOBAL_UNIT_ASSIGNED_CONTEXT ( ( #27032, #80059, #61682 ) ) REPRESENTATION_CONTEXT ( 'NONE', 'WORKASPACE' ) );
#67378 = CARTESIAN_POINT ( 'NONE',  ( 9.499643733017418157, -9.912496545390952818, -0.08228199421454375495 ) ) ;
#67379 = SURFACE_SIDE_STYLE ('',( #199526 ) ) ;
#67380 = CARTESIAN_POINT ( 'NONE',  ( 4.989037340148863464, 8.764367963574922982, -0.7216878364870257245 ) ) ;
#67382 = CARTESIAN_POINT ( 'NONE',  ( 5.208266738515407113, 1.258803676730145371, -1.702402541353124077 ) ) ;
#67381 = CARTESIAN_POINT ( 'NONE',  ( -2.656508033273816238, 5.186677574539687363, -1.199719254218446718 ) ) ;
#67383 = CARTESIAN_POINT ( 'NONE',  ( 0.4796413896344040029, 2.016494124141111399, -0.7793912508547717888 ) ) ;
#67384 = CARTESIAN_POINT ( 'NONE',  ( -4.125423880308188629, 8.035021303660014880, -0.7998128361456481317 ) ) ;
#67385 = CARTESIAN_POINT ( 'NONE',  ( 4.355912491740495440, 8.303924683664389406, 0.000000000000000000 ) ) ;
#67386 = CARTESIAN_POINT ( 'NONE',  ( 1.149113351018778539, -1.436424422225426767, -1.126575773451453433 ) ) ;
#67387 = CARTESIAN_POINT ( 'NONE',  ( -4.765854690403601879, 5.518917546014321829, 1.199719254218462483 ) ) ;
#67388 = CARTESIAN_POINT ( 'NONE',  ( 3.205874166558682514, -1.823564452915670042, 0.08818595847179949709 ) ) ;
#67389 = EDGE_CURVE ( 'NONE', #80820, #58907, #17150, .T. ) ;
#67390 = CARTESIAN_POINT ( 'NONE',  ( 10.81010058466664425, 10.31570469300483950, 6.498163104334348183 ) ) ;
#67391 = ORIENTED_EDGE ( 'NONE', *, *, #16861, .T. ) ;
#67392 = CARTESIAN_POINT ( 'NONE',  ( 2.295301284060722313, -1.760697607696968037, 0.8827641120334356328 ) ) ;
#67393 = CARTESIAN_POINT ( 'NONE',  ( 4.317874670498635048, 1.191976824791032064, -1.533171632797071693 ) ) ;
#67394 = CARTESIAN_POINT ( 'NONE',  ( -8.086512275908061653, 8.398962174839683215, 0.000000000000000000 ) ) ;
#67396 = CARTESIAN_POINT ( 'NONE',  ( 3.849942018323779358, -1.464806807754112539, -1.533599281611098597 ) ) ;
#67395 = CARTESIAN_POINT ( 'NONE',  ( 7.614839552730775729, 8.913009562054615031, 1.199719254218452047 ) ) ;
#67397 = CARTESIAN_POINT ( 'NONE',  ( -5.717509255324293882, 7.006698007003660855, -2.500000000000000444 ) ) ;
#67398 = CARTESIAN_POINT ( 'NONE',  ( 2.631394046745598736, -0.1854624247320437458, 1.903247139735386284 ) ) ;
#67399 = CARTESIAN_POINT ( 'NONE',  ( 5.915399107357110609, 6.142141269072955545, 0.7871259410536131096 ) ) ;
#67400 = DIRECTION ( 'NONE',  ( 0.7592566023653005702, -0.6507913734559639396, 0.000000000000000000 ) ) ;
#67401 = ORIENTED_EDGE ( 'NONE', *, *, #162793, .T. ) ;
#67402 = CARTESIAN_POINT ( 'NONE',  ( -0.8997935122536572239, 14.48154075026818965, 12.00000000000000000 ) ) ;
#67403 = CARTESIAN_POINT ( 'NONE',  ( 5.740951700743842423, 5.662474837148078421, -0.7998128361456481317 ) ) ;
#67404 = FACE_OUTER_BOUND ( 'NONE', #18670, .T. ) ;
#67405 = CARTESIAN_POINT ( 'NONE',  ( 4.617693566336190436, -1.789886777702164089, 0.3589094947460610974 ) ) ;
#67406 = CARTESIAN_POINT ( 'NONE',  ( 10.99954523395721218, -9.918132210574695407, -0.1000458187401192384 ) ) ;
#67407 = CARTESIAN_POINT ( 'NONE',  ( -9.680158490477310806, 10.39586578175276266, 0.7216878364870438212 ) ) ;
#67408 = CARTESIAN_POINT ( 'NONE',  ( -6.212075186202199006, 7.030024481103895440, 1.038766164041710738 ) ) ;
#67409 = CARTESIAN_POINT ( 'NONE',  ( 1.150196859685074235, 2.895291321728038714, -0.7750000000000022427 ) ) ;
#67410 = CARTESIAN_POINT ( 'NONE',  ( 5.700035372616791385, -1.870836310086241294, 0.001406584917262864625 ) ) ;
#67411 = CARTESIAN_POINT ( 'NONE',  ( 8.098297826064319693, 8.342435640030188893, 0.7998128361456481317 ) ) ;
#67412 = CARTESIAN_POINT ( 'NONE',  ( -3.913499895838973508, 7.717500311787445000, 1.040834085586084257E-14 ) ) ;
#67413 = CARTESIAN_POINT ( 'NONE',  ( 3.246287715468270108, 5.874753870433235825, 1.199719254218450271 ) ) ;
#67414 = CARTESIAN_POINT ( 'NONE',  ( -1.364683531250000748, 10.92187500034139802, 0.000000000000000000 ) ) ;
#67415 = CARTESIAN_POINT ( 'NONE',  ( -5.117312914154178216, 8.057616602233474978, -1.199719254218452047 ) ) ;
#67416 = CARTESIAN_POINT ( 'NONE',  ( 3.871016551901614200, 4.474939717762034697, -1.199719254218446718 ) ) ;
#67417 = CARTESIAN_POINT ( 'NONE',  ( -3.648552735408990166, 6.310376387068841630, -1.082531754730546636 ) ) ;
#67418 = CARTESIAN_POINT ( 'NONE',  ( -5.259673527097670664, 8.223703984000886535, -1.199719254218446718 ) ) ;
#67419 = CARTESIAN_POINT ( 'NONE',  ( 0.4970418144054839504, 0.3504251219754518365, 2.040211723117946629 ) ) ;
#67420 = CARTESIAN_POINT ( 'NONE',  ( 1.036884384669316539, -1.666496236897334615, 1.305811245984341173 ) ) ;
#67421 = CARTESIAN_POINT ( 'NONE',  ( 9.426996880203592610, 9.892584536526015881, -0.7998128361456281477 ) ) ;
#67422 = CARTESIAN_POINT ( 'NONE',  ( 0.1263921867887890238, 7.050106634750518353, 4.033475513000639445 ) ) ;
#67423 = CARTESIAN_POINT ( 'NONE',  ( 6.737176827083626307, -0.09545985418329960837, -2.068160202195384656 ) ) ;
#67425 = CARTESIAN_POINT ( 'NONE',  ( 4.670798236633449285, 6.855725761985807409, -1.225018586207384352 ) ) ;
#67424 = CARTESIAN_POINT ( 'NONE',  ( 1.364538772237647413, 0.1349417713633893900, -1.836341338755695940 ) ) ;
#67426 = CARTESIAN_POINT ( 'NONE',  ( 5.341549334104188418, 7.254893527920112994, 1.443375672974062551 ) ) ;
#67428 = DIRECTION ( 'NONE',  ( 0.000000000000000000, 0.000000000000000000, 1.000000000000000000 ) ) ;
#67427 = CARTESIAN_POINT ( 'NONE',  ( 3.475000000000000533, -3.704166666666666163, 2.006292185433948827 ) ) ;
#67429 = CARTESIAN_POINT ( 'NONE',  ( 1.535548486519675571, -1.662869323620078665, -1.577994866025609566 ) ) ;
#67431 = CARTESIAN_POINT ( 'NONE',  ( 0.2333690889706820926, 2.873202992247088083, -2.541887414127189881 ) ) ;
#67430 = CARTESIAN_POINT ( 'NONE',  ( -1.360600954992994938, 3.300000000000193445, 0.1676728910578147713 ) ) ;
#67432 = ORIENTED_EDGE ( 'NONE', *, *, #177718, .T. ) ;
#67433 = CARTESIAN_POINT ( 'NONE',  ( 7.849807752188022292, 11.14156422998596696, -1.082531754730543083 ) ) ;
#67434 = ADVANCED_FACE ( 'NONE', ( #890 ), #51757, .T. ) ;
#67435 = CARTESIAN_POINT ( 'NONE',  ( 0.9318904303841836212, -1.963229875443720074, 0.4450799344311164862 ) ) ;
#67436 = CARTESIAN_POINT ( 'NONE',  ( 0.7956631384608278124, -1.383255022760669251, -1.391342014947573924 ) ) ;
#67437 = CARTESIAN_POINT ( 'NONE',  ( -9.296355089585910693E-16, 2.750000000682797818, -1.225000000000007860 ) ) ;
#67439 = CARTESIAN_POINT ( 'NONE',  ( -9.748930057865852206, 3.057420161666833280, -6.444087955423147385 ) ) ;
#67438 = CARTESIAN_POINT ( 'NONE',  ( -9.189729191964438826, 9.615772233580322848, 1.040834085586084257E-14 ) ) ;
#67440 = CARTESIAN_POINT ( 'NONE',  ( 3.285556943749998737, -0.3427083328553764408, -1.896917185911906500 ) ) ;
#67442 = CARTESIAN_POINT ( 'NONE',  ( 2.395042364772178356, 1.366200922416866526, 1.125074557178520118 ) ) ;
#67441 = CARTESIAN_POINT ( 'NONE',  ( 4.083990600187762610, -2.067889708199427190, -0.3066597852425279047 ) ) ;
#67443 = CARTESIAN_POINT ( 'NONE',  ( -1.886825320689270225, 2.480000000000016858, 2.459652456995881753 ) ) ;
#67445 = CARTESIAN_POINT ( 'NONE',  ( 5.613300874620239078, -2.237517390240588711, 0.4973276143641935931 ) ) ;
#67444 = CARTESIAN_POINT ( 'NONE',  ( -1.225000000000028066, 2.020833333333377446, 0.7072540797572697269 ) ) ;
#67446 = CARTESIAN_POINT ( 'NONE',  ( 3.591523995615089948, -1.738451970352115961, -0.08344189160913899339 ) ) ;
#67447 = CARTESIAN_POINT ( 'NONE',  ( 8.530051201292206287, 13.10347683481629488, 0.000000000000000000 ) ) ;
#67448 = CARTESIAN_POINT ( 'NONE',  ( 2.846726617453724906, -0.8940771029739991160, 1.485372309294562543 ) ) ;
#67449 = CARTESIAN_POINT ( 'NONE',  ( 3.086559893568251223, 1.208301842568102247, -1.803703480758335642 ) ) ;
#67450 = CARTESIAN_POINT ( 'NONE',  ( 3.472859903394816872, 7.203420320602605287, -0.7998128361456291469 ) ) ;
#67451 = CARTESIAN_POINT ( 'NONE',  ( 6.175017591530616023, 1.752142144017948100, -0.9981200475188132248 ) ) ;
#67452 = CARTESIAN_POINT ( 'NONE',  ( 6.750000000000005329, 0.5343081985527837752, 2.030663454312888305 ) ) ;
#67453 = CARTESIAN_POINT ( 'NONE',  ( 0.7499999999999920064, 4.514583334016150751, 1.299038105676669330 ) ) ;
#67454 = CARTESIAN_POINT ( 'NONE',  ( 2.590742828618552984, -0.3275076452619613554, -1.898194946008352035 ) ) ;
#67455 = CARTESIAN_POINT ( 'NONE',  ( 1.499999999999997113, 9.177083334016128191, -0.8660254037844378194 ) ) ;
#67456 = CARTESIAN_POINT ( 'NONE',  ( 5.853820293109783357, -1.608621682386938589, -1.532244055152881312 ) ) ;
#67457 = ORIENTED_EDGE ( 'NONE', *, *, #139381, .T. ) ;
#67458 = CARTESIAN_POINT ( 'NONE',  ( -0.1108833634137010027, 2.037774818562386514, -2.313487243312782216 ) ) ;
#67459 = CARTESIAN_POINT ( 'NONE',  ( 1.499999999999987121, 1.254166666666689300, 0.8660254037844524744 ) ) ;
#67460 = CARTESIAN_POINT ( 'NONE',  ( 5.113396490648394632, 9.117379672398465473, 1.040834085586084257E-14 ) ) ;
#67461 = CARTESIAN_POINT ( 'NONE',  ( 5.626270559546826533, 5.666329862333828515, 0.7216878364870317197 ) ) ;
#67462 = CARTESIAN_POINT ( 'NONE',  ( 3.285556943749998737, -2.005208332855377140, -1.896917185911906722 ) ) ;
#67463 = CARTESIAN_POINT ( 'NONE',  ( 1.401376347886007068, -0.3305552470432049916, -2.196467622588905932 ) ) ;
#67464 = CARTESIAN_POINT ( 'NONE',  ( 0.4294077647110511320, -6.532648833121157850, 9.469892045836672878 ) ) ;
#67465 = CARTESIAN_POINT ( 'NONE',  ( 9.422553571817644524, 10.09532670998316384, 0.000000000000000000 ) ) ;
#67466 =( NAMED_UNIT ( * ) PLANE_ANGLE_UNIT ( ) SI_UNIT ( $, .RADIAN. ) );
#67467 = CARTESIAN_POINT ( 'NONE',  ( 6.766858430912646938, -2.064281441484459023, -0.9263300772878214628 ) ) ;
#67468 = CARTESIAN_POINT ( 'NONE',  ( 5.337069745634900997, 6.255611453776062980, 1.199719254218452047 ) ) ;
#67469 = CARTESIAN_POINT ( 'NONE',  ( -5.329763783947941036, 5.390681634126922361, 0.000000000000000000 ) ) ;
#67470 = CARTESIAN_POINT ( 'NONE',  ( 4.000476411064065374, 2.052455503700638229, 0.2052804401120340017 ) ) ;
#67471 = CARTESIAN_POINT ( 'NONE',  ( -4.608882153641705059, 7.464447381635583412, -1.199719254218452047 ) ) ;
#67472 =( BOUNDED_CURVE ( )  B_SPLINE_CURVE ( 2, ( #27007, #93113, #182862, #46483, #16074, #113676, #100552 ),
 .UNSPECIFIED., .F., .T. ) 
 B_SPLINE_CURVE_WITH_KNOTS ( ( 3, 2, 2, 3 ),
 ( 0.3959408239114771133, 0.3988095238095238360, 0.4047619047619047672, 0.4076306046599514343 ),
 .UNSPECIFIED. ) 
 CURVE ( )  GEOMETRIC_REPRESENTATION_ITEM ( )  RATIONAL_B_SPLINE_CURVE ( ( 0.9331000818465633451, 0.9354320710352559409, 1.000000000000000000, 0.8660254037844387076, 1.000000000000000000, 0.9354320710352564960, 0.9331000818465632340 ) ) 
 REPRESENTATION_ITEM ( '' )  );
#67473 = VECTOR ( 'NONE', #155665, 1000.000000000000227 ) ;
#67474 = CARTESIAN_POINT ( 'NONE',  ( -0.7500000000000215383, 4.472916667349482012, 1.299038105676671107 ) ) ;
#67475 = CARTESIAN_POINT ( 'NONE',  ( 1.364683531249988757, 0.1343750003414204142, 0.000000000000000000 ) ) ;
#67476 = CARTESIAN_POINT ( 'NONE',  ( 5.958239543830243790, 0.7576973323653664050, 1.710380810381225913 ) ) ;
#67477 = CARTESIAN_POINT ( 'NONE',  ( 4.535645802837630747, -1.388783131305007634, 1.038275480396163353 ) ) ;
#67478 = CARTESIAN_POINT ( 'NONE',  ( 4.757210230733205591, 1.720523950154304371, -0.2617468875206073742 ) ) ;
#67479 = CARTESIAN_POINT ( 'NONE',  ( 2.672928840188529609, 6.270167413528593414, 0.000000000000000000 ) ) ;
#67480 = ADVANCED_FACE ( 'NONE', ( #88596 ), #97313, .F. ) ;
#67481 = CARTESIAN_POINT ( 'NONE',  ( 1.488225144363482189, -2.281859108288700089, -0.2192131398826550337 ) ) ;
#67482 = CARTESIAN_POINT ( 'NONE',  ( -1.364683531250010295, 4.842708333674756283, 0.7879004041258379498 ) ) ;
#67483 = CARTESIAN_POINT ( 'NONE',  ( 6.128480205876102538, 0.2055166225264984381, 2.080635545183810553 ) ) ;
#67484 = CARTESIAN_POINT ( 'NONE',  ( 0.1812672858593766811, -0.8707521589867758260, 1.622202602641155345 ) ) ;
#67485 = CARTESIAN_POINT ( 'NONE',  ( 0.1062647551455935674, -6.683951888245091233, 9.488025208486869033 ) ) ;
#67486 = CARTESIAN_POINT ( 'NONE',  ( 2.092422861153935276, -0.4390285686692517175, 1.967888031366466395 ) ) ;
#67487 = FACE_OUTER_BOUND ( 'NONE', #172415, .T. ) ;
#67488 = CARTESIAN_POINT ( 'NONE',  ( 8.346583974317809407, 13.15480872911727594, -8.542606490713003708 ) ) ;
#67489 = CARTESIAN_POINT ( 'NONE',  ( -8.040148788103921973, 9.338927326664741457, 1.199719254218462483 ) ) ;
#67490 =( BOUNDED_SURFACE ( )  B_SPLINE_SURFACE ( 3, 2, ( 
 ( #158159, #59569, #125727 ),
 ( #27063, #62761, #77954 ),
 ( #128923, #174419, #79016 ),
 ( #112661, #191688, #176530 ),
 ( #109468, #29215, #146186 ),
 ( #145133, #144075, #212200 ),
 ( #28142, #178670, #44411 ),
 ( #30284, #60636, #160276 ),
 ( #194902, #192754, #11878 ),
 ( #210071, #61710, #127878 ),
 ( #25995, #43348, #13999 ),
 ( #193828, #12937, #9750 ),
 ( #95305, #175476, #63837 ),
 ( #45478, #93169, #161354 ) ),
 .UNSPECIFIED., .F., .F., .F. ) 
 B_SPLINE_SURFACE_WITH_KNOTS ( ( 4, 2, 2, 2, 2, 2, 4 ),
 ( 3, 3 ),
 ( 0.000000000000000000, 0.0002390010041311327435, 0.0004780020082622654870, 0.0009560040165245309741, 0.001195005020655663663, 0.001434006024786796570, 0.001912008033049061948 ),
 ( 0.000000000000000000, 1.000000000000000000 ),
 .UNSPECIFIED. ) 
 GEOMETRIC_REPRESENTATION_ITEM ( )  RATIONAL_B_SPLINE_SURFACE ( (
 ( 1.000000000000000000, 0.4915962107220928079, 1.000000000000000000),
 ( 1.000000000000000000, 0.4903111309377012894, 1.000000000000000000),
 ( 1.000000000000000000, 0.5057854813392914650, 1.000000000000000000),
 ( 1.000000000000000000, 0.5532305778937092189, 1.000000000000000000),
 ( 1.000000000000000000, 0.5846576190777243998, 1.000000000000000000),
 ( 1.000000000000000000, 0.6796638612361862730, 1.000000000000000000),
 ( 1.000000000000000000, 0.7435379557940324791, 1.000000000000000000),
 ( 1.000000000000000000, 0.8106661767825003029, 1.000000000000000000),
 ( 1.000000000000000000, 0.8285023559306291530, 1.000000000000000000),
 ( 1.000000000000000000, 0.8541358093761527437, 1.000000000000000000),
 ( 1.000000000000000000, 0.8615977546920583485, 1.000000000000000000),
 ( 1.000000000000000000, 0.8740883989871980342, 1.000000000000000000),
 ( 1.000000000000000000, 0.8700938199805592355, 1.000000000000000000),
 ( 1.000000000000000000, 0.8708456909032173954, 1.000000000000000000) ) ) 
 REPRESENTATION_ITEM ( '' )  SURFACE ( )  );
#67491 = CARTESIAN_POINT ( 'NONE',  ( 4.659198344590585350, 8.587481835331020719, 0.7998128361456462443 ) ) ;
#67492 = CARTESIAN_POINT ( 'NONE',  ( 1.360316468750001784, 2.286458333674732835, -0.7853790794158941324 ) ) ;
#67494 = B_SPLINE_CURVE_WITH_KNOTS ( 'NONE', 3,
 ( #96686, #180041, #31663, #82518, #147546, #162735, #68386, #163799 ),
 .UNSPECIFIED., .F., .F.,
 ( 4, 2, 2, 4 ),
 ( 0.000000000000000000, 0.0005156231957999836413, 0.0007734347936999756788, 0.001031246391599967716 ),
 .UNSPECIFIED. ) ;
#67493 = CARTESIAN_POINT ( 'NONE',  ( 3.123802294713691641, -0.4116375371931815796, 2.079978743196985391 ) ) ;
#67495 = CARTESIAN_POINT ( 'NONE',  ( -1.402160292154681736E-14, -0.5531249996585814177, -1.575800808251665908 ) ) ;
#67497 = EDGE_CURVE ( 'NONE', #139854, #209617, #174747, .T. ) ;
#67496 = CARTESIAN_POINT ( 'NONE',  ( 5.461492464141177727, 0.3521552718798379722, -1.791230276788812414 ) ) ;
#67498 = ORIENTED_EDGE ( 'NONE', *, *, #64465, .F. ) ;
#67499 = CARTESIAN_POINT ( 'NONE',  ( -6.469175572376043348, 7.576401584974034265, 1.199719254218452047 ) ) ;
#67500 = CARTESIAN_POINT ( 'NONE',  ( 1.001543065824772753E-15, -3.018749999044083587, 4.012584370867899430 ) ) ;
#67501 = CARTESIAN_POINT ( 'NONE',  ( -6.728924311084075960, 6.744833205886536120, 1.040834085586084257E-14 ) ) ;
#67502 = CARTESIAN_POINT ( 'NONE',  ( 3.304948908139183406, -0.3981353638667082806, -1.979975013379015936 ) ) ;
#67503 = CARTESIAN_POINT ( 'NONE',  ( 6.598651186688741177, -0.5821561243712966016, -2.128545807824663960 ) ) ;
#67504 = CARTESIAN_POINT ( 'NONE',  ( 3.555356577358064207, 1.464247429212956808, 1.148356018212342233 ) ) ;
#67505 = CARTESIAN_POINT ( 'NONE',  ( 8.055515824813896941, 12.54985222892493368, 0.7998128361456462443 ) ) ;
#67506 =( BOUNDED_CURVE ( )  B_SPLINE_CURVE ( 2, ( #197850, #211963, #63602, #49482, #115602, #129756, #177360, #195741, #47378 ),
 .UNSPECIFIED., .F., .T. ) 
 B_SPLINE_CURVE_WITH_KNOTS ( ( 3, 2, 2, 2, 3 ),
 ( 0.3482142857142856429, 0.3511904761904761640, 0.3571428571428571508, 0.3630952380952380820, 0.3660714285714286031 ),
 .UNSPECIFIED. ) 
 CURVE ( )  GEOMETRIC_REPRESENTATION_ITEM ( )  RATIONAL_B_SPLINE_CURVE ( ( 0.9330127018922194093, 0.9330127018922180770, 1.000000000000000000, 0.8660254037844387076, 1.000000000000000000, 0.8660254037844387076, 1.000000000000000000, 0.9330127018922187432, 0.9330127018922194093 ) ) 
 REPRESENTATION_ITEM ( '' )  );
#67507 = CARTESIAN_POINT ( 'NONE',  ( 10.59763834280244232, 12.29999999999999893, -3.303285708550596222 ) ) ;
#67508 = CARTESIAN_POINT ( 'NONE',  ( -2.605138072120212200, 6.191078184115536232, -0.7998128361456281477 ) ) ;
#67509 = CARTESIAN_POINT ( 'NONE',  ( -6.645467848992654858, 10.90479625713344625, 0.7998128361456481317 ) ) ;
#67510 = CIRCLE ( 'NONE', #22673, 0.08000000000000020983 ) ;
#67512 = CARTESIAN_POINT ( 'NONE',  ( -4.920796802804098924, 6.860114910817498135, 1.449587651302047364 ) ) ;
#67511 = CARTESIAN_POINT ( 'NONE',  ( -6.831329296439251131, 9.063246493969506545, -1.599625672291271394 ) ) ;
#67513 = CARTESIAN_POINT ( 'NONE',  ( 5.396826230253299883, 7.665096674459883630, -1.326205021280580265 ) ) ;
#67514 = CARTESIAN_POINT ( 'NONE',  ( 1.598581759805017155, 0.8596790983186454183, -1.505624278722474951 ) ) ;
#67515 = CARTESIAN_POINT ( 'NONE',  ( 0.7084657485305994040, -0.2594935844701939387, 1.720731466566546519 ) ) ;
#67517 = CARTESIAN_POINT ( 'NONE',  ( 8.459924665247367415, 8.972259652317825740, -0.7216878364870267237 ) ) ;
#67516 = CARTESIAN_POINT ( 'NONE',  ( 0.2007804849885147513, -2.307177064702860214, -0.05170730859792996986 ) ) ;
#67518 = CARTESIAN_POINT ( 'NONE',  ( -10.99931038725301846, 6.873658557531565627, -3.960823121322395224 ) ) ;
#67519 = CARTESIAN_POINT ( 'NONE',  ( 1.247419646546283234, -1.622699693697586820, -1.270148745232473564 ) ) ;
#67520 = CARTESIAN_POINT ( 'NONE',  ( 4.157546660884947620, 8.002221537674429896, 1.040834085586084257E-14 ) ) ;
#67521 = CARTESIAN_POINT ( 'NONE',  ( 6.292345239091892140, -2.167472901860421519, 0.7650227848022586041 ) ) ;
#67522 = CARTESIAN_POINT ( 'NONE',  ( 0.000000000000000000, 3.956598013261175772, 0.000000000000000000 ) ) ;
#67523 = CARTESIAN_POINT ( 'NONE',  ( -6.459533842268148973, 6.500820668926428958, 0.000000000000000000 ) ) ;
#67524 = EDGE_CURVE ( 'NONE', #204725, #52497, #80857, .T. ) ;
#67525 = CARTESIAN_POINT ( 'NONE',  ( 6.508674657442179878, 1.384610780642284711, -1.258058027910214927 ) ) ;
#67526 = PRESENTATION_LAYER_ASSIGNMENT (  '', '', ( #119428 ) ) ;
#67528 = CARTESIAN_POINT ( 'NONE',  ( -7.593975437430151132, 8.032261896522864930, -0.7216878364870338292 ) ) ;
#67527 = CARTESIAN_POINT ( 'NONE',  ( 5.115449499555525747, 1.566912803841558732, 1.096118974231160781 ) ) ;
#67529 = CARTESIAN_POINT ( 'NONE',  ( 6.586557750117827403, -2.163372447211810989, -0.4352210726449382006 ) ) ;
#67530 = CARTESIAN_POINT ( 'NONE',  ( -6.234224025626352805, -6.938199013094628498, -6.849482339516213436 ) ) ;
#67531 = CARTESIAN_POINT ( 'NONE',  ( 3.879041346841291649, 7.539648981374564407, 1.040834085586084257E-14 ) ) ;
#67532 = VECTOR ( 'NONE', #114422, 1000.000000000000000 ) ;
#67533 = CARTESIAN_POINT ( 'NONE',  ( -3.458738584817664385, 7.049295759013638474, 0.7216878364870338292 ) ) ;
#67534 = CARTESIAN_POINT ( 'NONE',  ( -0.05793207083453711520, -1.244369569480655136, -1.591280167384064637 ) ) ;
#67535 = ORIENTED_EDGE ( 'NONE', *, *, #99878, .F. ) ;
#67536 = CARTESIAN_POINT ( 'NONE',  ( 3.223938161889360110, -2.224449554215703895, 0.6136290147475926826 ) ) ;
#67537 = CARTESIAN_POINT ( 'NONE',  ( 4.896903505236655185, 0.3334610245491422265, 1.933150054703360432 ) ) ;
#67538 = CARTESIAN_POINT ( 'NONE',  ( 1.217545072937670225, 0.3881152535412414339, -1.922811240370206232 ) ) ;
#67539 = CARTESIAN_POINT ( 'NONE',  ( 2.250290310188348464, 5.569163095287620990, 0.7216878364870438212 ) ) ;
#67540 = CARTESIAN_POINT ( 'NONE',  ( 2.494940289813108780, 4.000000000000003553, -11.73777120880564695 ) ) ;
#67541 = VERTEX_POINT ( 'NONE', #111304 ) ;
#67542 = CARTESIAN_POINT ( 'NONE',  ( 0.5502106600992883179, 1.049441996780882125, 1.838938355043976847 ) ) ;
#67543 = CARTESIAN_POINT ( 'NONE',  ( -5.434120640978981065, 5.234228924097238611, -0.7998128361456221525 ) ) ;
#67544 = CARTESIAN_POINT ( 'NONE',  ( -8.832353407160665526, 3.956598013261175772, -7.432338980325321920 ) ) ;
#67545 = CARTESIAN_POINT ( 'NONE',  ( 3.907220266852969637, -1.778082601562074094, 1.245552836545896769 ) ) ;
#67546 = CARTESIAN_POINT ( 'NONE',  ( -0.4771755680234849861, 3.000978323161636485, 1.942502113148306231 ) ) ;
#67547 = CARTESIAN_POINT ( 'NONE',  ( 2.250376613284802207, 0.9954810856505689198, -1.872389709364124188 ) ) ;
#67548 = CARTESIAN_POINT ( 'NONE',  ( -1.201851678989727383E-14, 3.618750000682816381, -1.732050807568863648 ) ) ;
#67549 = FACE_OUTER_BOUND ( 'NONE', #124933, .T. ) ;
#67550 = LINE ( 'NONE', #117468, #174078 ) ;
#67551 = CARTESIAN_POINT ( 'NONE',  ( 6.564609147483420060, 6.793222102749934876, 0.3624652974001541517 ) ) ;
#67552 = CARTESIAN_POINT ( 'NONE',  ( 1.985689569138231914, 1.418919563317089017, 1.494737215543304965 ) ) ;
#67554 = CARTESIAN_POINT ( 'NONE',  ( 1.361729690220290223, 3.300000000000025135, 0.6158276295007287793 ) ) ;
#67553 = CARTESIAN_POINT ( 'NONE',  ( -8.853638004923878313, 10.28799807962136548, 1.199719254218462483 ) ) ;
#67555 = CARTESIAN_POINT ( 'NONE',  ( -1.364683531249997417, 2.509375000341422357, 1.214306433183764966E-14 ) ) ;
#67556 = CARTESIAN_POINT ( 'NONE',  ( -4.913752204202785023, 4.881785571126718182, -0.5639616748225815268 ) ) ;
#67557 = CARTESIAN_POINT ( 'NONE',  ( 5.769883596960928784, 7.349226441320860559, -1.350955626351646233 ) ) ;
#67558 = ORIENTED_EDGE ( 'NONE', *, *, #117585, .F. ) ;
#67559 = CARTESIAN_POINT ( 'NONE',  ( 4.178302048780179412, 0.9043031410675538284, 1.684961085834511874 ) ) ;
#67560 =( BOUNDED_SURFACE ( )  B_SPLINE_SURFACE ( 3, 3, ( 
 ( #68196, #200333, #53031, #171045, #118109, #88752, #54111, #35713, #167859, #19456, #120246 ),
 ( #58372, #60490, #141797, #95153, #208859, #140728, #29070, #44266, #45332, #127730, #124526 ),
 ( #108257, #177456, #8542, #94095, #175336, #191547, #189433, #206741, #74624, #173208, #90891 ),
 ( #77809, #11733, #190483, #193688, #109328, #76736, #111451, #174278, #93027, #10664, #159068 ),
 ( #41075, #142855, #61564, #126648, #192613, #110388, #176393, #207801, #73545, #26918, #27998 ),
 ( #42142, #143930, #7466, #139648, #43212, #25853, #91963, #156950, #160134, #158022, #9610 ),
 ( #209925, #205669, #75687, #59429, #125587, #57307, #123470, #107182, #24788, #33321, #96222 ) ),
 .UNSPECIFIED., .T., .F., .T. ) 
 B_SPLINE_SURFACE_WITH_KNOTS ( ( 4, 3, 4 ),
 ( 4, 1, 1, 1, 1, 1, 1, 1, 4 ),
 ( 0.000000000000000000, 0.5000000000000000000, 1.000000000000000000 ),
 ( 0.000000000000000000, 0.2256926809922864541, 0.3979886288388991278, 0.5260859906349554249, 0.6192013483571605637, 0.6864504996671639825, 0.7364865548622955282, 0.7772638159577213157, 1.000000000000000000 ),
 .UNSPECIFIED. ) 
 GEOMETRIC_REPRESENTATION_ITEM ( )  RATIONAL_B_SPLINE_SURFACE ( (
 ( 1.000000000000000222, 1.000000000000000222, 0.9999999999999997780, 1.000000000000000222, 0.9999999999999996669, 1.000000000000000000, 1.000000000000000222, 0.9999999999999996669, 1.000000000000000444, 1.000000000000000222, 1.000000000000000222),
 ( 0.3333333333333334259, 0.3333333333333334259, 0.3333333333333333148, 0.3333333333333333703, 0.3333333333333333703, 0.3333333333333332593, 0.3333333333333334814, 0.3333333333333332038, 0.3333333333333335924, 0.3333333333333334259, 0.3333333333333334259),
 ( 0.3333333333333334259, 0.3333333333333334259, 0.3333333333333333148, 0.3333333333333333703, 0.3333333333333333703, 0.3333333333333332593, 0.3333333333333334814, 0.3333333333333332038, 0.3333333333333335924, 0.3333333333333334259, 0.3333333333333334259),
 ( 1.000000000000000222, 1.000000000000000222, 0.9999999999999997780, 1.000000000000000222, 0.9999999999999996669, 1.000000000000000000, 1.000000000000000222, 0.9999999999999996669, 1.000000000000000444, 1.000000000000000222, 1.000000000000000222),
 ( 0.3333333333333334259, 0.3333333333333334259, 0.3333333333333333148, 0.3333333333333333703, 0.3333333333333333703, 0.3333333333333332593, 0.3333333333333334814, 0.3333333333333332038, 0.3333333333333335924, 0.3333333333333334259, 0.3333333333333334259),
 ( 0.3333333333333334259, 0.3333333333333334259, 0.3333333333333333148, 0.3333333333333333703, 0.3333333333333333703, 0.3333333333333332593, 0.3333333333333334814, 0.3333333333333332038, 0.3333333333333335924, 0.3333333333333334259, 0.3333333333333334259),
 ( 1.000000000000000222, 1.000000000000000222, 0.9999999999999997780, 1.000000000000000222, 0.9999999999999996669, 1.000000000000000000, 1.000000000000000222, 0.9999999999999996669, 1.000000000000000444, 1.000000000000000222, 1.000000000000000222) ) ) 
 REPRESENTATION_ITEM ( '' )  SURFACE ( )  );
#67561 = CARTESIAN_POINT ( 'NONE',  ( 11.84101807917483740, 9.989784997391206289, 1.444039656437077657 ) ) ;
#67562 = CARTESIAN_POINT ( 'NONE',  ( 1.950798113461976735, 0.7085273209575352338, 2.148688966898488761 ) ) ;
#67563 = CARTESIAN_POINT ( 'NONE',  ( -4.302014814237876017, 3.913438792899272212, 0.7998128361456341429 ) ) ;
#67564 = CARTESIAN_POINT ( 'NONE',  ( 1.740194394521710430, 1.041001882027743353, -1.482411077883559747 ) ) ;
#67565 = CARTESIAN_POINT ( 'NONE',  ( 2.254979328032254760, 0.08947561643129221809, -1.913730806789506245 ) ) ;
#67566 = CARTESIAN_POINT ( 'NONE',  ( 2.717306809760032138, -1.800131872397674471, -1.022606600864908399 ) ) ;
#67567 = CARTESIAN_POINT ( 'NONE',  ( 1.364683531249988535, 1.426041667008083991, 0.7879004041258500513 ) ) ;
#67568 = CARTESIAN_POINT ( 'NONE',  ( 0.3914019522827461017, 1.459281966464224256, 1.325753552615087871 ) ) ;
#67569 = CARTESIAN_POINT ( 'NONE',  ( 5.988885569479125870, -0.2852814255829403955, -1.905149068243816579 ) ) ;
#67571 = CARTESIAN_POINT ( 'NONE',  ( 6.396603524444617328, 6.809554808131969672, -0.5206029305389828776 ) ) ;
#67570 = CARTESIAN_POINT ( 'NONE',  ( 6.463508838306311510, 0.3818026259072569983, -2.173449913608487716 ) ) ;
#67572 = CARTESIAN_POINT ( 'NONE',  ( -0.6823417656250003738, 2.217708333674753174, -1.181850606188749264 ) ) ;
#67573 = CARTESIAN_POINT ( 'NONE',  ( 4.809062498722087575, -1.658680843151142392, 1.225972815312638353 ) ) ;
#67574 = CARTESIAN_POINT ( 'NONE',  ( -7.061099074618889304, 7.132370430010492868, -0.7998128361456291469 ) ) ;
#67575 = CARTESIAN_POINT ( 'NONE',  ( 7.914208982075123799, 10.25632978388623684, -1.599625672291262513 ) ) ;
#67576 = CARTESIAN_POINT ( 'NONE',  ( 4.192495815123822744, 5.914331089109666983, -1.599625672291255185 ) ) ;
#67578 = CARTESIAN_POINT ( 'NONE',  ( 1.499999999999990896, 4.275000000000021672, 1.214306433183764966E-14 ) ) ;
#67577 = CARTESIAN_POINT ( 'NONE',  ( 4.717860591023939953, -2.065837571889141078, 0.4082076317219375250 ) ) ;
#67579 = CARTESIAN_POINT ( 'NONE',  ( 0.7312207505087648940, -2.044463659613379392, -0.7311735514200778940 ) ) ;
#67580 = CARTESIAN_POINT ( 'NONE',  ( 1.364683531249988535, 2.176041667008087543, 0.7879004041258500513 ) ) ;
#67581 = CARTESIAN_POINT ( 'NONE',  ( 5.378265110509337532, -1.205767192478784500, 1.793856531414832256 ) ) ;
#67582 = CARTESIAN_POINT ( 'NONE',  ( 5.268225494782738494, 2.017278875131154336, -0.1011536798302767465 ) ) ;
#67583 = CARTESIAN_POINT ( 'NONE',  ( -0.7158994178059416846, 2.800000000000024691, 1.161830092591057184 ) ) ;
#67584 = PRODUCT ( 'coil', 'coil', '', ( #117663 ) ) ;
#67587 = CARTESIAN_POINT ( 'NONE',  ( 4.189106276942576201, 7.831115056500907556, 1.040834085586084257E-14 ) ) ;
#67586 = CARTESIAN_POINT ( 'NONE',  ( 1.642778471875001811, -1.742708332855374298, 2.845375778867859751 ) ) ;
#67585 = CARTESIAN_POINT ( 'NONE',  ( 7.364013710877980401, 8.620379413226322285, -1.199719254218452047 ) ) ;
#67588 = CARTESIAN_POINT ( 'NONE',  ( -4.633854640820660009, 8.628190524257904670, -0.7998128361456362523 ) ) ;
#67589 = CARTESIAN_POINT ( 'NONE',  ( 3.643767777461913493, 2.000731686840724333, -0.2516315899964287617 ) ) ;
#67590 = CARTESIAN_POINT ( 'NONE',  ( -8.853638004923878313, 10.28799807962136548, 1.199719254218462483 ) ) ;
#67592 = CARTESIAN_POINT ( 'NONE',  ( -11.00023563321887643, -5.575210796978346650, -0.04341786867403560346 ) ) ;
#67591 = CARTESIAN_POINT ( 'NONE',  ( -9.408995418203979000, 12.00024729270324286, 1.443375672974076540 ) ) ;
#67594 = CARTESIAN_POINT ( 'NONE',  ( 0.6823417656249934904, 8.442708333674733723, 1.181850606188764807 ) ) ;
#67593 = CARTESIAN_POINT ( 'NONE',  ( 5.366167234668930419, 1.061923416652654550, 1.882811416686725359 ) ) ;
#67595 =( LENGTH_UNIT ( ) NAMED_UNIT ( * ) SI_UNIT ( .MILLI., .METRE. ) );
#67597 = CARTESIAN_POINT ( 'NONE',  ( 5.114861317887108072, 0.1511565883688982259, 2.010826320608386730 ) ) ;
#67596 = CARTESIAN_POINT ( 'NONE',  ( -7.985389288324710400, 8.418635045908049008, -0.7216878364870267237 ) ) ;
#67598 = CARTESIAN_POINT ( 'NONE',  ( -1.499999999999997780, 4.900000000000022560, 1.214306433183764966E-14 ) ) ;
#67599 = CARTESIAN_POINT ( 'NONE',  ( 0.7324925891301607983, 0.1221277223508714788, 1.720630200619164496 ) ) ;
#67600 = CARTESIAN_POINT ( 'NONE',  ( 5.910428620914669473, 5.860197910680708944, 0.000000000000000000 ) ) ;
#67602 = CARTESIAN_POINT ( 'NONE',  ( 5.885121196783658526, 9.023669275293071834, 1.199719254218452047 ) ) ;
#67601 = CARTESIAN_POINT ( 'NONE',  ( 7.619319141200063150, 9.912291636198670375, 1.443375672974076540 ) ) ;
#67603 = CARTESIAN_POINT ( 'NONE',  ( -11.33454210411463059, 7.665656903368001096, 3.947969875293493747 ) ) ;
#67604 = CARTESIAN_POINT ( 'NONE',  ( 5.694569522353672753, -0.4537686991618712362, -1.814561337198366875 ) ) ;
#67605 = CARTESIAN_POINT ( 'NONE',  ( 5.994395146102541538, -1.073393154543872852, 1.702996195706570681 ) ) ;
#67606 = CARTESIAN_POINT ( 'NONE',  ( 6.539320575229249144, 0.007148032025052972194, 1.896977914940492393 ) ) ;
#67607 = CARTESIAN_POINT ( 'NONE',  ( 3.999292125906911188, 4.728557570721922509, 1.082531754730560403 ) ) ;
#67608 = CARTESIAN_POINT ( 'NONE',  ( -6.821160681006823268, 9.051383109298335228, 1.443375672974064550 ) ) ;
#67609 = ORIENTED_EDGE ( 'NONE', *, *, #17759, .F. ) ;
#67611 = CARTESIAN_POINT ( 'NONE',  ( 1.845327587665198443, 0.3419125196015109225, -1.987051676161588620 ) ) ;
#67610 = CARTESIAN_POINT ( 'NONE',  ( 1.735180256192244919, 1.979698633766859395, 0.7602586827493148514 ) ) ;
#67612 = CARTESIAN_POINT ( 'NONE',  ( 1.212835290986268300, 1.479965279312319693, -1.044435387019273742 ) ) ;
#67613 = CARTESIAN_POINT ( 'NONE',  ( 8.188198428010544205, 8.517596018959260107, 0.000000000000000000 ) ) ;
#67614 = CARTESIAN_POINT ( 'NONE',  ( 5.928642344448160628, 2.082074431819755045, 0.5810635428650026135 ) ) ;
#67615 = ADVANCED_FACE ( 'NONE', ( #114501 ), #27847, .T. ) ;
#67616 = MECHANICAL_DESIGN_GEOMETRIC_PRESENTATION_REPRESENTATION (  '', ( #195536 ), #81430 ) ;
#67617 = CARTESIAN_POINT ( 'NONE',  ( 7.396136491454752715, 8.587579647240744407, 1.199719254218462483 ) ) ;
#67619 = CARTESIAN_POINT ( 'NONE',  ( -0.03024393743376960902, -0.9005804071154848156, 1.690789300719280908 ) ) ;
#67618 = CARTESIAN_POINT ( 'NONE',  ( -4.120788623549732854, 6.895004929861607401, -1.199719254218452047 ) ) ;
#67620 = CARTESIAN_POINT ( 'NONE',  ( 4.044555541517573793, 7.746237447724527492, 0.4662041258270445132 ) ) ;
#67621 = TOROIDAL_SURFACE ( 'NONE', #95204, 11.92000000000000171, 0.08000000000000000167 ) ;
#67622 = CARTESIAN_POINT ( 'NONE',  ( 5.788968402910805722, 7.776882441527838807, 1.443375672974062551 ) ) ;
#67623 = CARTESIAN_POINT ( 'NONE',  ( 0.6823417656249882723, 0.9885416670080832136, -1.181850606188749264 ) ) ;
#67624 = CARTESIAN_POINT ( 'NONE',  ( 2.562127843302666186, 5.932973550587659517, 0.000000000000000000 ) ) ;
#67625 = CARTESIAN_POINT ( 'NONE',  ( -4.783329267523015460, 4.474972321731942593, -0.7998128361456221525 ) ) ;
#67626 = CARTESIAN_POINT ( 'NONE',  ( 4.346650381253648554, 0.5737703434565506466, 2.084106190491950006 ) ) ;
#67627 = CARTESIAN_POINT ( 'NONE',  ( -5.302647476720585118, 9.200522799567075083, 0.000000000000000000 ) ) ;
#67628 = CARTESIAN_POINT ( 'NONE',  ( 5.397554552016226914, 6.430140077841320689, 1.082531754730549078 ) ) ;
#67629 = CARTESIAN_POINT ( 'NONE',  ( 2.004293344102888508, -0.9022931611136343344, 1.919180038594799687 ) ) ;
#67630 = CARTESIAN_POINT ( 'NONE',  ( 6.545924712158827319, 0.6954503440314525609, -1.688125835592364066 ) ) ;
#67631 = CARTESIAN_POINT ( 'NONE',  ( 3.655507913172794332, 0.4821067936548150135, -1.911365640376050612 ) ) ;
#67632 = ORIENTED_EDGE ( 'NONE', *, *, #207750, .T. ) ;
#67633 = CARTESIAN_POINT ( 'NONE',  ( 9.469892045836667549, -6.532648833121162291, -0.4294077647110499663 ) ) ;
#67634 = CARTESIAN_POINT ( 'NONE',  ( 6.303175665915636827, -1.664687476133955846, 1.052260723566181833 ) ) ;
#67635 = CARTESIAN_POINT ( 'NONE',  ( 1.552571996792909248, -1.665377644223103637, -0.9986158231547156428 ) ) ;
#67636 = ORIENTED_EDGE ( 'NONE', *, *, #48644, .T. ) ;
#67637 = CARTESIAN_POINT ( 'NONE',  ( -3.149236820124241110, 6.896136400112061970, -0.7998128361456481317 ) ) ;
#67639 = CARTESIAN_POINT ( 'NONE',  ( 1.859876166164115219, 2.485118833786766679, -2.480102205501340418 ) ) ;
#67638 = CARTESIAN_POINT ( 'NONE',  ( -6.943184063974178422, 8.233374508458908281, -1.082531754730549967 ) ) ;
#67640 = CARTESIAN_POINT ( 'NONE',  ( 7.253775878511261155, 8.421492265473332850, 1.199719254218462483 ) ) ;
#67642 = CARTESIAN_POINT ( 'NONE',  ( 4.489158259456265121, 7.291082831790689056, -1.082531754730548412 ) ) ;
#67641 = CARTESIAN_POINT ( 'NONE',  ( 5.621827251160867789, 9.710548892996357040, 1.040834085586084257E-14 ) ) ;
#67644 = ORIENTED_EDGE ( 'NONE', *, *, #144618, .F. ) ;
#67643 = CARTESIAN_POINT ( 'NONE',  ( 6.375647946566726176, 0.3219878414668366773, -1.884816399834337908 ) ) ;
#67645 = CARTESIAN_POINT ( 'NONE',  ( 2.737190076726934151, 0.2709513247245790013, 2.190122135706531914 ) ) ;
#67646 = CARTESIAN_POINT ( 'NONE',  ( 2.081372155488591780, -0.1082299263688718260, -2.204229314041641352 ) ) ;
#67647 = DIRECTION ( 'NONE',  ( 0.000000000000000000, 1.000000000000000000, 0.000000000000000000 ) ) ;
#67648 = CARTESIAN_POINT ( 'NONE',  ( 0.2758376730330712734, 1.891454726169951250, -0.2806862973558504892 ) ) ;
#67649 = CARTESIAN_POINT ( 'NONE',  ( -0.4370080631058587683, -8.003595416197006429, 10.68747925529770804 ) ) ;
#67650 = CARTESIAN_POINT ( 'NONE',  ( 7.055228938194279209, -8.176568542494891290, -6.396834479292358822 ) ) ;
#67651 = CARTESIAN_POINT ( 'NONE',  ( 3.367693471486675083, -0.4065805204805824635, 2.029877954327436118 ) ) ;
#67652 = CARTESIAN_POINT ( 'NONE',  ( -6.098470168048611306, 6.009303372345148553, 1.040834085586084257E-14 ) ) ;
#67653 = CARTESIAN_POINT ( 'NONE',  ( -5.303700083894403505, 7.646886670761364968, 1.227282432737321294 ) ) ;
#67655 = CARTESIAN_POINT ( 'NONE',  ( 1.428841412761387986, 2.083414371474631377, 0.5762002773818803991 ) ) ;
#67654 = CARTESIAN_POINT ( 'NONE',  ( -5.101945877444165944, 4.846691699973280976, 0.000000000000000000 ) ) ;
#67656 = CARTESIAN_POINT ( 'NONE',  ( 3.984055765753656164, -2.167877601896048390, -0.3204034371554059235 ) ) ;
#67657 = DIRECTION ( 'NONE',  ( -0.9999980456341538426, 0.000000000000000000, -0.001977050295949953074 ) ) ;
#67658 = CARTESIAN_POINT ( 'NONE',  ( 5.099275172515607579, 5.121778254122544283, -0.7216878364870458196 ) ) ;
#67659 = CARTESIAN_POINT ( 'NONE',  ( -1.500000000000031530, 4.702083334016148974, 0.8660254037844287156 ) ) ;
#67660 = CARTESIAN_POINT ( 'NONE',  ( -0.6823417656250003738, 14.46354166700806410, 1.181850606188754593 ) ) ;
#67661 = CARTESIAN_POINT ( 'NONE',  ( -4.620296487206990932, 8.612372678375294299, 0.000000000000000000 ) ) ;
#67662 = UNCERTAINTY_MEASURE_WITH_UNIT (LENGTH_MEASURE( 1.000000000000000082E-05 ), #86424, 'distance_accuracy_value', 'NONE');
#67663 = CARTESIAN_POINT ( 'NONE',  ( 5.977189187444425400, -1.726741413813812631, -0.1601111783383553921 ) ) ;
#67664 = CARTESIAN_POINT ( 'NONE',  ( -3.735435015764967837, 4.316761258935923884, -1.199719254218452047 ) ) ;
#67665 = CARTESIAN_POINT ( 'NONE',  ( 4.100488025649267954, 2.059819936833905185, 0.2079151390043249559 ) ) ;
#67666 = CARTESIAN_POINT ( 'NONE',  ( 4.605136521778616654, -0.1025035295275648906, 2.114849348554531883 ) ) ;
#67667 = CARTESIAN_POINT ( 'NONE',  ( 4.774442650306744085, 8.721933525333202653, -0.7998128361456281477 ) ) ;
#67668 = CARTESIAN_POINT ( 'NONE',  ( -1.364683531249997417, 4.259375000341424133, 1.214306433183764966E-14 ) ) ;
#67669 = CARTESIAN_POINT ( 'NONE',  ( 2.729305274051788022, 0.1014009245450513547, -1.966985261555218800 ) ) ;
#67670 = CARTESIAN_POINT ( 'NONE',  ( 0.9141475326900462273, -1.912571728325639153, 0.002704284578637640348 ) ) ;
#67671 = CARTESIAN_POINT ( 'NONE',  ( 5.103627735775233987, -2.281604237428825233, 0.2209099425345140144 ) ) ;
#67672 = CARTESIAN_POINT ( 'NONE',  ( 3.123480263227970344, -1.759325740769552393, 0.4874977319994436287 ) ) ;
#67673 = AXIS2_PLACEMENT_3D ( 'NONE', #169245, #106436, #40331 ) ;
#67674 = CARTESIAN_POINT ( 'NONE',  ( 3.379725431556547477, 7.165039780116438273, -1.734723475976807094E-15 ) ) ;
#67675 = CARTESIAN_POINT ( 'NONE',  ( 5.463572716182834910, 5.476515711742504067, 0.7216878364870317197 ) ) ;
#67676 = CARTESIAN_POINT ( 'NONE',  ( -7.531718027591449705, 8.745758106066849891, 1.199719254218462483 ) ) ;
#67677 = ORIENTED_EDGE ( 'NONE', *, *, #157331, .T. ) ;
#67678 = VERTEX_POINT ( 'NONE', #80868 ) ;
#67679 = CARTESIAN_POINT ( 'NONE',  ( 3.533450910810581824, -0.1440131911168585910, 2.008084626805274997 ) ) ;
#67680 = CARTESIAN_POINT ( 'NONE',  ( 4.188298518248589453, 1.053080760608171129, -1.654974388233184657 ) ) ;
#67681 = CARTESIAN_POINT ( 'NONE',  ( -5.831978632172702071, 9.955725504176825780, 0.7998128361456481317 ) ) ;
#67682 = CARTESIAN_POINT ( 'NONE',  ( -5.575427483717760424, 7.527751369135936343, 1.599625672291269396 ) ) ;
#67683 = CARTESIAN_POINT ( 'NONE',  ( 0.07536363704233049743, 2.002983476668462881, -2.558365315478607904 ) ) ;
#67685 = CARTESIAN_POINT ( 'NONE',  ( 5.225387627957367442, -1.679756879107903833, 0.5577133518330120721 ) ) ;
#67684 = CARTESIAN_POINT ( 'NONE',  ( 0.8375780558756993344, 0.8438101838260108067, -1.913087135030653974 ) ) ;
#67686 = CARTESIAN_POINT ( 'NONE',  ( 3.004449694157372175, 6.376150746295683014, 0.4906582928672916788 ) ) ;
#67687 = CARTESIAN_POINT ( 'NONE',  ( 1.763894328224338448, 1.128481436294457740, 1.878420861880884862 ) ) ;
#67688 = CARTESIAN_POINT ( 'NONE',  ( 6.474529609311859168, -0.09325562727019585940, -1.737965710822095389 ) ) ;
#67689 = CARTESIAN_POINT ( 'NONE',  ( 8.274553823041976841, 8.548067636504127265, 1.040834085586084257E-14 ) ) ;
#67690 = CARTESIAN_POINT ( 'NONE',  ( 0.2331713839410628208, 0.2432647426263275514, -1.987790486660771627 ) ) ;
#67691 = CARTESIAN_POINT ( 'NONE',  ( 0.1347971297303695026, -1.579520332396977089, 0.6935263066737175075 ) ) ;
#67692 = CARTESIAN_POINT ( 'NONE',  ( 1.212782571277282395, -1.812964642495185963, -1.412582873482233659 ) ) ;
#67693 = CARTESIAN_POINT ( 'NONE',  ( 1.066276686178056377, -1.386418637449363889, 1.697306931840412370 ) ) ;
#67694 = CARTESIAN_POINT ( 'NONE',  ( 2.649284799151204073, -1.834272514977531632, 1.226802785254533568 ) ) ;
#67695 = CARTESIAN_POINT ( 'NONE',  ( 0.2335667940002684184, 0.001055507091213009818, -2.153566573614831281 ) ) ;
#67696 = CARTESIAN_POINT ( 'NONE',  ( -1.854512760316423536, 0.000000000000000000, 2.484105960264900936 ) ) ;
#67697 = CARTESIAN_POINT ( 'NONE',  ( 1.745463160119866686, 0.3564436455325488695, -2.086969855494016368 ) ) ;
#67698 = CARTESIAN_POINT ( 'NONE',  ( 6.827182134110238110, 0.5514785450725538940, 2.340047124761033714 ) ) ;
#67699 = CARTESIAN_POINT ( 'NONE',  ( 5.139640169905585587, -1.362188071541370116, -1.362388069303143823 ) ) ;
#67700 = ORIENTED_EDGE ( 'NONE', *, *, #55489, .F. ) ;
#67702 = CARTESIAN_POINT ( 'NONE',  ( -0.7499999999999972244, 5.608333333333353821, -1.299038105676652011 ) ) ;
#67701 = CARTESIAN_POINT ( 'NONE',  ( 2.648291651658631007, 0.7751803744074429181, 2.157441745960963164 ) ) ;
#67703 = CARTESIAN_POINT ( 'NONE',  ( 4.359110081993588182, 5.044382169536003602, -1.199719254218452047 ) ) ;
#67704 = CARTESIAN_POINT ( 'NONE',  ( 6.440286661691305703, 7.472421512516709718, 1.199719254218462483 ) ) ;
#67705 = CARTESIAN_POINT ( 'NONE',  ( 4.407017973072342443, -0.4864924038828158381, -2.167217472756521879 ) ) ;
#67706 = CARTESIAN_POINT ( 'NONE',  ( -6.995644074971465010, 10.14503993989993091, 1.082531754730549967 ) ) ;
#67707 = CARTESIAN_POINT ( 'NONE',  ( -1.164422670175135899, 3.300000000000025135, -0.7116747751938151678 ) ) ;
#67708 = CARTESIAN_POINT ( 'NONE',  ( 6.155038550924150087, 7.243595066575396757, 1.082531754730558626 ) ) ;
#67709 = CARTESIAN_POINT ( 'NONE',  ( -7.117667457050096402, 10.28740055232499984, 1.082531754730549967 ) ) ;
#67710 = CARTESIAN_POINT ( 'NONE',  ( 6.387299765813869712, 6.624473612970537495, 0.000000000000000000 ) ) ;
#67711 = ORIENTED_EDGE ( 'NONE', *, *, #42400, .T. ) ;
#67712 = CARTESIAN_POINT ( 'NONE',  ( 2.813125141109920069, 1.117832431973438734, -1.678005364621336426 ) ) ;
#67714 = CARTESIAN_POINT ( 'NONE',  ( 0.5321751443473606846, 1.184493745614173310, 1.688377367428809173 ) ) ;
#67713 = CARTESIAN_POINT ( 'NONE',  ( 6.856673000209174695, 9.022537805042615489, 1.599625672291281386 ) ) ;
#67715 = CARTESIAN_POINT ( 'NONE',  ( 6.983263157960402090, -0.0002233252893329333382, 1.845923184817334084 ) ) ;
#67716 = CARTESIAN_POINT ( 'NONE',  ( 6.346625304528514810, 6.577020074804287297, 0.000000000000000000 ) ) ;
#67717 = CARTESIAN_POINT ( 'NONE',  ( -2.306848205364723903, 5.479977701987478689, -0.7739106563221284096 ) ) ;
#67718 = CARTESIAN_POINT ( 'NONE',  ( 1.364683531249990311, 3.884375000341417028, 1.214306433183764966E-14 ) ) ;
#67719 = CARTESIAN_POINT ( 'NONE',  ( 4.365290731249091394, 2.125951747006165959, -0.5312598475561494116 ) ) ;
#67720 = CARTESIAN_POINT ( 'NONE',  ( 1.793592486599729252, 1.492254607734722072, -1.356300734917381678 ) ) ;
#67721 = CARTESIAN_POINT ( 'NONE',  ( 1.487592393518050837, -1.832424703912252317, -0.1798031890194173865 ) ) ;
#67722 = CARTESIAN_POINT ( 'NONE',  ( 4.810265146351084375, 1.581823803905563430, -1.659390399702101337 ) ) ;
#67723 = CARTESIAN_POINT ( 'NONE',  ( 5.050657991863417351, -1.557144343216086968, -0.9820927893566462341 ) ) ;
#67724 = CARTESIAN_POINT ( 'NONE',  ( 8.072990401933337168, 11.50590700464255356, -1.199719254218446718 ) ) ;
#67725 = CARTESIAN_POINT ( 'NONE',  ( 4.348545414961950684, 0.4871326187540457875, 1.759326811173238303 ) ) ;
#67726 = CARTESIAN_POINT ( 'NONE',  ( 4.395157833011634096, -0.8647231026696032830, -1.821742675176166060 ) ) ;
#67727 = CARTESIAN_POINT ( 'NONE',  ( -8.690940161559884913, 10.09818392903003748, 1.199719254218462483 ) ) ;
#67729 = DIRECTION ( 'NONE',  ( 5.578564026256490882E-16, 1.000000000000000000, 9.066213480720158442E-32 ) ) ;
#67728 = CARTESIAN_POINT ( 'NONE',  ( 4.329186484417943959, 0.1072846252610352574, 2.260086081085868948 ) ) ;
#67730 = CARTESIAN_POINT ( 'NONE',  ( 0.1531350777018150311, -1.689991139269167109, 1.256553844878212978 ) ) ;
#67731 =( BOUNDED_CURVE ( )  B_SPLINE_CURVE ( 1, ( #295, #1369 ),
 .UNSPECIFIED., .F., .T. ) 
 B_SPLINE_CURVE_WITH_KNOTS ( ( 2, 2 ),
 ( 0.000000000000000000, 6.249999999999918815E-05 ),
 .UNSPECIFIED. ) 
 CURVE ( )  GEOMETRIC_REPRESENTATION_ITEM ( )  RATIONAL_B_SPLINE_CURVE ( ( 0.9345202395942815432, 0.9345202395942815432 ) ) 
 REPRESENTATION_ITEM ( '' )  );
#67732 = CARTESIAN_POINT ( 'NONE',  ( 4.457524453155742528, 1.660904245173303373, 1.235824716467534889 ) ) ;
#67733 = CARTESIAN_POINT ( 'NONE',  ( 9.240045382913317340, 10.73880668727576015, -1.199719254218446718 ) ) ;
#67734 = CARTESIAN_POINT ( 'NONE',  ( 0.6801582343749987825, 2.338541667008108060, -1.178068619123883165 ) ) ;
#67735 = PRODUCT_CONTEXT ( 'NONE', #181919, 'mechanical' ) ;
#67738 = EDGE_CURVE ( 'NONE', #210434, #179460, #192715, .T. ) ;
#67737 = CARTESIAN_POINT ( 'NONE',  ( 2.297378195909089982, 1.489297080225897574, 1.222053532002062903 ) ) ;
#67736 = CARTESIAN_POINT ( 'NONE',  ( -6.991200766141138168, 11.30815132714001159, 0.7998128361456481317 ) ) ;
#67739 = CARTESIAN_POINT ( 'NONE',  ( 4.041739190205284160, 7.729463131965888856, 0.000000000000000000 ) ) ;
#67740 = CARTESIAN_POINT ( 'NONE',  ( 6.368014371105396698, -1.954979222910321557, 0.2374047605521299453 ) ) ;
#67741 = CARTESIAN_POINT ( 'NONE',  ( 3.892599500454941630, 6.595097612955829192, 1.082531754730549078 ) ) ;
#67742 = CARTESIAN_POINT ( 'NONE',  ( 5.782412516234797017, 6.044064802175099338, 0.5499171889626064402 ) ) ;
#67743 = CARTESIAN_POINT ( 'NONE',  ( -2.740719608256871442, 6.349256642941639051, 0.7998128361456341429 ) ) ;
#67745 = CARTESIAN_POINT ( 'NONE',  ( 2.074768627854159053, 0.9548037322763336388, 2.005906060693471993 ) ) ;
#67744 = CARTESIAN_POINT ( 'NONE',  ( 0.8441712343106638761, -1.349783269286155774, -1.635521010841307410 ) ) ;
#67746 = CARTESIAN_POINT ( 'NONE',  ( 3.171027762369707848, -1.945216043820027663, -0.8074606443248407706 ) ) ;
#67747 = CARTESIAN_POINT ( 'NONE',  ( -6.882699257592852504, 8.058845884393651460, -1.199719254218452047 ) ) ;
#67748 = CARTESIAN_POINT ( 'NONE',  ( 7.772902139336337335, 7.962807338847539107, 0.7998128361456341429 ) ) ;
#67749 = CARTESIAN_POINT ( 'NONE',  ( 6.983263157960402090, -0.0002233252893329463486, 1.845923184817334084 ) ) ;
#67750 = CARTESIAN_POINT ( 'NONE',  ( 6.124532705071213279, 8.168374127381657246, -1.599625672291262513 ) ) ;
#67751 = CARTESIAN_POINT ( 'NONE',  ( -4.183908731771626144, 7.398323783528643283, -0.7858605482065593728 ) ) ;
#67752 = CARTESIAN_POINT ( 'NONE',  ( 4.741601036477289810, 6.554953847355395880, 1.599625672291267398 ) ) ;
#67753 = CARTESIAN_POINT ( 'NONE',  ( -4.475600106286965918, 8.235634200727838916, 0.7216878364870338292 ) ) ;
#67754 = CARTESIAN_POINT ( 'NONE',  ( -6.724481002698115439, 10.78905223654906109, -0.7216878364870267237 ) ) ;
#67755 = CARTESIAN_POINT ( 'NONE',  ( 1.266058358664986949, 0.6103625328083387425, -2.030891291126469600 ) ) ;
#67756 = CARTESIAN_POINT ( 'NONE',  ( -6.622231685632140596, 6.690634819517756959, 0.000000000000000000 ) ) ;
#67758 = CARTESIAN_POINT ( 'NONE',  ( 4.387127823891323608, 0.09410986116351567621, 1.959716250186482434 ) ) ;
#67757 = CARTESIAN_POINT ( 'NONE',  ( -0.6125000000000105915, 0.5416666666666625218, 1.060881119635880721 ) ) ;
#67759 = CARTESIAN_POINT ( 'NONE',  ( 3.133815226704575796, -1.450665623810345473, -1.602838778681405785 ) ) ;
#67760 = CARTESIAN_POINT ( 'NONE',  ( 1.346931166825489967, 0.5339940059071214273, -1.762130705996706181 ) ) ;
#67761 = CARTESIAN_POINT ( 'NONE',  ( -4.037710856648669022, 7.592775851288043221, -0.3149755216912339395 ) ) ;
#67762 = FACE_BOUND ( 'NONE', #64626, .T. ) ;
#67763 = CARTESIAN_POINT ( 'NONE',  ( 4.365022556061240344, 1.687170946148343953, -0.4262992432423305389 ) ) ;
#67764 = CARTESIAN_POINT ( 'NONE',  ( 0.6674790882332717334, 15.00000000000000888, -11.66566053519550827 ) ) ;
#67765 = CARTESIAN_POINT ( 'NONE',  ( 6.643132081016125845, 6.852668304048034287, 0.7216878364870317197 ) ) ;
#67766 = CARTESIAN_POINT ( 'NONE',  ( -10.60630588279735242, 5.715763139788331948, 4.896273837757428637 ) ) ;
#67767 = CARTESIAN_POINT ( 'NONE',  ( 1.446389902895691693, 2.159248346720197276, 0.1057134262518744372 ) ) ;
#67768 = VECTOR ( 'NONE', #117458, 1000.000000000000000 ) ;
#67769 = CARTESIAN_POINT ( 'NONE',  ( 3.233749808020690342, -1.861731463674856979, -0.7741979076196570109 ) ) ;
#67770 = CARTESIAN_POINT ( 'NONE',  ( -8.473482818416657736, 12.82955435488738516, -0.7216878364870267237 ) ) ;
#67771 = CARTESIAN_POINT ( 'NONE',  ( 1.253037233087474611, -1.703760181015579134, 1.330383891403746688 ) ) ;
#67772 = ADVANCED_FACE ( 'NONE', ( #45189 ), #91135, .T. ) ;
#67773 = CARTESIAN_POINT ( 'NONE',  ( 3.432457938460992342, 1.923125764579440844, 0.4332125842720236375 ) ) ;
#67774 = CIRCLE ( 'NONE', #178387, 0.5000000000000004441 ) ;
#67775 = CARTESIAN_POINT ( 'NONE',  ( 6.609000000000015085, -6.653734696158637751E-05, 2.100160721423645960 ) ) ;
#67776 = CARTESIAN_POINT ( 'NONE',  ( 3.034642427012054444, -1.711418951474739991, 0.9179939537737377142 ) ) ;
#67779 = ORIENTED_EDGE ( 'NONE', *, *, #193855, .F. ) ;
#67778 = CARTESIAN_POINT ( 'NONE',  ( -3.851925040058337579, 6.547644075826416277, -1.082531754730546636 ) ) ;
#67777 = CARTESIAN_POINT ( 'NONE',  ( -8.744645890690007306, 12.18554205823825498, 1.082531754730558626 ) ) ;
#67780 = CARTESIAN_POINT ( 'NONE',  ( -4.950135482320929370, 5.908151163196758482, -1.082531754730549967 ) ) ;
#67781 = CARTESIAN_POINT ( 'NONE',  ( 2.925527285498711549, 6.635141943048991742, 0.7998128361456281477 ) ) ;
#67782 = CARTESIAN_POINT ( 'NONE',  ( -5.330290668828105538, 6.247702530834755130, 1.199719254218452935 ) ) ;
#67783 = CARTESIAN_POINT ( 'NONE',  ( -4.959250327548641479, 9.007818825440551791, -0.7998128361456362523 ) ) ;
#67784 = CARTESIAN_POINT ( 'NONE',  ( -9.802181872555943087, 10.53822639417784046, 0.7216878364870438212 ) ) ;
#67785 = CARTESIAN_POINT ( 'NONE',  ( 6.282281253371452934, -1.241832687457484985, 1.944794379655417682 ) ) ;
#67786 = CARTESIAN_POINT ( 'NONE',  ( -3.285556943749998737, -3.580208332855374653, 1.896917185911908499 ) ) ;
#67787 = CARTESIAN_POINT ( 'NONE',  ( 5.242999579849755953, -0.2363135928187160284, -1.947375393322479109 ) ) ;
#67788 = CARTESIAN_POINT ( 'NONE',  ( 1.846327496167538884, 0.3419342931599393398, -1.987046799686801757 ) ) ;
#67789 = ORIENTED_EDGE ( 'NONE', *, *, #79325, .F. ) ;
#67790 = CARTESIAN_POINT ( 'NONE',  ( 2.940728227222836111, -1.600293368184166898, 1.386485470145684351 ) ) ;
#67791 = CARTESIAN_POINT ( 'NONE',  ( -1.201851678989727383E-14, 3.118750000682814161, -1.732050807568863648 ) ) ;
#67793 = CARTESIAN_POINT ( 'NONE',  ( -4.869349725602420520, 8.832658446511480577, 1.040834085586084257E-14 ) ) ;
#67792 = CARTESIAN_POINT ( 'NONE',  ( 0.1747926744264920174, 4.095712681614646300, -2.410328719303979739 ) ) ;
#67794 = CARTESIAN_POINT ( 'NONE',  ( 4.734224819668921391, 0.3176365174208677367, 1.813369535050498360 ) ) ;
#67795 = ORIENTED_EDGE ( 'NONE', *, *, #212859, .F. ) ;
#67796 = UNCERTAINTY_MEASURE_WITH_UNIT (LENGTH_MEASURE( 1.000000000000000082E-05 ), #49934, 'distance_accuracy_value', 'NONE');
#67797 = CARTESIAN_POINT ( 'NONE',  ( -8.646349277213090545, 11.11049346154719508, 1.599625672291269396 ) ) ;
#67798 = DIRECTION ( 'NONE',  ( 1.561251128379126077E-17, 1.301042606982605475E-17, 1.000000000000000000 ) ) ;
#67799 = CARTESIAN_POINT ( 'NONE',  ( 5.361630242575341931, -1.673063676233761621, -1.302930760576012092 ) ) ;
#67800 = DIRECTION ( 'NONE',  ( 0.000000000000000000, 0.000000000000000000, -1.000000000000000000 ) ) ;
#67801 = CARTESIAN_POINT ( 'NONE',  ( 8.098297826064319693, 8.342435640030188893, 0.7998128361456481317 ) ) ;
#67802 = CARTESIAN_POINT ( 'NONE',  ( 5.149710871190182893, 0.6505453885284390170, -1.955453191944044766 ) ) ;
#67805 = CARTESIAN_POINT ( 'NONE',  ( 2.225889136967126536, 1.786374552192676823, 0.4457033907802817052 ) ) ;
#67804 = CARTESIAN_POINT ( 'NONE',  ( 0.9943274703284404881, 1.832596168249778446, 0.3232805840463324198 ) ) ;
#67803 = CARTESIAN_POINT ( 'NONE',  ( -4.282998556134152146, 3.891253158444922811, -0.3219805702579207063 ) ) ;
#67806 = CARTESIAN_POINT ( 'NONE',  ( 7.560643217915098191, 11.97250085420964716, -0.7998128361456291469 ) ) ;
#67807 = FACE_OUTER_BOUND ( 'NONE', #214140, .T. ) ;
#67808 = CARTESIAN_POINT ( 'NONE',  ( -9.469892045836674654, -6.532648833121171172, 0.4294077647110563500 ) ) ;
#67809 = CARTESIAN_POINT ( 'NONE',  ( 7.777967379493318845, -6.134628647623485698, 7.664830294503448549 ) ) ;
#67810 = AXIS2_PLACEMENT_3D ( 'NONE', #28240, #166770, #51958 ) ;
#67811 = CARTESIAN_POINT ( 'NONE',  ( 2.280145854635793334, 1.358931147977986420, 1.738775483816151768 ) ) ;
#67812 = CARTESIAN_POINT ( 'NONE',  ( 4.622535034725678393, 1.396675434457357756, -1.779734664907887343 ) ) ;
#67813 = CARTESIAN_POINT ( 'NONE',  ( -6.968527767744110868, 9.153035033833367251, 1.443375672974078761 ) ) ;
#67814 = CARTESIAN_POINT ( 'NONE',  ( 5.273626195773981173, 0.3454419319289269708, -1.778163250140889717 ) ) ;
#67815 = CARTESIAN_POINT ( 'NONE',  ( 4.909359874374886523, -1.816983420234472790, 0.6072180050544163654 ) ) ;
#67816 = CARTESIAN_POINT ( 'NONE',  ( -0.6823417656250212460, 5.363541667008087543, 1.181850606188767472 ) ) ;
#67817 = MECHANICAL_DESIGN_GEOMETRIC_PRESENTATION_REPRESENTATION (  '', ( #199581 ), #137138 ) ;
#67818 = CARTESIAN_POINT ( 'NONE',  ( 3.660970522598467891, -1.737989841360635834, -0.9306492429120606369 ) ) ;
#67819 = CARTESIAN_POINT ( 'NONE',  ( 5.242975984329111050, -1.603930480038592510, 0.9624218375651683033 ) ) ;
#67820 = CARTESIAN_POINT ( 'NONE',  ( 4.316758383393053400, -1.379848157930125829, 1.249026149535825914 ) ) ;
#67821 = CARTESIAN_POINT ( 'NONE',  ( 1.836970198721030181E-16, 0.000000000000000000, 1.500000000000000222 ) ) ;
#67822 = CARTESIAN_POINT ( 'NONE',  ( 4.803428869931958722, -0.4704684023625771983, 1.706073424435787134 ) ) ;
#67823 = CARTESIAN_POINT ( 'NONE',  ( -0.01248194115436446205, -0.5331630387654020531, 1.944732228473695868 ) ) ;
#67825 = CARTESIAN_POINT ( 'NONE',  ( 1.946058636591390334, 0.8049280153260234272, -1.946384432229040673 ) ) ;
#67824 = CARTESIAN_POINT ( 'NONE',  ( -2.426546306721660606, 5.774795091243142053, 0.7216878364870317197 ) ) ;
#67826 = CARTESIAN_POINT ( 'NONE',  ( 8.401248741962376698, 12.95320729893149370, 0.7998128361456462443 ) ) ;
#67828 = CARTESIAN_POINT ( 'NONE',  ( -9.130526383799315582, 12.73969898348616070, 1.199719254218462483 ) ) ;
#67827 = CARTESIAN_POINT ( 'NONE',  ( 0.7500000000000006661, 11.94791666734946389, -1.299038105676657340 ) ) ;
#67829 = CARTESIAN_POINT ( 'NONE',  ( 3.146849984228027974, 2.069795010335002239, 0.4607391970517027979 ) ) ;
#67830 = DIRECTION ( 'NONE',  ( -0.3085202182251676195, 0.000000000000000000, 0.9512177852344304574 ) ) ;
#67831 = CARTESIAN_POINT ( 'NONE',  ( 1.476825778181306559, -1.425320297365587408, 1.431352559222300203 ) ) ;
#67832 = CARTESIAN_POINT ( 'NONE',  ( 1.364683531249986537, 2.655208333674754062, -0.7879004041258239610 ) ) ;
#67833 = CIRCLE ( 'NONE', #12508, 4.000000000000000000 ) ;
#67834 = CARTESIAN_POINT ( 'NONE',  ( 6.620655732516623537, 7.629137130509068498, 2.426260288887295058 ) ) ;
#67835 = CARTESIAN_POINT ( 'NONE',  ( 4.497554271431305040, 6.270232621468402989, -1.599625672291256295 ) ) ;
#67836 = ORIENTED_EDGE ( 'NONE', *, *, #101693, .F. ) ;
#67837 = CARTESIAN_POINT ( 'NONE',  ( 1.757319832705085627, -1.853012815387704570, -1.112828241397870066 ) ) ;
#67838 = CARTESIAN_POINT ( 'NONE',  ( 6.610000000000010090, 0.5825982378308904863, 2.053072689460200273 ) ) ;
#67841 = CARTESIAN_POINT ( 'NONE',  ( 6.189608320745400682, 5.317548586107500697, -2.438128985384273140 ) ) ;
#67840 = CARTESIAN_POINT ( 'NONE',  ( 11.94650005372638013, 9.948972996623616893, -1.135399707157281890 ) ) ;
#67839 = CARTESIAN_POINT ( 'NONE',  ( 3.923105346307896202, 5.670318552149568703, -1.599625672291269396 ) ) ;
#67842 = CARTESIAN_POINT ( 'NONE',  ( 8.703971429848968100, 13.09845773489176679, 0.000000000000000000 ) ) ;
#67843 = CARTESIAN_POINT ( 'NONE',  ( -1.499999999999997780, 3.931250000682819046, 1.214306433183764966E-14 ) ) ;
#67844 = CARTESIAN_POINT ( 'NONE',  ( -7.293923454472094114, 9.532663335016016148, 1.443375672974090751 ) ) ;
#67845 = CARTESIAN_POINT ( 'NONE',  ( 0.5565083568685527116, -1.583368386835169783, 1.515454571103365344 ) ) ;
#67846 = CARTESIAN_POINT ( 'NONE',  ( -1.138412281109779656E-15, -7.868711954895459826, -9.183873791909949347 ) ) ;
#67848 = CARTESIAN_POINT ( 'NONE',  ( -0.6823417656250039265, 11.81770833367473017, -1.181850606188755259 ) ) ;
#67847 = CARTESIAN_POINT ( 'NONE',  ( 1.446537619816448572, 2.259995149683653448, 0.1094724083178944679 ) ) ;
#67849 = CARTESIAN_POINT ( 'NONE',  ( -7.862839020921525091, 11.26073039346208660, -1.199719254218446718 ) ) ;
#67850 = CARTESIAN_POINT ( 'NONE',  ( -5.572037945092175981, 5.603058478803387032, 0.7216878364870317197 ) ) ;
#67851 = CARTESIAN_POINT ( 'NONE',  ( 0.6823417656249899377, 2.405208333674753618, 1.181850606188767472 ) ) ;
#67852 = CARTESIAN_POINT ( 'NONE',  ( 4.664027441776592120, 8.287593892024585074, -0.5126927951675692707 ) ) ;
#67853 = CARTESIAN_POINT ( 'NONE',  ( 0.7500000000000006661, 10.41666666666667140, -1.299038105676657340 ) ) ;
#67854 = CARTESIAN_POINT ( 'NONE',  ( 4.529763579968347997, -1.064299448457445729, -1.357287084437068803 ) ) ;
#67855 = CARTESIAN_POINT ( 'NONE',  ( 5.252858170651868441, 5.093032385374103299, -0.7998128361456481317 ) ) ;
#67856 = CARTESIAN_POINT ( 'NONE',  ( 3.743183411477500222, -1.338374212114415762, -1.157953421578450381 ) ) ;
#67857 = CARTESIAN_POINT ( 'NONE',  ( 5.702238492974306183, -2.206952906645575307, -0.005361432510411765114 ) ) ;
#67858 = EDGE_LOOP ( 'NONE', ( #47193, #124650, #40021, #45385 ) ) ;
#67859 = CARTESIAN_POINT ( 'NONE',  ( -5.960744811863571968, 6.983232364376142698, 1.199719254218452935 ) ) ;
#67860 = CARTESIAN_POINT ( 'NONE',  ( 5.150017624212761547, 0.9963180513538304472, 1.753022482293864481 ) ) ;
#67861 = ORIENTED_EDGE ( 'NONE', *, *, #59598, .F. ) ;
#67862 = EDGE_CURVE ( 'NONE', #15203, #125480, #14330, .T. ) ;
#67863 = CARTESIAN_POINT ( 'NONE',  ( 3.098369316282158614, -0.5415621961667067552, -1.790553177708480215 ) ) ;
#67864 = CARTESIAN_POINT ( 'NONE',  ( 2.043885321627556095, 1.424625833772466432, 1.502381739045772546 ) ) ;
#67865 = CARTESIAN_POINT ( 'NONE',  ( -6.075462232255183892, 10.10214001435745246, 0.000000000000000000 ) ) ;
#67866 = CARTESIAN_POINT ( 'NONE',  ( 2.355592738034977263, -1.419685808644566949, -1.281520755053264571 ) ) ;
#67867 = CARTESIAN_POINT ( 'NONE',  ( -0.4000000000000183964, 3.222996591249000176, 0.4134307888557075539 ) ) ;
#67868 = CARTESIAN_POINT ( 'NONE',  ( -10.87107728089202752, 4.495199002972934288, -4.557510466808897043 ) ) ;
#67869 = CARTESIAN_POINT ( 'NONE',  ( 5.872089928050245433, 6.023395468912886130, -0.7216878364870151774 ) ) ;
#67870 = CARTESIAN_POINT ( 'NONE',  ( 0.6823417656249917140, 4.405208333674755394, 1.181850606188765695 ) ) ;
#67871 = CARTESIAN_POINT ( 'NONE',  ( 0.1582721923853447621, 1.907395734848855051, 0.1385995803297388196 ) ) ;
#67872 = EDGE_CURVE ( 'NONE', #6267, #184258, #178380, .T. ) ;
#67873 = CARTESIAN_POINT ( 'NONE',  ( 5.316205630334249754, 7.295602216847000498, -1.443375672974078761 ) ) ;
#67874 = CARTESIAN_POINT ( 'NONE',  ( 2.154674626568295892, -0.5202524484802829585, -1.891573884155263396 ) ) ;
#67875 = DIRECTION ( 'NONE',  ( 1.014813233446432150E-15, 1.000000000000000000, -4.583713267641621330E-32 ) ) ;
#67876 = CARTESIAN_POINT ( 'NONE',  ( -5.418418667316934112, 6.350518529071726981, -1.199719254218453823 ) ) ;
#67877 = CARTESIAN_POINT ( 'NONE',  ( 5.554972086574996304, 0.4156608669513595089, 2.079290889414136423 ) ) ;
#67879 = CARTESIAN_POINT ( 'NONE',  ( 10.93186801223270521, -5.758458176070768708, 2.033726106357576692E-15 ) ) ;
#67878 = CARTESIAN_POINT ( 'NONE',  ( 8.748035429315576650, 11.22912730566677553, -1.599625672291255185 ) ) ;
#67880 = CARTESIAN_POINT ( 'NONE',  ( 6.327413238363588377, -1.857107522167710245, 0.6617740914907597194 ) ) ;
#67881 = CARTESIAN_POINT ( 'NONE',  ( 0.6823417656249899377, 2.342708333674753618, 1.181850606188767472 ) ) ;
#67882 = CARTESIAN_POINT ( 'NONE',  ( 1.441653692521651653, -1.894234556111865420, 0.6821031695033189513 ) ) ;
#67883 = ORIENTED_EDGE ( 'NONE', *, *, #12006, .T. ) ;
#67884 = VECTOR ( 'NONE', #80709, 1000.000000000000114 ) ;
#67886 = CARTESIAN_POINT ( 'NONE',  ( 1.142374532877686644, 0.8619398222155623124, 1.934021905983105416 ) ) ;
#67885 = CARTESIAN_POINT ( 'NONE',  ( -6.887178846062109727, 10.01849717283904262, -1.082531754730537976 ) ) ;
#67887 = CARTESIAN_POINT ( 'NONE',  ( 11.84050473577397966, 6.857368744533671290, -1.964541968951881490 ) ) ;
#67888 = CARTESIAN_POINT ( 'NONE',  ( 2.119664376568120012, 0.3561266789769075292, -2.039353370234835872 ) ) ;
#67889 = CARTESIAN_POINT ( 'NONE',  ( 4.258142763143749399, 7.125527769379820242, 1.199719254218451159 ) ) ;
#67890 = CARTESIAN_POINT ( 'NONE',  ( 4.760848217054122422, 5.583353003765119560, -1.199719254218452047 ) ) ;
#67891 = ORIENTED_EDGE ( 'NONE', *, *, #171810, .T. ) ;
#67893 = CARTESIAN_POINT ( 'NONE',  ( 4.273844736805816780, 6.009238164405336313, 1.599625672291267398 ) ) ;
#67892 = CARTESIAN_POINT ( 'NONE',  ( 4.171883282844288665, -1.203828960760118694, 1.709054251895093746 ) ) ;
#67896 = EDGE_LOOP ( 'NONE', ( #174478, #125021, #75552, #106237 ) ) ;
#67895 = CARTESIAN_POINT ( 'NONE',  ( 2.648825499136245654, 0.2233988552288330709, 1.797577217741084921 ) ) ;
#67894 = CARTESIAN_POINT ( 'NONE',  ( 3.733261478165556646, -1.687024869733319221, 0.6981082995600741414 ) ) ;
#67897 = CARTESIAN_POINT ( 'NONE',  ( 0.2999999999999877764, 3.322650755865456773, -0.5865692111442898371 ) ) ;
#67898 = CARTESIAN_POINT ( 'NONE',  ( 6.889999999999997016, 3.693514451062899884, 2.514185260296258662 ) ) ;
#67899 = CARTESIAN_POINT ( 'NONE',  ( 9.997100500050640548, 9.889488447269407345, -5.009837084036856680 ) ) ;
#67900 = CARTESIAN_POINT ( 'NONE',  ( 5.210101597250164751, -2.196594437182074255, 0.2116553293704941940 ) ) ;
#67901 = CARTESIAN_POINT ( 'NONE',  ( -1.364683531250014514, 9.401041667008062319, -0.7879004041258335089 ) ) ;
#67902 = ORIENTED_EDGE ( 'NONE', *, *, #200488, .T. ) ;
#67903 = CARTESIAN_POINT ( 'NONE',  ( 4.459560945705238311, -1.480416612418914424, -1.210464771850598975 ) ) ;
#67904 = CARTESIAN_POINT ( 'NONE',  ( -3.110706179331648169, 5.716575411607132118, 1.199719254218462483 ) ) ;
#67905 = CARTESIAN_POINT ( 'NONE',  ( 8.471147050440139381, 8.777426401801974976, -0.7998128361456281477 ) ) ;
#67906 = CARTESIAN_POINT ( 'NONE',  ( 0.6801582343749847936, 0.5052083336747614783, 1.178068619123803451 ) ) ;
#67907 = CARTESIAN_POINT ( 'NONE',  ( 3.999292125906899198, 6.649295999324608353, 1.082531754730558626 ) ) ;
#67908 = EDGE_CURVE ( 'NONE', #175582, #113279, #146494, .T. ) ;
#67909 = CARTESIAN_POINT ( 'NONE',  ( 10.99979681685432631, -6.306104522322590000, 0.07019693227477653841 ) ) ;
#67910 = DIRECTION ( 'NONE',  ( 0.000000000000000000, 0.7999999999999947153, -0.6000000000000068612 ) ) ;
#67911 = CARTESIAN_POINT ( 'NONE',  ( 0.6965153189463432204, 1.505040478001760107, 1.060415605250275339 ) ) ;
#67912 = CARTESIAN_POINT ( 'NONE',  ( -11.88168329227126563, 12.22000000000000064, -1.685799833707130269 ) ) ;
#67913 = CARTESIAN_POINT ( 'NONE',  ( 3.514787476322968285, 1.689724804184733253, 0.8026845837263293371 ) ) ;
#67914 = CARTESIAN_POINT ( 'NONE',  ( 7.506374323821472849, 8.786466794993730289, -1.199719254218452047 ) ) ;
#67915 = PLANE ( 'NONE',  #36622 ) ;
#67916 = CARTESIAN_POINT ( 'NONE',  ( -6.222829318992474157, 10.20379193889247382, 0.000000000000000000 ) ) ;
#67917 = AXIS2_PLACEMENT_3D ( 'NONE', #50412, #148974, #101280 ) ;
#67918 = CARTESIAN_POINT ( 'NONE',  ( 5.281064527722868718, 6.119995689553514140, 1.199719254218462483 ) ) ;
#67919 = CARTESIAN_POINT ( 'NONE',  ( 0.3913703952206915027, -1.802969083500185477, 0.7928767443170018359 ) ) ;
#67920 = EDGE_CURVE ( 'NONE', #156131, #111968, #21345, .T. ) ;
#67921 = CARTESIAN_POINT ( 'NONE',  ( 2.267204043252795120, 1.842440753109304330, -0.8197907266209791821 ) ) ;
#67922 = CARTESIAN_POINT ( 'NONE',  ( -9.332089804907933939, 9.781859615347734405, 1.040834085586084257E-14 ) ) ;
#67923 = CARTESIAN_POINT ( 'NONE',  ( 6.852720297064418986, 6.959538199522133262, 0.7998128361456331437 ) ) ;
#67924 = CARTESIAN_POINT ( 'NONE',  ( 2.836070844659248191, 2.175002134116140518, 0.2674123886829762875 ) ) ;
#67925 = CARTESIAN_POINT ( 'NONE',  ( 5.953692858212230377, 0.5253669772854427933, -1.748464709795935157 ) ) ;
#67926 = CARTESIAN_POINT ( 'NONE',  ( -4.298098390732130625, 4.973201863064262263, 1.199719254218462483 ) ) ;
#67927 = CARTESIAN_POINT ( 'NONE',  ( 5.560252395380215873, 6.619954228432645138, 1.082531754730549078 ) ) ;
#67928 = CARTESIAN_POINT ( 'NONE',  ( 9.368847842243145152, 10.88907622316056312, 1.199719254218453823 ) ) ;
#67929 = CARTESIAN_POINT ( 'NONE',  ( 3.192055101013606233, 5.811482486902795230, -1.199719254218446718 ) ) ;
#67930 = CARTESIAN_POINT ( 'NONE',  ( 5.560252395380198998, 9.501061871336672127, 0.7216878364870317197 ) ) ;
#67931 = ORIENTED_EDGE ( 'NONE', *, *, #119884, .T. ) ;
#67933 = CARTESIAN_POINT ( 'NONE',  ( 0.9088405895168538695, -0.4911093815175514021, -1.952142171939993842 ) ) ;
#67932 = CARTESIAN_POINT ( 'NONE',  ( 4.142028884782995135, 0.4951553702221401232, 1.773339192993342639 ) ) ;
#67934 = CARTESIAN_POINT ( 'NONE',  ( 2.601245504928787700, 1.085180258111384077, -2.026094289238103752 ) ) ;
#67936 = CARTESIAN_POINT ( 'NONE',  ( 1.445918188014534422, -0.8427435445049488161, 1.659298548423918884 ) ) ;
#67935 = FACE_OUTER_BOUND ( 'NONE', #48269, .T. ) ;
#67937 = CARTESIAN_POINT ( 'NONE',  ( 3.475000000000000533, -0.5541666666666681396, 2.006292185433948827 ) ) ;
#67938 = CARTESIAN_POINT ( 'NONE',  ( -6.064574784014443942, 5.969758757638621738, -0.7998128361456291469 ) ) ;
#67939 = CARTESIAN_POINT ( 'NONE',  ( 0.000000000000000000, 1.016439536705160407E-16, 11.18000000000000149 ) ) ;
#67940 = CARTESIAN_POINT ( 'NONE',  ( 4.658414424252744546, 1.907665749568526747, 0.1350064596054162680 ) ) ;
#67941 = CARTESIAN_POINT ( 'NONE',  ( -7.472515219426274946, 11.86968485597268064, 0.000000000000000000 ) ) ;
#67942 = CARTESIAN_POINT ( 'NONE',  ( 6.485343392949857844, 6.752073445700102816, -0.1478272009810890908 ) ) ;
#67943 = CARTESIAN_POINT ( 'NONE',  ( -7.160114521792834807, 8.486460042580672436, 1.082531754730549078 ) ) ;
#67945 = CARTESIAN_POINT ( 'NONE',  ( 2.676452114398766291, -1.789519730395791486, -0.5449050523786898026 ) ) ;
#67944 = CARTESIAN_POINT ( 'NONE',  ( 3.808215996505484036, 1.477046120823837683, -1.479981065426434483 ) ) ;
#67946 = CARTESIAN_POINT ( 'NONE',  ( 6.629573927402440781, 10.67832731537079383, 1.040834085586084257E-14 ) ) ;
#67947 = CARTESIAN_POINT ( 'NONE',  ( 1.364683531249988535, 5.467708333674750953, -0.7879004041258300672 ) ) ;
#67948 = CARTESIAN_POINT ( 'NONE',  ( 3.737644501653397455, 1.732476483319781657, 0.1661042753308156761 ) ) ;
#67949 = CARTESIAN_POINT ( 'NONE',  ( 3.337278367258157630, 7.045241861776501580, 0.7998128361456341429 ) ) ;
#67950 = CARTESIAN_POINT ( 'NONE',  ( 5.800636919132594826, 6.158450155783071978, -0.8617315278892097030 ) ) ;
#67951 = CARTESIAN_POINT ( 'NONE',  ( 4.055083665587292607, -1.435586732866575010, -0.9558459365816800446 ) ) ;
#67952 = CARTESIAN_POINT ( 'NONE',  ( -7.226659571283968297, 8.389856573708110332, 1.199719254218450271 ) ) ;
#67953 = CARTESIAN_POINT ( 'NONE',  ( 6.709632191794143274, -0.4886956906769434061, 2.160084693451309601 ) ) ;
#67954 = CARTESIAN_POINT ( 'NONE',  ( 6.983263157960365675, -0.006178392973848687020, 2.053544886540019210 ) ) ;
#67955 = AXIS2_PLACEMENT_3D ( 'NONE', #152392, #156674, #135094 ) ;
#67956 = CARTESIAN_POINT ( 'NONE',  ( -0.6125000000000314637, 0.8541666673494846540, 1.060881119635901593 ) ) ;
#67957 = CARTESIAN_POINT ( 'NONE',  ( 3.942362285364631624, -1.074967207919340861, 1.886227828529878803 ) ) ;
#67958 = CARTESIAN_POINT ( 'NONE',  ( 3.738726038629454074, 0.2694068579384528150, 1.805578518607708016 ) ) ;
#67959 = CARTESIAN_POINT ( 'NONE',  ( 0.7500000000000006661, 12.41666666666666607, -1.299038105676657340 ) ) ;
#67960 = CARTESIAN_POINT ( 'NONE',  ( 5.630101985619759830, 2.115003628044552553, 0.1013798475145138156 ) ) ;
#67961 = ORIENTED_EDGE ( 'NONE', *, *, #149140, .T. ) ;
#67963 = CARTESIAN_POINT ( 'NONE',  ( 0.6823417656249882723, 2.238541667008084435, -1.181850606188749264 ) ) ;
#67962 = CARTESIAN_POINT ( 'NONE',  ( 5.653944246587851552, 0.9260977375703757231, 2.097164529332084637 ) ) ;
#67964 = CARTESIAN_POINT ( 'NONE',  ( 8.028399517586572998, 12.51821653715971472, -0.7998128361456352531 ) ) ;
#67965 = AXIS2_PLACEMENT_3D ( 'NONE', #23580, #53967, #204448 ) ;
#67966 = CARTESIAN_POINT ( 'NONE',  ( 1.682450335255514240, 1.092831414372618326, 1.817064408815848964 ) ) ;
#67967 = CARTESIAN_POINT ( 'NONE',  ( -4.528060117284246289, 6.305822774963486310, 1.443375672974064550 ) ) ;
#67968 = CARTESIAN_POINT ( 'NONE',  ( 2.385871846325007706, 5.727341554113725586, -0.7216878364870267237 ) ) ;
#67969 = CARTESIAN_POINT ( 'NONE',  ( -4.717874267431199087, 8.448011045404303587, 1.040834085586084257E-14 ) ) ;
#67970 = CARTESIAN_POINT ( 'NONE',  ( 6.860228214211484321, -2.170771502548960452, 0.04436455139915015944 ) ) ;
#67973 = B_SPLINE_CURVE_WITH_KNOTS ( 'NONE', 3,
 ( #118276, #19633, #183206, #50015, #100887, #33757 ),
 .UNSPECIFIED., .F., .F.,
 ( 4, 2, 4 ),
 ( 0.000000000000000000, 0.0003172254002810696557, 0.0006344508005621393113 ),
 .UNSPECIFIED. ) ;
#67972 = CARTESIAN_POINT ( 'NONE',  ( -0.7500000000000179856, 12.32291666734946389, 1.299038105676658228 ) ) ;
#67971 = CARTESIAN_POINT ( 'NONE',  ( 0.000000000000000000, 13.88000000000000078, 0.000000000000000000 ) ) ;
#67975 = VERTEX_POINT ( 'NONE', #131791 ) ;
#67974 = CARTESIAN_POINT ( 'NONE',  ( 0.8389114244844765311, 1.318684809372525857, -1.787403929136616165 ) ) ;
#67976 = CARTESIAN_POINT ( 'NONE',  ( 0.07143917554365029898, -1.076037094620578616, 2.031297111741585226 ) ) ;
#67978 = CARTESIAN_POINT ( 'NONE',  ( 3.959878945198321620, -0.6033026367360559972, 1.972334540003743530 ) ) ;
#67977 = CARTESIAN_POINT ( 'NONE',  ( 5.345992642490140057, 5.131412925860272090, 1.040834085586084257E-14 ) ) ;
#67980 = CARTESIAN_POINT ( 'NONE',  ( 1.001543065824772753E-15, -3.412500000000000977, 4.012584370867899430 ) ) ;
#67979 = CARTESIAN_POINT ( 'NONE',  ( 6.801350335910821165, 7.963938809097990124, 1.199719254218452047 ) ) ;
#67981 = CARTESIAN_POINT ( 'NONE',  ( 6.068156270568149324, 9.237210194708310951, 1.199719254218452047 ) ) ;
#67982 = CARTESIAN_POINT ( 'NONE',  ( 1.642778471875001811, -1.042708332855375009, 2.845375778867859751 ) ) ;
#67983 = CARTESIAN_POINT ( 'NONE',  ( -2.788906526875773208E-15, 12.68749999999999822, -1.499999999999998446 ) ) ;
#67984 = CARTESIAN_POINT ( 'NONE',  ( 0.1641640845322315523, -1.364019775510204369, 1.584451847793943324 ) ) ;
#67985 = CARTESIAN_POINT ( 'NONE',  ( 4.324842380567116784, 0.8596320953860696612, -1.824118450417112847 ) ) ;
#67986 = CARTESIAN_POINT ( 'NONE',  ( 3.913478945735289205, -0.9499487412085620974, -1.577145280185827447 ) ) ;
#67987 = PRESENTATION_LAYER_ASSIGNMENT (  '', '', ( #140729 ) ) ;
#67988 = CARTESIAN_POINT ( 'NONE',  ( 4.843287188579786573, 6.673587691474970107, -1.599625672291256295 ) ) ;
#67989 = SURFACE_STYLE_USAGE ( .BOTH. , #120052 ) ;
#67990 = CARTESIAN_POINT ( 'NONE',  ( 0.7973487315477224557, -0.6271472479968034364, 1.606907058918445985 ) ) ;
#67991 = CARTESIAN_POINT ( 'NONE',  ( 0.3742329010679063539, -2.001858617179689492, -0.2420261300371470137 ) ) ;
#67992 = CARTESIAN_POINT ( 'NONE',  ( 1.038157343047078296, -1.808118644657311203, 1.419311033984706816 ) ) ;
#67993 = CARTESIAN_POINT ( 'NONE',  ( -6.573005544526917099, 6.562927978236513304, -0.7998128361456291469 ) ) ;
#67994 = CARTESIAN_POINT ( 'NONE',  ( 1.195004664211458456, -0.5499296976853912389, -2.194457269061194982 ) ) ;
#67995 = CARTESIAN_POINT ( 'NONE',  ( 3.475310780013381340, 0.05149396089606420035, -2.105609240523627967 ) ) ;
#67996 = CARTESIAN_POINT ( 'NONE',  ( -6.296835998904160014, 6.311006518335105397, 0.000000000000000000 ) ) ;
#67997 = CARTESIAN_POINT ( 'NONE',  ( 5.438792177376376991, 9.497007973581119700, 1.040834085586084257E-14 ) ) ;
#67998 = CARTESIAN_POINT ( 'NONE',  ( 5.872089928050205465, 6.023395468912922546, -0.7216878364870458196 ) ) ;
#67999 = CARTESIAN_POINT ( 'NONE',  ( 6.000000000000004441, -3.414667428843525066E-13, -2.052068128417939619 ) ) ;
#68001 = ADVANCED_FACE ( 'NONE', ( #185801 ), #65642, .T. ) ;
#68000 = CARTESIAN_POINT ( 'NONE',  ( -5.063080299699540987, 7.994345218703034384, 1.199719254218464037 ) ) ;
#68002 = CARTESIAN_POINT ( 'NONE',  ( 6.765155463094761679, 6.995028916473103209, 0.7216878364870317197 ) ) ;
#68003 = CARTESIAN_POINT ( 'NONE',  ( -1.201851678989727383E-14, 2.462500000000023004, 1.732050807568877637 ) ) ;
#68004 = CARTESIAN_POINT ( 'NONE',  ( -4.135400547368138113, 4.783387712472935149, 1.199719254218462483 ) ) ;
#68005 = CARTESIAN_POINT ( 'NONE',  ( 5.344044365905453731, -1.409322151232726750, -1.717068368634220299 ) ) ;
#68006 = CARTESIAN_POINT ( 'NONE',  ( 3.486445073788289051, -0.4274320362823453290, -2.149191018322317515 ) ) ;
#68007 = CARTESIAN_POINT ( 'NONE',  ( -5.250031796989778066, 7.148123067953287446, 1.599625672291267398 ) ) ;
#68008 = CARTESIAN_POINT ( 'NONE',  ( -11.94980361723156292, 10.09761943414563845, 1.099999926404457984 ) ) ;
#68009 = CARTESIAN_POINT ( 'NONE',  ( 1.364683531249988535, 3.405208333674749621, -0.7879004041258239610 ) ) ;
#68010 = CARTESIAN_POINT ( 'NONE',  ( 6.889999999999997016, 3.693514451062899884, 2.514185260296258217 ) ) ;
#68011 = CARTESIAN_POINT ( 'NONE',  ( -4.121315508874255684, 7.752025827087861920, -0.7216878364870267237 ) ) ;
#68012 = CARTESIAN_POINT ( 'NONE',  ( 5.010073305087408002, -0.7609581946756528437, 1.979555329295646260 ) ) ;
#68013 = CARTESIAN_POINT ( 'NONE',  ( -7.783789588021474692, 8.253711738879413673, 0.7216878364870317197 ) ) ;
#68014 = VERTEX_POINT ( 'NONE', #133915 ) ;
#68016 = CARTESIAN_POINT ( 'NONE',  ( 6.719591497160966931, -2.098179372288328182, 0.5198544864785522579 ) ) ;
#68015 = CARTESIAN_POINT ( 'NONE',  ( -5.722950238744243023, 7.770137593325314285, 1.443375672974058777 ) ) ;
#68017 = CARTESIAN_POINT ( 'NONE',  ( 5.331380718671758778, 7.243030143248949670, -1.599625672291256295 ) ) ;
#68018 = CARTESIAN_POINT ( 'NONE',  ( 5.759284750224211713, 1.812880138157666465, -0.3211251414683007899 ) ) ;
#68019 = UNCERTAINTY_MEASURE_WITH_UNIT (LENGTH_MEASURE( 1.000000000000000082E-05 ), #72500, 'distance_accuracy_value', 'NONE');
#68020 = FILL_AREA_STYLE ('',( #33418 ) ) ;
#68021 = CARTESIAN_POINT ( 'NONE',  ( 0.6823417656249917140, 3.405208333674754506, 1.181850606188765695 ) ) ;
#68022 = CARTESIAN_POINT ( 'NONE',  ( 0.7666889417085223091, 1.677783727127066804, -0.4624100818488885434 ) ) ;
#68023 = CARTESIAN_POINT ( 'NONE',  ( -1.387358672536802340, 7.315968950354509559, 4.254625267136455058 ) ) ;
#68024 = DIRECTION ( 'NONE',  ( 3.330669073875478989E-16, -3.540251991789410786E-16, -1.000000000000000000 ) ) ;
#68025 = CARTESIAN_POINT ( 'NONE',  ( 10.92268642758943642, 8.218322760642331914, -4.985627623770443329 ) ) ;
#68026 = CARTESIAN_POINT ( 'NONE',  ( 5.032170685167933755, 1.114402916724830161, -1.852182961850391774 ) ) ;
#68027 = EDGE_CURVE ( 'NONE', #170885, #177299, #3944, .T. ) ;
#68028 = CARTESIAN_POINT ( 'NONE',  ( -4.946027110887008860, 4.664786472323266153, -0.7998128361456221525 ) ) ;
#68029 = CARTESIAN_POINT ( 'NONE',  ( -6.344852701071109102, 10.34615255131755163, 0.000000000000000000 ) ) ;
#68030 = CARTESIAN_POINT ( 'NONE',  ( 4.258765444007106105, -1.603684720688375975, 1.449730421305382544 ) ) ;
#68031 = CARTESIAN_POINT ( 'NONE',  ( -0.6823417656250003738, 2.467708333674753618, -1.181850606188749264 ) ) ;
#68032 = CARTESIAN_POINT ( 'NONE',  ( 6.151636724293027214, 0.5744773170833740172, -1.885769548957224817 ) ) ;
#68033 = CARTESIAN_POINT ( 'NONE',  ( 5.430864382934267987, 0.8560856307190685133, 1.507619432454242681 ) ) ;
#68034 = CARTESIAN_POINT ( 'NONE',  ( 1.523247060345904291, -2.062048068855956373, 0.7425582295156886170 ) ) ;
#68035 = CARTESIAN_POINT ( 'NONE',  ( 2.468180027558197320, 2.263118346622743360, -0.4500467933809069176 ) ) ;
#68036 = CARTESIAN_POINT ( 'NONE',  ( 4.305972304023081954, -2.055534471369814487, 0.1475827967423407050 ) ) ;
#68037 = CARTESIAN_POINT ( 'NONE',  ( 6.462452672982783142, -1.777441430900746688, -0.7828909329169189135 ) ) ;
#68038 = CARTESIAN_POINT ( 'NONE',  ( -6.683806541412762314, 9.781229484081471526, -1.082531754730537976 ) ) ;
#68039 = B_SPLINE_CURVE_WITH_KNOTS ( 'NONE', 3,
 ( #198619, #69683, #53454, #19876 ),
 .UNSPECIFIED., .F., .F.,
 ( 4, 4 ),
 ( 0.000000000000000000, 9.170750103568812571E-05 ),
 .UNSPECIFIED. ) ;
#68041 = EDGE_CURVE ( 'NONE', #123271, #101393, #96063, .T. ) ;
#68040 = CARTESIAN_POINT ( 'NONE',  ( -2.979759899953417612, 6.698413326579433225, 0.7998128361456352531 ) ) ;
#68042 = CARTESIAN_POINT ( 'NONE',  ( -1.772826578343124959, 3.950000000000009059, -0.4500000000000423661 ) ) ;
#68043 = CYLINDRICAL_SURFACE ( 'NONE', #101887, 11.99999999999999112 ) ;
#68044 = CARTESIAN_POINT ( 'NONE',  ( 1.565077508395201988, -1.076315722900993643, 1.704939445326451475 ) ) ;
#68045 = CARTESIAN_POINT ( 'NONE',  ( -6.683806541412768532, 8.820860269780128604, -1.443375672974058777 ) ) ;
#68046 = CARTESIAN_POINT ( 'NONE',  ( 3.469938103458301892, 2.153457811087633011, -0.4814610123115290463 ) ) ;
#68047 = CARTESIAN_POINT ( 'NONE',  ( -3.285556943750000070, -1.246874999522043392, 0.000000000000000000 ) ) ;
#68048 = CARTESIAN_POINT ( 'NONE',  ( 1.744728380183872218, -0.2665191970635071295, -1.841615994452956873 ) ) ;
#68049 = CARTESIAN_POINT ( 'NONE',  ( 1.931788062848141441E-13, 7.054063922337705073, -3.955400951015614730 ) ) ;
#68050 = DIRECTION ( 'NONE',  ( 1.000000000000000000, -5.391474854832587087E-16, 0.000000000000000000 ) ) ;
#68053 = AXIS2_PLACEMENT_3D ( 'NONE', #163691, #61921, #145347 ) ;
#68052 = CARTESIAN_POINT ( 'NONE',  ( 6.925078400183575233, 4.688909937558557672, 2.706876980850602354 ) ) ;
#68051 = CARTESIAN_POINT ( 'NONE',  ( -4.671432059311929841, 8.392430178223424520, -0.5935467769075646327 ) ) ;
#68054 = CARTESIAN_POINT ( 'NONE',  ( -1.743066579297358008E-15, 2.187499999999992006, -1.225000000000032951 ) ) ;
#68055 = ORIENTED_EDGE ( 'NONE', *, *, #164497, .T. ) ;
#68056 = CARTESIAN_POINT ( 'NONE',  ( 3.485278940986863638, 1.863876800102952203, -0.8796150190680316339 ) ) ;
#68057 = CARTESIAN_POINT ( 'NONE',  ( -0.6801582343750125492, 2.182291667008062763, 1.178068619123824323 ) ) ;
#68058 = UNCERTAINTY_MEASURE_WITH_UNIT (LENGTH_MEASURE( 1.000000000000000082E-05 ), #89298, 'distance_accuracy_value', 'NONE');
#68059 = CARTESIAN_POINT ( 'NONE',  ( -5.032047568966410367, 9.022472597102808578, 1.214306433183764966E-14 ) ) ;
#68060 = CARTESIAN_POINT ( 'NONE',  ( 2.069016002695713397, -1.559697248980717266, 1.283103002569847106 ) ) ;
#68061 = CARTESIAN_POINT ( 'NONE',  ( -1.500000000000015099, -1.079166666666641961, 0.8660254037844403729 ) ) ;
#68062 = CARTESIAN_POINT ( 'NONE',  ( 3.063252641683779753, 5.661212951017999373, 1.199719254218450271 ) ) ;
#68063 = CARTESIAN_POINT ( 'NONE',  ( 1.956002958106726419, 2.055451868484101219, -0.1503645474096800549 ) ) ;
#68065 = CARTESIAN_POINT ( 'NONE',  ( -1.364683531250000748, 13.10937500034139980, 0.000000000000000000 ) ) ;
#68064 = DIRECTION ( 'NONE',  ( 0.000000000000000000, 0.000000000000000000, -1.000000000000000000 ) ) ;
#68066 = CARTESIAN_POINT ( 'NONE',  ( 4.659198344590585350, 8.587481835331020719, 0.7998128361456462443 ) ) ;
#68067 = CARTESIAN_POINT ( 'NONE',  ( -0.1411974294641681893, 1.383765339824583052, -2.157932961605046440 ) ) ;
#68068 = CARTESIAN_POINT ( 'NONE',  ( 6.650339433524894872, -1.499410535642144549, 1.233700977392115705 ) ) ;
#68069 = ADVANCED_FACE ( 'NONE', ( #151202 ), #176372, .T. ) ;
#68070 = CARTESIAN_POINT ( 'NONE',  ( 5.338574060078519423, 2.173733305800494175, 0.3801736985692484305 ) ) ;
#68071 = CARTESIAN_POINT ( 'NONE',  ( 4.864343252252968597, 8.897093904262280972, 0.000000000000000000 ) ) ;
#68072 = CARTESIAN_POINT ( 'NONE',  ( 1.353037089713942320, -1.704917477850418805, 1.328741451194020762 ) ) ;
#68073 = CARTESIAN_POINT ( 'NONE',  ( -3.958617665510272943, 6.601842462195195438, -1.082531754730549967 ) ) ;
#68074 = CARTESIAN_POINT ( 'NONE',  ( 1.850796360583713884, -1.845628094615419768, -0.8128149310912060610 ) ) ;
#68075 = EDGE_CURVE ( 'NONE', #122713, #46203, #86864, .T. ) ;
#68076 = CARTESIAN_POINT ( 'NONE',  ( 2.073957380999270850, 1.703569143382680506, -1.543048383257297207 ) ) ;
#68077 = AXIS2_PLACEMENT_3D ( 'NONE', #55269, #6491, #72566 ) ;
#68078 = LINE ( 'NONE', #151510, #94140 ) ;
#68079 = CARTESIAN_POINT ( 'NONE',  ( 0.2505829665140328899, -1.505242420826727656, 1.110479572284161831 ) ) ;
#68080 = CARTESIAN_POINT ( 'NONE',  ( 2.149089010626914931, -1.500894351328721621, -1.116326037436713881 ) ) ;
#68081 = CIRCLE ( 'NONE', #102597, 0.5000000000000000000 ) ;
#68082 = CARTESIAN_POINT ( 'NONE',  ( 3.995327539805045181, -0.3399590882401174463, 1.987497567597557468 ) ) ;
#68084 = CARTESIAN_POINT ( 'NONE',  ( 10.01911233037457905, 11.75168114260095109, 1.082531754730548412 ) ) ;
#68083 = CARTESIAN_POINT ( 'NONE',  ( -1.201851678989727383E-14, 2.071875000341422801, 1.575800808251672791 ) ) ;
#68086 = CARTESIAN_POINT ( 'NONE',  ( 4.670599442626208742, -1.376304852316366789, 1.594240983682773782 ) ) ;
#68085 = CARTESIAN_POINT ( 'NONE',  ( -6.503107236049161521, 10.73870887536603291, 0.7998128361456481317 ) ) ;
#68087 = CARTESIAN_POINT ( 'NONE',  ( 5.670397268163976712, -0.9275489576153757021, -1.851018422006404096 ) ) ;
#68088 = CARTESIAN_POINT ( 'NONE',  ( 6.795661308947685164, 8.951357498570873261, -1.599625672291262513 ) ) ;
#68089 = CARTESIAN_POINT ( 'NONE',  ( -5.852315862593199469, 9.979452273000736895, 0.7998128361456481317 ) ) ;
#68090 = CARTESIAN_POINT ( 'NONE',  ( -1.608462485350629301, 8.735270501766756013, 2.463594439587650342 ) ) ;
#68091 = CARTESIAN_POINT ( 'NONE',  ( 5.554946522049384328, 0.3980760423633997180, 1.979986811436624805 ) ) ;
#68092 = CARTESIAN_POINT ( 'NONE',  ( -1.402160292154681736E-14, -0.6312499993171797330, -1.732050807568870754 ) ) ;
#68093 = CARTESIAN_POINT ( 'NONE',  ( 0.7079710255328255375, 0.6504495457556063176, -1.957355765043818696 ) ) ;
#68094 = CARTESIAN_POINT ( 'NONE',  ( 8.948018195339340508, 9.541702104091804415, -0.7216878364870197293 ) ) ;
#68095 = CARTESIAN_POINT ( 'NONE',  ( 5.993586425693011144, 9.150212042353954800, -1.199719254218452047 ) ) ;
#68096 = CARTESIAN_POINT ( 'NONE',  ( 5.306037014901791693, 7.283738832175834510, 1.599625672291269396 ) ) ;
#68097 = CARTESIAN_POINT ( 'NONE',  ( 0.6823417656249882723, 0.4052083336747516751, 1.181850606188755259 ) ) ;
#68099 =( NAMED_UNIT ( * ) SI_UNIT ( $, .STERADIAN. ) SOLID_ANGLE_UNIT ( ) );
#68098 = CARTESIAN_POINT ( 'NONE',  ( 6.052789233858158369, 6.026285292448116948, 0.000000000000000000 ) ) ;
#68100 = CARTESIAN_POINT ( 'NONE',  ( 6.927853306458743532, 9.105581495667113501, 1.443375672974076540 ) ) ;
#68102 = CARTESIAN_POINT ( 'NONE',  ( -6.180810755953226376, 5.328981043924833294, -2.500000000000671019 ) ) ;
#68101 = CARTESIAN_POINT ( 'NONE',  ( 2.735037655519993560, -2.077075009683257090, -0.6322084445426826571 ) ) ;
#68104 = CARTESIAN_POINT ( 'NONE',  ( 3.122423488780329492, 0.04808623196613136253, 1.840796284283818585 ) ) ;
#68103 = CARTESIAN_POINT ( 'NONE',  ( -4.853455804012230423, 6.685451076146141425, 1.443375672974064550 ) ) ;
#68105 = CARTESIAN_POINT ( 'NONE',  ( -0.6823417656249969321, 3.967708333674754950, -1.181850606188749264 ) ) ;
#68106 = CARTESIAN_POINT ( 'NONE',  ( 4.915667883426772633, -1.172277214026868464, -1.851500752446763709 ) ) ;
#68107 = CARTESIAN_POINT ( 'NONE',  ( 8.621587210660656808, 13.70538846753250795, 8.347036492328824053 ) ) ;
#68108 = CARTESIAN_POINT ( 'NONE',  ( 5.348581951612152885, 0.6511601234850499242, 2.166799557567296919 ) ) ;
#68109 = CARTESIAN_POINT ( 'NONE',  ( -3.716906668440817185, 7.488141546489591072, 0.7998128361456341429 ) ) ;
#68110 = CARTESIAN_POINT ( 'NONE',  ( -6.471393748265563239, 5.229711127717889596, 2.420000000000002149 ) ) ;
#68111 = CARTESIAN_POINT ( 'NONE',  ( 4.681345713234763117, 8.384430392927429310, -0.5894114041281351968 ) ) ;
#68112 = CARTESIAN_POINT ( 'NONE',  ( -5.383996397958228819, 8.335060660042973524, 1.082531754730550855 ) ) ;
#68113 = CARTESIAN_POINT ( 'NONE',  ( 3.879041347285658414, 6.579279767591636130, -1.082531754730548412 ) ) ;
#68114 = CARTESIAN_POINT ( 'NONE',  ( 6.591055360535956531, 1.538344802651976373, -0.8746889052434738687 ) ) ;
#68115 = VECTOR ( 'NONE', #25581, 1000.000000000000000 ) ;
#68116 = CARTESIAN_POINT ( 'NONE',  ( 4.354156267015011572, 0.8588168762691525959, -1.820826276449886150 ) ) ;
#68117 = CARTESIAN_POINT ( 'NONE',  ( 8.118635056484817980, 8.366162408854107113, 0.7998128361456481317 ) ) ;
#68118 = CARTESIAN_POINT ( 'NONE',  ( 2.538226622342924177, 0.9936286567288643568, -1.856823529840909481 ) ) ;
#68119 = CARTESIAN_POINT ( 'NONE',  ( 1.546349530022947727, -1.353405651413071453, 1.355934989043396044 ) ) ;
#68121 = CARTESIAN_POINT ( 'NONE',  ( -0.7500000000000215383, 2.941666666666689522, 1.299038105676671107 ) ) ;
#68120 = CARTESIAN_POINT ( 'NONE',  ( -8.012344526598182026E-15, 12.29687500034140513, -1.575800808251669460 ) ) ;
#68122 = B_SPLINE_CURVE_WITH_KNOTS ( 'NONE', 3,
 ( #11162, #78307, #77239, #126081, #142284, #176887 ),
 .UNSPECIFIED., .F., .F.,
 ( 4, 2, 4 ),
 ( 0.0004065497138311910700, 0.0007003026727366323291, 0.0009940556316420734798 ),
 .UNSPECIFIED. ) ;
#68124 = EDGE_CURVE ( 'NONE', #198880, #200740, #115316, .T. ) ;
#68123 = CARTESIAN_POINT ( 'NONE',  ( 2.400782916097830455, 0.4286735998642232648, 1.922169311629307931 ) ) ;
#68125 = CARTESIAN_POINT ( 'NONE',  ( 0.07479286986305370977, 0.004866263145587856019, -1.855573292446038414 ) ) ;
#68126 = CARTESIAN_POINT ( 'NONE',  ( 0.7484013653801385724, -1.946605496936428370, -0.2438083268051088881 ) ) ;
#68128 = ORIENTED_EDGE ( 'NONE', *, *, #17772, .F. ) ;
#68127 = CARTESIAN_POINT ( 'NONE',  ( 0.6328886395040033142, 1.767934563615305432, 0.7296191750566642931 ) ) ;
#68129 = CARTESIAN_POINT ( 'NONE',  ( 6.968527767744109980, 7.232296605230681408, 0.7216878364870317197 ) ) ;
#68130 = TOROIDAL_SURFACE ( 'NONE', #26719, 6.909076424898650259, 0.08000000000000000167 ) ;
#68131 = CARTESIAN_POINT ( 'NONE',  ( -0.6823417656250246877, 0.1135416670080893753, 1.181850606188755259 ) ) ;
#68132 = CARTESIAN_POINT ( 'NONE',  ( 5.471519871388384360, 1.802534880541529994, -0.5000026934619330454 ) ) ;
#68133 = CARTESIAN_POINT ( 'NONE',  ( 9.999301985278609806, 11.62460605670194447, 1.199719254218452047 ) ) ;
#68134 = CARTESIAN_POINT ( 'NONE',  ( -0.6823417656250212460, 2.801041667008084879, 1.181850606188767472 ) ) ;
#68135 = CARTESIAN_POINT ( 'NONE',  ( 5.489151832033660305, 0.1466973765328460355, 2.065091666743318122 ) ) ;
#68136 = FILL_AREA_STYLE_COLOUR ( '', #138982 ) ;
#68137 = CARTESIAN_POINT ( 'NONE',  ( -4.055297343818976330, 5.824542549245813383, 1.443375672974065660 ) ) ;
#68138 = CARTESIAN_POINT ( 'NONE',  ( 0.2036857628631080219, -1.599406074100502506, -1.314310892166506095 ) ) ;
#68139 = CARTESIAN_POINT ( 'NONE',  ( -1.500000000000015099, 0.1291666666666918539, -0.8660254037844383745 ) ) ;
#68140 = CARTESIAN_POINT ( 'NONE',  ( 5.777746017718023097, 9.892454120646377191, 0.7998128361456462443 ) ) ;
#68141 = CARTESIAN_POINT ( 'NONE',  ( -7.506410603460441422, 11.90922947067921278, -0.7998128361456291469 ) ) ;
#68142 = CARTESIAN_POINT ( 'NONE',  ( 6.313256805818848960, 7.394496357324014113, 1.199719254218452047 ) ) ;
#68143 = CARTESIAN_POINT ( 'NONE',  ( -1.364683531250000748, 1.259375000341421469, 0.000000000000000000 ) ) ;
#68144 = CONICAL_SURFACE ( 'NONE', #16355, 10.99999999999999112, 0.7853981633974479459 ) ;
#68145 = ORIENTED_EDGE ( 'NONE', *, *, #184735, .T. ) ;
#68147 = ADVANCED_FACE ( 'NONE', ( #174667 ), #120904, .T. ) ;
#68146 = CARTESIAN_POINT ( 'NONE',  ( 1.499999999999989120, 2.275000000000019895, 1.214306433183764966E-14 ) ) ;
#68149 = CARTESIAN_POINT ( 'NONE',  ( 3.174580523894166006, 6.855427711185178019, 0.7998128361456341429 ) ) ;
#68148 = CARTESIAN_POINT ( 'NONE',  ( 4.773855682050706761, -1.924389145058275963, 0.3807478752155256663 ) ) ;
#68150 = CARTESIAN_POINT ( 'NONE',  ( 3.550157523342876154, 1.823840110401256931, -0.8594984857327038208 ) ) ;
#68151 = CARTESIAN_POINT ( 'NONE',  ( 2.940549639715861030, -1.447296733178250250, 1.255168957218324666 ) ) ;
#68152 = CARTESIAN_POINT ( 'NONE',  ( 0.02921319935947005314, -2.001080581411585513, 0.8940957790435491992 ) ) ;
#68153 = CARTESIAN_POINT ( 'NONE',  ( 0.1331715793776600265, 0.003733371859311259821, -1.953671397793784070 ) ) ;
#68154 = CARTESIAN_POINT ( 'NONE',  ( 3.514787476322968285, 1.689724804184733253, 0.8026845837263293371 ) ) ;
#68155 = CARTESIAN_POINT ( 'NONE',  ( 1.499999999999985123, -0.1729166659838496101, -0.8660254037844323793 ) ) ;
#68156 = CARTESIAN_POINT ( 'NONE',  ( -8.016948904382338981, 8.247528564734524892, -0.7998128361456291469 ) ) ;
#68158 = CARTESIAN_POINT ( 'NONE',  ( 4.464542613241986757, -2.054094600764106548, -0.5127786416893320709 ) ) ;
#68157 = CARTESIAN_POINT ( 'NONE',  ( -4.446711195602252253, 6.210915699667823198, -1.443375672974053447 ) ) ;
#68159 = B_SPLINE_CURVE_WITH_KNOTS ( 'NONE', 3,
 ( #194201, #175841, #9051, #211506, #210441, #109830 ),
 .UNSPECIFIED., .F., .F.,
 ( 4, 2, 4 ),
 ( 0.001496030744711039119, 0.002086206484339677911, 0.002676382223968317136 ),
 .UNSPECIFIED. ) ;
#68160 = CARTESIAN_POINT ( 'NONE',  ( 4.227444969362701421, 3.826440640544909400, 1.214306433183764966E-14 ) ) ;
#68161 = CARTESIAN_POINT ( 'NONE',  ( 5.600075274486990828, 0.8424382930321882013, -1.891409743246947217 ) ) ;
#68163 = CARTESIAN_POINT ( 'NONE',  ( 6.620655732516651071, 2.021119449029490589, 2.477762541108457839 ) ) ;
#68162 = CARTESIAN_POINT ( 'NONE',  ( 2.665665183201745947, 1.120710701610077908, 1.764813211807507942 ) ) ;
#68165 = VERTEX_POINT ( 'NONE', #191931 ) ;
#68164 = CARTESIAN_POINT ( 'NONE',  ( 0.7270763493693053192, -1.639898566368836130, 0.5346300883638678281 ) ) ;
#68166 = CARTESIAN_POINT ( 'NONE',  ( 7.284808609244363353, 7.393364887073558656, 0.7998128361456341429 ) ) ;
#68167 = SURFACE_STYLE_USAGE ( .BOTH. , #134299 ) ;
#68168 = CARTESIAN_POINT ( 'NONE',  ( -0.09264309395031754268, -9.919020119916163836, -9.499548513212880962 ) ) ;
#68169 = CARTESIAN_POINT ( 'NONE',  ( -10.55163518180063242, 5.124035624933899413, 7.011265714045999076 ) ) ;
#68171 = CARTESIAN_POINT ( 'NONE',  ( 6.222829318548112276, 9.243422724072711816, -1.082531754730537976 ) ) ;
#68170 = CARTESIAN_POINT ( 'NONE',  ( 7.470706336329915764, 8.674577799595093452, -1.199719254218441611 ) ) ;
#68173 =( BOUNDED_SURFACE ( )  B_SPLINE_SURFACE ( 3, 2, ( 
 ( #3659, #51392, #200800 ),
 ( #16724, #50320, #102259 ),
 ( #68670, #184564, #149962 ),
 ( #183506, #198675, #151032 ),
 ( #66526, #19928, #165133 ),
 ( #82809, #132669, #54581 ) ),
 .UNSPECIFIED., .F., .F., .T. ) 
 B_SPLINE_SURFACE_WITH_KNOTS ( ( 4, 2, 4 ),
 ( 3, 3 ),
 ( 0.000000000000000000, 0.0003754689591423961527, 0.0007509379182847923054 ),
 ( 0.000000000000000000, 1.000000000000000000 ),
 .UNSPECIFIED. ) 
 GEOMETRIC_REPRESENTATION_ITEM ( )  RATIONAL_B_SPLINE_SURFACE ( (
 ( 1.000000000000000000, 0.7071067811865475727, 1.000000000000000000),
 ( 1.000000000000000000, 0.7018599272026954106, 1.000000000000000000),
 ( 1.000000000000000000, 0.6927733177256546471, 1.000000000000000000),
 ( 1.000000000000000000, 0.6772007068877438085, 1.000000000000000000),
 ( 1.000000000000000000, 0.6709974581634233770, 1.000000000000000000),
 ( 1.000000000000000000, 0.6711954675835484219, 1.000000000000000000) ) ) 
 REPRESENTATION_ITEM ( '' )  SURFACE ( )  );
#68172 = CARTESIAN_POINT ( 'NONE',  ( 3.719872605471109761, 6.605953636083950364, -2.420000000000002149 ) ) ;
#68175 = CARTESIAN_POINT ( 'NONE',  ( 0.4338566731940462495, -0.9675643781421030543, -1.531218756180543927 ) ) ;
#68174 = CARTESIAN_POINT ( 'NONE',  ( 5.508355548902068577, 9.648441583686274470, 0.7998128361456331437 ) ) ;
#68176 = CARTESIAN_POINT ( 'NONE',  ( -7.588813295347149435, 9.876701482703580837, -1.599625672291263179 ) ) ;
#68177 = CARTESIAN_POINT ( 'NONE',  ( 5.691725559638619814, 5.534767995866836543, 1.040834085586084257E-14 ) ) ;
#68178 = CARTESIAN_POINT ( 'NONE',  ( -5.288707357724018898, 7.660230058424141397, 1.223219983389673748 ) ) ;
#68179 = CARTESIAN_POINT ( 'NONE',  ( 7.147083253059300922, 8.367293879104554577, 1.199719254218452935 ) ) ;
#68180 = CARTESIAN_POINT ( 'NONE',  ( -7.110792111438893670, -7.169578370797517586, -7.767011945534271433 ) ) ;
#68181 = CARTESIAN_POINT ( 'NONE',  ( 4.143432174609324115, 7.404820066527033617, -0.7413545030366501809 ) ) ;
#68182 = CARTESIAN_POINT ( 'NONE',  ( 8.758204044747998296, 11.24099069033793974, 1.443375672974076540 ) ) ;
#68183 = ORIENTED_EDGE ( 'NONE', *, *, #143796, .T. ) ;
#68184 = CARTESIAN_POINT ( 'NONE',  ( 0.8783700953360704666, -0.4667435877003899836, -1.857722024819864037 ) ) ;
#68185 = CARTESIAN_POINT ( 'NONE',  ( 0.1356056236470788157, -0.09959319089659908475, 2.118264760961988458 ) ) ;
#68186 = DIRECTION ( 'NONE',  ( 3.330669073875479482E-16, -3.330669073875479482E-16, -1.000000000000000000 ) ) ;
#68187 = CARTESIAN_POINT ( 'NONE',  ( 0.000000000000000000, 15.00041888085534758, 0.000000000000000000 ) ) ;
#68188 = CARTESIAN_POINT ( 'NONE',  ( -1.507330767849605069, 8.672482115169964700, -2.545833800658952484 ) ) ;
#68189 = CARTESIAN_POINT ( 'NONE',  ( -3.958617665510272943, 6.601842462195195438, -1.082531754730549967 ) ) ;
#68190 = CARTESIAN_POINT ( 'NONE',  ( 7.429504990608736037, 11.61158022244479682, -0.7216878364870267237 ) ) ;
#68191 = CARTESIAN_POINT ( 'NONE',  ( 3.028127619189690201, 1.049479266250245901, 1.666313143567710542 ) ) ;
#68192 = ADVANCED_FACE ( 'NONE', ( #203110 ), #14404, .T. ) ;
#68193 = CARTESIAN_POINT ( 'NONE',  ( 1.998837940877351116, -2.080155006269391205, -0.4107514010402503746 ) ) ;
#68194 = CARTESIAN_POINT ( 'NONE',  ( -5.229694566569281555, 7.124396299129368337, 1.599625672291267398 ) ) ;
#68195 = CARTESIAN_POINT ( 'NONE',  ( -10.49167095263961613, 5.343775707538777731, -5.730694126968513658 ) ) ;
#68196 = CARTESIAN_POINT ( 'NONE',  ( 6.727182134110222478, 7.629137130509071163, 2.789055895399249252 ) ) ;
#68197 = CARTESIAN_POINT ( 'NONE',  ( 6.123007039855313138, -2.064672272812938747, 0.7349105657750015785 ) ) ;
#68198 = DIRECTION ( 'NONE',  ( 0.000000000000000000, -0.000000000000000000, 1.000000000000000000 ) ) ;
#68199 = CARTESIAN_POINT ( 'NONE',  ( 3.750929837476246753, -1.575545889128293853, 1.108190883620339795 ) ) ;
#68200 = CARTESIAN_POINT ( 'NONE',  ( -7.965578943228732278, 9.251929174310385307, -1.199719254218446718 ) ) ;
#68201 = EDGE_CURVE ( 'NONE', #53040, #12133, #155503, .T. ) ;
#68202 = CARTESIAN_POINT ( 'NONE',  ( -0.3282377607281385390, 2.363835450998165388, 1.224999999999973221 ) ) ;
#68203 = CARTESIAN_POINT ( 'NONE',  ( 0.5048604690408053930, -0.7474223562033956991, -2.076596198196341003 ) ) ;
#68204 = SPHERICAL_SURFACE ( 'NONE', #141222, 9.500000000000001776 ) ;
#68205 = EDGE_LOOP ( 'NONE', ( #147491, #142626, #170758, #105531 ) ) ;
#68206 = CARTESIAN_POINT ( 'NONE',  ( 3.834746474454188013E-15, 10.59375000068279604, 1.500000000000001554 ) ) ;
#68207 = CARTESIAN_POINT ( 'NONE',  ( 5.875830846898042914, -1.922239612846994294, 0.4278824943488717114 ) ) ;
#68208 = CARTESIAN_POINT ( 'NONE',  ( 0.7845916355662507780, 1.712027273464492350, -0.9168598982515554496 ) ) ;
#68209 = VECTOR ( 'NONE', #90927, 1000.000000000000000 ) ;
#68210 = CARTESIAN_POINT ( 'NONE',  ( 6.239697403921985241, -2.179564881273305943, -0.7296402976008103947 ) ) ;
#68212 = CARTESIAN_POINT ( 'NONE',  ( 4.363987150452108388, -1.856190122274929077, 0.1334137851533196695 ) ) ;
#68211 = CARTESIAN_POINT ( 'NONE',  ( -5.772739544368596043, 9.956889578397179363, -0.7998128361456362523 ) ) ;
#68214 = CARTESIAN_POINT ( 'NONE',  ( 6.713222337422018349, 7.861122810861019161, -1.199719254218452047 ) ) ;
#68213 = B_SPLINE_CURVE_WITH_KNOTS ( 'NONE', 3,
 ( #36831, #118162, #184147, #102914, #20575, #86659 ),
 .UNSPECIFIED., .F., .F.,
 ( 4, 2, 4 ),
 ( 0.000000000000000000, 0.0003172254002810694388, 0.0006344508005621388776 ),
 .UNSPECIFIED. ) ;
#68215 = CARTESIAN_POINT ( 'NONE',  ( 0.000000000000000000, 12.30000000000000071, 0.000000000000000000 ) ) ;
#68216 = FACE_OUTER_BOUND ( 'NONE', #97335, .T. ) ;
#68217 = CARTESIAN_POINT ( 'NONE',  ( -4.855791571988752331, 8.816840600628864877, 0.7998128361456481317 ) ) ;
#68218 = CARTESIAN_POINT ( 'NONE',  ( -3.299093274330711978, -0.9061123214685398164, 0.2492867766378724925 ) ) ;
#68219 = CARTESIAN_POINT ( 'NONE',  ( -0.1290005225502675879, -0.006633637972621592160, -2.173875058097324064 ) ) ;
#68220 = CARTESIAN_POINT ( 'NONE',  ( 5.016153647376205171, 6.875265226737464985, 1.443375672974062551 ) ) ;
#68221 = ORIENTED_EDGE ( 'NONE', *, *, #184032, .T. ) ;
#68222 = DIRECTION ( 'NONE',  ( -0.6483454320283789096, 0.000000000000000000, 0.7613463080411795314 ) ) ;
#68223 = DIRECTION ( 'NONE',  ( 0.000000000000000000, 0.000000000000000000, -1.000000000000000000 ) ) ;
#68224 = CARTESIAN_POINT ( 'NONE',  ( 0.2580658466875830337, 0.6954254843183353962, 1.688255465954719536 ) ) ;
#68225 = CARTESIAN_POINT ( 'NONE',  ( -3.276266675996675204, 6.974061555304760240, -0.7998128361456281477 ) ) ;
#68226 = CARTESIAN_POINT ( 'NONE',  ( 2.197566421822871874, 1.549772363009613407, 0.7782106121714903457 ) ) ;
#68227 = SURFACE_STYLE_USAGE ( .BOTH. , #119196 ) ;
#68228 = CARTESIAN_POINT ( 'NONE',  ( 6.509000000000034092, 7.052765612591089806, 2.598154238703707541 ) ) ;
#68229 = CARTESIAN_POINT ( 'NONE',  ( 0.1176308287326099516, -1.889623933557175617, 0.3742946393059803367 ) ) ;
#68230 = CARTESIAN_POINT ( 'NONE',  ( 3.502741298630154709, 0.4721981695934416856, 1.903977903881831191 ) ) ;
#68231 = CARTESIAN_POINT ( 'NONE',  ( -3.838364070418780027, 7.492192144726518954, 0.0001517565043702621237 ) ) ;
#68232 = CARTESIAN_POINT ( 'NONE',  ( -8.208571938070008400, 11.66408546346865016, -1.199719254218446718 ) ) ;
#68233 = CARTESIAN_POINT ( 'NONE',  ( 6.636879889089462026, 7.701780277814560982, -1.199719254218446718 ) ) ;
#68234 = CARTESIAN_POINT ( 'NONE',  ( 5.162787349232583090, 0.6159572760087471677, 2.029033592890214788 ) ) ;
#68235 = CARTESIAN_POINT ( 'NONE',  ( 5.494797395288433250, 9.632623737803665875, 0.000000000000000000 ) ) ;
#68236 = CARTESIAN_POINT ( 'NONE',  ( -8.971744963941075568, 11.49012176272984931, 1.599625672291269396 ) ) ;
#68237 = CARTESIAN_POINT ( 'NONE',  ( 3.204029340230400091, 0.7494766052340908757, -1.929994576353490032 ) ) ;
#68239 = CARTESIAN_POINT ( 'NONE',  ( 1.364683531249986537, 0.1760416670080860446, 0.7879004041258500513 ) ) ;
#68238 = CARTESIAN_POINT ( 'NONE',  ( -11.97929049433705551, 11.29999999999999893, 0.7046979865771804130 ) ) ;
#68241 = ORIENTED_EDGE ( 'NONE', *, *, #162949, .F. ) ;
#68240 = CARTESIAN_POINT ( 'NONE',  ( 4.477308758892056595, -1.984000869926884736, -0.9990560778978144763 ) ) ;
#68242 = CARTESIAN_POINT ( 'NONE',  ( 2.936492027000091376, -1.880918663215241926, -1.321213444053377373 ) ) ;
#68243 = CARTESIAN_POINT ( 'NONE',  ( 7.293923454472069245, 11.45340176361870199, 0.7216878364870438212 ) ) ;
#68245 = CARTESIAN_POINT ( 'NONE',  ( -1.642778471874998480, -2.851041666188706802, 2.845375778867863303 ) ) ;
#68244 = CARTESIAN_POINT ( 'NONE',  ( 5.994113311017540191, 9.046863725278862844, -1.082531754730548412 ) ) ;
#68246 = B_SPLINE_CURVE_WITH_KNOTS ( 'NONE', 3,
 ( #183344, #1368, #85849, #117347, #67430, #133573, #34948, #150868, #52287, #151926 ),
 .UNSPECIFIED., .F., .F.,
 ( 4, 2, 2, 2, 4 ),
 ( 1.563658610346539661E-18, 0.0003961377057362423597, 0.0007922754114724830932, 0.001188413117208723989, 0.001584550822944964668 ),
 .UNSPECIFIED. ) ;
#68247 = FILL_AREA_STYLE_COLOUR ( '', #133929 ) ;
#68248 = CARTESIAN_POINT ( 'NONE',  ( -10.79163161203180543, 4.451778906049931095, 5.251089395658656400 ) ) ;
#68249 = ORIENTED_EDGE ( 'NONE', *, *, #108709, .F. ) ;
#68250 = DIRECTION ( 'NONE',  ( 0.000000000000000000, 1.000000000000000000, 0.000000000000000000 ) ) ;
#68251 = CARTESIAN_POINT ( 'NONE',  ( 4.289254230599209627, -0.005406649120142519548, -1.912571728590661380 ) ) ;
#68252 = DIRECTION ( 'NONE',  ( 0.000000000000000000, 0.000000000000000000, 1.000000000000000000 ) ) ;
#68253 = CARTESIAN_POINT ( 'NONE',  ( 5.561458258421018819, 0.3325557151471290052, -1.692213012293216190 ) ) ;
#68254 = CARTESIAN_POINT ( 'NONE',  ( 2.975796278104339887, -0.8128168404246680634, 1.845627246706407432 ) ) ;
#68255 = CARTESIAN_POINT ( 'NONE',  ( 5.274211419651455124, 2.028235465341983623, -1.081840468886515305 ) ) ;
#68256 = LINE ( 'NONE', #53094, #46063 ) ;
#68257 = CARTESIAN_POINT ( 'NONE',  ( 6.674446291637649686, -1.297315479741867117, 1.659578660624160706 ) ) ;
#68258 = CARTESIAN_POINT ( 'NONE',  ( -4.936577329151611515, 7.813071746435248599, 1.082531754730549967 ) ) ;
#68259 = ORIENTED_EDGE ( 'NONE', *, *, #173988, .F. ) ;
#68260 = CARTESIAN_POINT ( 'NONE',  ( 5.940640833738206616, 0.3468769465994473444, 1.735210755170372376 ) ) ;
#68262 = CARTESIAN_POINT ( 'NONE',  ( 1.764052804016162268, 1.181211026566388211, 1.964360346841328209 ) ) ;
#68261 = CARTESIAN_POINT ( 'NONE',  ( 4.552505719138623341, 8.533283448962240669, 0.7998128361456341429 ) ) ;
#68263 = CARTESIAN_POINT ( 'NONE',  ( 6.544863656343847147, -1.481929198830441274, -1.092355128777318107 ) ) ;
#68264 = CARTESIAN_POINT ( 'NONE',  ( -4.295235737431041478, 3.905529869957963029, -0.7998128361456221525 ) ) ;
#68265 =( NAMED_UNIT ( * ) PLANE_ANGLE_UNIT ( ) SI_UNIT ( $, .RADIAN. ) );
#68266 = CARTESIAN_POINT ( 'NONE',  ( -5.015590482412729756, 4.816220082428420923, 0.000000000000000000 ) ) ;
#68267 = CARTESIAN_POINT ( 'NONE',  ( -1.360316468750042862, -0.5572916663252566183, 0.7853790794158701516 ) ) ;
#68268 = CARTESIAN_POINT ( 'NONE',  ( -8.767665818636368513, 15.44694762192558279, 8.178568214798543679 ) ) ;
#68269 = CARTESIAN_POINT ( 'NONE',  ( 6.725056259267968350, -1.891221747171191403, -0.8428681758992571105 ) ) ;
#68270 = CARTESIAN_POINT ( 'NONE',  ( 1.675017921984035096, 1.752138005693338441, -0.9981273289914743829 ) ) ;
#68271 = STYLED_ITEM ( 'NONE', ( #40424 ), #101103 ) ;
#68272 = CARTESIAN_POINT ( 'NONE',  ( -1.402160292154681736E-14, -0.3812499993171785673, -1.732050807568870754 ) ) ;
#68273 = CARTESIAN_POINT ( 'NONE',  ( 5.760362637647353345, 0.7829873311157690141, 1.760386188003287611 ) ) ;
#68274 = CARTESIAN_POINT ( 'NONE',  ( 1.364683531250000303, 11.00520833367473550, -0.7879004041258355073 ) ) ;
#68275 = CARTESIAN_POINT ( 'NONE',  ( 1.811064542976594360, -0.5979718353220222493, -2.139333889645285147 ) ) ;
#68276 = ORIENTED_EDGE ( 'NONE', *, *, #164365, .F. ) ;
#68277 = CARTESIAN_POINT ( 'NONE',  ( -1.332267629550188046E-16, 3.900000000000000799, 2.400000000000007461 ) ) ;
#68278 = CARTESIAN_POINT ( 'NONE',  ( 3.740030321153864801, 7.357464482200652078, -0.2303333660634114821 ) ) ;
#68279 = CARTESIAN_POINT ( 'NONE',  ( 9.728138913005292210, 11.30824913904973705, -1.199719254218440723 ) ) ;
#68280 = CARTESIAN_POINT ( 'NONE',  ( -1.001543065824772872E-14, 5.243750000682815937, 1.732050807568877637 ) ) ;
#68281 = CARTESIAN_POINT ( 'NONE',  ( 3.809144859872759525, 7.350721511173911260, -0.4830196155153026472 ) ) ;
#68282 = CARTESIAN_POINT ( 'NONE',  ( 4.809955069398625938, 1.195453170786121788, -1.265177307932338513 ) ) ;
#68284 = CARTESIAN_POINT ( 'NONE',  ( 2.172246964874047670, -0.9220853831424129510, -1.731647142839589870 ) ) ;
#68283 = PRESENTATION_LAYER_ASSIGNMENT (  '', '', ( #144441 ) ) ;
#68286 = CARTESIAN_POINT ( 'NONE',  ( -6.182154858151506893, 9.195969186943299789, 1.082531754730548412 ) ) ;
#68285 = CARTESIAN_POINT ( 'NONE',  ( 2.984766373302843778, 6.633977868828633717, -0.7998128361456291469 ) ) ;
#68287 = CARTESIAN_POINT ( 'NONE',  ( -5.911504460181634002, 6.000493611234613667, 0.05175081109743372154 ) ) ;
#68288 = CARTESIAN_POINT ( 'NONE',  ( -3.474999999999997868, -2.027083332377417335, 2.006292185433951047 ) ) ;
#68289 = CARTESIAN_POINT ( 'NONE',  ( 1.328664801108740523, -1.309985447229580213, 1.593267124675311841 ) ) ;
#68290 = CARTESIAN_POINT ( 'NONE',  ( -7.182068686937172153, 9.402166106225269715, 1.599625672291283607 ) ) ;
#68291 = CARTESIAN_POINT ( 'NONE',  ( -3.890826896997578999, 7.483122446565064756, 0.7216878364870317197 ) ) ;
#68292 = CARTESIAN_POINT ( 'NONE',  ( 1.305971919559431704, -0.5478059591418303897, 2.195072679011981442 ) ) ;
#68293 = ORIENTED_EDGE ( 'NONE', *, *, #93285, .F. ) ;
#68294 = CARTESIAN_POINT ( 'NONE',  ( -0.7500000000000006661, -0.1104166659838465292, -1.299038105676652011 ) ) ;
#68295 = CARTESIAN_POINT ( 'NONE',  ( 2.495189509527053762, 1.443206194050347557, 1.189963633554675937 ) ) ;
#68296 = CARTESIAN_POINT ( 'NONE',  ( 1.054805789555151696, -1.101345310128332367, 1.339526040370845772 ) ) ;
#68297 = CARTESIAN_POINT ( 'NONE',  ( 5.056268342064010213, -1.587557771011731678, 1.511049258477934032 ) ) ;
#68298 = CARTESIAN_POINT ( 'NONE',  ( 5.473738792520003393, 2.225791634824420218, -0.6087584347118053518 ) ) ;
#68299 = CARTESIAN_POINT ( 'NONE',  ( 1.762645127485995555, -1.458140857472267626, 1.456663342728149901 ) ) ;
#68300 = CARTESIAN_POINT ( 'NONE',  ( 3.081904124835439074, -1.913310220277367080, -0.3314154666464886323 ) ) ;
#68301 = AXIS2_PLACEMENT_3D ( 'NONE', #103734, #54979, #173010 ) ;
#68302 = CARTESIAN_POINT ( 'NONE',  ( -3.999292125906916073, 5.688926785023260102, 1.443375672974064550 ) ) ;
#68303 = CARTESIAN_POINT ( 'NONE',  ( 5.694569522353671864, -0.4537686991618711807, -1.814561337198366653 ) ) ;
#68304 = CARTESIAN_POINT ( 'NONE',  ( 1.968750000000001332, 0.7852924748298835134, -1.895863743164130755 ) ) ;
#68305 = EDGE_CURVE ( 'NONE', #209617, #93151, #210758, .T. ) ;
#68306 = CARTESIAN_POINT ( 'NONE',  ( 0.7080714767514932895, 13.29905055995279106, 1.258874868610346809 ) ) ;
#68307 = CARTESIAN_POINT ( 'NONE',  ( 6.890000000000050306, -0.002781820520068867264, 1.999840353888074240 ) ) ;
#68308 = CARTESIAN_POINT ( 'NONE',  ( 3.933273961740296087, 6.642551151122080277, 1.082531754730549078 ) ) ;
#68309 = CARTESIAN_POINT ( 'NONE',  ( 0.6801582343749970061, 0.8072916670080754198, -1.178068619123858962 ) ) ;
#68310 = CARTESIAN_POINT ( 'NONE',  ( 4.447888798048591497, -1.802416534049579910, -0.9041112711936499791 ) ) ;
#68311 = CARTESIAN_POINT ( 'NONE',  ( -3.673896439178936824, 5.309298483840612093, 1.443375672974064550 ) ) ;
#68312 = CARTESIAN_POINT ( 'NONE',  ( 7.747594715205354809, 11.12627870345989756, -1.199719254218446718 ) ) ;
#68313 = CARTESIAN_POINT ( 'NONE',  ( 3.715816618597135523, 6.492813934075403637, -1.199719254218453823 ) ) ;
#68315 = DIRECTION ( 'NONE',  ( 1.039099362110107450E-15, 1.000000000000000000, -4.583713267641621330E-32 ) ) ;
#68314 = CARTESIAN_POINT ( 'NONE',  ( 2.191784710619415044, -0.7813054520266484726, 1.650194661559079456 ) ) ;
#68316 = CARTESIAN_POINT ( 'NONE',  ( -3.935609729716867289, 7.813571461303467913, 0.7998128361456352531 ) ) ;
#68317 = DIRECTION ( 'NONE',  ( 0.000000000000000000, 0.000000000000000000, -1.000000000000000000 ) ) ;
#68318 = CARTESIAN_POINT ( 'NONE',  ( -9.348561386651960348, 4.000000000000000888, 7.001914024036569373 ) ) ;
#68319 = ORIENTED_EDGE ( 'NONE', *, *, #32090, .T. ) ;
#68320 = CARTESIAN_POINT ( 'NONE',  ( -4.624739795592931912, 8.409630504918133909, -0.7216878364870338292 ) ) ;
#68321 = CARTESIAN_POINT ( 'NONE',  ( -6.773846765317318663, -7.246166700180828535, 6.773846765317342644 ) ) ;
#68322 = CARTESIAN_POINT ( 'NONE',  ( -8.941766003412679353, 10.39081407785832845, -1.199719254218446718 ) ) ;
#68323 = CARTESIAN_POINT ( 'NONE',  ( 5.883464967995201356, 0.1463045851861736191, -2.014419601194089804 ) ) ;
#68325 = ORIENTED_EDGE ( 'NONE', *, *, #39143, .T. ) ;
#68324 = CARTESIAN_POINT ( 'NONE',  ( 0.1707708301344288138, 0.8156354886642532831, 1.957547177562010354 ) ) ;
#68326 = CARTESIAN_POINT ( 'NONE',  ( -7.259464905474441565, 7.434073576000447048, -0.7998128361456362523 ) ) ;
#68327 = CARTESIAN_POINT ( 'NONE',  ( 3.669453130792974971, 7.432779085900453886, 1.040834085586084257E-14 ) ) ;
#68328 = CARTESIAN_POINT ( 'NONE',  ( 5.049710947255391602, 0.6486796242286404501, -1.956199288699921768 ) ) ;
#68329 = CARTESIAN_POINT ( 'NONE',  ( 4.975232503164924935, -2.001511053420693020, -0.2440319332882301961 ) ) ;
#68330 = VERTEX_POINT ( 'NONE', #34917 ) ;
#68331 = VERTEX_POINT ( 'NONE', #88761 ) ;
#68332 = CARTESIAN_POINT ( 'NONE',  ( 2.913866314233864774, 6.444514562149673331, 0.4333858203510139173 ) ) ;
#68333 = CARTESIAN_POINT ( 'NONE',  ( 7.065207446497155708, 9.336104335703744539, 0.000000000000000000 ) ) ;
#68335 = ORIENTED_EDGE ( 'NONE', *, *, #32247, .F. ) ;
#68334 = CARTESIAN_POINT ( 'NONE',  ( -4.471156797456668386, 8.438376373666578445, -0.7998128361456362523 ) ) ;
#68336 = CARTESIAN_POINT ( 'NONE',  ( 4.817101577040221905, 8.228953320636518853, 0.8951067572735508238 ) ) ;
#68337 = CARTESIAN_POINT ( 'NONE',  ( 4.727888646976695419, -1.799647678597478206, -0.9090046787488814672 ) ) ;
#68338 = CARTESIAN_POINT ( 'NONE',  ( 4.540845788227630742, -1.424921066559198257, -1.165926479108070346 ) ) ;
#68339 = CARTESIAN_POINT ( 'NONE',  ( 9.617648866954018771, -9.063431457505044975, -0.6035590660249217088 ) ) ;
#68340 = CARTESIAN_POINT ( 'NONE',  ( 1.752963477315866658, 0.7269187894614470569, 2.190284518487267906 ) ) ;
#68341 = CARTESIAN_POINT ( 'NONE',  ( 5.643937085038755797, 9.806620042512378177, -0.7998128361456481317 ) ) ;
#68342 = CARTESIAN_POINT ( 'NONE',  ( 5.272814564875167420, -2.033366364591123521, -0.7337546567489708904 ) ) ;
#68343 = CARTESIAN_POINT ( 'NONE',  ( 8.880754312151170282, 10.31963377138658089, 1.199719254218453823 ) ) ;
#68344 = CARTESIAN_POINT ( 'NONE',  ( 0.3275467377269140057, 0.9974989819340736030, -1.666164454441501297 ) ) ;
#68345 = CARTESIAN_POINT ( 'NONE',  ( -3.927058049452637700, 7.733318157670055371, -0.7998128361456281477 ) ) ;
#68346 = EDGE_CURVE ( 'NONE', #61789, #173182, #187304, .T. ) ;
#68347 = CARTESIAN_POINT ( 'NONE',  ( 11.86145016429273191, 10.09412123665269689, 1.099999999999996758 ) ) ;
#68348 = CARTESIAN_POINT ( 'NONE',  ( -3.980200614063634568, 6.801261928786307642, 1.199719254218452935 ) ) ;
#68349 = CARTESIAN_POINT ( 'NONE',  ( 3.397188523315307407, 1.473948685399184333, 1.151750840393983344 ) ) ;
#68352 = CARTESIAN_POINT ( 'NONE',  ( -7.110325215724114578, 7.260077271291732082, 0.000000000000000000 ) ) ;
#68351 = CARTESIAN_POINT ( 'NONE',  ( -1.402160292154681736E-14, -0.5062499993171791779, 1.732050807568877637 ) ) ;
#68350 = CARTESIAN_POINT ( 'NONE',  ( 0.1406777020166137260, 1.830675540527426648, 0.5531436448603862521 ) ) ;
#68353 = CARTESIAN_POINT ( 'NONE',  ( 2.332911791115964473, 2.140974936812658935, 0.5348262304398290201 ) ) ;
#68354 = CARTESIAN_POINT ( 'NONE',  ( 11.07790593930098311, 12.30000000000000071, 0.6999999999999992895 ) ) ;
#68355 = CARTESIAN_POINT ( 'NONE',  ( 4.355193658487811703, 6.104145239700998538, -1.599625672291255185 ) ) ;
#68356 = DIRECTION ( 'NONE',  ( 0.000000000000000000, 0.000000000000000000, -1.000000000000000000 ) ) ;
#68357 = CARTESIAN_POINT ( 'NONE',  ( -4.111146893441842920, 5.819424013814012753, 1.599625672291267398 ) ) ;
#68358 = CARTESIAN_POINT ( 'NONE',  ( -8.054952659850432184, 8.570068656013202002, 0.000000000000000000 ) ) ;
#68359 = CARTESIAN_POINT ( 'NONE',  ( 0.3507686748964663481, -1.586079953665324060, 1.170567870040557290 ) ) ;
#68360 = CARTESIAN_POINT ( 'NONE',  ( 0.2007804849885147513, -2.307177064702860214, -0.05170730859792996986 ) ) ;
#68361 = CARTESIAN_POINT ( 'NONE',  ( 1.012071980069819910, 1.959787197952606252, -0.09269708818125664551 ) ) ;
#68362 = CARTESIAN_POINT ( 'NONE',  ( 3.784078317859154605, -1.224626257592566159, -1.659553996539532283 ) ) ;
#68363 = CARTESIAN_POINT ( 'NONE',  ( 5.558479791922850133, 6.547609847740540445, -1.082531754730542195 ) ) ;
#68364 = CARTESIAN_POINT ( 'NONE',  ( 7.018280793729500644, 8.217024343219755167, -1.199719254218452047 ) ) ;
#68365 = ORIENTED_EDGE ( 'NONE', *, *, #109904, .F. ) ;
#68366 =( BOUNDED_SURFACE ( )  B_SPLINE_SURFACE ( 3, 2, ( 
 ( #146787, #27667, #144665 ),
 ( #126320, #160878, #163017 ),
 ( #62307, #12472, #11404 ),
 ( #15665, #93762, #192281 ) ),
 .UNSPECIFIED., .F., .F., .T. ) 
 B_SPLINE_SURFACE_WITH_KNOTS ( ( 4, 4 ),
 ( 3, 3 ),
 ( 0.005239860189960162014, 0.008266248133684695604 ),
 ( 0.000000000000000000, 1.000000000000000000 ),
 .UNSPECIFIED. ) 
 GEOMETRIC_REPRESENTATION_ITEM ( )  RATIONAL_B_SPLINE_SURFACE ( (
 ( 1.000000000000000000, 0.7187737999613659223, 1.000000000000000000),
 ( 1.000000000000000000, 0.7186585579881040742, 1.000000000000000000),
 ( 1.000000000000000000, 0.7185467277397524777, 1.000000000000000000),
 ( 1.000000000000000000, 0.7184380228464086748, 1.000000000000000000) ) ) 
 REPRESENTATION_ITEM ( '' )  SURFACE ( )  );
#68367 = CARTESIAN_POINT ( 'NONE',  ( 7.985389288324691748, 10.33937347451072775, -1.443375672974058777 ) ) ;
#68368 = CARTESIAN_POINT ( 'NONE',  ( -1.364683531249997417, 5.071875000341417916, 1.214306433183764966E-14 ) ) ;
#68369 = CARTESIAN_POINT ( 'NONE',  ( -10.85972809853354093, 4.659267788818126199, -5.106963847164690762 ) ) ;
#68370 = CARTESIAN_POINT ( 'NONE',  ( 4.677199806590210507, 4.559080650551097236, -0.7216878364870197293 ) ) ;
#68371 = CARTESIAN_POINT ( 'NONE',  ( 6.391115334191724173, 0.2064332055253786102, 2.161336459811058042 ) ) ;
#68373 = CARTESIAN_POINT ( 'NONE',  ( 6.181194517112824194, 1.274813594131599226, 1.328792456347933637 ) ) ;
#68372 = CARTESIAN_POINT ( 'NONE',  ( 0.000000000000000000, 13.49999999999999822, -0.6500000000000000222 ) ) ;
#68374 = CARTESIAN_POINT ( 'NONE',  ( 5.329058858627603534, 6.340665403613130913, -1.104591990443883454 ) ) ;
#68375 = CARTESIAN_POINT ( 'NONE',  ( -11.91294103507081026, 12.48539910043594503, -1.446263142085586262 ) ) ;
#68376 = CARTESIAN_POINT ( 'NONE',  ( 0.9306671693925671063, 0.1315677519515070781, 1.865966016356377821 ) ) ;
#68377 = CARTESIAN_POINT ( 'NONE',  ( -6.104320841615721527, 6.016881168963393200, -0.3405398961462170471 ) ) ;
#68378 = CARTESIAN_POINT ( 'NONE',  ( 1.249999999999961142, 8.500000000000000000, -10.85702537530424472 ) ) ;
#68379 = EDGE_CURVE ( 'NONE', #38381, #26620, #149763, .T. ) ;
#68380 = CARTESIAN_POINT ( 'NONE',  ( 6.328358748234019338, 6.951510624437585939, -0.8854765018257749754 ) ) ;
#68381 = CARTESIAN_POINT ( 'NONE',  ( 1.364683531249988535, 4.717708333674756283, -0.7879004041258300672 ) ) ;
#68382 = CARTESIAN_POINT ( 'NONE',  ( 0.7153071762652126742, 1.563590412251715911, 1.100639817434710954 ) ) ;
#68383 = CARTESIAN_POINT ( 'NONE',  ( 2.764225215535959457, -1.222102382295175760, 1.280393980213704763 ) ) ;
#68385 = CARTESIAN_POINT ( 'NONE',  ( 0.1879522776407696050, 1.101030317643518330, 1.563299796079109072 ) ) ;
#68384 = VECTOR ( 'NONE', #89043, 1000.000000000000000 ) ;
#68387 = CARTESIAN_POINT ( 'NONE',  ( 4.780823714695519477, 1.590225366507077354, -1.067722475238532365 ) ) ;
#68386 = CARTESIAN_POINT ( 'NONE',  ( 7.503508839934897701, -6.893137084989714225, 8.043940816608046163 ) ) ;
#68388 = CARTESIAN_POINT ( 'NONE',  ( -2.974588534184118949, 6.690032103375380679, 0.07232793336444105770 ) ) ;
#68389 = CARTESIAN_POINT ( 'NONE',  ( 5.019951571474082996, 1.948400538373602497, -0.2868881896359152806 ) ) ;
#68390 = CARTESIAN_POINT ( 'NONE',  ( 0.4750491441844888474, -1.531729482103380224, 1.466773057065169361 ) ) ;
#68391 = DIRECTION ( 'NONE',  ( 0.000000000000000000, -1.000000000000000000, 0.000000000000000000 ) ) ;
#68392 = CARTESIAN_POINT ( 'NONE',  ( 3.924554409752772699, 1.776107677202539925, 0.5873546117282567591 ) ) ;
#68394 = ORIENTED_EDGE ( 'NONE', *, *, #205051, .F. ) ;
#68393 = CARTESIAN_POINT ( 'NONE',  ( 0.5920835508136900183, -1.811502216344462735, -0.2265648652611390590 ) ) ;
#68396 = DIRECTION ( 'NONE',  ( -0.000000000000000000, -1.000000000000000000, -0.000000000000000000 ) ) ;
#68395 = CARTESIAN_POINT ( 'NONE',  ( 3.668774463136436736, -1.482526648764719734, 1.634931011441637771 ) ) ;
#68397 = CARTESIAN_POINT ( 'NONE',  ( -0.6823417656249969321, 5.030208333674755394, -1.181850606188749264 ) ) ;
#68398 = CARTESIAN_POINT ( 'NONE',  ( 0.7134213396373456639, -1.741552128810987421, -1.105017490550715742 ) ) ;
#68399 = CARTESIAN_POINT ( 'NONE',  ( 6.856673000209174695, 9.022537805042615489, 1.599625672291281386 ) ) ;
#68400 = CARTESIAN_POINT ( 'NONE',  ( -9.515124878692420296, 9.995400534762978850, 1.040834085586084257E-14 ) ) ;
#68401 = CARTESIAN_POINT ( 'NONE',  ( -8.581532217057265655, 3.975933801733725570, -7.726846314510518177 ) ) ;
#68402 = CARTESIAN_POINT ( 'NONE',  ( 0.000000000000000000, 8.500000000000000000, 0.000000000000000000 ) ) ;
#68403 = CARTESIAN_POINT ( 'NONE',  ( -1.499999999999960476, 7.193113254731351880, 10.88798745763944176 ) ) ;
#68404 = AXIS2_PLACEMENT_3D ( 'NONE', #140817, #206830, #58464 ) ;
#68405 = ORIENTED_EDGE ( 'NONE', *, *, #201770, .F. ) ;
#68406 = CARTESIAN_POINT ( 'NONE',  ( 3.402844027952243167, 0.5003511028610057032, 2.008882729757965890 ) ) ;
#68407 = CARTESIAN_POINT ( 'NONE',  ( 0.7499999999999920064, 4.733333333333352932, 1.299038105676669330 ) ) ;
#68408 = CARTESIAN_POINT ( 'NONE',  ( 1.335488691732108046, -1.954760257947166568, 0.9229496955955732718 ) ) ;
#68409 = CARTESIAN_POINT ( 'NONE',  ( -6.602617837901656017, 6.766230214585198688, 0.2136612715164920018 ) ) ;
#68410 = CARTESIAN_POINT ( 'NONE',  ( 0.7506560300556723853, 1.990167900158135605, 0.3429568431373567483 ) ) ;
#68411 = DIRECTION ( 'NONE',  ( -0.000000000000000000, 1.000000000000000000, -0.000000000000000000 ) ) ;
#68412 = ORIENTED_EDGE ( 'NONE', *, *, #162518, .F. ) ;
#68413 = EDGE_CURVE ( 'NONE', #72363, #166249, #169409, .T. ) ;
#68415 = CARTESIAN_POINT ( 'NONE',  ( 8.649738815838679429, 10.15407870897571563, -1.082531754730543083 ) ) ;
#68414 = CARTESIAN_POINT ( 'NONE',  ( -3.474999999999998312, -2.420833333333334725, 2.006292185433951047 ) ) ;
#68416 = CARTESIAN_POINT ( 'NONE',  ( 6.503279807981922289, 1.993766592317405273, 0.2985777636397292101 ) ) ;
#68417 = CARTESIAN_POINT ( 'NONE',  ( 0.04025042243083893495, 0.7762349914572730381, 1.861342399428978389 ) ) ;
#68418 = DIRECTION ( 'NONE',  ( 0.7592566023653005702, -0.6507913734559639396, 0.000000000000000000 ) ) ;
#68419 = CARTESIAN_POINT ( 'NONE',  ( 5.478137895480934105, -2.137967713159651506, -0.4810252310911074525 ) ) ;
#68420 = CARTESIAN_POINT ( 'NONE',  ( -1.201851678989727383E-14, 2.868750000682821266, -1.732050807568863648 ) ) ;
#68421 = CARTESIAN_POINT ( 'NONE',  ( 3.093911922779784440, 1.216618333484908998, 1.475457842794763996 ) ) ;
#68422 = CARTESIAN_POINT ( 'NONE',  ( -5.362413449404877852, 6.214902764849178141, -1.199719254218446718 ) ) ;
#68423 = CARTESIAN_POINT ( 'NONE',  ( 4.216222583725566686, 4.981643104843690217, -1.082531754730548412 ) ) ;
#68425 = CARTESIAN_POINT ( 'NONE',  ( 1.599232692168949699, -0.2440074622011619843, 2.001515180871694888 ) ) ;
#68424 = CARTESIAN_POINT ( 'NONE',  ( -8.636180661780651135, 13.01936850547871138, -0.7216878364870257245 ) ) ;
#68426 = CARTESIAN_POINT ( 'NONE',  ( -0.6823417656250003738, 10.71354166700806765, 1.181850606188754593 ) ) ;
#68428 = CARTESIAN_POINT ( 'NONE',  ( -6.140917232347002042, 6.129101290685087911, -0.7998128361456362523 ) ) ;
#68427 = CARTESIAN_POINT ( 'NONE',  ( 0.09973926083830295108, -0.6030689337076476919, 2.211586693686658389 ) ) ;
#68429 = CARTESIAN_POINT ( 'NONE',  ( 3.610098185430905104, -0.6985691267104906510, -1.577150584296799440 ) ) ;
#68430 = CARTESIAN_POINT ( 'NONE',  ( 0.1394461523057501928, 1.435241935670927171, -1.984817279021661829 ) ) ;
#68431 = CARTESIAN_POINT ( 'NONE',  ( 2.510230996824538430, 6.080353262937265413, 0.000000000000000000 ) ) ;
#68432 = CARTESIAN_POINT ( 'NONE',  ( -1.244150428498999705, 2.928773246564666977, -0.7749999999999988010 ) ) ;
#68433 = CARTESIAN_POINT ( 'NONE',  ( 0.8011316787140990714, -1.684513426579350659, 1.005393624328714264 ) ) ;
#68434 = ADVANCED_FACE ( 'NONE', ( #83871 ), #68173, .T. ) ;
#68435 = CARTESIAN_POINT ( 'NONE',  ( 9.508009452561562824, 4.000000000000000888, 7.612500000000001599 ) ) ;
#68436 = CARTESIAN_POINT ( 'NONE',  ( 5.030238685870051185, 5.827365540725222282, -1.199719254218452047 ) ) ;
#68437 = CARTESIAN_POINT ( 'NONE',  ( 0.1751657365761521701, 1.361037063587458906, -2.300812366989886559 ) ) ;
#68438 = EDGE_LOOP ( 'NONE', ( #176637, #191786, #32731, #211080 ) ) ;
#68439 = VECTOR ( 'NONE', #142730, 1000.000000000000000 ) ;
#68440 = FACE_OUTER_BOUND ( 'NONE', #189568, .T. ) ;
#68441 = ORIENTED_EDGE ( 'NONE', *, *, #169486, .T. ) ;
#68442 = CARTESIAN_POINT ( 'NONE',  ( 3.439928307436474597, -1.081519596823855345, -1.453003583242311381 ) ) ;
#68443 = EDGE_LOOP ( 'NONE', ( #144118, #197274, #1825, #32053 ) ) ;
#68444 = CARTESIAN_POINT ( 'NONE',  ( 5.830888582329017744, 8.960397891762626799, -1.199719254218452047 ) ) ;
#68445 = CARTESIAN_POINT ( 'NONE',  ( 4.085803189671889157, 5.860132702740892263, -1.599625672291273171 ) ) ;
#68446 = CARTESIAN_POINT ( 'NONE',  ( 4.898965649768390662, -0.2269230896460339986, -1.797137895798770479 ) ) ;
#68447 = CARTESIAN_POINT ( 'NONE',  ( 5.655159470231527763, 9.611786791996525636, -0.7216878364870458196 ) ) ;
#68448 =( LENGTH_UNIT ( ) NAMED_UNIT ( * ) SI_UNIT ( .MILLI., .METRE. ) );
#68449 = CARTESIAN_POINT ( 'NONE',  ( 5.365762136054953224, 6.315268812753259020, -1.079746804988683806 ) ) ;
#68450 = AXIS2_PLACEMENT_3D ( 'NONE', #157192, #42390, #93273 ) ;
#68452 = CARTESIAN_POINT ( 'NONE',  ( 8.191097360950562845, 12.70803068775103739, -0.7998128361456352531 ) ) ;
#68451 = CARTESIAN_POINT ( 'NONE',  ( 6.197681965292040296, -1.348592564218813905, -1.282738352563756123 ) ) ;
#68453 = CARTESIAN_POINT ( 'NONE',  ( 3.269047429782430125, 1.730524700466531396, -0.8218109994902050852 ) ) ;
#68454 = CARTESIAN_POINT ( 'NONE',  ( -6.444907381559357162, -8.233136965322206180, -6.980013479859866976 ) ) ;
#68455 = CARTESIAN_POINT ( 'NONE',  ( -11.31087111570240467, 5.182330806778288057, -5.726608797552268371 ) ) ;
#68456 = CARTESIAN_POINT ( 'NONE',  ( -10.99954523395721218, -9.918132210574695407, 0.1000458187401208898 ) ) ;
#68457 = CARTESIAN_POINT ( 'NONE',  ( -15.75000000000000000, 13.39999999999998259, 1.799999999999999600 ) ) ;
#68458 = CARTESIAN_POINT ( 'NONE',  ( 5.612712406377503349, 8.531619659873665995, -1.082531754730543083 ) ) ;
#68459 = EDGE_CURVE ( 'NONE', #138893, #93013, #104906, .T. ) ;
#68460 = CARTESIAN_POINT ( 'NONE',  ( -3.358669367883384105, 4.941533567329135401, -1.599625672291262513 ) ) ;
#68461 = CARTESIAN_POINT ( 'NONE',  ( 1.042116488573753497, 0.8753402851892390091, -1.976733581976031218 ) ) ;
#68462 = CARTESIAN_POINT ( 'NONE',  ( -4.827585214917754719, 7.789877296449459365, -1.199719254218453823 ) ) ;
#68463 = CARTESIAN_POINT ( 'NONE',  ( 4.206772801990143584, 8.129928378955675328, 0.7998128361456271485 ) ) ;
#68464 = CARTESIAN_POINT ( 'NONE',  ( 1.377666516899571647, 1.084121917808708035, 1.468671923017292658 ) ) ;
#68465 = CARTESIAN_POINT ( 'NONE',  ( -3.405069135326500351, 7.124331091189553433, 1.040834085586084257E-14 ) ) ;
#68466 = EDGE_CURVE ( 'NONE', #53040, #118869, #186702, .T. ) ;
#68467 = CARTESIAN_POINT ( 'NONE',  ( 3.698116152863577977, -1.823479002399010396, -0.09026698595545472326 ) ) ;
#68468 = CARTESIAN_POINT ( 'NONE',  ( 11.15162045555251957, 9.712998552558403276, 5.837063001226317382 ) ) ;
#68469 = CARTESIAN_POINT ( 'NONE',  ( 1.916128293556786044, -1.911906470838855343, 0.05044092668918254141 ) ) ;
#68470 = CARTESIAN_POINT ( 'NONE',  ( 2.646873730718673379, -0.3338169989568114948, -1.940879108454116375 ) ) ;
#68471 = CARTESIAN_POINT ( 'NONE',  ( 4.282717048480193078, 1.733172068543160416, -0.8763712590400226654 ) ) ;
#68472 = CARTESIAN_POINT ( 'NONE',  ( -6.912678218121246942, 9.158153569265168770, 1.599625672291269396 ) ) ;
#68474 = CARTESIAN_POINT ( 'NONE',  ( 4.342108446431157454, -1.306982937058022820, -1.669832246961988176 ) ) ;
#68473 = CARTESIAN_POINT ( 'NONE',  ( 3.061108821635398769, 6.793320401875094561, -0.7998128361456362523 ) ) ;
#68475 = CARTESIAN_POINT ( 'NONE',  ( -10.50000000000000533, 13.50709944181895139, 3.599999999999998312 ) ) ;
#68476 = CARTESIAN_POINT ( 'NONE',  ( 7.886038904643079661, 12.35212915539230139, -0.7998128361456352531 ) ) ;
#68477 = CARTESIAN_POINT ( 'NONE',  ( 6.103366240126457676, 6.022929404904433071, 0.2034074856576886248 ) ) ;
#68478 = ORIENTED_EDGE ( 'NONE', *, *, #109387, .T. ) ;
#68479 = TOROIDAL_SURFACE ( 'NONE', #68935, 10.75000000000000000, 0.5000000000000007772 ) ;
#68480 = CARTESIAN_POINT ( 'NONE',  ( 5.468734858265785093, 7.473552982767158070, 1.599625672291269396 ) ) ;
#68481 = DIRECTION ( 'NONE',  ( 0.000000000000000000, 1.000000000000000000, 0.000000000000000000 ) ) ;
#68483 = CARTESIAN_POINT ( 'NONE',  ( 6.069546051295945155, 1.394081536189460069, 1.457239770841619597 ) ) ;
#68482 = CARTESIAN_POINT ( 'NONE',  ( 3.861776535121093090, 1.811678901967550326, -0.2252020330209548171 ) ) ;
#68484 = CARTESIAN_POINT ( 'NONE',  ( 10.99943592164172657, -9.900000000000005684, -0.1113975120798811613 ) ) ;
#68485 = CARTESIAN_POINT ( 'NONE',  ( -9.666600336863641729, 10.38004793587015584, 1.040834085586084257E-14 ) ) ;
#68486 = CARTESIAN_POINT ( 'NONE',  ( -5.181409149560055383, 7.856748536063159705, 1.265847179423916335 ) ) ;
#68487 = DIRECTION ( 'NONE',  ( 8.638326563840814399E-31, 0.000000000000000000, 1.000000000000000000 ) ) ;
#68488 = CARTESIAN_POINT ( 'NONE',  ( 6.121928861531041655, -1.040746078065577063, -1.554202398018275755 ) ) ;
#68489 = CARTESIAN_POINT ( 'NONE',  ( 6.751070424600909448, 9.963667031088037973, -1.199719254218441611 ) ) ;
#68490 = CARTESIAN_POINT ( 'NONE',  ( 3.668508669297173341, -1.293070320541231721, 1.428231264829373126 ) ) ;
#68491 = CARTESIAN_POINT ( 'NONE',  ( -5.057354993097396445, 5.859001232490445688, -1.199719254218446718 ) ) ;
#68492 = CIRCLE ( 'NONE', #175840, 0.5000000000000007772 ) ;
#68493 = CARTESIAN_POINT ( 'NONE',  ( 1.364683531249996529, 8.776041667008067648, 0.7879004041258405033 ) ) ;
#68494 = CARTESIAN_POINT ( 'NONE',  ( -6.261168011412601153, 6.199117522936475666, 1.040834085586084257E-14 ) ) ;
#68495 = CARTESIAN_POINT ( 'NONE',  ( 4.033714395265605823, 4.664753868353354704, -1.199719254218446718 ) ) ;
#68496 = CARTESIAN_POINT ( 'NONE',  ( -4.977251789548269301, 4.979417640660637190, 0.7216878364870257245 ) ) ;
#68497 = CARTESIAN_POINT ( 'NONE',  ( 1.652128961607162827, 1.091750937195800519, 1.813926670343589898 ) ) ;
#68498 = CARTESIAN_POINT ( 'NONE',  ( 9.738834413317897898, 10.25639499182604730, 0.000000000000000000 ) ) ;
#68499 = CARTESIAN_POINT ( 'NONE',  ( -4.053528829375205866, 3.783736749027349244, 2.445701138906847039 ) ) ;
#68500 = CARTESIAN_POINT ( 'NONE',  ( 5.875854205266583641, -2.021069926245163906, 0.4479438709683660202 ) ) ;
#68502 = CARTESIAN_POINT ( 'NONE',  ( 3.998507505471064594, 7.829874410826325182, -0.01819030738507872169 ) ) ;
#68501 = CARTESIAN_POINT ( 'NONE',  ( 1.557894219809667247, -1.301531972126177772, 1.302644501960325885 ) ) ;
#68503 = CARTESIAN_POINT ( 'NONE',  ( 5.992340707560160240, 7.053780915984068756, 1.082531754730558626 ) ) ;
#68505 = CARTESIAN_POINT ( 'NONE',  ( 0.7500000000000006661, 9.697916667349467446, -1.299038105676657340 ) ) ;
#68504 = CARTESIAN_POINT ( 'NONE',  ( 2.929970594329034395, 6.432399770110250437, -0.7216878364870338292 ) ) ;
#68506 = CARTESIAN_POINT ( 'NONE',  ( 1.465189672511356900, 0.1648890142370383061, -2.286389102023842490 ) ) ;
#68507 = DIRECTION ( 'NONE',  ( -0.7806247490453480653, -4.396526966619892032E-05, 0.6249999993959538536 ) ) ;
#68508 = CARTESIAN_POINT ( 'NONE',  ( 5.824156380204161820, 1.872177270857039000, 0.5156464658115608168 ) ) ;
#68509 = ORIENTED_EDGE ( 'NONE', *, *, #28884, .T. ) ;
#68510 = CARTESIAN_POINT ( 'NONE',  ( 9.042925270190638187, 9.652427024751663254, 0.7216878364870458196 ) ) ;
#68511 = CARTESIAN_POINT ( 'NONE',  ( 0.3693899063928334781, -1.702925086422102163, -1.073505336752482053 ) ) ;
#68512 = CARTESIAN_POINT ( 'NONE',  ( 6.456263137377812988, -1.236968576560823818, 1.593241027169019830 ) ) ;
#68514 = FACE_OUTER_BOUND ( 'NONE', #139958, .T. ) ;
#68513 = CARTESIAN_POINT ( 'NONE',  ( -9.338868881714763148, 9.789768538289042255, -0.7998128361456291469 ) ) ;
#68515 = CARTESIAN_POINT ( 'NONE',  ( -6.633258869711600170, 6.703499867610458018, -0.5492115505440260392 ) ) ;
#68517 = CARTESIAN_POINT ( 'NONE',  ( 1.814973546968738027, -0.2204486908502552300, 1.755991699180702748 ) ) ;
#68516 = CARTESIAN_POINT ( 'NONE',  ( 3.679701837385487284, -1.030134525132427203, 1.819138145232774839 ) ) ;
#68518 = LINE ( 'NONE', #33904, #36632 ) ;
#68520 = CARTESIAN_POINT ( 'NONE',  ( 5.173897996269102961, -1.276782452619073860, 1.903577390058891261 ) ) ;
#68519 = CARTESIAN_POINT ( 'NONE',  ( -11.86691703139814535, 7.727552885927400084, -1.800178980557079367 ) ) ;
#68521 = CARTESIAN_POINT ( 'NONE',  ( 3.767295573485733851, 0.9686143178696275946, 1.445635114442943348 ) ) ;
#68522 = CARTESIAN_POINT ( 'NONE',  ( 9.728138913005292210, 11.30824913904973705, -1.199719254218440723 ) ) ;
#68523 = CARTESIAN_POINT ( 'NONE',  ( 3.739016502318667445, 7.584212696005614873, 0.7998128361456271485 ) ) ;
#68524 = CARTESIAN_POINT ( 'NONE',  ( 3.479597601185040912, 1.566717760139114901, 0.7430284921127163766 ) ) ;
#68525 = CARTESIAN_POINT ( 'NONE',  ( 3.613895077877467443, 0.5305607931336644434, -2.105228361949755378 ) ) ;
#68526 = CARTESIAN_POINT ( 'NONE',  ( 4.334856428067313416, 6.080418470877079429, -1.599625672291256295 ) ) ;
#68527 = EDGE_CURVE ( 'NONE', #31530, #62971, #52450, .T. ) ;
#68528 = CARTESIAN_POINT ( 'NONE',  ( 4.592982591267942283, 1.756852934926198317, 0.9896879400849432074 ) ) ;
#68529 = CARTESIAN_POINT ( 'NONE',  ( 0.9062500000000004441, 1.895863743164069470, -0.7852924748300356139 ) ) ;
#68530 = CARTESIAN_POINT ( 'NONE',  ( 0.7499999999999902300, 3.847916667349481123, -1.299038105676658228 ) ) ;
#68531 = CARTESIAN_POINT ( 'NONE',  ( 1.711812753757115502, -1.912122584522325086, 0.2334695860961126246 ) ) ;
#68532 = CARTESIAN_POINT ( 'NONE',  ( -1.402160292154681736E-14, 8.593750000682796042, 1.732050807568881190 ) ) ;
#68533 = CARTESIAN_POINT ( 'NONE',  ( 5.554997651100567424, 0.4332456915393156915, 2.178594967391647597 ) ) ;
#68534 = ORIENTED_EDGE ( 'NONE', *, *, #175999, .T. ) ;
#68535 = CARTESIAN_POINT ( 'NONE',  ( -0.2106854629475426177, 0.2415373081153374957, -2.031805921504933554 ) ) ;
#68536 = CARTESIAN_POINT ( 'NONE',  ( -1.402160292154681736E-14, 1.087500000000024336, -1.732050807568863648 ) ) ;
#68537 = CARTESIAN_POINT ( 'NONE',  ( 6.799577732453452761, 7.891594428405881878, -1.199719254218446718 ) ) ;
#68538 = CARTESIAN_POINT ( 'NONE',  ( 5.314433026432511475, 5.302519407033794430, 1.040834085586084257E-14 ) ) ;
#68539 = CARTESIAN_POINT ( 'NONE',  ( 3.285556943750000070, -0.9843749995220412163, 0.000000000000000000 ) ) ;
#68540 = CARTESIAN_POINT ( 'NONE',  ( 0.5225339808294949817, -2.210013125053798433, 0.2238140636349055246 ) ) ;
#68541 = CARTESIAN_POINT ( 'NONE',  ( 5.670351692713981429, -0.8806477319739226539, -1.753155087565357428 ) ) ;
#68542 = CARTESIAN_POINT ( 'NONE',  ( 7.944714827928043732, 10.29191993738131927, 1.443375672974076540 ) ) ;
#68543 = FILL_AREA_STYLE ('',( #133612 ) ) ;
#68544 = CARTESIAN_POINT ( 'NONE',  ( 6.397788901632932124, -0.7711469528366134973, 2.127058432633963658 ) ) ;
#68545 = CARTESIAN_POINT ( 'NONE',  ( 5.564695703766185275, 5.456842840674144490, 0.000000000000000000 ) ) ;
#68547 = VECTOR ( 'NONE', #207978, 1000.000000000000000 ) ;
#68546 = AXIS2_PLACEMENT_3D ( 'NONE', #79187, #45644, #198249 ) ;
#68548 = CARTESIAN_POINT ( 'NONE',  ( -3.987506576194992824, 7.666191748953863794, 0.7216878364870338292 ) ) ;
#68549 = CARTESIAN_POINT ( 'NONE',  ( 3.895030958483152173, 0.2998364479755392664, 2.040644712996171339 ) ) ;
#68550 = CARTESIAN_POINT ( 'NONE',  ( -4.904298879841297421, 6.744767997946721216, 1.599625672291267398 ) ) ;
#68551 = CARTESIAN_POINT ( 'NONE',  ( -0.7500000000000215383, 3.972916667349481123, 1.299038105676671107 ) ) ;
#68552 = CARTESIAN_POINT ( 'NONE',  ( -1.364683531250014514, 0.2385416670080863499, -0.7879004041258359514 ) ) ;
#68553 = CARTESIAN_POINT ( 'NONE',  ( 6.257094453949625823, -1.604276942902042480, -0.9616840659161307592 ) ) ;
#68554 = CARTESIAN_POINT ( 'NONE',  ( 4.307042110543488178, 1.062484115506344473, -1.370455642081182646 ) ) ;
#68555 = CARTESIAN_POINT ( 'NONE',  ( 4.229842819227870976, 1.707864474872609062, 0.3341882380870179192 ) ) ;
#68556 = CARTESIAN_POINT ( 'NONE',  ( 8.988692655735958326, 12.47026328412523988, -1.082531754730543083 ) ) ;
#68557 = CARTESIAN_POINT ( 'NONE',  ( 1.945279335750784711, -1.843959696387540204, -1.361743503316152681 ) ) ;
#68558 = CARTESIAN_POINT ( 'NONE',  ( -1.201851678989727383E-14, 4.259375000341417028, -1.575800808251660134 ) ) ;
#68559 = CARTESIAN_POINT ( 'NONE',  ( 5.548407312280490444, -1.647412313956169605, 1.287198389022710998 ) ) ;
#68560 = CARTESIAN_POINT ( 'NONE',  ( 6.685517510867199142, -0.8268063683338886527, 1.755141085440144355 ) ) ;
#68561 = CARTESIAN_POINT ( 'NONE',  ( -6.735631571019096932E-15, -9.954378579146949235, 10.91970693179565544 ) ) ;
#68562 = CARTESIAN_POINT ( 'NONE',  ( 1.951796282902381163, -1.844710420878793444, -0.8146254186931353169 ) ) ;
#68563 = CARTESIAN_POINT ( 'NONE',  ( 0.6565081633774123571, -1.584678946828571133, 1.513927167823600595 ) ) ;
#68564 = CARTESIAN_POINT ( 'NONE',  ( 8.830611090300100940, 13.64794954589311082, -9.281763806552183027 ) ) ;
#68565 = CARTESIAN_POINT ( 'NONE',  ( -8.538937818508475885, 8.856515631215026829, 1.040834085586084257E-14 ) ) ;
#68566 = CARTESIAN_POINT ( 'NONE',  ( 4.469384193999260901, 8.366031992974468423, -0.7998128361456231517 ) ) ;
#68567 = CARTESIAN_POINT ( 'NONE',  ( 2.596466591541984226, -1.087938976695131066, 1.819974527870950265 ) ) ;
#68568 = CARTESIAN_POINT ( 'NONE',  ( 1.364683531249986537, -0.3447916663252443836, -0.7879004041258309554 ) ) ;
#68569 = CARTESIAN_POINT ( 'NONE',  ( 5.180226163740526246, -1.011166736308216629, 1.519887457628710248 ) ) ;
#68570 = ORIENTED_EDGE ( 'NONE', *, *, #26940, .T. ) ;
#68571 = CARTESIAN_POINT ( 'NONE',  ( -5.596483547390937119, 9.751257581923240991, 0.000000000000000000 ) ) ;
#68572 = DIRECTION ( 'NONE',  ( 1.224643483124941457E-16, 0.002327115863041261980, 0.9999972922622142324 ) ) ;
#68573 = CARTESIAN_POINT ( 'NONE',  ( -3.285556943749998737, -1.217708332855376607, 1.896917185911908499 ) ) ;
#68574 = CARTESIAN_POINT ( 'NONE',  ( -4.706651882238427120, 8.642844295920152575, 1.040834085586084257E-14 ) ) ;
#68575 = CARTESIAN_POINT ( 'NONE',  ( 2.795180614130913010, -0.1526695769738794506, -2.014101982623817566 ) ) ;
#68576 = CARTESIAN_POINT ( 'NONE',  ( 6.475609205405274515, 2.113627995098281254, -0.6344055572156809264 ) ) ;
#68577 = ADVANCED_FACE ( 'NONE', ( #135841 ), #181091, .T. ) ;
#68578 = CARTESIAN_POINT ( 'NONE',  ( 9.215791728987056786, 11.77484298861683598, -1.599625672291262513 ) ) ;
#68579 = CARTESIAN_POINT ( 'NONE',  ( 4.416758307032777608, -1.381121683685157642, 1.247472197611438016 ) ) ;
#68580 = CARTESIAN_POINT ( 'NONE',  ( 7.540305987494599016, 11.94877408538573427, -0.7998128361456291469 ) ) ;
#68581 = CARTESIAN_POINT ( 'NONE',  ( 3.208946231067535848, 6.430484326561804131, 0.7152403155292674786 ) ) ;
#68582 = ORIENTED_EDGE ( 'NONE', *, *, #138558, .F. ) ;
#68583 = CARTESIAN_POINT ( 'NONE',  ( -4.790108344329849110, 4.482881244673243337, 0.7998128361456341429 ) ) ;
#68584 = CARTESIAN_POINT ( 'NONE',  ( -6.886651960737580680, 10.12184548991413457, -1.199719254218440723 ) ) ;
#68586 = CARTESIAN_POINT ( 'NONE',  ( -4.181557753866925964, 7.584876391898649928, 0.9328056193420256603 ) ) ;
#68585 = CARTESIAN_POINT ( 'NONE',  ( -6.587282531393266360, 8.778525268082516320, 1.599625672291269396 ) ) ;
#68587 = CARTESIAN_POINT ( 'NONE',  ( -1.364683531250014514, -0.5114583329919092369, -0.7879004041258359514 ) ) ;
#68588 = CARTESIAN_POINT ( 'NONE',  ( 1.651252135258261422, -0.2480751513778757522, -1.715843305285965403 ) ) ;
#68589 = CARTESIAN_POINT ( 'NONE',  ( 1.675334203684273771, -0.9328193774022232043, 1.469000774227617434 ) ) ;
#68591 = CARTESIAN_POINT ( 'NONE',  ( 7.727784370109387346, 10.99920361756089093, -1.082531754730543083 ) ) ;
#68590 = CARTESIAN_POINT ( 'NONE',  ( 5.180430901434020186, -1.285682204016626029, 1.916193241175147666 ) ) ;
#68592 = CARTESIAN_POINT ( 'NONE',  ( -10.50659947519749693, 5.359800460605414152, -5.105385958519358169 ) ) ;
#68593 = CARTESIAN_POINT ( 'NONE',  ( 0.8607048193125128588, -1.494471031236654257, 1.419199468611084480 ) ) ;
#68594 = CARTESIAN_POINT ( 'NONE',  ( 4.320244504248938355, 8.192035688265757898, 1.040834085586084257E-14 ) ) ;
#68596 = EDGE_CURVE ( 'NONE', #94456, #32497, #163741, .T. ) ;
#68595 = CIRCLE ( 'NONE', #144735, 0.08000000000000040412 ) ;
#68597 = EDGE_CURVE ( 'NONE', #5398, #138555, #37754, .T. ) ;
#68598 = CARTESIAN_POINT ( 'NONE',  ( 6.679114621301890153, -1.074570768553984479, -2.031732957927368410 ) ) ;
#68599 = CARTESIAN_POINT ( 'NONE',  ( 6.856061878569608298E-15, 0.9375000000000238698, -1.225000000000010303 ) ) ;
#68600 = CARTESIAN_POINT ( 'NONE',  ( -6.771371375382467583, 6.864631124226471037, -0.7998128361456362523 ) ) ;
#68601 = CARTESIAN_POINT ( 'NONE',  ( 0.07499057489264608634, 0.002531239327739977750, -1.955573237620360949 ) ) ;
#68603 = CARTESIAN_POINT ( 'NONE',  ( -5.465345320084574965, 9.390336950158399532, 0.000000000000000000 ) ) ;
#68602 = CARTESIAN_POINT ( 'NONE',  ( 4.711142613322857109, 1.586760866459841379, -1.067142987418716604 ) ) ;
#68604 = CARTESIAN_POINT ( 'NONE',  ( 6.498651167236064730, -0.5841124237929047336, -2.128106146270396071 ) ) ;
#68605 = CARTESIAN_POINT ( 'NONE',  ( 0.6124999999999949374, 1.645833334016133520, 1.060881119635922243 ) ) ;
#68606 = CARTESIAN_POINT ( 'NONE',  ( -7.769310276573725638, -5.221243112839681011, -7.769310276573695440 ) ) ;
#68607 = CARTESIAN_POINT ( 'NONE',  ( 4.380693030546916944, 6.204170850428461392, 1.443375672974058777 ) ) ;
#68608 = CARTESIAN_POINT ( 'NONE',  ( -7.608060475923978494, 8.905100639113307182, 1.199719254218452047 ) ) ;
#68609 = CARTESIAN_POINT ( 'NONE',  ( 0.2408861781304712513, 1.933338575160881367, 0.5842326518414300285 ) ) ;
#68610 = CARTESIAN_POINT ( 'NONE',  ( 3.997355382689435466, 1.951332032848082099, -1.231501813138028423 ) ) ;
#68611 = CARTESIAN_POINT ( 'NONE',  ( 5.072687121480487171, 1.354251660176824856, -1.419695456575476689 ) ) ;
#68612 = CARTESIAN_POINT ( 'NONE',  ( 0.5319879461419263489, 1.124744735265088780, 1.607134405190835391 ) ) ;
#68613 = CARTESIAN_POINT ( 'NONE',  ( 8.917737905728806425, 3.447199233515649386, 8.029567276306217138 ) ) ;
#68614 = CARTESIAN_POINT ( 'NONE',  ( -9.404393214968951753, 15.50974221445264156, 7.453732458498741664 ) ) ;
#68615 = ORIENTED_EDGE ( 'NONE', *, *, #31584, .F. ) ;
#68616 = CARTESIAN_POINT ( 'NONE',  ( 0.005274918996244109745, -0.09700444455036473512, 2.115223206416060098 ) ) ;
#68618 = CARTESIAN_POINT ( 'NONE',  ( -6.997979842947967377, 11.31606025008131233, -0.7998128361456291469 ) ) ;
#68617 = CARTESIAN_POINT ( 'NONE',  ( -4.249591082879585535, 7.045274465746411252, 1.199719254218464037 ) ) ;
#68619 = CARTESIAN_POINT ( 'NONE',  ( -15.75000000000000000, 10.90000000000000036, 1.099999999999996758 ) ) ;
#68620 = CARTESIAN_POINT ( 'NONE',  ( 2.711994142844989408, 0.5828001693900261015, -2.091290491527279194 ) ) ;
#68621 = CARTESIAN_POINT ( 'NONE',  ( -0.1942909893604273797, 2.636497617442806529, 1.993158123458445230 ) ) ;
#68622 = CARTESIAN_POINT ( 'NONE',  ( 0.8617730121942971389, -1.675286201960282995, -1.300076073212981242 ) ) ;
#68623 = CARTESIAN_POINT ( 'NONE',  ( 1.499999999999987121, 1.577083334016150751, -0.8660254037844253849 ) ) ;
#68624 = CARTESIAN_POINT ( 'NONE',  ( 8.540746701604824409, 12.05162268759261224, -1.199719254218446718 ) ) ;
#68625 = CARTESIAN_POINT ( 'NONE',  ( 11.94105721237522921, 13.40000000000000036, -1.187919463087248939 ) ) ;
#68626 = CARTESIAN_POINT ( 'NONE',  ( 6.459053645710411296, 6.863086831863287607, 0.6637952124323226455 ) ) ;
#68627 = AXIS2_PLACEMENT_3D ( 'NONE', #65702, #179506, #181606 ) ;
#68628 = CARTESIAN_POINT ( 'NONE',  ( 1.774756598535260466, -1.955815263226182932, -0.6494449766335576024 ) ) ;
#68630 = CARTESIAN_POINT ( 'NONE',  ( 8.213877987985293672, 14.20293839921164469, -8.687862046754464274 ) ) ;
#68629 = CARTESIAN_POINT ( 'NONE',  ( -8.992082194361570302, 11.51384853155376220, 1.599625672291269396 ) ) ;
#68631 = CARTESIAN_POINT ( 'NONE',  ( 0.6823417656249899377, 2.092708333674753174, 1.181850606188767472 ) ) ;
#68632 = CARTESIAN_POINT ( 'NONE',  ( -3.697672731464882734, 7.367968498737599958, 2.499999999999998668 ) ) ;
#68633 = ORIENTED_EDGE ( 'NONE', *, *, #155535, .F. ) ;
#68634 = CARTESIAN_POINT ( 'NONE',  ( 4.125576785117724299, -0.3237648511281773778, 1.884507068624697190 ) ) ;
#68635 = CARTESIAN_POINT ( 'NONE',  ( -11.92619525870747665, 11.02622296793678025, 1.328859154005173959 ) ) ;
#68636 = CARTESIAN_POINT ( 'NONE',  ( 1.546537457781042235, 2.259796958156198077, 0.1114739384607699862 ) ) ;
#68637 = CARTESIAN_POINT ( 'NONE',  ( -9.110716038703348119, 12.61262389758715408, 1.082531754730560403 ) ) ;
#68638 = CARTESIAN_POINT ( 'NONE',  ( 1.634716215409822260, 1.691188361570634235, 0.6499044650936767198 ) ) ;
#68639 = CARTESIAN_POINT ( 'NONE',  ( 1.358442855636652791, -1.820242846481026078, -0.5975442777857197241 ) ) ;
#68640 = AXIS2_PLACEMENT_3D ( 'NONE', #10846, #23901, #139831 ) ;
#68641 = CARTESIAN_POINT ( 'NONE',  ( 2.313015868914463091, -1.601887806243259771, 1.311650804931147274 ) ) ;
#68642 = CARTESIAN_POINT ( 'NONE',  ( -1.402160292154681736E-14, 0.7593750003414168059, -1.575800808251659024 ) ) ;
#68643 = CARTESIAN_POINT ( 'NONE',  ( 0.4265601315296633778, 1.885908329847274745, 0.5744540738892388587 ) ) ;
#68644 = CARTESIAN_POINT ( 'NONE',  ( 5.742784330379758551, 0.3781152824756833231, 1.888869927322960329 ) ) ;
#68646 = CARTESIAN_POINT ( 'NONE',  ( 5.880365472892705725, 7.167286867907723291, -1.140585135024022811 ) ) ;
#68645 = CARTESIAN_POINT ( 'NONE',  ( 0.1711457161924005987, -1.502117798334397403, 1.751973695569712497 ) ) ;
#68647 = CARTESIAN_POINT ( 'NONE',  ( 0.6823417656249882723, 1.176041667008083325, -1.181850606188749264 ) ) ;
#68648 = CARTESIAN_POINT ( 'NONE',  ( 4.510253362402360189, 2.062282729996979924, -0.04753222776765659435 ) ) ;
#68649 = CARTESIAN_POINT ( 'NONE',  ( -7.009729113465285266, 8.136771039586342624, -1.199719254218446718 ) ) ;
#68650 = CARTESIAN_POINT ( 'NONE',  ( 7.618792255875527886, 10.97600916757510170, 1.199719254218460707 ) ) ;
#68651 = DIRECTION ( 'NONE',  ( 0.000000000000000000, 0.7996470168499997255, 0.6004703560067694568 ) ) ;
#68652 = CARTESIAN_POINT ( 'NONE',  ( 6.356075086708249167, 6.309842444114747373, -0.7998128361456281477 ) ) ;
#68654 = CARTESIAN_POINT ( 'NONE',  ( 1.499999999999990896, 4.025000000000021672, 1.214306433183764966E-14 ) ) ;
#68653 = CARTESIAN_POINT ( 'NONE',  ( 5.051841681570322429, 0.6635009534815727861, -1.998768678292896839 ) ) ;
#68655 = CARTESIAN_POINT ( 'NONE',  ( 0.1393978552833140261, -0.1497620924123649333, -2.137132186964474378 ) ) ;
#68656 = CARTESIAN_POINT ( 'NONE',  ( -1.364683531250000748, 0.8218750003414210248, 0.000000000000000000 ) ) ;
#68657 = CARTESIAN_POINT ( 'NONE',  ( 4.569695524216377258, 2.097929177840287540, -0.5203329012281321386 ) ) ;
#68658 = CARTESIAN_POINT ( 'NONE',  ( 5.531901104011129000, -1.969946598288346618, 0.4446316349850876759 ) ) ;
#68659 = CARTESIAN_POINT ( 'NONE',  ( -0.1399997263889594112, -0.002789056014654289761, -2.000146600338557956 ) ) ;
#68660 = EDGE_CURVE ( 'NONE', #13289, #148685, #63589, .T. ) ;
#68663 = CARTESIAN_POINT ( 'NONE',  ( 4.175548123328908900, 7.815297210618305179, -0.7216878364870197293 ) ) ;
#68662 = CARTESIAN_POINT ( 'NONE',  ( 1.642778471875000035, -1.276041666188710400, -2.845375778867859751 ) ) ;
#68661 = CARTESIAN_POINT ( 'NONE',  ( -4.369846591600387242, 14.55265095719298252, -11.13739096725714894 ) ) ;
#68664 = CARTESIAN_POINT ( 'NONE',  ( -6.577640801285370209, 7.702944352034914566, -1.199719254218452047 ) ) ;
#68665 = CARTESIAN_POINT ( 'NONE',  ( 3.292204118033771110, -0.8216723425069611952, -1.841733987974409237 ) ) ;
#68666 = CARTESIAN_POINT ( 'NONE',  ( -9.826962411806732689, 10.35921099006301382, -0.7998128361456291469 ) ) ;
#68668 = CARTESIAN_POINT ( 'NONE',  ( -15.75000000000000000, 13.40000000000000036, -0.7000000000000009548 ) ) ;
#68667 = CARTESIAN_POINT ( 'NONE',  ( -4.009460741339347045, 5.700790169694431420, -1.599625672291256295 ) ) ;
#68670 = CARTESIAN_POINT ( 'NONE',  ( -11.88237264505823987, 12.34322961531690410, -0.9087825512663008087 ) ) ;
#68669 = CARTESIAN_POINT ( 'NONE',  ( 5.454052192070485638, 2.159419290912270029, -0.1019294599445344784 ) ) ;
#68671 =( NAMED_UNIT ( * ) PLANE_ANGLE_UNIT ( ) SI_UNIT ( $, .RADIAN. ) );
#68672 = DIRECTION ( 'NONE',  ( -1.000000000000000000, 0.000000000000000000, 0.000000000000000000 ) ) ;
#68674 = CARTESIAN_POINT ( 'NONE',  ( 4.499625164952708367, -1.976952908697379607, 0.3961224619316304763 ) ) ;
#68673 = CARTESIAN_POINT ( 'NONE',  ( -8.148087131688699358, 8.608449196499371681, -0.7216878364870267237 ) ) ;
#68675 = CARTESIAN_POINT ( 'NONE',  ( -0.7499999999999972244, 5.608333333333353821, -1.299038105676652011 ) ) ;
#68676 = CARTESIAN_POINT ( 'NONE',  ( 0.5391470445266118849, -1.216214603651460724, -1.223400588829765878 ) ) ;
#68677 = CARTESIAN_POINT ( 'NONE',  ( 6.387826650694035990, 7.481494509678370264, -1.199719254218452047 ) ) ;
#68679 = CARTESIAN_POINT ( 'NONE',  ( 0.4694063952341808177, -6.893137084989842123, 10.98997987423603995 ) ) ;
#68678 = CARTESIAN_POINT ( 'NONE',  ( 8.459924665247367415, 8.972259652317825740, -0.7216878364870267237 ) ) ;
#68680 = CARTESIAN_POINT ( 'NONE',  ( -11.29625252127160628, 7.648179254756541035, 3.920601804043121419 ) ) ;
#68681 = CARTESIAN_POINT ( 'NONE',  ( 5.536355731483205922, 1.842701317132239724, 0.3206550288221421963 ) ) ;
#68682 = CARTESIAN_POINT ( 'NONE',  ( 6.135026823787811168, 1.880036687389478489, 0.7205229627402914838 ) ) ;
#68683 = SURFACE_SIDE_STYLE ('',( #117525 ) ) ;
#68684 = ORIENTED_EDGE ( 'NONE', *, *, #198992, .F. ) ;
#68685 = CIRCLE ( 'NONE', #48029, 0.04999999999999969746 ) ;
#68686 = CARTESIAN_POINT ( 'NONE',  ( -5.411112705185557203, 9.327065566109540740, 0.7216878364870267237 ) ) ;
#68687 = ORIENTED_EDGE ( 'NONE', *, *, #82785, .T. ) ;
#68688 = CARTESIAN_POINT ( 'NONE',  ( 9.368320956918608999, 11.95279375453699622, 1.443375672974076540 ) ) ;
#68689 = CARTESIAN_POINT ( 'NONE',  ( 0.1929827526203631294, 1.755782054984224683, 0.9913788669043410717 ) ) ;
#68690 = CARTESIAN_POINT ( 'NONE',  ( 1.124954419467529831, 1.598432135740068372, 0.8524628987082534248 ) ) ;
#68691 = CARTESIAN_POINT ( 'NONE',  ( 6.230854113932139171, 9.427024345299638952, 1.199719254218452047 ) ) ;
#68692 = CARTESIAN_POINT ( 'NONE',  ( 5.858325616802108726, 0.8718737102157668728, 1.978260574764856283 ) ) ;
#68693 = CARTESIAN_POINT ( 'NONE',  ( 5.913327553854682783, 10.05063257947248800, -0.7998128361456291469 ) ) ;
#68695 = CARTESIAN_POINT ( 'NONE',  ( 0.6904808011564408377, 1.448434100015457693, -1.253846941973751683 ) ) ;
#68694 = CARTESIAN_POINT ( 'NONE',  ( -5.904739593951539689, 6.847616600153594746, 1.199719254218450271 ) ) ;
#68696 = VECTOR ( 'NONE', #12839, 1000.000000000000000 ) ;
#68697 = DIRECTION ( 'NONE',  ( 1.000000000000000000, 0.000000000000000000, 0.000000000000000000 ) ) ;
#68698 = DIRECTION ( 'NONE',  ( -0.000000000000000000, -1.000000000000000000, -0.000000000000000000 ) ) ;
#68699 = CARTESIAN_POINT ( 'NONE',  ( -1.402160292154681736E-14, -0.3656249996585805295, 1.575800808251672791 ) ) ;
#68700 = CARTESIAN_POINT ( 'NONE',  ( 3.389175213736297820, 4.977123720824209840, 1.443375672974062551 ) ) ;
#68701 = CARTESIAN_POINT ( 'NONE',  ( -3.216308754939891212, 4.775446185561722956, -1.599625672291262513 ) ) ;
#68702 = EDGE_CURVE ( 'NONE', #41289, #129277, #73813, .T. ) ;
#68703 = CARTESIAN_POINT ( 'NONE',  ( 4.416967121957662279, 1.975198431823081302, 0.8787980929093121008 ) ) ;
#68704 = CARTESIAN_POINT ( 'NONE',  ( -5.587368702607575344, 8.572328348800551723, 1.082531754730550855 ) ) ;
#68705 = CARTESIAN_POINT ( 'NONE',  ( 5.966997003790217136, 8.054858819212300958, -1.443375672974078761 ) ) ;
#68706 = CARTESIAN_POINT ( 'NONE',  ( 0.8266187642571948269, -0.9586779626098644869, -1.891633453305548773 ) ) ;
#68707 = CARTESIAN_POINT ( 'NONE',  ( -1.225000000000046052, 2.520833333333404092, 0.7072540797572777205 ) ) ;
#68708 = CARTESIAN_POINT ( 'NONE',  ( 2.512907010818050679, 1.759183109745281692, 0.8898679072262619671 ) ) ;
#68709 = CARTESIAN_POINT ( 'NONE',  ( 4.957238921819991262, -1.637161358497842389, 0.9882132959125531357 ) ) ;
#68710 = ORIENTED_EDGE ( 'NONE', *, *, #6564, .F. ) ;
#68712 = EDGE_CURVE ( 'NONE', #144405, #8531, #101612, .T. ) ;
#68711 = CARTESIAN_POINT ( 'NONE',  ( -3.179715765502671321, 5.975770656120749535, -2.499999999999998668 ) ) ;
#68713 = CARTESIAN_POINT ( 'NONE',  ( 6.180130249528606790, -1.092802789126966934, -1.638350696670291651 ) ) ;
#68715 = B_SPLINE_CURVE_WITH_KNOTS ( 'NONE', 3,
 ( #120149, #170953, #6299, #153651, #85436, #152571 ),
 .UNSPECIFIED., .F., .F.,
 ( 4, 2, 4 ),
 ( 1.748223473168672935E-18, 0.0003191287515899651349, 0.0006382575031799285351 ),
 .UNSPECIFIED. ) ;
#68714 = CARTESIAN_POINT ( 'NONE',  ( 1.183423309950997870, -0.8736912582980368436, 1.734375191483277900 ) ) ;
#68716 = ORIENTED_EDGE ( 'NONE', *, *, #191917, .F. ) ;
#68717 = CARTESIAN_POINT ( 'NONE',  ( -4.634908411025374875, 6.500755460986618495, 1.599625672291263179 ) ) ;
#68718 = CARTESIAN_POINT ( 'NONE',  ( -4.604929450496978660, 5.401447776115099408, -1.199719254218453823 ) ) ;
#68720 = CARTESIAN_POINT ( 'NONE',  ( 3.865483193227626124, 7.523831135491951372, -0.7216878364870338292 ) ) ;
#68719 = CARTESIAN_POINT ( 'NONE',  ( 5.635385404774530649, 9.726366738878972740, 0.7998128361456462443 ) ) ;
#68722 = ORIENTED_EDGE ( 'NONE', *, *, #40853, .F. ) ;
#68721 = CARTESIAN_POINT ( 'NONE',  ( 4.775979982822478931, 1.890921987351320777, -0.2842533987747336566 ) ) ;
#68723 = CARTESIAN_POINT ( 'NONE',  ( 3.774219598512587037, 1.225428716765289527, 1.835190637982798023 ) ) ;
#68724 = CARTESIAN_POINT ( 'NONE',  ( 2.432911661931828284, 2.140371652790736601, 0.5367425311649312025 ) ) ;
#68725 = AXIS2_PLACEMENT_3D ( 'NONE', #135219, #4093, #19291 ) ;
#68726 = CARTESIAN_POINT ( 'NONE',  ( 1.580000000000019389, 8.674529973577556063, 2.499999999999961364 ) ) ;
#68727 = CARTESIAN_POINT ( 'NONE',  ( 0.7153071762652126742, 1.563590412251715911, 1.100639817434710954 ) ) ;
#68728 = CARTESIAN_POINT ( 'NONE',  ( -0.02338929933906607611, 7.629137130509112907, -2.310989781590186976 ) ) ;
#68729 = CARTESIAN_POINT ( 'NONE',  ( -10.51595811585100648, 13.61340346008145019, -3.553980774159643197 ) ) ;
#68730 = CARTESIAN_POINT ( 'NONE',  ( -0.5987734146285321746, 6.693217038951044806, 3.557622718601344047 ) ) ;
#68731 = CARTESIAN_POINT ( 'NONE',  ( 3.473154722801426786, 1.870513717286937716, 0.8877811045280564750 ) ) ;
#68732 = CARTESIAN_POINT ( 'NONE',  ( -6.261168011412601153, 6.199117522936475666, 1.040834085586084257E-14 ) ) ;
#68733 = CARTESIAN_POINT ( 'NONE',  ( -5.941092982759174745, 7.138105816550336158, 1.109076209742832164 ) ) ;
#68735 = CARTESIAN_POINT ( 'NONE',  ( 0.6378455412261313517, -1.529572671500577297, -1.527792216034072670 ) ) ;
#68734 = CARTESIAN_POINT ( 'NONE',  ( -4.223528545856940042, 4.886203710709899006, -1.199719254218446718 ) ) ;
#68736 = CARTESIAN_POINT ( 'NONE',  ( 3.298540952264991777, 1.726358142885858316, -1.349911518210664241 ) ) ;
#68737 = CARTESIAN_POINT ( 'NONE',  ( -0.1216878429548678975, 3.463015919485879834, -1.996294584693599994 ) ) ;
#68738 = CARTESIAN_POINT ( 'NONE',  ( 4.760321332173959696, 4.726332107057286791, 0.000000000000000000 ) ) ;
#68739 = CARTESIAN_POINT ( 'NONE',  ( 4.805347440941809738E-16, 2.000000000000001776, -2.649999999999999911 ) ) ;
#68740 = CARTESIAN_POINT ( 'NONE',  ( -0.6823417656250039265, 13.13020833367473017, -1.181850606188755259 ) ) ;
#68741 = CARTESIAN_POINT ( 'NONE',  ( -6.656127069666307072, 6.730179434224282886, 0.7998128361456341429 ) ) ;
#68742 = CARTESIAN_POINT ( 'NONE',  ( 5.678250988984351544, 1.318717643421193575, 1.126304846749843769 ) ) ;
#68743 = EDGE_CURVE ( 'NONE', #163067, #30915, #184621, .T. ) ;
#68744 = CARTESIAN_POINT ( 'NONE',  ( -8.785320351975364872, 12.23299559640450518, 1.082531754730560403 ) ) ;
#68745 = CARTESIAN_POINT ( 'NONE',  ( 3.450112209602332669, -0.8433740631265237431, 1.890881698631073249 ) ) ;
#68746 = CARTESIAN_POINT ( 'NONE',  ( 5.097310499321968003, -0.3096355862501755096, 2.094337834851481617 ) ) ;
#68747 = CARTESIAN_POINT ( 'NONE',  ( 7.461064606222022277, 7.598996883547496139, 1.040834085586084257E-14 ) ) ;
#68748 = CARTESIAN_POINT ( 'NONE',  ( 1.364683531249988535, 4.363541667008089320, 0.7879004041258499402 ) ) ;
#68749 = CARTESIAN_POINT ( 'NONE',  ( 3.010559277710533888, 0.6591459557328577246, 1.856027811050243947 ) ) ;
#68750 = CARTESIAN_POINT ( 'NONE',  ( 1.002048865836258518, -0.8573748960705518396, 1.709468765625526521 ) ) ;
#68751 = CARTESIAN_POINT ( 'NONE',  ( 5.296947879282962290, 1.871547875688117424, 1.323312301801358393 ) ) ;
#68752 = CARTESIAN_POINT ( 'NONE',  ( 2.560947663861262491, -1.588335953301520220, -0.9000364273514870339 ) ) ;
#68753 = CARTESIAN_POINT ( 'NONE',  ( 8.000720045840086669, 8.506797273001177828, 0.7216878364870267237 ) ) ;
#68754 = CARTESIAN_POINT ( 'NONE',  ( 4.812781342726855982, 7.598366752281232372, 1.082531754730558626 ) ) ;
#68755 = CARTESIAN_POINT ( 'NONE',  ( -6.612626235163205024, 8.737816579155630592, -1.599625672291263179 ) ) ;
#68756 = B_SPLINE_CURVE_WITH_KNOTS ( 'NONE', 3,
 ( #162566, #79164, #95455, #177745, #114927, #211286, #112806, #29360, #82352, #213407, #163631 ),
 .UNSPECIFIED., .F., .F.,
 ( 4, 1, 1, 1, 1, 1, 1, 1, 4 ),
 ( 0.000000000000000000, 0.2256085737580844630, 0.3975982043691296264, 0.5251069566405043298, 0.6172860083021659561, 0.6832860984239963464, 0.7321959383537668398, 0.7728624839797392232, 1.000000000000000000 ),
 .UNSPECIFIED. ) ;
#68757 = CARTESIAN_POINT ( 'NONE',  ( 4.201435496602879738, 1.796340046740346086, -0.9091319694144882613 ) ) ;
#68758 =( BOUNDED_CURVE ( )  B_SPLINE_CURVE ( 2, ( #20310, #152464, #66901, #136225, #169772, #69048, #199041 ),
 .UNSPECIFIED., .F., .T. ) 
 B_SPLINE_CURVE_WITH_KNOTS ( ( 3, 2, 2, 3 ),
 ( 0.2750000000000000222, 0.2833333333333331039, 0.2916666666666662966, 0.2999999999999993783 ),
 .UNSPECIFIED. ) 
 CURVE ( )  GEOMETRIC_REPRESENTATION_ITEM ( )  RATIONAL_B_SPLINE_CURVE ( ( 1.000000000000000000, 0.8660254037844387076, 1.000000000000000000, 0.8660254037844387076, 1.000000000000000000, 0.8660254037844484776, 0.9999999999999902300 ) ) 
 REPRESENTATION_ITEM ( '' )  );
#68759 = CARTESIAN_POINT ( 'NONE',  ( 3.959774770350584561, -0.5736532364168048792, 1.875976257969473648 ) ) ;
#68760 = CARTESIAN_POINT ( 'NONE',  ( -8.518600588087975822, 8.832788862391110385, 1.040834085586084257E-14 ) ) ;
#68761 = CARTESIAN_POINT ( 'NONE',  ( -6.098470168048611306, 6.009303372345148553, 1.040834085586084257E-14 ) ) ;
#68762 = CARTESIAN_POINT ( 'NONE',  ( 0.1755611466353265426, 6.947017789483680872, -2.839095415174418768 ) ) ;
#68764 = CARTESIAN_POINT ( 'NONE',  ( 5.559369761212399119, 0.3421458929979518948, -1.736264261622854743 ) ) ;
#68763 = CARTESIAN_POINT ( 'NONE',  ( 0.4684514965578719381, -1.969967889910573033, -0.7007429371770137472 ) ) ;
#68765 = CARTESIAN_POINT ( 'NONE',  ( 7.671537448944488015E-16, -0.6185895741317448682, -6.264285714285709794 ) ) ;
#68766 = CARTESIAN_POINT ( 'NONE',  ( 1.640847625397081622, -1.850035366842089024, 1.174371965539475093 ) ) ;
#68767 = CARTESIAN_POINT ( 'NONE',  ( 6.281193118957388855, 1.205677877666534892, 1.255287683557136491 ) ) ;
#68768 = VECTOR ( 'NONE', #23304, 1000.000000000000000 ) ;
#68769 = CARTESIAN_POINT ( 'NONE',  ( 7.775764792637399836, 9.030479331953833011, -1.199719254218441611 ) ) ;
#68770 = CARTESIAN_POINT ( 'NONE',  ( 0.9434950454815290710, 0.7028112840000885209, -1.575391610592514757 ) ) ;
#68771 = CARTESIAN_POINT ( 'NONE',  ( 0.6326644773376333131, 0.2229630159884201934, -2.287572974657641645 ) ) ;
#68772 =( BOUNDED_SURFACE ( )  B_SPLINE_SURFACE ( 3, 2, ( 
 ( #141997, #56446, #124731 ),
 ( #59635, #172334, #188569 ),
 ( #42349, #125793, #108464 ),
 ( #71598, #40200, #105212 ) ),
 .UNSPECIFIED., .F., .F., .F. ) 
 B_SPLINE_SURFACE_WITH_KNOTS ( ( 4, 4 ),
 ( 3, 3 ),
 ( 0.04893088146668655297, 0.05137248493452929027 ),
 ( 0.000000000000000000, 1.000000000000000000 ),
 .UNSPECIFIED. ) 
 GEOMETRIC_REPRESENTATION_ITEM ( )  RATIONAL_B_SPLINE_SURFACE ( (
 ( 1.000000000000000000, 0.7169884966214685740, 1.000000000000000000),
 ( 1.000000000000000000, 0.7174883642158066399, 1.000000000000000000),
 ( 1.000000000000000000, 0.7180610417773352072, 1.000000000000000000),
 ( 1.000000000000000000, 0.7187540717311200478, 1.000000000000000000) ) ) 
 REPRESENTATION_ITEM ( '' )  SURFACE ( )  );
#68773 = CARTESIAN_POINT ( 'NONE',  ( 0.5213437761196970666, -2.079166062760181788, 0.6930039600180630810 ) ) ;
#68774 = CARTESIAN_POINT ( 'NONE',  ( 6.134130222960958889, 0.1235499018571624141, -1.729521282446895070 ) ) ;
#68775 = CARTESIAN_POINT ( 'NONE',  ( 3.440233207309027375, 0.9924059104887033023, -1.971224004288201881 ) ) ;
#68776 = CARTESIAN_POINT ( 'NONE',  ( 6.478989045741552211, 2.023467559352111866, 0.7875856005067942700 ) ) ;
#68777 = CARTESIAN_POINT ( 'NONE',  ( 0.000000000000000000, 0.08000000000000020983, 0.000000000000000000 ) ) ;
#68778 = CARTESIAN_POINT ( 'NONE',  ( 0.9368845280443529600, -1.665339089426773000, 1.307453795268032071 ) ) ;
#68779 = CARTESIAN_POINT ( 'NONE',  ( 6.827182134110200806, 4.685259207053684705, 2.851548537572299313 ) ) ;
#68780 = CARTESIAN_POINT ( 'NONE',  ( 5.491212607897098863, 1.698784202212012762, -0.9083314536618128932 ) ) ;
#68781 = VERTEX_POINT ( 'NONE', #22041 ) ;
#68783 = CARTESIAN_POINT ( 'NONE',  ( 1.499999999999990896, 5.525000000000022560, 1.214306433183764966E-14 ) ) ;
#68782 = CARTESIAN_POINT ( 'NONE',  ( 1.242159777398026410, 2.290014686995527793, 0.1064554428192917290 ) ) ;
#68784 = CARTESIAN_POINT ( 'NONE',  ( 3.009020027229115879, 5.597941567487558778, -1.199719254218446718 ) ) ;
#68785 = CARTESIAN_POINT ( 'NONE',  ( 5.656776405399742025, 7.622658444431597680, -1.599625672291262513 ) ) ;
#68786 = CARTESIAN_POINT ( 'NONE',  ( 4.565202069552391606, -1.784334575089935981, 1.322790477621762051 ) ) ;
#68787 = CARTESIAN_POINT ( 'NONE',  ( -6.236387472606141458, 10.21960978477508952, -0.7216878364870278340 ) ) ;
#68788 = CARTESIAN_POINT ( 'NONE',  ( 0.000000000000000000, 4.006659545634088992, 0.000000000000000000 ) ) ;
#68789 = CARTESIAN_POINT ( 'NONE',  ( 5.016153647376201619, 7.835634441038803466, 1.082531754730558626 ) ) ;
#68790 = CARTESIAN_POINT ( 'NONE',  ( -8.636180661780668899, 10.13826086257468795, -1.082531754730543083 ) ) ;
#68791 = CARTESIAN_POINT ( 'NONE',  ( 6.265276383290871109, 7.442482214328385304, -1.082531754730548412 ) ) ;
#68792 = CARTESIAN_POINT ( 'NONE',  ( 2.391250195717840477, -0.7743161457766101208, -1.862016636315230844 ) ) ;
#68794 = CARTESIAN_POINT ( 'NONE',  ( 1.604420861476773208, 2.060019368494928838, 0.1054051996416793119 ) ) ;
#68793 = CARTESIAN_POINT ( 'NONE',  ( 6.577677080924314801, 10.82570702772039262, 1.040834085586084257E-14 ) ) ;
#68795 = CARTESIAN_POINT ( 'NONE',  ( -11.80251051724219202, 13.79999999999998295, 1.695257889419070851 ) ) ;
#68796 = CARTESIAN_POINT ( 'NONE',  ( 6.658462837642799670, 6.940830530104329377, 0.7216878364870328300 ) ) ;
#68797 = B_SPLINE_CURVE_WITH_KNOTS ( 'NONE', 3,
 ( #106163, #23779, #89885, #189491 ),
 .UNSPECIFIED., .F., .F.,
 ( 4, 4 ),
 ( 0.001812203442042607240, 0.002059939351771563048 ),
 .UNSPECIFIED. ) ;
#68798 = DIRECTION ( 'NONE',  ( -1.000000000000000000, 5.578174157656879309E-15, -1.224646799147768099E-16 ) ) ;
#68799 = CARTESIAN_POINT ( 'NONE',  ( 1.364683531249988535, 3.905208333674751842, -0.7879004041258239610 ) ) ;
#68800 = CARTESIAN_POINT ( 'NONE',  ( 3.873126987144244193, 2.063651454400210028, -0.7377723227853100196 ) ) ;
#68801 = CARTESIAN_POINT ( 'NONE',  ( 0.8619541869999207684, -0.05229984143813663777, -2.015912905633105101 ) ) ;
#68802 = CARTESIAN_POINT ( 'NONE',  ( 0.9426144736941791669, -1.451487892885485742, -1.132780452900377099 ) ) ;
#68803 = CARTESIAN_POINT ( 'NONE',  ( 5.425394459833968064, -1.452027641166652172, -1.773832485185691032 ) ) ;
#68804 = CARTESIAN_POINT ( 'NONE',  ( 3.521284115754549582, -1.097709940230184200, -1.477957507169822104 ) ) ;
#68805 = CARTESIAN_POINT ( 'NONE',  ( 9.582915646760733708, 10.07448976417602893, 0.7998128361456462443 ) ) ;
#68806 = CARTESIAN_POINT ( 'NONE',  ( 4.418855976699648025, 1.669273799801282765, 0.7395231729718022562 ) ) ;
#68807 = CARTESIAN_POINT ( 'NONE',  ( 5.502577337681268332, -1.966645332631598908, 0.4444998760482973821 ) ) ;
#68808 = CARTESIAN_POINT ( 'NONE',  ( -7.479294296233107708, 11.87759377891399204, 0.7998128361456481317 ) ) ;
#68810 = CARTESIAN_POINT ( 'NONE',  ( -7.957709816578236506, 8.248692638954882028, 0.7998128361456341429 ) ) ;
#68809 = CARTESIAN_POINT ( 'NONE',  ( 4.311571290614625518, -0.3905533787264577894, 2.228413237907675537 ) ) ;
#68811 = CARTESIAN_POINT ( 'NONE',  ( 6.194376850977553417, -2.095475641407635425, -0.2099330270173524471 ) ) ;
#68812 = CARTESIAN_POINT ( 'NONE',  ( 3.121598655985452275, 0.3063859900464052100, -2.047459029603612368 ) ) ;
#68813 = CARTESIAN_POINT ( 'NONE',  ( 4.376584659113025744, 4.000436945253625254, 0.7998128361456341429 ) ) ;
#68814 = CARTESIAN_POINT ( 'NONE',  ( 1.360316468749951602, 2.526041667008117830, 0.7853790794158560518 ) ) ;
#68815 = APPLICATION_PROTOCOL_DEFINITION ( 'draft international standard', 'automotive_design', 1998, #104451 ) ;
#68817 = CARTESIAN_POINT ( 'NONE',  ( 2.385270436692279006, 1.761333987333755013, -0.7808530812865380755 ) ) ;
#68816 = CARTESIAN_POINT ( 'NONE',  ( -8.877891658850122880, 9.251961778280284321, 0.7998128361456462443 ) ) ;
#68818 = CARTESIAN_POINT ( 'NONE',  ( 0.000000000000000000, 14.55305236562704252, -11.95586206896551928 ) ) ;
#68819 = CARTESIAN_POINT ( 'NONE',  ( 6.772316245210458163, -0.9252316606085030370, -1.738535334629727647 ) ) ;
#68820 = CARTESIAN_POINT ( 'NONE',  ( 3.540087506499646874, 7.144202834309300698, -0.7216878364870338292 ) ) ;
#68821 = CARTESIAN_POINT ( 'NONE',  ( 5.228900738148710481, 6.411469580122314049, 1.161126877744517838 ) ) ;
#68822 = CARTESIAN_POINT ( 'NONE',  ( 1.270916165646588603, 3.290225491120026380, -0.7749999999999910294 ) ) ;
#68823 = CARTESIAN_POINT ( 'NONE',  ( -2.279742385392243165, 5.811449882932888222, -0.7998128361456281477 ) ) ;
#68824 = CARTESIAN_POINT ( 'NONE',  ( 1.266231527720959926, 0.6383494478915030523, -2.127751457625071563 ) ) ;
#68825 = CARTESIAN_POINT ( 'NONE',  ( 3.698352234880129874, -2.103465879664846216, -0.1051872838587295522 ) ) ;
#68826 = CARTESIAN_POINT ( 'NONE',  ( -7.761116589180078407, 8.019333873657032541, 0.000000000000000000 ) ) ;
#68827 = CARTESIAN_POINT ( 'NONE',  ( 5.940443861082012944, 10.08226827123770697, 0.7998128361456462443 ) ) ;
#68828 = CARTESIAN_POINT ( 'NONE',  ( 0.4845113730182957767, 1.779151863920569232, 0.5459849130424464514 ) ) ;
#68829 = CARTESIAN_POINT ( 'NONE',  ( 6.636879889089462026, 7.701780277814560982, -1.199719254218446718 ) ) ;
#68830 = CARTESIAN_POINT ( 'NONE',  ( 3.960953433486789521, 7.772862772376584850, -0.7998128361456221525 ) ) ;
#68831 = CARTESIAN_POINT ( 'NONE',  ( -6.048345925472225382, 8.149765894507963182, 1.443375672974058777 ) ) ;
#68832 = CARTESIAN_POINT ( 'NONE',  ( -8.866669273657352690, 9.446795028796142191, 0.7216878364870438212 ) ) ;
#68833 =( BOUNDED_SURFACE ( )  B_SPLINE_SURFACE ( 3, 2, ( 
 ( #208325, #75148, #76205 ),
 ( #56761, #142315, #141258 ),
 ( #207266, #58897, #125050 ),
 ( #191005, #108780, #174806 ) ),
 .UNSPECIFIED., .F., .F., .T. ) 
 B_SPLINE_SURFACE_WITH_KNOTS ( ( 4, 4 ),
 ( 3, 3 ),
 ( 3.141592653589793116, 4.712388980384689674 ),
 ( 0.000000000000000000, 1.000000000000000000 ),
 .UNSPECIFIED. ) 
 GEOMETRIC_REPRESENTATION_ITEM ( )  RATIONAL_B_SPLINE_SURFACE ( (
 ( 1.000000000000000000, 0.8661919058288514162, 1.000000000000000000),
 ( 1.000000000000000000, 0.8676977444974305342, 1.000000000000000000),
 ( 1.000000000000000000, 0.8014503788335436418, 1.000000000000000000),
 ( 1.000000000000000000, 0.7071067811865416886, 1.000000000000000000) ) ) 
 REPRESENTATION_ITEM ( '' )  SURFACE ( )  );
#68835 = CARTESIAN_POINT ( 'NONE',  ( 0.9144942500491148873, -2.120778211678171488, 0.005759991200282587286 ) ) ;
#68834 = AXIS2_PLACEMENT_3D ( 'NONE', #113915, #198260, #32583 ) ;
#68836 = CARTESIAN_POINT ( 'NONE',  ( -5.264308783856126439, 9.363720357799287797, -0.7998128361456362523 ) ) ;
#68838 = CARTESIAN_POINT ( 'NONE',  ( 4.633228507203630997, 0.002057781214020309134, -1.962046631861932067 ) ) ;
#68837 = CARTESIAN_POINT ( 'NONE',  ( -0.6124999999999880540, 0.2916666666666900554, 1.060881119635892933 ) ) ;
#68839 = CARTESIAN_POINT ( 'NONE',  ( 3.362350911093567873, 0.9703303321016673033, 1.931748911306984784 ) ) ;
#68840 = CARTESIAN_POINT ( 'NONE',  ( 1.593040506729075823, -0.6195558395927207584, 1.734028948791266345 ) ) ;
#68841 = CARTESIAN_POINT ( 'NONE',  ( -4.118090981180881016, 7.482401814132296103, -0.6348448669579254133 ) ) ;
#68842 = CARTESIAN_POINT ( 'NONE',  ( -0.6823417656250003738, -0.9697916663252494907, -1.181850606188749264 ) ) ;
#68843 = CARTESIAN_POINT ( 'NONE',  ( 4.083748955185668272, -1.721791984697383482, -0.2523947965055831633 ) ) ;
#68844 = CARTESIAN_POINT ( 'NONE',  ( -3.960390268523300339, 7.634556056670224855, 1.214306433183764966E-14 ) ) ;
#68845 = CARTESIAN_POINT ( 'NONE',  ( 5.829642864196171281, 5.903597551091405826, 0.7216878364870317197 ) ) ;
#68846 = CARTESIAN_POINT ( 'NONE',  ( -10.61922739175395236, 7.618143447610075114, 4.514851702475597861 ) ) ;
#68847 = EDGE_CURVE ( 'NONE', #65209, #5754, #171525, .T. ) ;
#68848 = CARTESIAN_POINT ( 'NONE',  ( 2.360439101503517101, 0.9236781337260314695, 1.954550705658316456 ) ) ;
#68849 = CARTESIAN_POINT ( 'NONE',  ( 3.479842141819572632, 1.821463063354014533, 0.8645922719773959653 ) ) ;
#68850 = CARTESIAN_POINT ( 'NONE',  ( -0.3423093779010150106, 2.999999999999981792, -0.3423093779010167315 ) ) ;
#68851 = CARTESIAN_POINT ( 'NONE',  ( 1.762795743007524063, -1.528684080660724920, 1.528680807790387286 ) ) ;
#68852 = CARTESIAN_POINT ( 'NONE',  ( 3.784019197727214401, -0.9729451851334305346, 1.714598810357757630 ) ) ;
#68853 = CARTESIAN_POINT ( 'NONE',  ( 6.608999999999983999, 4.692729314731947099, 2.662616042240486536 ) ) ;
#68854 = CARTESIAN_POINT ( 'NONE',  ( 3.438947998021203656, -1.472602994093423545, -1.266235326041851961 ) ) ;
#68857 = ORIENTED_EDGE ( 'NONE', *, *, #134927, .F. ) ;
#68856 = DIRECTION ( 'NONE',  ( -0.000000000000000000, -1.000000000000000000, -0.000000000000000000 ) ) ;
#68855 = CARTESIAN_POINT ( 'NONE',  ( -7.334597915313094241, 9.580116872663850813, 1.040834085586084257E-14 ) ) ;
#68858 = CARTESIAN_POINT ( 'NONE',  ( -5.628043163004235794, 5.738674243025936761, 0.7216878364870257245 ) ) ;
#68859 = CARTESIAN_POINT ( 'NONE',  ( -0.1108833634136767443, 0.0002062650063822807356, -1.896853557917008271 ) ) ;
#68860 = CARTESIAN_POINT ( 'NONE',  ( 5.845500506147374153, 6.848780674373954547, 1.199719254218453823 ) ) ;
#68861 = CARTESIAN_POINT ( 'NONE',  ( -4.468294144155606773, 7.370704380560280100, 1.199719254218452935 ) ) ;
#68862 = CARTESIAN_POINT ( 'NONE',  ( -4.308458954092677651, 8.248562223075252220, -0.7998128361456362523 ) ) ;
#68863 = CARTESIAN_POINT ( 'NONE',  ( -8.419250203962027612, 11.80591375705560608, 1.082531754730549967 ) ) ;
#68864 = CARTESIAN_POINT ( 'NONE',  ( 6.704155097142892927, -2.307279366673311127, 0.04705588035085367382 ) ) ;
#68865 = CARTESIAN_POINT ( 'NONE',  ( 1.642778471875000035, -3.726041666188707691, -2.845375778867859751 ) ) ;
#68866 = CARTESIAN_POINT ( 'NONE',  ( 4.364078322825436729, -1.956782558839207375, 0.1401112987177987601 ) ) ;
#68867 = CARTESIAN_POINT ( 'NONE',  ( 6.747154001095143627, 11.02343010125301959, -0.7998128361456291469 ) ) ;
#68868 = CARTESIAN_POINT ( 'NONE',  ( 2.180314765559120183, 1.560501322096979449, 1.277041908422072991 ) ) ;
#68869 = ORIENTED_EDGE ( 'NONE', *, *, #98123, .T. ) ;
#68870 = CARTESIAN_POINT ( 'NONE',  ( 3.292305547686771305, -0.8622227623886582482, -1.934024985413025810 ) ) ;
#68871 = CARTESIAN_POINT ( 'NONE',  ( -1.201851678989727383E-14, 2.868750000682821266, -1.732050807568863648 ) ) ;
#68873 = CARTESIAN_POINT ( 'NONE',  ( -6.230135280679522936, 7.227244901336242755, 1.199719254218450271 ) ) ;
#68872 = DIRECTION ( 'NONE',  ( -0.6483454320283800199, 0.000000000000000000, 0.7613463080411787542 ) ) ;
#68874 = CARTESIAN_POINT ( 'NONE',  ( 3.046634964419430158, -1.505538468004435027, -1.059505732788845966 ) ) ;
#68875 = VERTEX_POINT ( 'NONE', #155286 ) ;
#68876 = CARTESIAN_POINT ( 'NONE',  ( -8.134002093194872884, 11.57708731111429401, 1.199719254218453823 ) ) ;
#68877 = CARTESIAN_POINT ( 'NONE',  ( -15.75000000000000000, 12.69999999999998153, 1.399999999999998579 ) ) ;
#68878 = CARTESIAN_POINT ( 'NONE',  ( 5.150683391976684788, 2.089615912265533559, 0.3601871064465370087 ) ) ;
#68879 = CARTESIAN_POINT ( 'NONE',  ( 7.124973419181436007, 8.271222729588529887, -1.199719254218446718 ) ) ;
#68880 = CARTESIAN_POINT ( 'NONE',  ( 5.466112512051848782, 1.011855222795062348, 1.795159749414678929 ) ) ;
#68881 = STYLED_ITEM ( 'NONE', ( #10044 ), #23845 ) ;
#68883 = CARTESIAN_POINT ( 'NONE',  ( 3.069684041021227827, -1.094477399149307306, 1.480508570315848482 ) ) ;
#68882 = CARTESIAN_POINT ( 'NONE',  ( 0.3439184179485414439, -0.8825062887024995861, 1.638522830676287789 ) ) ;
#68884 = CARTESIAN_POINT ( 'NONE',  ( 8.561083932025322696, 12.07534945641652158, -1.199719254218446718 ) ) ;
#68885 = CARTESIAN_POINT ( 'NONE',  ( 5.960673519960956845, 6.112995148063339101, -0.7021749152587808407 ) ) ;
#68886 = CARTESIAN_POINT ( 'NONE',  ( -6.071018923869249129, 10.30488218781460574, 0.7998128361456291469 ) ) ;
#68887 = CARTESIAN_POINT ( 'NONE',  ( 10.91804383151480806, -8.407420853759271395, -0.1905751639681791121 ) ) ;
#68888 = CARTESIAN_POINT ( 'NONE',  ( 2.526237079854487089, -1.271617311931704686, -1.803507373242494438 ) ) ;
#68889 = CARTESIAN_POINT ( 'NONE',  ( 4.815850035042070765, -2.220064692501269477, 0.4349022163744782343 ) ) ;
#68890 = CARTESIAN_POINT ( 'NONE',  ( -7.876924059859742755, 8.292092279365579799, 1.040834085586084257E-14 ) ) ;
#68891 = CARTESIAN_POINT ( 'NONE',  ( 4.763805435907580765, 0.5614848394812530508, -1.722472548925155778 ) ) ;
#68892 = CARTESIAN_POINT ( 'NONE',  ( 4.663251631000405517, 1.785207739607551414, -0.6954431434487169383 ) ) ;
#68893 = DIRECTION ( 'NONE',  ( 0.000000000000000000, 0.000000000000000000, -1.000000000000000000 ) ) ;
#68894 = CARTESIAN_POINT ( 'NONE',  ( 3.959811223838666905, 1.956698650606549350, -0.2402693447622703815 ) ) ;
#68895 = CARTESIAN_POINT ( 'NONE',  ( 5.102362337376947998, -0.6309395149336484154, -1.761181640970375106 ) ) ;
#68896 = STYLED_ITEM ( 'NONE', ( #11962 ), #10478 ) ;
#68897 = CARTESIAN_POINT ( 'NONE',  ( 5.142936340713559318, -0.2273772366201456396, -1.847015746109672119 ) ) ;
#68898 = CARTESIAN_POINT ( 'NONE',  ( 0.04481625915944963123, -9.999534456186202291, 9.500049708089882472 ) ) ;
#68899 = CARTESIAN_POINT ( 'NONE',  ( 0.4093891192313535710, -1.913260280790154866, 0.6371585790938688598 ) ) ;
#68901 = CARTESIAN_POINT ( 'NONE',  ( 1.190214010286832602, -0.9452824899213798648, 1.882083610947625107 ) ) ;
#68900 = CARTESIAN_POINT ( 'NONE',  ( -4.419594887930571758, 4.258541578781506409, 1.214306433183764966E-14 ) ) ;
#68902 = CARTESIAN_POINT ( 'NONE',  ( 10.73535870392234237, 11.41900666419791399, 0.000000000000000000 ) ) ;
#68904 = CARTESIAN_POINT ( 'NONE',  ( -8.319899820280397762, 12.85830022363583147, -0.7998128361456281477 ) ) ;
#68903 = CARTESIAN_POINT ( 'NONE',  ( 1.364683531249990311, 5.676041667008088432, 0.7879004041258500513 ) ) ;
#68905 = CARTESIAN_POINT ( 'NONE',  ( 3.498385214435925317, -1.041973313016024472, 1.846846941210858351 ) ) ;
#68906 = CARTESIAN_POINT ( 'NONE',  ( -4.983766652555303267, 4.889725027032487681, 0.3176639355364049844 ) ) ;
#68907 = CARTESIAN_POINT ( 'NONE',  ( 1.353777543752776591, -1.465856132443652760, -1.389804628120022478 ) ) ;
#68908 = CARTESIAN_POINT ( 'NONE',  ( 1.364683531249988535, 2.363541667008088432, 0.7879004041258500513 ) ) ;
#68909 = CARTESIAN_POINT ( 'NONE',  ( -3.470524135418306511, 5.072030796119872953, -1.443375672974053447 ) ) ;
#68910 = CARTESIAN_POINT ( 'NONE',  ( 5.345992642490140057, 5.131412925860272090, 1.040834085586084257E-14 ) ) ;
#68911 = ORIENTED_EDGE ( 'NONE', *, *, #113819, .F. ) ;
#68912 = CARTESIAN_POINT ( 'NONE',  ( 2.337400524717429207, -1.931973293601353392, 0.9696072025056484689 ) ) ;
#68913 = CARTESIAN_POINT ( 'NONE',  ( 7.664830294503436114, -6.134628647623485698, -7.777967379493309075 ) ) ;
#68916 = CARTESIAN_POINT ( 'NONE',  ( 3.145128448690309053, 4.692402494937224056, -1.443375672974057666 ) ) ;
#68915 =( NAMED_UNIT ( * ) SI_UNIT ( $, .STERADIAN. ) SOLID_ANGLE_UNIT ( ) );
#68914 = CARTESIAN_POINT ( 'NONE',  ( 5.761288931164342486, 5.686201605971993978, -0.7998128361456481317 ) ) ;
#68917 = CARTESIAN_POINT ( 'NONE',  ( 9.205623113554612047, 12.72334881824701469, 1.082531754730546636 ) ) ;
#68918 = CARTESIAN_POINT ( 'NONE',  ( -7.778383330260346007, -6.134628647623487474, 7.778383330260379758 ) ) ;
#68919 = CARTESIAN_POINT ( 'NONE',  ( -8.026063749610063525, 8.466088584074293877, -0.7216878364870278340 ) ) ;
#68920 = CARTESIAN_POINT ( 'NONE',  ( 0.7850416839378616674, 1.930235501049954339, -1.037882601892345713 ) ) ;
#68921 = DIRECTION ( 'NONE',  ( -0.04267330865764933784, 4.780913106218958965E-15, -0.9990890794760041160 ) ) ;
#68923 = CARTESIAN_POINT ( 'NONE',  ( 0.6823417656249969321, 11.52604166700806765, -1.181850606188757036 ) ) ;
#68922 = CARTESIAN_POINT ( 'NONE',  ( 1.885968558009487595, 1.560753693757486849, 1.638220756346415508 ) ) ;
#68924 = CARTESIAN_POINT ( 'NONE',  ( -8.646349277213090545, 11.11049346154719508, 1.599625672291269396 ) ) ;
#68925 = CARTESIAN_POINT ( 'NONE',  ( -5.382223794500845315, 6.341977850748185652, -1.082531754730543971 ) ) ;
#68927 = AXIS2_PLACEMENT_3D ( 'NONE', #54799, #102480, #168546 ) ;
#68926 = CARTESIAN_POINT ( 'NONE',  ( -1.364683531249997417, 2.571875000341422357, 1.214306433183764966E-14 ) ) ;
#68928 = CARTESIAN_POINT ( 'NONE',  ( 4.597294405107005488, 8.370805622008914426, 0.1071034531749150143 ) ) ;
#68929 = CARTESIAN_POINT ( 'NONE',  ( -6.009258394948636914E-15, 9.187500000000003553, -1.732050807568875195 ) ) ;
#68930 = CARTESIAN_POINT ( 'NONE',  ( 3.984733165684080092, -0.1715787546078418324, -1.716317334075837975 ) ) ;
#68931 = CARTESIAN_POINT ( 'NONE',  ( 4.686278372178935392, 5.496354851410763409, 1.199719254218452047 ) ) ;
#68932 = CARTESIAN_POINT ( 'NONE',  ( 2.108344674345350445, 1.315072395666099236, -1.184512757523252358 ) ) ;
#68933 = CARTESIAN_POINT ( 'NONE',  ( 5.631908123138919642, -1.395923778694251105, -1.709176034821748624 ) ) ;
#68934 = ORIENTED_EDGE ( 'NONE', *, *, #3938, .T. ) ;
#68936 = CARTESIAN_POINT ( 'NONE',  ( 4.324476463189423470, -0.8673186339709404447, -1.824254535609586725 ) ) ;
#68935 = AXIS2_PLACEMENT_3D ( 'NONE', #141804, #24794, #106114 ) ;
#68937 = CARTESIAN_POINT ( 'NONE',  ( -6.286140498591554326, 7.362860665558790707, 1.199719254218452047 ) ) ;
#68938 = CARTESIAN_POINT ( 'NONE',  ( 4.446888776373093322, -1.802426293348384334, -0.9040943451460029534 ) ) ;
#68939 = ORIENTED_EDGE ( 'NONE', *, *, #196923, .T. ) ;
#68940 = STYLED_ITEM ( 'NONE', ( #459 ), #158894 ) ;
#68941 = CARTESIAN_POINT ( 'NONE',  ( 2.535844406030359544, 0.8837261853790435717, -1.648756255988912178 ) ) ;
#68942 = CARTESIAN_POINT ( 'NONE',  ( -11.94105721237523099, 11.02740390989733221, -1.187919463087249827 ) ) ;
#68943 = CARTESIAN_POINT ( 'NONE',  ( 1.705181254219298115, 1.662258477346746588, -0.9455041445245655485 ) ) ;
#68944 = LINE ( 'NONE', #21260, #36289 ) ;
#68945 = CARTESIAN_POINT ( 'NONE',  ( -11.05174500248992331, 4.511067306307721125, -6.216760965876352962 ) ) ;
#68946 = CARTESIAN_POINT ( 'NONE',  ( 0.000000000000000000, 6.999999999999999112, 0.000000000000000000 ) ) ;
#68947 = CARTESIAN_POINT ( 'NONE',  ( -0.6823417656250003738, 2.780208333674753618, -1.181850606188749264 ) ) ;
#68948 = CARTESIAN_POINT ( 'NONE',  ( -0.1933232215488022709, -0.4202133615931051835, -1.872389726556406897 ) ) ;
#68949 = EDGE_CURVE ( 'NONE', #169163, #71477, #146637, .T. ) ;
#68950 = CARTESIAN_POINT ( 'NONE',  ( 5.560252395380206103, 8.540692657035327429, 1.082531754730547524 ) ) ;
#68951 = CARTESIAN_POINT ( 'NONE',  ( 1.978885927095444863, 1.829411362569667743, 0.7090815385668995940 ) ) ;
#68952 = CARTESIAN_POINT ( 'NONE',  ( 8.790098660144264997, 13.29414747594432455, 8.101455065885630802 ) ) ;
#68953 = CARTESIAN_POINT ( 'NONE',  ( -5.478376588373717659, 8.549133898814758936, -1.199719254218452047 ) ) ;
#68954 = CARTESIAN_POINT ( 'NONE',  ( 5.238584497427841491, 1.261362679698872169, -1.704546977916908457 ) ) ;
#68956 = PRESENTATION_STYLE_ASSIGNMENT (( #84165 ) ) ;
#68955 = CARTESIAN_POINT ( 'NONE',  ( 9.423080456697809026, 10.95234760669099749, -1.199719254218446718 ) ) ;
#68958 = EDGE_CURVE ( 'NONE', #27161, #160642, #178930, .T. ) ;
#68957 = CARTESIAN_POINT ( 'NONE',  ( 5.835224730271552751, -1.783237572924928127, 0.8406590917669158891 ) ) ;
#68959 = CARTESIAN_POINT ( 'NONE',  ( 1.364683531249986537, 2.155208333674751398, -0.7879004041258239610 ) ) ;
#68960 = CARTESIAN_POINT ( 'NONE',  ( 0.3166526355253923009, -0.6820779544549429030, -1.894243553402875202 ) ) ;
#68961 = ORIENTED_EDGE ( 'NONE', *, *, #157657, .T. ) ;
#68962 = CARTESIAN_POINT ( 'NONE',  ( 1.458780272697857594, -2.011719176664223951, -0.6602987507247930488 ) ) ;
#68964 = EDGE_CURVE ( 'NONE', #54346, #82463, #160381, .T. ) ;
#68963 = CARTESIAN_POINT ( 'NONE',  ( 11.05588078634535698, 8.012831956445918280, -4.553764956315686341 ) ) ;
#68965 = CARTESIAN_POINT ( 'NONE',  ( 3.104029480343179603, 0.7476448069429382226, -1.930825944200013966 ) ) ;
#68966 = CARTESIAN_POINT ( 'NONE',  ( 4.366607992053101128, 7.252070536440704096, -1.199719254218448494 ) ) ;
#68967 = CARTESIAN_POINT ( 'NONE',  ( 5.712781623311797397, 7.758274208654143855, -1.599625672291283607 ) ) ;
#68968 = ORIENTED_EDGE ( 'NONE', *, *, #61168, .F. ) ;
#68970 = CARTESIAN_POINT ( 'NONE',  ( 5.192936529234042808, 6.017179691316550283, -1.199719254218452047 ) ) ;
#68969 = CARTESIAN_POINT ( 'NONE',  ( 4.505862177948306346, -0.8935697331868618365, -1.890194782795044492 ) ) ;
#68973 = VERTEX_POINT ( 'NONE', #126066 ) ;
#68972 = CARTESIAN_POINT ( 'NONE',  ( 2.947712979364258690, -1.218347856841961452, -1.340696891046004868 ) ) ;
#68971 = CARTESIAN_POINT ( 'NONE',  ( 2.907047201455060570, 1.541221212934189344, 0.9781624729086122461 ) ) ;
#68974 = CARTESIAN_POINT ( 'NONE',  ( 8.543609354905870035, 13.11929468069890525, 0.7998128361456462443 ) ) ;
#68975 = PLANE ( 'NONE',  #192592 ) ;
#68976 = CARTESIAN_POINT ( 'NONE',  ( 9.262488864310125081, 13.63671387857607975, 6.830742452943137089 ) ) ;
#68977 = CARTESIAN_POINT ( 'NONE',  ( 5.842855468016632692, 0.4250294216477692455, 2.165293060021292515 ) ) ;
#68978 = CARTESIAN_POINT ( 'NONE',  ( 0.6823417656249934904, 9.505208333674728394, 1.181850606188764807 ) ) ;
#68979 = ORIENTED_EDGE ( 'NONE', *, *, #25018, .T. ) ;
#68980 = CARTESIAN_POINT ( 'NONE',  ( 4.354103434560454566, 0.8146061972254794448, -1.730223316255767196 ) ) ;
#68981 = CARTESIAN_POINT ( 'NONE',  ( -2.300079615812729905, 5.835176651756807331, -0.7998128361456281477 ) ) ;
#68982 = COLOUR_RGB ( '', 0.40784314, 0.44705882, 0.49803922) ;
#68983 = CARTESIAN_POINT ( 'NONE',  ( 8.555358625423188812, 9.940005470203933768, 1.199719254218462483 ) ) ;
#68984 = CARTESIAN_POINT ( 'NONE',  ( 6.215297738502283842, -1.773692237561547147, -1.067698627785176768 ) ) ;
#68985 = CARTESIAN_POINT ( 'NONE',  ( 1.360316468749957597, 0.7760416670081096147, 0.7853790794158520550 ) ) ;
#68986 = CARTESIAN_POINT ( 'NONE',  ( 5.138177029454847222, 6.057256624861201644, 1.082531754730560403 ) ) ;
#68987 = FACE_OUTER_BOUND ( 'NONE', #58245, .T. ) ;
#68988 = CARTESIAN_POINT ( 'NONE',  ( 8.628817749835317130, 13.71606850217345119, -8.341300610551938277 ) ) ;
#68989 = CARTESIAN_POINT ( 'NONE',  ( -9.488968570712932760, -6.747343053191825923, 0.2633404184769590484 ) ) ;
#68990 = ORIENTED_EDGE ( 'NONE', *, *, #182079, .T. ) ;
#68991 = CARTESIAN_POINT ( 'NONE',  ( 4.951193585101709260, 7.980601645383334386, 1.044180363230226893 ) ) ;
#68992 = CARTESIAN_POINT ( 'NONE',  ( 3.110468855859845672, 1.357358932127524120, -1.287316363804760888 ) ) ;
#68993 = CARTESIAN_POINT ( 'NONE',  ( 7.991605200612358573, 8.288237253661408843, 0.7998128361456281477 ) ) ;
#68994 = PLANE ( 'NONE',  #26266 ) ;
#68995 = ADVANCED_FACE ( 'NONE', ( #106584 ), #55644, .F. ) ;
#68996 = CARTESIAN_POINT ( 'NONE',  ( -6.561783159334137139, 8.678499657355050800, -1.443375672974059665 ) ) ;
#68997 = CARTESIAN_POINT ( 'NONE',  ( -0.1757481403069499348, -0.8193859263425256056, -1.726394157293544840 ) ) ;
#68998 = CARTESIAN_POINT ( 'NONE',  ( 5.497994985541524215, 6.373081223675282736, -1.199719254218445830 ) ) ;
#68999 = CARTESIAN_POINT ( 'NONE',  ( 6.912946559606852226, -1.604190412254998810, 1.308348183162249434 ) ) ;
#69000 = CARTESIAN_POINT ( 'NONE',  ( 1.669546221992053603, 1.392560760841387246, 1.458543886677300394 ) ) ;
#69001 = CARTESIAN_POINT ( 'NONE',  ( -10.15913717534155047, 10.74674821418697057, 0.7998128361456462443 ) ) ;
#69002 = CARTESIAN_POINT ( 'NONE',  ( 6.801350335910821165, 7.963938809097990124, 1.199719254218452047 ) ) ;
#69003 = CARTESIAN_POINT ( 'NONE',  ( 2.310781476690497271, 5.467761476598782089, -0.5169845646830224517 ) ) ;
#69004 = CARTESIAN_POINT ( 'NONE',  ( 1.763894328224338448, 1.128481436294457740, 1.878420861880884862 ) ) ;
#69005 = CARTESIAN_POINT ( 'NONE',  ( 6.639283661800273961, -1.628176093627232479, 0.8261057939347239421 ) ) ;
#69006 = CARTESIAN_POINT ( 'NONE',  ( -4.295235737431041478, 3.905529869957963029, -0.7998128361456221525 ) ) ;
#69007 = CARTESIAN_POINT ( 'NONE',  ( 6.075462232699553766, 6.260663157670496304, -0.7216878364870458196 ) ) ;
#69008 = CARTESIAN_POINT ( 'NONE',  ( 8.940712233207955606, 12.51824914112961729, 1.199719254218450271 ) ) ;
#69009 = CARTESIAN_POINT ( 'NONE',  ( 3.680148631105580215, 6.380924938676771241, -1.199719254218446718 ) ) ;
#69010 = CARTESIAN_POINT ( 'NONE',  ( 3.444653546323793947, 6.176457016423196222, 1.199719254218451159 ) ) ;
#69011 = ORIENTED_EDGE ( 'NONE', *, *, #127553, .T. ) ;
#69013 = CARTESIAN_POINT ( 'NONE',  ( 0.1354021741525688050, -0.09674683032310191222, 2.010873914455484801 ) ) ;
#69012 = CARTESIAN_POINT ( 'NONE',  ( 3.368544699895597461, 0.04196216268675251326, -1.840931771443871101 ) ) ;
#69014 = CARTESIAN_POINT ( 'NONE',  ( 2.284880952019330280, -2.229702823797473865, 0.5573334316414603196 ) ) ;
#69016 = CARTESIAN_POINT ( 'NONE',  ( 0.7075644152179439983, 0.5912319408809820764, -1.764584214936999684 ) ) ;
#69015 = CARTESIAN_POINT ( 'NONE',  ( 3.389175213736292047, 5.937492935125556315, 1.082531754730558626 ) ) ;
#69017 = CARTESIAN_POINT ( 'NONE',  ( -3.475000000000000533, -0.3499999999999996447, 0.000000000000000000 ) ) ;
#69018 = CARTESIAN_POINT ( 'NONE',  ( -4.497554271431319250, 6.270232621468402989, -1.599625672291256295 ) ) ;
#69019 = FILL_AREA_STYLE_COLOUR ( '', #50257 ) ;
#69020 = CARTESIAN_POINT ( 'NONE',  ( 4.465046277278037934, -1.532637281380120564, 1.143568071694904598 ) ) ;
#69021 = CARTESIAN_POINT ( 'NONE',  ( -10.48453286206953727, 11.12637651536962125, 0.7998128361456462443 ) ) ;
#69022 = CARTESIAN_POINT ( 'NONE',  ( 6.381672224870991172, 6.819330018336470012, -0.5576268912585117254 ) ) ;
#69023 = CARTESIAN_POINT ( 'NONE',  ( -6.536439455564198475, 8.719208346281938304, 1.443375672974064550 ) ) ;
#69025 = CARTESIAN_POINT ( 'NONE',  ( 1.815107966846595255, -0.2319292346777863389, 1.856160199827073587 ) ) ;
#69024 = CARTESIAN_POINT ( 'NONE',  ( 3.439088004391201991, -1.584594249056283877, -1.364047514679037620 ) ) ;
#69026 = CARTESIAN_POINT ( 'NONE',  ( 8.920901888111997025, 10.47043562662792304, 1.082531754730549967 ) ) ;
#69027 = CARTESIAN_POINT ( 'NONE',  ( -6.609253696060815031, -8.104785249476799791, -6.824425546749153249 ) ) ;
#69028 = CARTESIAN_POINT ( 'NONE',  ( 3.438731153704393417, -1.320290108414169605, -1.134124902983554062 ) ) ;
#69029 = AXIS2_PLACEMENT_3D ( 'NONE', #35072, #16685, #32963 ) ;
#69030 = CARTESIAN_POINT ( 'NONE',  ( 4.684505768721569652, 5.424010470718658716, -1.199719254218452047 ) ) ;
#69031 = CARTESIAN_POINT ( 'NONE',  ( -5.570361349191150779, 5.866663122702686195, 0.5491554309224304653 ) ) ;
#69032 = CARTESIAN_POINT ( 'NONE',  ( 3.826516835200497457, 1.638561065401537897, 0.5390252620694930830 ) ) ;
#69033 = CARTESIAN_POINT ( 'NONE',  ( -6.581593504430098385, 9.765943957555402122, -1.199719254218440723 ) ) ;
#69034 = CARTESIAN_POINT ( 'NONE',  ( 3.597391730528697540, -0.6346259394694170330, 2.097678010650514402 ) ) ;
#69035 = CARTESIAN_POINT ( 'NONE',  ( 6.375609195709820654, 2.113139023092651225, -0.6363509056886568205 ) ) ;
#69036 = CARTESIAN_POINT ( 'NONE',  ( 4.083024739667787451, 2.059781850948108506, 0.6862965400120830672 ) ) ;
#69037 = CARTESIAN_POINT ( 'NONE',  ( 1.910518402784128433, 1.353611321597010253, -1.225282022559864625 ) ) ;
#69038 = DIRECTION ( 'NONE',  ( 1.000000000000000000, -0.000000000000000000, -0.000000000000000000 ) ) ;
#69039 = CARTESIAN_POINT ( 'NONE',  ( 5.770749444886737578, -0.3132382886438951908, -2.093953712743265694 ) ) ;
#69040 = EDGE_LOOP ( 'NONE', ( #83118, #125798 ) ) ;
#69042 = CARTESIAN_POINT ( 'NONE',  ( 0.6823417656249882723, 2.738541667008084879, -1.181850606188749264 ) ) ;
#69041 = CARTESIAN_POINT ( 'NONE',  ( 6.427265082780700745, -1.493544900618107185, -1.739104490089713462 ) ) ;
#69043 = CARTESIAN_POINT ( 'NONE',  ( 6.720655732516646275, 4.698042323276835575, 2.488944259588221186 ) ) ;
#69044 = CARTESIAN_POINT ( 'NONE',  ( 3.728655938958122196, 4.308852335994623139, -1.199719254218446718 ) ) ;
#69045 = CARTESIAN_POINT ( 'NONE',  ( 1.401209248766785542, -0.3145075555085960484, -2.096923750572597722 ) ) ;
#69046 = CARTESIAN_POINT ( 'NONE',  ( -4.446711195602252253, 6.210915699667823198, -1.443375672974053447 ) ) ;
#69047 = CIRCLE ( 'NONE', #20663, 6.961139734775127152 ) ;
#69048 = CARTESIAN_POINT ( 'NONE',  ( 5.844973620822802474, 5.991759777147735555, 0.7216878364870634721 ) ) ;
#69049 = CARTESIAN_POINT ( 'NONE',  ( -5.219525951136850139, 7.112532914458205013, -1.443375672974051449 ) ) ;
#69051 = CARTESIAN_POINT ( 'NONE',  ( 1.499999999999997113, 12.17708333401613352, -0.8660254037844378194 ) ) ;
#69050 = CARTESIAN_POINT ( 'NONE',  ( 6.883263157960358924, 7.052235917045241997, 2.651962373728885325 ) ) ;
#69052 = VERTEX_POINT ( 'NONE', #140128 ) ;
#69053 = CARTESIAN_POINT ( 'NONE',  ( 6.539686446881147752, -1.556848207870220602, 1.281141925495055123 ) ) ;
#69055 = CARTESIAN_POINT ( 'NONE',  ( 4.856332268735650715, -2.061987677746464076, -0.05593471103338721467 ) ) ;
#69054 = CARTESIAN_POINT ( 'NONE',  ( 3.649115900372475796, 7.409052317076538330, 1.040834085586084257E-14 ) ) ;
#69057 = CARTESIAN_POINT ( 'NONE',  ( 0.000000000000000000, -3.237499999999997602, -4.012584370867899430 ) ) ;
#69056 = CARTESIAN_POINT ( 'NONE',  ( 7.340813827156391191, 7.528980651296110160, 0.7998128361456281477 ) ) ;
#69058 = CARTESIAN_POINT ( 'NONE',  ( 5.365994935958575240, 9.482354201918870018, 0.7998128361456341429 ) ) ;
#69059 = CARTESIAN_POINT ( 'NONE',  ( 3.285556943749998737, -0.9552083328553737651, -1.896917185911906500 ) ) ;
#69060 = CARTESIAN_POINT ( 'NONE',  ( -0.5000000000000108802, 3.950000000000001954, -0.5000000000000091038 ) ) ;
#69061 = CARTESIAN_POINT ( 'NONE',  ( 0.7969595931820300239, 1.710167217185576183, 1.202247156440580556 ) ) ;
#69062 = CARTESIAN_POINT ( 'NONE',  ( 4.588517629802620235, -0.5350896943857390564, 1.944070981013111155 ) ) ;
#69063 = CARTESIAN_POINT ( 'NONE',  ( 4.300242120186610784, 1.420457692841030850, -1.171515996850613694 ) ) ;
#69064 = CARTESIAN_POINT ( 'NONE',  ( 7.169564303528210836, 7.258913197071374945, -0.7998128361456281477 ) ) ;
#69065 = SURFACE_STYLE_USAGE ( .BOTH. , #21379 ) ;
#69066 = CARTESIAN_POINT ( 'NONE',  ( 0.4633286609967076086, 1.707074611214503435, -0.2455724507211871910 ) ) ;
#69067 = CARTESIAN_POINT ( 'NONE',  ( 0.2511858651975951151, 0.1928294586405615574, -2.007256720055437871 ) ) ;
#69068 = CARTESIAN_POINT ( 'NONE',  ( 1.003029240585759263, -2.241230121681879073, 0.5102270476868026039 ) ) ;
#69069 = CARTESIAN_POINT ( 'NONE',  ( -4.726989112658928072, 8.666571064744069020, 1.040834085586084257E-14 ) ) ;
#69070 = CARTESIAN_POINT ( 'NONE',  ( 1.757462551082995095, -1.940025152074912551, -1.163771565304895450 ) ) ;
#69071 = CARTESIAN_POINT ( 'NONE',  ( 2.754625382576633807, 0.7102545713932090221, 1.982823988820613170 ) ) ;
#69072 = CARTESIAN_POINT ( 'NONE',  ( -5.798046968499580345, 6.793418213784815585, 1.199719254218452935 ) ) ;
#69073 = CARTESIAN_POINT ( 'NONE',  ( 6.089583550832340819, 10.25626457594641749, 1.040834085586084257E-14 ) ) ;
#69074 = CARTESIAN_POINT ( 'NONE',  ( 5.017926250389229459, 8.868348035513836436, 0.000000000000000000 ) ) ;
#69075 = FILL_AREA_STYLE_COLOUR ( '', #48610 ) ;
#69076 = CARTESIAN_POINT ( 'NONE',  ( -6.437424008390261854, 6.404749519410410485, 0.7998128361456341429 ) ) ;
#69077 = CARTESIAN_POINT ( 'NONE',  ( 7.117667457050084856, 7.406292909420979953, -0.7216878364870257245 ) ) ;
#69078 = CARTESIAN_POINT ( 'NONE',  ( 4.618624277135228162, 7.133842259902017702, 1.345135577604664512 ) ) ;
#69079 = CARTESIAN_POINT ( 'NONE',  ( -3.327636637150278798, 5.969660945728899826, -1.199719254218452935 ) ) ;
#69080 = CARTESIAN_POINT ( 'NONE',  ( 4.781579470667713494, 0.2167243770262658464, -2.210780252931910717 ) ) ;
#69081 = CARTESIAN_POINT ( 'NONE',  ( 2.783357461837578484, 1.550338952211056220, 1.549093164327268068 ) ) ;
#69082 = CARTESIAN_POINT ( 'NONE',  ( -6.084912014434944894, 5.993485526462540847, -0.7998128361456291469 ) ) ;
#69083 = CARTESIAN_POINT ( 'NONE',  ( -5.144392941742557568, 4.966489618313220333, -0.7998128361456362523 ) ) ;
#69084 = CARTESIAN_POINT ( 'NONE',  ( 5.617619635959271385, 0.3843197845415853853, -1.923678648292715732 ) ) ;
#69085 = CARTESIAN_POINT ( 'NONE',  ( 0.6823417656249899377, 1.592708333674752730, 1.181850606188755259 ) ) ;
#69086 = CARTESIAN_POINT ( 'NONE',  ( 6.890000000000015667, 0.5768591945385994624, 2.052260346930290247 ) ) ;
#69087 = CARTESIAN_POINT ( 'NONE',  ( -3.795919822146277767, 7.372397525905215687, -0.7216878364870267237 ) ) ;
#69088 = CARTESIAN_POINT ( 'NONE',  ( 5.115537534566190203, 1.735013203181461350, 1.219038288318145646 ) ) ;
#69089 = CARTESIAN_POINT ( 'NONE',  ( -7.621091744657483069, 8.063897588288083895, 0.7216878364870317197 ) ) ;
#69090 = VERTEX_POINT ( 'NONE', #125004 ) ;
#69092 = CARTESIAN_POINT ( 'NONE',  ( -1.500000000000079936, 7.268077025657370349, 4.207854987879517950 ) ) ;
#69091 = CARTESIAN_POINT ( 'NONE',  ( -6.468648687495877958, 6.719380688266201496, 0.000000000000000000 ) ) ;
#69093 = CARTESIAN_POINT ( 'NONE',  ( 7.169564303528210836, 7.258913197071374945, -0.7998128361456281477 ) ) ;
#69094 = CARTESIAN_POINT ( 'NONE',  ( 5.407694413872749628, -0.8332299576223768378, -1.642021276980778932 ) ) ;
#69095 = CARTESIAN_POINT ( 'NONE',  ( 0.1007326007325878847, -9.919999999999998153, 10.99953876047308476 ) ) ;
#69096 = CARTESIAN_POINT ( 'NONE',  ( -1.201851678989727383E-14, 2.759375000341417916, -1.575800808251660134 ) ) ;
#69097 = CARTESIAN_POINT ( 'NONE',  ( 0.8721245864499425071, -0.04093463707061052725, -1.740139661330299514 ) ) ;
#69098 = CARTESIAN_POINT ( 'NONE',  ( 11.94105721237523277, 10.90000000000000036, -1.187919463087249827 ) ) ;
#69099 = CARTESIAN_POINT ( 'NONE',  ( 1.364683531249988757, -0.8031249996585804185, 0.000000000000000000 ) ) ;
#69100 = CARTESIAN_POINT ( 'NONE',  ( -0.4336004510535704792, 3.058108253035755730, 0.4198436715060500091 ) ) ;
#69102 = ADVANCED_FACE ( 'NONE', ( #39398 ), #37836, .F. ) ;
#69101 = PRESENTATION_LAYER_ASSIGNMENT (  '', '', ( #20712 ) ) ;
#69103 = CARTESIAN_POINT ( 'NONE',  ( 5.489210439962995736, 1.908424935776025455, -1.015307555102950010 ) ) ;
#69104 = CARTESIAN_POINT ( 'NONE',  ( -4.243865776277440993, 4.909930479533815451, -1.199719254218446718 ) ) ;
#69105 = CARTESIAN_POINT ( 'NONE',  ( -7.659993601596720936, 8.999375959026737704, -1.082531754730543083 ) ) ;
#69106 = CARTESIAN_POINT ( 'NONE',  ( 4.153314892778156242, -1.795761387672462961, -1.203114871582221079 ) ) ;
#69107 = CARTESIAN_POINT ( 'NONE',  ( -1.201851678989727383E-14, 2.696875000341417916, -1.575800808251660134 ) ) ;
#69108 = CARTESIAN_POINT ( 'NONE',  ( 4.305907937463241630, -1.966273716216637046, 0.1420514027590073225 ) ) ;
#69109 = CARTESIAN_POINT ( 'NONE',  ( 4.253097392439049607, -1.714905526014463666, -0.2545648513426115311 ) ) ;
#69110 = CARTESIAN_POINT ( 'NONE',  ( 0.5916818631664167993, -0.7834642122952638621, 2.046923429677327100 ) ) ;
#69111 = CARTESIAN_POINT ( 'NONE',  ( 2.116686800396328838, -1.088458544310743736, -2.034734824932447506 ) ) ;
#69112 = CARTESIAN_POINT ( 'NONE',  ( 4.921196286130338216, -0.1051130969715245306, 2.058245376175421804 ) ) ;
#69113 = CARTESIAN_POINT ( 'NONE',  ( 6.444875487053635332, -1.562622460104126310, -1.153009275138028089 ) ) ;
#69114 = CARTESIAN_POINT ( 'NONE',  ( -5.856759170979136897, 9.776710099543576504, 0.000000000000000000 ) ) ;
#69115 = CARTESIAN_POINT ( 'NONE',  ( -6.493429226302317225, 6.540365283632955773, 0.7998128361456341429 ) ) ;
#69116 = CARTESIAN_POINT ( 'NONE',  ( 0.000000000000000000, 6.999999999999999112, 0.000000000000000000 ) ) ;
#69117 = CARTESIAN_POINT ( 'NONE',  ( 4.716359525368828436E-16, 1.899999999999999023, -2.650000000000008349 ) ) ;
#69118 = CARTESIAN_POINT ( 'NONE',  ( 0.9674229098759130618, -1.967888300253183953, -0.4390273639364171698 ) ) ;
#69119 = CARTESIAN_POINT ( 'NONE',  ( -7.334597914868741242, 8.619747657844088806, -1.082531754730543083 ) ) ;
#69120 = CARTESIAN_POINT ( 'NONE',  ( 3.786314268594536347, -1.089870966172037825, 1.918795532666245363 ) ) ;
#69121 = CARTESIAN_POINT ( 'NONE',  ( -3.285556943749998737, -1.217708332855376607, 1.896917185911908499 ) ) ;
#69122 = CARTESIAN_POINT ( 'NONE',  ( 0.6548463511123479019, 1.551493821935068906, -1.027296181188163571 ) ) ;
#69123 = CARTESIAN_POINT ( 'NONE',  ( 1.456019627564700825, 3.350498733230925286, -0.3924612876561414665 ) ) ;
#69124 = CARTESIAN_POINT ( 'NONE',  ( 6.539320575229249144, 0.007148032025052972194, 1.896977914940492393 ) ) ;
#69125 = CARTESIAN_POINT ( 'NONE',  ( 5.300027894412070673, 4.752150942167815195, -2.500000000000000444 ) ) ;
#69127 = CARTESIAN_POINT ( 'NONE',  ( 6.925078400183550364, 3.684205305355064297, 2.658256427561227486 ) ) ;
#69126 = CARTESIAN_POINT ( 'NONE',  ( -5.345048817422858534, 7.707963373851138833, -1.327269471787644317 ) ) ;
#69128 = CARTESIAN_POINT ( 'NONE',  ( 11.94105721237522921, 13.52740390989733221, 1.187919463087248273 ) ) ;
#69129 = ORIENTED_EDGE ( 'NONE', *, *, #77767, .F. ) ;
#69130 = CARTESIAN_POINT ( 'NONE',  ( 3.538010501442095723, 0.9279861380482921085, -1.840221436749614803 ) ) ;
#69131 = CARTESIAN_POINT ( 'NONE',  ( 1.360316468749981800, 1.744791667008098290, 0.7853790794158680422 ) ) ;
#69132 = CARTESIAN_POINT ( 'NONE',  ( -7.067878151425722955, 7.140279352951794500, 0.7998128361456341429 ) ) ;
#69133 = CARTESIAN_POINT ( 'NONE',  ( 2.051431352050979040, -1.803145959232739237, 0.9099833227969624794 ) ) ;
#69134 = CARTESIAN_POINT ( 'NONE',  ( -1.500000000000013101, 0.1708333333333560411, 0.8660254037844403729 ) ) ;
#69135 = CARTESIAN_POINT ( 'NONE',  ( 4.196412238629597447, 4.854568018944682706, -1.199719254218452047 ) ) ;
#69136 = CARTESIAN_POINT ( 'NONE',  ( 1.674756777405971064, -1.956562173829911044, -0.6475767382677873885 ) ) ;
#69138 = CARTESIAN_POINT ( 'NONE',  ( -1.364683531250010295, 13.88020833367473195, 0.7879004041258445001 ) ) ;
#69137 = DIRECTION ( 'NONE',  ( 2.486899575160350966E-14, 0.000000000000000000, -1.000000000000000000 ) ) ;
#69139 = CARTESIAN_POINT ( 'NONE',  ( 5.296431564432884542, 9.330920591813708143, 1.040834085586084257E-14 ) ) ;
#69140 = STYLED_ITEM ( 'NONE', ( #127541 ), #176823 ) ;
#69141 = CARTESIAN_POINT ( 'NONE',  ( -0.1411974294642098227, 4.091293698307607585, -2.455098582995118406 ) ) ;
#69142 = EDGE_CURVE ( 'NONE', #77381, #147625, #134586, .T. ) ;
#69143 = CARTESIAN_POINT ( 'NONE',  ( 5.408869034151480903, 1.673104959687292448, -1.439203791633147267 ) ) ;
#69144 = CARTESIAN_POINT ( 'NONE',  ( 1.370646902836635261, -1.372427557409527488, 1.669970663979184256 ) ) ;
#69145 = CARTESIAN_POINT ( 'NONE',  ( -3.633221978782283923, 7.182583375313884133, -0.7216878364870267237 ) ) ;
#69146 = CARTESIAN_POINT ( 'NONE',  ( 0.5324358445358172709, 0.5899921999869184308, 1.928256190492839028 ) ) ;
#69147 = CARTESIAN_POINT ( 'NONE',  ( 2.161834534229470695, -0.6120774379556602751, -2.215351195248612459 ) ) ;
#69148 = FACE_OUTER_BOUND ( 'NONE', #14547, .T. ) ;
#69149 = CARTESIAN_POINT ( 'NONE',  ( -0.02081124878883705218, 7.037281880797342737, 4.016375841068750674 ) ) ;
#69150 = CARTESIAN_POINT ( 'NONE',  ( 1.880823357903570248, 8.986349088233119176, -0.7749999999999996891 ) ) ;
#69151 = CARTESIAN_POINT ( 'NONE',  ( 1.885419139999934934, 1.287927767047767125, 1.356919574424742203 ) ) ;
#69152 = CARTESIAN_POINT ( 'NONE',  ( 4.012907874177486178, 0.1037781579101039742, 2.014008197856680393 ) ) ;
#69155 = ADVANCED_FACE ( 'NONE', ( #183290 ), #198459, .F. ) ;
#69154 = CARTESIAN_POINT ( 'NONE',  ( 3.469446951953614189E-15, 6.400000000000023448, 1.214306433183764966E-14 ) ) ;
#69153 = CARTESIAN_POINT ( 'NONE',  ( 1.364683531249988757, 1.634375000341421691, 0.000000000000000000 ) ) ;
#69157 = CARTESIAN_POINT ( 'NONE',  ( 4.828798294617491216, 2.015104956129540881, 0.6122756557535751210 ) ) ;
#69156 = CARTESIAN_POINT ( 'NONE',  ( -6.665805079413154921, 10.92852302595736447, 0.7998128361456481317 ) ) ;
#69158 = CARTESIAN_POINT ( 'NONE',  ( 7.039708073993665494, 9.236078724457858158, 1.599625672291281386 ) ) ;
#69159 = CARTESIAN_POINT ( 'NONE',  ( -6.958359152311683893, 9.141171649162195934, -1.599625672291263179 ) ) ;
#69160 = CARTESIAN_POINT ( 'NONE',  ( -0.003376046620579863274, -7.161464053357567749, -9.586610838029415049 ) ) ;
#69161 = CARTESIAN_POINT ( 'NONE',  ( 5.414321571020942692, -2.019972751022606872, 0.004158903309840755735 ) ) ;
#69162 = CARTESIAN_POINT ( 'NONE',  ( 0.7499999999999867883, -0.4020833326505157679, -1.299038105676652899 ) ) ;
#69163 = CARTESIAN_POINT ( 'NONE',  ( 0.8661725458788569476, -2.052963606700756394, 0.1985000389403013821 ) ) ;
#69164 = CARTESIAN_POINT ( 'NONE',  ( 8.934460041725669655, 9.525884258209195821, 1.040834085586084257E-14 ) ) ;
#69165 = CARTESIAN_POINT ( 'NONE',  ( 5.397027666691686321, 8.454226823519094935, 1.199719254218451159 ) ) ;
#69166 = CARTESIAN_POINT ( 'NONE',  ( 4.715203562502613188, 8.723097599553565118, 0.7998128361456341429 ) ) ;
#69167 = CARTESIAN_POINT ( 'NONE',  ( -1.201851678989727383E-14, 1.134375000341418582, 1.575800808251672791 ) ) ;
#69169 = DIRECTION ( 'NONE',  ( 1.000000000000000000, -5.578564026256504688E-16, 0.000000000000000000 ) ) ;
#69168 = CARTESIAN_POINT ( 'NONE',  ( 4.878955176071345434, 6.785476686873604280, -1.599625672291269396 ) ) ;
#69170 = CARTESIAN_POINT ( 'NONE',  ( 6.548225005276093746, 9.623051025255367819, -1.082531754730537976 ) ) ;
#69172 = CARTESIAN_POINT ( 'NONE',  ( -3.627759838191260577, 3.517451378710267029, -2.499999999999886757 ) ) ;
#69171 = CARTESIAN_POINT ( 'NONE',  ( 3.332658328316660423, -1.295540365661397297, 1.742140367482351238 ) ) ;
#69174 = CARTESIAN_POINT ( 'NONE',  ( 1.540310226958538475, -1.555040833713853710, 0.9856339240054690087 ) ) ;
#69173 = CARTESIAN_POINT ( 'NONE',  ( -3.795919822146283540, 6.412028311603867436, -1.082531754730549967 ) ) ;
#69175 = CARTESIAN_POINT ( 'NONE',  ( -1.201851678989727383E-14, 3.946875000341423689, -1.575800808251660134 ) ) ;
#69176 = CARTESIAN_POINT ( 'NONE',  ( 4.335597073515660149, 0.9364531651635084053, -1.981528385891350386 ) ) ;
#69177 = CARTESIAN_POINT ( 'NONE',  ( 6.983263157960391432, 4.691677264508577139, 2.616375093613742209 ) ) ;
#69178 = CARTESIAN_POINT ( 'NONE',  ( 5.278307949308306490, -1.261584246701217715, 1.877956315871305071 ) ) ;
#69179 = CARTESIAN_POINT ( 'NONE',  ( -6.878064000834399394, 6.918829510595249310, -0.7998128361456291469 ) ) ;
#69180 = FACE_OUTER_BOUND ( 'NONE', #13047, .T. ) ;
#69181 = CARTESIAN_POINT ( 'NONE',  ( 4.701115458738250652, 8.361069499448168685, -0.6471830670988186762 ) ) ;
#69182 = CARTESIAN_POINT ( 'NONE',  ( 0.7500000000000006661, 14.08333333333333570, 1.299038105676657340 ) ) ;
#69183 = CARTESIAN_POINT ( 'NONE',  ( -6.739811759324840779, 7.035737605399991601, -0.7216878364870338292 ) ) ;
#69184 = CARTESIAN_POINT ( 'NONE',  ( 5.750066545971570520, 5.881034856487848295, -0.7216878364870458196 ) ) ;
#69185 = CARTESIAN_POINT ( 'NONE',  ( 5.887929786387328335, -0.7941975946151798027, 1.581623468068603433 ) ) ;
#69186 = CARTESIAN_POINT ( 'NONE',  ( 3.211590615979207364, 1.588433223196554778, 1.236618793847492626 ) ) ;
#69187 = CARTESIAN_POINT ( 'NONE',  ( 7.446452682403650769, 9.710614100936176385, -1.599625672291262513 ) ) ;
#69188 = CARTESIAN_POINT ( 'NONE',  ( 2.098786246049421766, -0.5609894644466472124, -2.029802036486601846 ) ) ;
#69190 = CARTESIAN_POINT ( 'NONE',  ( 1.499999999999987121, 2.045833333333356929, -0.8660254037844262731 ) ) ;
#69189 = CARTESIAN_POINT ( 'NONE',  ( -1.364683531250014514, 11.83854166700806587, -0.7879004041258335089 ) ) ;
#69191 = CARTESIAN_POINT ( 'NONE',  ( 2.101947443238092017, 0.7566099462053441638, -1.818632640566263614 ) ) ;
#69192 = DIRECTION ( 'NONE',  ( 0.000000000000000000, 0.000000000000000000, 1.000000000000000000 ) ) ;
#69193 = CARTESIAN_POINT ( 'NONE',  ( 0.4319881149899909567, 1.126445828788334991, 1.606065282034954578 ) ) ;
#69195 = EDGE_LOOP ( 'NONE', ( #33188, #13487, #140415, #126451 ) ) ;
#69194 = CARTESIAN_POINT ( 'NONE',  ( 6.152603492317154199, 1.793228361101945056, 0.2563216274220745938 ) ) ;
#69196 = CARTESIAN_POINT ( 'NONE',  ( 4.826339496784873617, 8.574553812983598533, -0.7216878364870257245 ) ) ;
#69197 = CARTESIAN_POINT ( 'NONE',  ( 0.6823417656249864960, -1.011458332991911568, -1.181850606188749264 ) ) ;
#69198 = CIRCLE ( 'NONE', #103721, 0.7499999999999997780 ) ;
#69199 = CARTESIAN_POINT ( 'NONE',  ( 6.297708355432167338, -0.6282832542035889922, 1.762108908958268216 ) ) ;
#69200 = CARTESIAN_POINT ( 'NONE',  ( 4.390142812726693045, 4.016254791136236513, 1.214306433183764966E-14 ) ) ;
#69201 = CARTESIAN_POINT ( 'NONE',  ( 8.581532217057311840, 3.975933801733725126, 7.726846314510468439 ) ) ;
#69202 = CARTESIAN_POINT ( 'NONE',  ( 5.612195314557796522, 2.068136773602911038, -0.09592777784667855245 ) ) ;
#69203 = CARTESIAN_POINT ( 'NONE',  ( 0.6124999999999914957, 2.583333333333347248, 1.060881119635894487 ) ) ;
#69204 = CARTESIAN_POINT ( 'NONE',  ( -4.299344108864953995, 7.069632989434141201, -1.082531754730551743 ) ) ;
#69205 = DIRECTION ( 'NONE',  ( -1.276756478318932585E-15, 1.000000000000000000, -1.665334536937738262E-16 ) ) ;
#69206 = CARTESIAN_POINT ( 'NONE',  ( 0.7499999999999885647, -0.01666666666664401442, 1.299038105676657340 ) ) ;
#69207 = CARTESIAN_POINT ( 'NONE',  ( 6.740374924288304648, 11.01552117831172062, 1.040834085586084257E-14 ) ) ;
#69208 = CARTESIAN_POINT ( 'NONE',  ( -9.352427035328430449, 9.805586384171650849, 1.040834085586084257E-14 ) ) ;
#69209 = CARTESIAN_POINT ( 'NONE',  ( 7.205232291019763480, 7.370802192470005565, -0.7998128361456341429 ) ) ;
#69210 = CARTESIAN_POINT ( 'NONE',  ( 1.364683531249988757, 1.384375000341421469, 0.000000000000000000 ) ) ;
#69211 = ORIENTED_EDGE ( 'NONE', *, *, #145312, .F. ) ;
#69212 = CARTESIAN_POINT ( 'NONE',  ( -1.500000000000015099, 0.8791666666666874130, -0.8660254037844313801 ) ) ;
#69214 = CARTESIAN_POINT ( 'NONE',  ( 4.172158584703322681, 5.890604320285754980, -1.599625672291256295 ) ) ;
#69213 = CARTESIAN_POINT ( 'NONE',  ( 4.967221142815226642, 1.706001049663580460, 0.9686458024478412643 ) ) ;
#69215 = CARTESIAN_POINT ( 'NONE',  ( 3.427111092251767133, 0.9039706872599994059, 1.802141633730186543 ) ) ;
#69216 = CARTESIAN_POINT ( 'NONE',  ( 2.430754934859931549, -1.590173441703069956, 1.067998681346548961 ) ) ;
#69217 = DIRECTION ( 'NONE',  ( 1.000000000000000000, -0.000000000000000000, 1.224646799147353207E-16 ) ) ;
#69218 = CARTESIAN_POINT ( 'NONE',  ( 0.5213437761196969555, -2.079166062760181788, 0.6930039600180629700 ) ) ;
#69219 = CARTESIAN_POINT ( 'NONE',  ( 0.1331715793776418189, 1.377430125279802686, -2.211494238769554865 ) ) ;
#69220 = CARTESIAN_POINT ( 'NONE',  ( 3.321420150926617687, -1.803644938814071175, 0.4956094624995326381 ) ) ;
#69221 = CARTESIAN_POINT ( 'NONE',  ( -0.7500000000000249800, -1.027083332650516212, 1.299038105676659116 ) ) ;
#69222 = CARTESIAN_POINT ( 'NONE',  ( 4.218997895827368616, 1.553599190986540091, -1.280318274872578543 ) ) ;
#69223 = CARTESIAN_POINT ( 'NONE',  ( -6.645467848992654858, 10.90479625713344625, 0.7998128361456481317 ) ) ;
#69225 = CARTESIAN_POINT ( 'NONE',  ( 4.042653799040228257, -1.567611697763098055, 1.423267961261857950 ) ) ;
#69224 = CARTESIAN_POINT ( 'NONE',  ( -4.270455198624581783, 7.926022131796578662, 1.040834085586084257E-14 ) ) ;
#69227 = EDGE_CURVE ( 'NONE', #135649, #66179, #172030, .T. ) ;
#69226 = CARTESIAN_POINT ( 'NONE',  ( -0.09916492693102199607, -10.00000000000016520, -9.499482423651642193 ) ) ;
#69228 = CARTESIAN_POINT ( 'NONE',  ( 5.582505937350194181, 1.236201877336528643, -1.660625051266072960 ) ) ;
#69230 = CARTESIAN_POINT ( 'NONE',  ( 6.720655732516649827, 2.940181725866806151, 2.725612257524675730 ) ) ;
#69229 = CARTESIAN_POINT ( 'NONE',  ( 1.171554334673271303, 1.248344470866637135, 1.676987088486236566 ) ) ;
#69232 = ORIENTED_EDGE ( 'NONE', *, *, #25480, .T. ) ;
#69231 = CARTESIAN_POINT ( 'NONE',  ( 6.545924712158827319, 0.6954503440314525609, -1.688125835592364066 ) ) ;
#69233 = CARTESIAN_POINT ( 'NONE',  ( 7.507464373665139412, 9.781794407407920389, 1.599625672291281386 ) ) ;
#69234 =( LENGTH_UNIT ( ) NAMED_UNIT ( * ) SI_UNIT ( .MILLI., .METRE. ) );
#69235 = CARTESIAN_POINT ( 'NONE',  ( -9.706334639731263536, 5.108299517166001280, 6.477055075394225092 ) ) ;
#69236 = CARTESIAN_POINT ( 'NONE',  ( 5.612712405933139692, 9.491988873656591608, 1.040834085586084257E-14 ) ) ;
#69237 = CARTESIAN_POINT ( 'NONE',  ( -15.75000000000000000, 10.19999999999998153, 1.399999999999998579 ) ) ;
#69239 = CARTESIAN_POINT ( 'NONE',  ( 0.6799528615496954753, 0.8915946574989388473, 1.576789060086491778 ) ) ;
#69238 = CARTESIAN_POINT ( 'NONE',  ( 6.373214726875630731, 9.593111727067046957, 1.199719254218452047 ) ) ;
#69240 = CARTESIAN_POINT ( 'NONE',  ( -6.659026002606323047, 10.92061410301605662, 0.000000000000000000 ) ) ;
#69241 = CARTESIAN_POINT ( 'NONE',  ( 5.331380718671758778, 7.243030143248949670, -1.599625672291256295 ) ) ;
#69242 = CARTESIAN_POINT ( 'NONE',  ( 6.013923656113508542, 9.173938811177871244, -1.199719254218452047 ) ) ;
#69243 = DIRECTION ( 'NONE',  ( 0.000000000000000000, 1.000000000000000000, 0.000000000000000000 ) ) ;
#69244 = FACE_OUTER_BOUND ( 'NONE', #131664, .T. ) ;
#69245 = CARTESIAN_POINT ( 'NONE',  ( 9.083599731475976213, 12.58098820582193689, 1.082531754730546636 ) ) ;
#69246 = ORIENTED_EDGE ( 'NONE', *, *, #208932, .F. ) ;
#69247 = MECHANICAL_DESIGN_GEOMETRIC_PRESENTATION_REPRESENTATION (  '', ( #131643 ), #103922 ) ;
#69248 = CARTESIAN_POINT ( 'NONE',  ( 6.046499952770106212, -1.423952032562772807, 1.427948417171531759 ) ) ;
#69249 = CARTESIAN_POINT ( 'NONE',  ( 0.3465379015402513252, 1.086389676674501148, -1.820904993421072371 ) ) ;
#69250 = CARTESIAN_POINT ( 'NONE',  ( 0.8018101603110124875, -8.116362469078496434E-15, -0.9920850708466935064 ) ) ;
#69251 = CARTESIAN_POINT ( 'NONE',  ( 0.1405533004714799583, 4.081756738537394291, -2.834601852798774413 ) ) ;
#69252 = DIRECTION ( 'NONE',  ( -6.695352868347761696E-17, 0.000000000000000000, -1.000000000000000000 ) ) ;
#69253 = CARTESIAN_POINT ( 'NONE',  ( -3.253593677599670109, 5.779314476299451719, 1.082531754730560403 ) ) ;
#69254 = CARTESIAN_POINT ( 'NONE',  ( 7.782016984564043227, 12.02284421539267356, 0.7216878364870438212 ) ) ;
#69255 = CARTESIAN_POINT ( 'NONE',  ( 3.274220328336883146, -0.9665011448860871823, -1.715865690870149285 ) ) ;
#69256 = CARTESIAN_POINT ( 'NONE',  ( 4.991814629660241920, -2.006445540622634915, 0.2004526995145126111 ) ) ;
#69257 = CARTESIAN_POINT ( 'NONE',  ( -5.018489415352746619, 9.006654751220198207, 0.7998128361456481317 ) ) ;
#69258 =( NAMED_UNIT ( * ) SI_UNIT ( $, .STERADIAN. ) SOLID_ANGLE_UNIT ( ) );
#69259 = CARTESIAN_POINT ( 'NONE',  ( -1.115562610750309283E-14, 9.812500000000000000, 1.500000000000001554 ) ) ;
#69260 = CARTESIAN_POINT ( 'NONE',  ( 4.347736757272718577, 2.190986304709115373, -0.05254992341368477232 ) ) ;
#69261 = CARTESIAN_POINT ( 'NONE',  ( 3.930962900855079489, 2.807348321460013452, 0.7750000000000135669 ) ) ;
#69262 = CARTESIAN_POINT ( 'NONE',  ( 3.838824069632059910, 0.2817418319709265040, 1.905555271966542952 ) ) ;
#69263 = CARTESIAN_POINT ( 'NONE',  ( -8.193204901359996128, 8.453160561208463264, 1.040834085586084257E-14 ) ) ;
#69264 = CARTESIAN_POINT ( 'NONE',  ( -0.1296875068448125334, 2.048176110289974261, -2.243787855586779401 ) ) ;
#69265 = CARTESIAN_POINT ( 'NONE',  ( 0.08304785351339466493, -2.141800023564765620, -0.5316218738360134477 ) ) ;
#69266 = SURFACE_STYLE_USAGE ( .BOTH. , #3195 ) ;
#69267 = ORIENTED_EDGE ( 'NONE', *, *, #147671, .F. ) ;
#69268 = CARTESIAN_POINT ( 'NONE',  ( 3.255366281057017197, 6.812028071292901998, -0.7216878364870338292 ) ) ;
#69269 = CARTESIAN_POINT ( 'NONE',  ( 5.330891317213126257, -1.853047821147445484, -0.6673286768130722857 ) ) ;
#69271 = CARTESIAN_POINT ( 'NONE',  ( 3.914701103513482661, -0.6334807629873323576, -1.910874176753782461 ) ) ;
#69270 = CARTESIAN_POINT ( 'NONE',  ( 0.6439600106935819968, 0.5648315236305987419, 1.858087668232853984 ) ) ;
#69272 = CARTESIAN_POINT ( 'NONE',  ( 5.993622264137510314, 2.212772176713458716, 0.6212890515704305727 ) ) ;
#69274 = CARTESIAN_POINT ( 'NONE',  ( 4.873795578896718439, -1.825537460381383870, 0.3603196638213671532 ) ) ;
#69273 = CARTESIAN_POINT ( 'NONE',  ( -6.312203035614172286, 9.521931420595302953, -1.199719254218452047 ) ) ;
#69275 = CARTESIAN_POINT ( 'NONE',  ( 7.309781096423290769, 8.557108029695882578, 1.199719254218452935 ) ) ;
#69276 = FACE_BOUND ( 'NONE', #161351, .T. ) ;
#69277 =( NAMED_UNIT ( * ) PLANE_ANGLE_UNIT ( ) SI_UNIT ( $, .RADIAN. ) );
#69278 = CARTESIAN_POINT ( 'NONE',  ( -5.669280788808708671, 9.765911353585494226, 0.7998128361456481317 ) ) ;
#69279 = CARTESIAN_POINT ( 'NONE',  ( -4.014622883422336308, 5.777089012116397804, -1.443375672974066548 ) ) ;
#69280 = CARTESIAN_POINT ( 'NONE',  ( 0.8729168595149154886, -0.05911722906676297740, -2.190938979806676734 ) ) ;
#69281 = CARTESIAN_POINT ( 'NONE',  ( 3.226477370372293763, 6.708047998835573900, 0.7216878364870317197 ) ) ;
#69282 = ORIENTED_EDGE ( 'NONE', *, *, #17805, .T. ) ;
#69283 = SURFACE_SIDE_STYLE ('',( #73572 ) ) ;
#69284 = CYLINDRICAL_SURFACE ( 'NONE', #103195, 0.07999999999999954370 ) ;
#69285 = CARTESIAN_POINT ( 'NONE',  ( 0.5569169099325711469, -1.540613122784354916, -0.9793164655157863274 ) ) ;
#69286 = CARTESIAN_POINT ( 'NONE',  ( -5.111587607552082524, 5.922272616020886282, 1.199719254218450271 ) ) ;
#69287 =( GEOMETRIC_REPRESENTATION_CONTEXT ( 3 ) GLOBAL_UNCERTAINTY_ASSIGNED_CONTEXT ( ( #147905 ) ) GLOBAL_UNIT_ASSIGNED_CONTEXT ( ( #51279, #2486, #165019 ) ) REPRESENTATION_CONTEXT ( 'NONE', 'WORKASPACE' ) );
#69288 = CARTESIAN_POINT ( 'NONE',  ( 3.041388834704723099, -1.310848641452688979, 1.135385315042459542 ) ) ;
#69289 = CARTESIAN_POINT ( 'NONE',  ( 0.6124999999999932720, 1.979166667349464781, -1.060881119635938008 ) ) ;
#69290 = CARTESIAN_POINT ( 'NONE',  ( 7.654042494670958593E-16, 0.9200000000000041478, -6.250000000000000000 ) ) ;
#69291 = CARTESIAN_POINT ( 'NONE',  ( 6.938893903907228378E-15, 10.64264068711930733, 1.214306433183764966E-14 ) ) ;
#69292 = CARTESIAN_POINT ( 'NONE',  ( 5.127504350819418910, -1.732488751877172772, 0.5760870007271366999 ) ) ;
#69293 = CARTESIAN_POINT ( 'NONE',  ( 3.573055779259231457, 1.771592698278463107, 0.8429337356923997104 ) ) ;
#69294 = CARTESIAN_POINT ( 'NONE',  ( -1.225000000000000089, -0.1666666659838688114, 0.7072540797572937077 ) ) ;
#69295 = CARTESIAN_POINT ( 'NONE',  ( -9.840520565420403543, 10.37502883594562597, 1.040834085586084257E-14 ) ) ;
#69296 = CARTESIAN_POINT ( 'NONE',  ( 7.962716289927667113, 8.184257181204083409, -0.7998128361456291469 ) ) ;
#69297 = CARTESIAN_POINT ( 'NONE',  ( 4.951869195850400196, -1.499954228463634465, -1.499123153458590929 ) ) ;
#69298 = CARTESIAN_POINT ( 'NONE',  ( 7.452141709366786770, 8.723195411463290583, 1.199719254218452047 ) ) ;
#69299 = CARTESIAN_POINT ( 'NONE',  ( -7.960608749518247151, 12.43912730774665576, 0.000000000000000000 ) ) ;
#69300 = CARTESIAN_POINT ( 'NONE',  ( 2.782155020660907141, -1.188329515115684076, -1.695063343828225877 ) ) ;
#69302 = CARTESIAN_POINT ( 'NONE',  ( 0.6823417656249882723, -0.3447916663252489911, 1.181850606188755259 ) ) ;
#69301 = CARTESIAN_POINT ( 'NONE',  ( -11.88237264505823987, 11.25677038468317015, 0.9087825512662228711 ) ) ;
#69303 = ORIENTED_EDGE ( 'NONE', *, *, #62099, .T. ) ;
#69305 = ORIENTED_EDGE ( 'NONE', *, *, #198010, .F. ) ;
#69304 = CARTESIAN_POINT ( 'NONE',  ( 4.371885135981863790, 0.4866971690204218159, -2.167184880714991824 ) ) ;
#69306 = CARTESIAN_POINT ( 'NONE',  ( 2.356409458221408126, 0.1091249688820790792, -2.296199191736052025 ) ) ;
#69307 = CARTESIAN_POINT ( 'NONE',  ( 7.944714827928039291, 11.25228915168265864, 1.082531754730557072 ) ) ;
#69309 = CARTESIAN_POINT ( 'NONE',  ( -1.642778471874998480, -2.501041666188707158, 2.845375778867863303 ) ) ;
#69308 = CARTESIAN_POINT ( 'NONE',  ( 6.617788377246179188, 8.814115421577600529, -1.443375672974078761 ) ) ;
#69310 = DIRECTION ( 'NONE',  ( 0.000000000000000000, 0.000000000000000000, 1.000000000000000000 ) ) ;
#69311 = CARTESIAN_POINT ( 'NONE',  ( -9.758911886679570102, 3.481540744127374243, 6.987834039733272107 ) ) ;
#69312 = VERTEX_POINT ( 'NONE', #102051 ) ;
#69313 = CARTESIAN_POINT ( 'NONE',  ( -5.223082171297989432E-15, -6.148216694138040950, 10.67870335800436798 ) ) ;
#69314 = CARTESIAN_POINT ( 'NONE',  ( 3.111475685156277038, 1.510342251817019532, 1.173009309769344588 ) ) ;
#69315 = DIRECTION ( 'NONE',  ( -0.6483454320283799088, 0.000000000000000000, 0.7613463080411786432 ) ) ;
#69316 = CARTESIAN_POINT ( 'NONE',  ( 4.524228514566789983, 1.059873738895898310, -1.360581713153318884 ) ) ;
#69317 = CARTESIAN_POINT ( 'NONE',  ( 2.923064838257955156, -1.776166165677966591, 0.9548571111624851726 ) ) ;
#69318 = CARTESIAN_POINT ( 'NONE',  ( 4.535913861531776448, -1.846855032230051208, 1.368429651993019025 ) ) ;
#69319 = CARTESIAN_POINT ( 'NONE',  ( -11.33772463945043540, 12.69999999999999041, -3.600000000000078693 ) ) ;
#69320 = CARTESIAN_POINT ( 'NONE',  ( 6.287733905706966553, 1.451067878312240822, 1.526644127000365003 ) ) ;
#69321 = CARTESIAN_POINT ( 'NONE',  ( -6.129694847154231852, 6.323934541200937787, -0.7216878364870338292 ) ) ;
#69322 = ORIENTED_EDGE ( 'NONE', *, *, #121638, .F. ) ;
#69323 = CARTESIAN_POINT ( 'NONE',  ( 5.272599804957129876, -1.666481374185318609, -0.5959551625853221068 ) ) ;
#69325 = CARTESIAN_POINT ( 'NONE',  ( 1.359778343217881602, 2.257671611795939004, -0.3959128255837316979 ) ) ;
#69324 = CARTESIAN_POINT ( 'NONE',  ( 7.686546744304875389, 7.932335721302671949, 0.7998128361456291469 ) ) ;
#69326 = CARTESIAN_POINT ( 'NONE',  ( 0.4271921415617612183, 0.8987490902026186168, -1.490136572063437637 ) ) ;
#69327 = CARTESIAN_POINT ( 'NONE',  ( -6.851666526859749418, 9.086973262793417661, -1.599625672291271394 ) ) ;
#69328 = CARTESIAN_POINT ( 'NONE',  ( 6.509741685903361663, -1.029359178063901092, -1.934661654277470166 ) ) ;
#69329 = CARTESIAN_POINT ( 'NONE',  ( -3.923105346307911745, 5.670318552149568703, -1.599625672291283607 ) ) ;
#69330 = CARTESIAN_POINT ( 'NONE',  ( -4.757329562667670667E-14, -0.8906249996585621220, -1.570758158831818241 ) ) ;
#69331 = CARTESIAN_POINT ( 'NONE',  ( 0.000000000000000000, 13.79999999999999893, 0.000000000000000000 ) ) ;
#69332 = CARTESIAN_POINT ( 'NONE',  ( 0.3621003815536598669, -0.5783089063249653439, 2.092656953901766315 ) ) ;
#69333 = CARTESIAN_POINT ( 'NONE',  ( 1.042204282965590201, 0.8216761606248854655, 1.841732292558920570 ) ) ;
#69334 = CARTESIAN_POINT ( 'NONE',  ( -1.402160292154681736E-14, -1.256249999317182953, 1.732050807568877637 ) ) ;
#69335 = CARTESIAN_POINT ( 'NONE',  ( 5.320897925068237555, 1.780805307305334040, 0.7354040419824976471 ) ) ;
#69336 = CARTESIAN_POINT ( 'NONE',  ( 1.364683531249997417, 11.98437500034139980, 2.602085213965210642E-15 ) ) ;
#69337 = CARTESIAN_POINT ( 'NONE',  ( 1.301376502765494658, -0.3325571857498362260, -2.196291469625763160 ) ) ;
#69339 = ORIENTED_EDGE ( 'NONE', *, *, #168924, .F. ) ;
#69338 = CARTESIAN_POINT ( 'NONE',  ( 10.05353459973327368, 11.68787744023238417, -1.199719254218440723 ) ) ;
#69341 = CARTESIAN_POINT ( 'NONE',  ( -1.123270288250339366, 3.283552654332833054, 0.7749999999993804067 ) ) ;
#69340 = CARTESIAN_POINT ( 'NONE',  ( 0.000000000000000000, 1.000000000000000888, 0.000000000000000000 ) ) ;
#69342 = CARTESIAN_POINT ( 'NONE',  ( -4.733205024502264102, 7.575804057677677505, 1.082531754730549967 ) ) ;
#69343 = CARTESIAN_POINT ( 'NONE',  ( 8.890396042259068210, 11.39521468743417998, -1.599625672291257406 ) ) ;
#69344 = LINE ( 'NONE', #135455, #163418 ) ;
#69345 = CARTESIAN_POINT ( 'NONE',  ( 3.846074041338778393, 7.345424771109255957, -0.6475569374996810179 ) ) ;
#69346 = CARTESIAN_POINT ( 'NONE',  ( 4.124340800031966126, 0.09048578169197672716, 1.738227929847275588 ) ) ;
#69347 = CARTESIAN_POINT ( 'NONE',  ( 2.242563829109287088, -1.923402688547710904, -0.3857071251459272543 ) ) ;
#69349 = CARTESIAN_POINT ( 'NONE',  ( 1.364683531249986537, 2.467708333674753174, -0.7879004041258239610 ) ) ;
#69348 = CARTESIAN_POINT ( 'NONE',  ( 2.998324526916512411, 6.649795714711241423, 0.000000000000000000 ) ) ;
#69350 = EDGE_CURVE ( 'NONE', #207685, #63797, #177653, .T. ) ;
#69351 = CARTESIAN_POINT ( 'NONE',  ( -5.897748123441601820, 6.008673066555767051, -0.2037434952626964724 ) ) ;
#69352 = CARTESIAN_POINT ( 'NONE',  ( 0.000000000000000000, 7.250000000000006217, -8.500000000000000000 ) ) ;
#69353 = CARTESIAN_POINT ( 'NONE',  ( 6.777797683793751915, -1.903277019102869616, 0.4755351429900215310 ) ) ;
#69354 = CARTESIAN_POINT ( 'NONE',  ( -8.993135964566285168, 9.386413468282476913, -0.7998128361456291469 ) ) ;
#69355 =( BOUNDED_CURVE ( )  B_SPLINE_CURVE ( 2, ( #14944, #29098, #114675, #111477, #180667, #208887, #60518 ),
 .UNSPECIFIED., .F., .T. ) 
 B_SPLINE_CURVE_WITH_KNOTS ( ( 3, 2, 2, 3 ),
 ( 0.2375000000000004052, 0.2416666666666670293, 0.2458333333333336534, 0.2500000000000002776 ),
 .UNSPECIFIED. ) 
 CURVE ( )  GEOMETRIC_REPRESENTATION_ITEM ( )  RATIONAL_B_SPLINE_CURVE ( ( 0.9999999999999865663, 0.8660254037844521413, 1.000000000000000000, 0.8660254037844387076, 1.000000000000000000, 0.8660254037844298258, 1.000000000000008882 ) ) 
 REPRESENTATION_ITEM ( '' )  );
#69356 = CARTESIAN_POINT ( 'NONE',  ( -5.395781948114519722, 5.397426482329451325, 0.000000000000000000 ) ) ;
#69357 = CARTESIAN_POINT ( 'NONE',  ( 5.137907791644652278, 2.014008302827663854, -0.1037760698975112861 ) ) ;
#69358 = CARTESIAN_POINT ( 'NONE',  ( 1.112636518468415270, -1.019398372879092962, -2.019907345245135932 ) ) ;
#69360 = ORIENTED_EDGE ( 'NONE', *, *, #107456, .F. ) ;
#69359 = CARTESIAN_POINT ( 'NONE',  ( -6.742482464697739708, 6.760651051769146491, 0.7998128361456341429 ) ) ;
#69361 = CARTESIAN_POINT ( 'NONE',  ( 1.499999999999989120, 0.5562500006828161592, 0.000000000000000000 ) ) ;
#69362 = CARTESIAN_POINT ( 'NONE',  ( 1.510794437334112672, 1.647127454408814362, 0.8865631655482277829 ) ) ;
#69363 = CARTESIAN_POINT ( 'NONE',  ( 0.6856605700745866949, 1.416429869936095542, 1.000165270844357801 ) ) ;
#69364 = CARTESIAN_POINT ( 'NONE',  ( 4.564136437409766600, -1.431273618155091576, 1.659743667367798103 ) ) ;
#69365 = CARTESIAN_POINT ( 'NONE',  ( 5.087122877145462851, -0.2765918260761930925, -2.290891016797763413 ) ) ;
#69366 = CARTESIAN_POINT ( 'NONE',  ( 0.8485939591743509869, 0.5976917523492016882, 1.972322469454860672 ) ) ;
#69367 = CARTESIAN_POINT ( 'NONE',  ( 3.292849172082324305, 1.531446531863265736, 1.193990500783614905 ) ) ;
#69368 = CARTESIAN_POINT ( 'NONE',  ( -4.080641047588914994, 5.783833860318930320, -1.443375672974051449 ) ) ;
#69369 = ADVANCED_FACE ( 'NONE', ( #20769 ), #152930, .T. ) ;
#69370 = CARTESIAN_POINT ( 'NONE',  ( 5.448468942325162878, 0.5420331153751513087, 1.790312535500695024 ) ) ;
#69371 = CARTESIAN_POINT ( 'NONE',  ( 3.994299746785815231, 7.604083813490793098, 0.004591788735710394809 ) ) ;
#69372 = CARTESIAN_POINT ( 'NONE',  ( 0.3855818064394588851, -0.09363725165581829324, 1.731465614217362559 ) ) ;
#69373 = CARTESIAN_POINT ( 'NONE',  ( 3.594320121398666856, 7.207474218358159490, -1.734723475976807094E-15 ) ) ;
#69374 = CARTESIAN_POINT ( 'NONE',  ( 1.360316468749955598, 1.536458333674721288, -0.7853790794159342115 ) ) ;
#69375 = CARTESIAN_POINT ( 'NONE',  ( 5.098279808040273586, -0.2930726886911338425, 1.994869512123042199 ) ) ;
#69376 = CARTESIAN_POINT ( 'NONE',  ( -3.429849674132942727, 5.984946472254969230, -1.082531754730549078 ) ) ;
#69377 = CARTESIAN_POINT ( 'NONE',  ( 9.596473800374404561, 10.09030761005864285, 0.000000000000000000 ) ) ;
#69379 = CARTESIAN_POINT ( 'NONE',  ( -7.015831072854292749, -6.604036961759870650, 6.576431128232877121 ) ) ;
#69378 = CARTESIAN_POINT ( 'NONE',  ( 2.033574986395149775, -1.191784744093337123, -1.383114941912518159 ) ) ;
#69380 = CARTESIAN_POINT ( 'NONE',  ( -5.147255595043616516, 6.034161611419515125, 1.199719254218452935 ) ) ;
#69381 = CARTESIAN_POINT ( 'NONE',  ( -8.673617379884035472E-15, -6.268611901546719878, -10.55819884875826453 ) ) ;
#69382 = CARTESIAN_POINT ( 'NONE',  ( -10.49071307728992153, 3.038037579769635066, 7.129592439487457689 ) ) ;
#69383 = VERTEX_POINT ( 'NONE', #59690 ) ;
#69384 = CARTESIAN_POINT ( 'NONE',  ( -4.923019175093582334, 8.757623114335565617, 0.7216878364870267237 ) ) ;
#69385 = CARTESIAN_POINT ( 'NONE',  ( -4.451154503988200339, 4.087435097607984957, 1.214306433183764966E-14 ) ) ;
#69386 = CARTESIAN_POINT ( 'NONE',  ( -10.14557902172788495, 10.73093036830436553, 1.040834085586084257E-14 ) ) ;
#69387 = CARTESIAN_POINT ( 'NONE',  ( 6.059241617823571957, -1.705078594313869988, 1.082191098076368929 ) ) ;
#69389 = ORIENTED_EDGE ( 'NONE', *, *, #6353, .F. ) ;
#69388 = CARTESIAN_POINT ( 'NONE',  ( 0.03014954708456181465, -2.078685333231004684, 0.4181070283913386199 ) ) ;
#69390 = CARTESIAN_POINT ( 'NONE',  ( -7.435720902452096936, 7.639705572474380091, 0.000000000000000000 ) ) ;
#69391 = CARTESIAN_POINT ( 'NONE',  ( 4.924636110261782385, 6.768494766770632332, 1.599625672291267398 ) ) ;
#69392 =( GEOMETRIC_REPRESENTATION_CONTEXT ( 3 ) GLOBAL_UNCERTAINTY_ASSIGNED_CONTEXT ( ( #26803 ) ) GLOBAL_UNIT_ASSIGNED_CONTEXT ( ( #181442, #16792, #53579 ) ) REPRESENTATION_CONTEXT ( 'NONE', 'WORKASPACE' ) );
#69393 = CARTESIAN_POINT ( 'NONE',  ( 4.926665654204026801, 1.971471998011574467, 0.6004258549221918040 ) ) ;
#69394 = CARTESIAN_POINT ( 'NONE',  ( 5.414685466650038137, -1.281359335986744341, -1.556910257834144051 ) ) ;
#69395 = ORIENTED_EDGE ( 'NONE', *, *, #63218, .T. ) ;
#69396 = ORIENTED_EDGE ( 'NONE', *, *, #197437, .T. ) ;
#69397 = CARTESIAN_POINT ( 'NONE',  ( 4.766981195426724938, 4.885374124022287212, -0.7701443108643934998 ) ) ;
#69398 = CARTESIAN_POINT ( 'NONE',  ( -1.886825320689270225, 2.480000000000016858, 2.459652456995881753 ) ) ;
#69400 = VERTEX_POINT ( 'NONE', #158282 ) ;
#69399 = CARTESIAN_POINT ( 'NONE',  ( -5.926849427829407269, 6.943687749669614995, -1.199719254218453823 ) ) ;
#69401 = CARTESIAN_POINT ( 'NONE',  ( 4.641544345285703699, 8.432478572106539616, -0.4375188090333537727 ) ) ;
#69402 = CARTESIAN_POINT ( 'NONE',  ( 4.886092203009785528, -0.1017338195800701617, 2.013677658187912556 ) ) ;
#69403 = CARTESIAN_POINT ( 'NONE',  ( 3.802549092506895878, 1.579937072410386278, 0.9450539169142122553 ) ) ;
#69404 = EDGE_CURVE ( 'NONE', #170914, #40241, #90349, .T. ) ;
#69405 = CARTESIAN_POINT ( 'NONE',  ( -0.8145602173408781344, -4.140925090156072130, -0.5891403177412749548 ) ) ;
#69406 = CARTESIAN_POINT ( 'NONE',  ( 1.700300771062040361, -0.7742048122164610913, 2.174079040713126076 ) ) ;
#69407 = CARTESIAN_POINT ( 'NONE',  ( 7.126746022638799971, 8.343567110280638133, 1.199719254218452047 ) ) ;
#69408 = CARTESIAN_POINT ( 'NONE',  ( 4.429101881081805914, 0.1011787780425543737, 2.159334005894457231 ) ) ;
#69409 = CARTESIAN_POINT ( 'NONE',  ( 7.771848369131631351, 10.09024240211882351, -1.599625672291262513 ) ) ;
#69410 = CARTESIAN_POINT ( 'NONE',  ( 0.04629046987890492182, -1.559278246393133838, 1.157480633202745635 ) ) ;
#69411 = CARTESIAN_POINT ( 'NONE',  ( -5.759516327706961647, 5.613857225279885732, -0.7998128361456221525 ) ) ;
#69412 = COLOUR_RGB ( '', 0.66274510, 0.83137255, 0.94901961) ;
#69413 = CARTESIAN_POINT ( 'NONE',  ( 4.007374829128952598, 2.286843722993581185, 0.2302655642077624243 ) ) ;
#69414 = CARTESIAN_POINT ( 'NONE',  ( -9.523390464577085268, 15.37761368573234044, -7.301111590705639642 ) ) ;
#69415 = CARTESIAN_POINT ( 'NONE',  ( 3.502682687546424312, 1.475339254275360279, -1.149998991230333223 ) ) ;
#69416 = CARTESIAN_POINT ( 'NONE',  ( 0.1808907491311480820, -0.1332662104699660066, -1.940345832946618554 ) ) ;
#69419 = ADVANCED_FACE ( 'NONE', ( #125853 ), #177705, .T. ) ;
#69418 = CARTESIAN_POINT ( 'NONE',  ( -7.262327558775498737, 8.501745569106741840, 1.199719254218452047 ) ) ;
#69417 = CARTESIAN_POINT ( 'NONE',  ( -1.500000000000015099, -1.297916665983847029, 0.8660254037844403729 ) ) ;
#69420 = CARTESIAN_POINT ( 'NONE',  ( 2.245003380770736801, 0.4850519687749441644, 2.152760086278446394 ) ) ;
#69421 = ORIENTED_EDGE ( 'NONE', *, *, #181457, .T. ) ;
#69422 = CARTESIAN_POINT ( 'NONE',  ( 6.620655732516651071, -0.002413161512292844035, 2.173887093218453082 ) ) ;
#69423 = CARTESIAN_POINT ( 'NONE',  ( 3.018661757337009810, 6.673522483535157868, 0.000000000000000000 ) ) ;
#69424 = CARTESIAN_POINT ( 'NONE',  ( -3.262708522383007903, 6.958243709422141876, 1.040834085586084257E-14 ) ) ;
#69425 = CARTESIAN_POINT ( 'NONE',  ( 3.511198596259283544, 6.271927390929313617, -2.420000000000000373 ) ) ;
#69426 = CARTESIAN_POINT ( 'NONE',  ( 1.053909416342192484, 1.969286043147522980, -0.09259992539933233069 ) ) ;
#69427 = ADVANCED_FACE ( 'NONE', ( #142050 ), #105270, .T. ) ;
#69428 = CARTESIAN_POINT ( 'NONE',  ( 0.5171989335802311682, 1.588149187230869952, -1.674348222103681172 ) ) ;
#69429 = CARTESIAN_POINT ( 'NONE',  ( 0.6077679335219284829, 0.6189715888181289705, -1.861716921216026055 ) ) ;
#69430 = CARTESIAN_POINT ( 'NONE',  ( 3.871981579112850458, -2.032873796296597479, 0.3478246332576060973 ) ) ;
#69431 = CARTESIAN_POINT ( 'NONE',  ( 6.019457014787495730, 6.125047393447951016, -0.7216878364870257245 ) ) ;
#69432 = CARTESIAN_POINT ( 'NONE',  ( 6.424584688029230328, 8.588711117491191871, 1.599625672291268286 ) ) ;
#69433 = ORIENTED_EDGE ( 'NONE', *, *, #21052, .T. ) ;
#69434 = CARTESIAN_POINT ( 'NONE',  ( 8.229436053370683624, 8.703356271795033905, 0.7216878364870458196 ) ) ;
#69435 = CARTESIAN_POINT ( 'NONE',  ( -1.364683531250012516, 4.301041667008089320, -0.7879004041258300672 ) ) ;
#69436 = CARTESIAN_POINT ( 'NONE',  ( 5.788968402910816380, 5.856144012925152076, 0.7216878364870317197 ) ) ;
#69437 = CARTESIAN_POINT ( 'NONE',  ( 6.760228240101231023, -2.170840268647770799, 0.04637219581851703687 ) ) ;
#69439 = CARTESIAN_POINT ( 'NONE',  ( 5.267088776126935379, 1.772936381825638952, -0.4966186330585887210 ) ) ;
#69438 = CARTESIAN_POINT ( 'NONE',  ( 9.497898427948536337, -9.431315562283165477, -0.2398643602167310762 ) ) ;
#69441 = CARTESIAN_POINT ( 'NONE',  ( -11.88172094500852971, 12.22000005601549688, -1.685553348215899083 ) ) ;
#69440 = B_SPLINE_CURVE_WITH_KNOTS ( 'NONE', 3,
 ( #51714, #64738, #1849, #84192, #150279, #32248 ),
 .UNSPECIFIED., .F., .F.,
 ( 4, 2, 4 ),
 ( 0.000000000000000000, 0.0003155923098472858596, 0.0006311846196945720446 ),
 .UNSPECIFIED. ) ;
#69442 = CARTESIAN_POINT ( 'NONE',  ( -4.503925953283787642, 7.237052973511334919, 1.308369160636771333 ) ) ;
#69443 = DIRECTION ( 'NONE',  ( 0.000000000000000000, 1.000000000000000000, 0.000000000000000000 ) ) ;
#69444 = CARTESIAN_POINT ( 'NONE',  ( 6.212391540903618115, 7.031971956796816414, -1.022972206104319826 ) ) ;
#69445 = CARTESIAN_POINT ( 'NONE',  ( -1.364683531250010295, 5.592708333674750953, 0.7879004041258379498 ) ) ;
#69446 = CARTESIAN_POINT ( 'NONE',  ( 0.9086806230526077721, -0.4651930584498394916, -1.854694524013176693 ) ) ;
#69447 =( BOUNDED_CURVE ( )  B_SPLINE_CURVE ( 2, ( #163227, #34265, #51603, #117728, #151238, #64644, #183717 ),
 .UNSPECIFIED., .F., .T. ) 
 B_SPLINE_CURVE_WITH_KNOTS ( ( 3, 2, 2, 3 ),
 ( 0.1785714285714287142, 0.1845238095238095899, 0.1904761904761904656, 0.1964285714285713413 ),
 .UNSPECIFIED. ) 
 CURVE ( )  GEOMETRIC_REPRESENTATION_ITEM ( )  RATIONAL_B_SPLINE_CURVE ( ( 0.9999999999999968914, 0.8660254037844418162, 1.000000000000000000, 0.8660254037844387076, 1.000000000000000000, 0.8660254037844405950, 0.9999999999999981126 ) ) 
 REPRESENTATION_ITEM ( '' )  );
#69448 =( GEOMETRIC_REPRESENTATION_CONTEXT ( 3 ) GLOBAL_UNCERTAINTY_ASSIGNED_CONTEXT ( ( #67662 ) ) GLOBAL_UNIT_ASSIGNED_CONTEXT ( ( #86424, #70142, #158893 ) ) REPRESENTATION_CONTEXT ( 'NONE', 'WORKASPACE' ) );
#69449 = CARTESIAN_POINT ( 'NONE',  ( 3.572906242625200068, 0.04398576871290219709, -1.769473305487194281 ) ) ;
#69450 = CARTESIAN_POINT ( 'NONE',  ( 5.918613486546395741, -0.7266362437793117968, -1.877539736040201079 ) ) ;
#69452 = CARTESIAN_POINT ( 'NONE',  ( 4.675340500466128368, 1.422229311605049507, 1.283493733622777189 ) ) ;
#69451 = CARTESIAN_POINT ( 'NONE',  ( -8.130085669689073313, 12.63685038127928806, 0.7998128361456481317 ) ) ;
#69453 = AXIS2_PLACEMENT_3D ( 'NONE', #142230, #15103, #156326 ) ;
#69454 = CARTESIAN_POINT ( 'NONE',  ( -2.974698719455045381, 6.690899969729074748, -0.05384663926280564006 ) ) ;
#69455 = CARTESIAN_POINT ( 'NONE',  ( 5.353942763280384654, -0.7107094859252837127, 1.837027094894280399 ) ) ;
#69456 = CARTESIAN_POINT ( 'NONE',  ( 1.037531286769650452, -0.04638328994046451298, 2.120250110247793085 ) ) ;
#69457 = CARTESIAN_POINT ( 'NONE',  ( -1.452583904633382383, -1.374772708486751593, 1.500000000000001332 ) ) ;
#69458 = CARTESIAN_POINT ( 'NONE',  ( 3.906994808788874174, 1.604092888448312326, 0.9621832354540849064 ) ) ;
#69460 = ORIENTED_EDGE ( 'NONE', *, *, #193595, .F. ) ;
#69459 = CARTESIAN_POINT ( 'NONE',  ( 6.498688201949993193, -0.4681372660274349951, -1.660085793416385513 ) ) ;
#69462 = CARTESIAN_POINT ( 'NONE',  ( 3.795919822146273326, 5.451659097302528068, -1.443375672974051449 ) ) ;
#69461 = CARTESIAN_POINT ( 'NONE',  ( 3.826972293661185187, 2.095320012007126476, 0.6930106488920934060 ) ) ;
#69463 = CARTESIAN_POINT ( 'NONE',  ( -1.201851678989727383E-14, 4.134375000341417028, 1.575800808251672791 ) ) ;
#69464 = CARTESIAN_POINT ( 'NONE',  ( 1.117717378214663881, 0.4042816502292169711, -2.022510655824232728 ) ) ;
#69465 = CARTESIAN_POINT ( 'NONE',  ( 8.125414133291656071, 8.374071331795406081, -0.7998128361456291469 ) ) ;
#69466 = CARTESIAN_POINT ( 'NONE',  ( -9.840520565420403543, 10.37502883594562597, 1.040834085586084257E-14 ) ) ;
#69467 = CARTESIAN_POINT ( 'NONE',  ( -8.846456096353129794, 0.9706168436483477713, -7.965384846859585366 ) ) ;
#69468 = CARTESIAN_POINT ( 'NONE',  ( -4.928552533767591726, 5.708731696605642725, 1.199719254218462483 ) ) ;
#69469 = DIRECTION ( 'NONE',  ( -7.387867266669436732E-31, 1.000000000000000000, 8.546850786086424434E-32 ) ) ;
#69470 = EDGE_LOOP ( 'NONE', ( #205022, #115670, #13319 ) ) ;
#69471 = CARTESIAN_POINT ( 'NONE',  ( 3.350112325975619587, -0.8415805752714689003, 1.891790567983504312 ) ) ;
#69472 = CARTESIAN_POINT ( 'NONE',  ( -0.7499999999999972244, 4.858333333333353821, -1.299038105676652011 ) ) ;
#69473 = CARTESIAN_POINT ( 'NONE',  ( 3.472859903394816872, 7.203420320602605287, -0.7998128361456291469 ) ) ;
#69474 = CARTESIAN_POINT ( 'NONE',  ( -6.600870636098118638, 6.767368133241304484, -0.2259646751960984468 ) ) ;
#69475 = CARTESIAN_POINT ( 'NONE',  ( 0.9967468350138152244, -1.970926226424707606, -0.4403189329902043037 ) ) ;
#69476 = FACE_OUTER_BOUND ( 'NONE', #179566, .T. ) ;
#69478 = CARTESIAN_POINT ( 'NONE',  ( 8.432808358020025707, 9.900993174853955026, 1.082531754730558626 ) ) ;
#69477 = CARTESIAN_POINT ( 'NONE',  ( 0.07499057489264347731, 6.948553613792602057, -2.550573651218261517 ) ) ;
#69479 = CARTESIAN_POINT ( 'NONE',  ( 6.204453847213379447, -1.458334814074750740, -1.392330997281837623 ) ) ;
#69480 = CARTESIAN_POINT ( 'NONE',  ( 6.350803879971770982, -1.754615558991738267, -0.7693843322766678039 ) ) ;
#69481 = CARTESIAN_POINT ( 'NONE',  ( 6.639320575229257670, 1.230867875982581738, 2.315960674347458781 ) ) ;
#69482 = CARTESIAN_POINT ( 'NONE',  ( 4.001666433686186686, -2.185622478633037602, 0.1623105178310546570 ) ) ;
#69483 = CARTESIAN_POINT ( 'NONE',  ( 0.7499999999999902300, 2.764583334016148974, 1.299038105676669330 ) ) ;
#69484 = CARTESIAN_POINT ( 'NONE',  ( 3.375170810042011915, -1.688748480992762868, -0.8973671847329609541 ) ) ;
#69485 = CARTESIAN_POINT ( 'NONE',  ( -3.903858165731105778, 6.641919395739846799, 1.199719254218464037 ) ) ;
#69486 = CARTESIAN_POINT ( 'NONE',  ( 5.165293336682183600, 5.128523102325077687, -0.7216878364870197293 ) ) ;
#69488 = CARTESIAN_POINT ( 'NONE',  ( 1.353138909097661768, 0.1455122274086443901, -2.011206940682720212 ) ) ;
#69487 = CARTESIAN_POINT ( 'NONE',  ( 3.556032804726692920, 7.337844839197152247, -0.2427830827038110206 ) ) ;
#69490 = EDGE_CURVE ( 'NONE', #161364, #66472, #84156, .T. ) ;
#69489 = CARTESIAN_POINT ( 'NONE',  ( -8.012344526598182026E-15, 10.85937500034139624, -1.575800808251669460 ) ) ;
#69492 = CARTESIAN_POINT ( 'NONE',  ( -4.899292406491858820, 6.809203455697518947, -1.599625672291271394 ) ) ;
#69491 = CARTESIAN_POINT ( 'NONE',  ( -0.1230140872038130023, -0.1644519934839226150, -2.256176000670232717 ) ) ;
#69494 = ORIENTED_EDGE ( 'NONE', *, *, #160909, .F. ) ;
#69493 = CARTESIAN_POINT ( 'NONE',  ( 2.590480338954644246, -0.2921314510030656453, -1.699667543312991747 ) ) ;
#69495 = CARTESIAN_POINT ( 'NONE',  ( 0.1394461523057137220, 5.725876337386284654, -2.313825101289856967 ) ) ;
#69496 = CARTESIAN_POINT ( 'NONE',  ( 7.609150525767641504, 9.900428251527500834, -1.599625672291262513 ) ) ;
#69497 = CARTESIAN_POINT ( 'NONE',  ( 5.996784015946103885, 5.890669528225568996, 1.040834085586084257E-14 ) ) ;
#69498 = CARTESIAN_POINT ( 'NONE',  ( 1.530808498934191324E-16, -0.5000000000000004441, -1.249999999999999778 ) ) ;
#69499 = CARTESIAN_POINT ( 'NONE',  ( 1.363640982571033611, -0.4799814350611387725, 1.902108589862220311 ) ) ;
#69500 = LINE ( 'NONE', #34873, #105461 ) ;
#69501 = CARTESIAN_POINT ( 'NONE',  ( 5.678167406024951624, 5.518950149984223508, 0.7998128361456341429 ) ) ;
#69502 = CARTESIAN_POINT ( 'NONE',  ( 0.07556134207192373442, 6.947017789483680872, -2.839293120204011256 ) ) ;
#69503 = ORIENTED_EDGE ( 'NONE', *, *, #100213, .F. ) ;
#69504 = CARTESIAN_POINT ( 'NONE',  ( 0.000000000000000000, 0.000000000000000000, 0.000000000000000000 ) ) ;
#69505 = ORIENTED_EDGE ( 'NONE', *, *, #206116, .T. ) ;
#69506 = CARTESIAN_POINT ( 'NONE',  ( 3.650846288169238729, 0.2690317868887618369, 1.791254203397556477 ) ) ;
#69507 = VERTEX_POINT ( 'NONE', #155071 ) ;
#69508 = CARTESIAN_POINT ( 'NONE',  ( -5.346851039111045978, 6.199209027673974859, 1.173132900504408438 ) ) ;
#69509 = CARTESIAN_POINT ( 'NONE',  ( 4.828658830049068484, 1.245459390374216380, -1.315641719143684885 ) ) ;
#69510 = DIRECTION ( 'NONE',  ( -2.664535259100375697E-15, 0.000000000000000000, 1.000000000000000000 ) ) ;
#69511 = CARTESIAN_POINT ( 'NONE',  ( -6.594971851908696614, -6.631671897293978546, -6.818239719371401719 ) ) ;
#69512 = CARTESIAN_POINT ( 'NONE',  ( 5.859090863903361424, 5.997168572722006097, -0.3086645125121977862 ) ) ;
#69514 = CARTESIAN_POINT ( 'NONE',  ( 10.71502147350184231, 11.39527989537399755, 0.000000000000000000 ) ) ;
#69513 = CARTESIAN_POINT ( 'NONE',  ( 4.738624546071780408, -1.804922690063763824, -0.4530168641722984169 ) ) ;
#69515 = EDGE_CURVE ( 'NONE', #149864, #195844, #118996, .T. ) ;
#69516 = CARTESIAN_POINT ( 'NONE',  ( 2.970226572681373689, -1.887729772399210804, -0.3245638568863758455 ) ) ;
#69517 = CARTESIAN_POINT ( 'NONE',  ( 5.736508392357904107, 5.865217010605237924, 0.000000000000000000 ) ) ;
#69518 = CARTESIAN_POINT ( 'NONE',  ( -11.97594889418004804, 7.449136658168690417, 0.9368335759953716479 ) ) ;
#69519 = CIRCLE ( 'NONE', #90278, 11.49999999999998934 ) ;
#69520 = CARTESIAN_POINT ( 'NONE',  ( 1.499999999999990896, 5.556250000682820378, 1.214306433183764966E-14 ) ) ;
#69521 = CARTESIAN_POINT ( 'NONE',  ( -1.364683531250000748, -0.9906249996585805295, 0.000000000000000000 ) ) ;
#69522 = CARTESIAN_POINT ( 'NONE',  ( 5.748293942514166588, 7.729428904398431222, -1.443375672974057666 ) ) ;
#69523 = CARTESIAN_POINT ( 'NONE',  ( -9.164948653157990677, 11.71552606681625619, -1.443375672974059665 ) ) ;
#69524 = CARTESIAN_POINT ( 'NONE',  ( 0.3741789627117291239, 1.245922373857488274, 1.766349570875298758 ) ) ;
#69525 = CARTESIAN_POINT ( 'NONE',  ( -5.562588163356775972, 9.711712967216715953, 0.7998128361456291469 ) ) ;
#69526 = CARTESIAN_POINT ( 'NONE',  ( 1.957086829145736173, 0.3561595965777020756, -2.059905414565963433 ) ) ;
#69527 = CARTESIAN_POINT ( 'NONE',  ( 4.342354338126830804, 8.288106837781779035, -0.7998128361456381397 ) ) ;
#69528 = CARTESIAN_POINT ( 'NONE',  ( 0.6569167496461197908, -1.539450689919025450, -0.9809549629347169564 ) ) ;
#69529 = CARTESIAN_POINT ( 'NONE',  ( -4.205000198532790279, 8.057583998263570635, 0.7998128361456341429 ) ) ;
#69530 = CARTESIAN_POINT ( 'NONE',  ( 2.520284954824199453, 1.194270260598716771, -1.380820861806408617 ) ) ;
#69531 = CARTESIAN_POINT ( 'NONE',  ( 9.691970092379245116, 13.38142374607198803, 8.152522038325429321 ) ) ;
#69532 = CARTESIAN_POINT ( 'NONE',  ( 2.214975196874233720, 1.533708969217022933, -1.142120075431733994 ) ) ;
#69533 = CARTESIAN_POINT ( 'NONE',  ( 2.365619736264668038, -0.4344343780767513374, 1.920862584678226348 ) ) ;
#69534 = CARTESIAN_POINT ( 'NONE',  ( 3.421366544187495418, -1.159031000169882475, -1.558129983894075865 ) ) ;
#69535 = CARTESIAN_POINT ( 'NONE',  ( -7.761116589180078407, 8.019333873657032541, 0.000000000000000000 ) ) ;
#69537 = CARTESIAN_POINT ( 'NONE',  ( 4.605793411009856619, 1.573235607984494688, 1.422142093439874522 ) ) ;
#69536 = CARTESIAN_POINT ( 'NONE',  ( 8.018721507839716267, 8.319872945426633137, -0.7998128361456341429 ) ) ;
#69538 = DIRECTION ( 'NONE',  ( 1.000000000000000000, 0.000000000000000000, 0.000000000000000000 ) ) ;
#69539 = CARTESIAN_POINT ( 'NONE',  ( 8.829384350997564468, 11.32403438096243775, 1.599625672291281386 ) ) ;
#69540 = CARTESIAN_POINT ( 'NONE',  ( 6.112872195911107198, 6.017013290715023111, -0.08730524813132384265 ) ) ;
#69541 = CARTESIAN_POINT ( 'NONE',  ( 0.000000000000000000, -3.600000000000005862, 0.000000000000000000 ) ) ;
#69542 = CIRCLE ( 'NONE', #266, 2.080000000000000071 ) ;
#69543 = CARTESIAN_POINT ( 'NONE',  ( 6.607619761813720238, 8.802252036906432764, 1.599625672291268286 ) ) ;
#69544 = CARTESIAN_POINT ( 'NONE',  ( 4.318856058802469811, 1.670182456744148336, 0.7377305746401884301 ) ) ;
#69545 = CARTESIAN_POINT ( 'NONE',  ( -8.514157279702020631, 11.91663867875229776, -1.082531754730543971 ) ) ;
#69546 = CARTESIAN_POINT ( 'NONE',  ( -5.621078624820424530, 7.474595091574217420, 1.344519841555512629 ) ) ;
#69547 = PLANE ( 'NONE',  #11995 ) ;
#69548 = CARTESIAN_POINT ( 'NONE',  ( 4.662891624058607576, -1.671085903211678270, -0.8408918736509605196 ) ) ;
#69549 = CARTESIAN_POINT ( 'NONE',  ( 8.613507663383630941, 8.943513783569379427, -0.7998128361456221525 ) ) ;
#69550 = CARTESIAN_POINT ( 'NONE',  ( 1.893070592381540740, 1.676246824859698892, -0.9494106994061870530 ) ) ;
#69551 = CARTESIAN_POINT ( 'NONE',  ( 6.842638302680405182, -1.923265442670134551, -0.3857968560932593660 ) ) ;
#69552 = MECHANICAL_DESIGN_GEOMETRIC_PRESENTATION_REPRESENTATION (  '', ( #111090 ), #28150 ) ;
#69553 = CARTESIAN_POINT ( 'NONE',  ( 3.354752944377597856, 6.001296637494123232, -1.199719254218446718 ) ) ;
#69554 = CARTESIAN_POINT ( 'NONE',  ( 1.364683531249997417, 9.296875000341403350, 2.602085213965210642E-15 ) ) ;
#69555 = CARTESIAN_POINT ( 'NONE',  ( -7.413611068574208041, 7.543634422958360730, 0.7998128361456341429 ) ) ;
#69556 = CARTESIAN_POINT ( 'NONE',  ( 2.835626683552519012, 6.459981564119914310, 0.000000000000000000 ) ) ;
#69557 = EDGE_CURVE ( 'NONE', #2638, #36822, #151308, .T. ) ;
#69558 = CARTESIAN_POINT ( 'NONE',  ( -4.299344108864961989, 6.109263775132799168, -1.443375672974066548 ) ) ;
#69559 = CARTESIAN_POINT ( 'NONE',  ( 1.212693198809017270, 2.041623912717607237, 0.5605823208302792571 ) ) ;
#69560 = CARTESIAN_POINT ( 'NONE',  ( -2.449742653233059286, 3.300000000000011369, 0.3999999999999750422 ) ) ;
#69561 = CARTESIAN_POINT ( 'NONE',  ( -2.734094378161644023, 2.930569811600738817, 2.453211638583631782 ) ) ;
#69562 = CARTESIAN_POINT ( 'NONE',  ( 6.473496638176248652, -0.2593738453590052617, 2.053908440964563376 ) ) ;
#69564 = CARTESIAN_POINT ( 'NONE',  ( 3.998447120444656555, 7.829958269474884602, 0.005269623924535754567 ) ) ;
#69563 = CARTESIAN_POINT ( 'NONE',  ( 0.06366010765614799061, -1.203631707120488947, 1.393476991864414760 ) ) ;
#69565 = CARTESIAN_POINT ( 'NONE',  ( 5.801499429514798578, 1.546190052965769057, -1.701143905309614679 ) ) ;
#69566 = CARTESIAN_POINT ( 'NONE',  ( 5.910991785878156435, 7.919243054989755670, -1.443375672974057666 ) ) ;
#69568 = CARTESIAN_POINT ( 'NONE',  ( 1.499999999999996891, 9.677083334016129967, -0.8660254037844378194 ) ) ;
#69567 = CARTESIAN_POINT ( 'NONE',  ( 4.746763178560261309, 5.670883475476017566, 1.082531754730549078 ) ) ;
#69569 = CARTESIAN_POINT ( 'NONE',  ( 1.482826411003408840, -0.3401602582979300626, -2.266773921731002339 ) ) ;
#69570 = CARTESIAN_POINT ( 'NONE',  ( -9.499984059629559496, -7.809931833644718324, -0.02724524595755116463 ) ) ;
#69571 = CARTESIAN_POINT ( 'NONE',  ( -6.798487682609798632, 6.896266815991691779, 0.7998128361456341429 ) ) ;
#69572 = CARTESIAN_POINT ( 'NONE',  ( 5.859312505936116189, 1.912822604199882148, -0.3342364482464658115 ) ) ;
#69573 = ORIENTED_EDGE ( 'NONE', *, *, #7569, .F. ) ;
#69574 = CARTESIAN_POINT ( 'NONE',  ( 7.415946836550703303, 11.59576237604377091, 0.7216878364870438212 ) ) ;
#69575 = CARTESIAN_POINT ( 'NONE',  ( 1.177990849177086075, 1.982702329297232113, -0.3483419944294365300 ) ) ;
#69576 = CARTESIAN_POINT ( 'NONE',  ( -9.001723924469462901, 12.58942944760136484, -1.199719254218446718 ) ) ;
#69578 = CARTESIAN_POINT ( 'NONE',  ( 0.000000000000000000, 13.49999999999999822, -1.500000000000000222 ) ) ;
#69577 = CARTESIAN_POINT ( 'NONE',  ( -8.097244055859620815, 10.46987070330147063, -1.599625672291263179 ) ) ;
#69579 = CARTESIAN_POINT ( 'NONE',  ( -10.19097401674926395, 4.476076320095182304, 5.708917106338025960 ) ) ;
#69581 = CARTESIAN_POINT ( 'NONE',  ( 1.059032582198644601, 0.3505281480379630610, -1.734596922625891713 ) ) ;
#69580 = CARTESIAN_POINT ( 'NONE',  ( 2.501997717985538383, -0.8009308590465279432, -1.931334861377894008 ) ) ;
#69582 = CARTESIAN_POINT ( 'NONE',  ( 6.504528880466823537, -1.955196382115764964, 0.4926337920100053447 ) ) ;
#69584 = CARTESIAN_POINT ( 'NONE',  ( 4.646573614920027850, -1.842837963294202464, 1.363044294324888162 ) ) ;
#69583 = DIRECTION ( 'NONE',  ( 1.000000000000000000, -5.578564026256490882E-16, -5.570868214615546318E-48 ) ) ;
#69585 = CARTESIAN_POINT ( 'NONE',  ( 3.116877616926060135, -1.676954032530679761, 0.4650628940853319682 ) ) ;
#69586 = EDGE_CURVE ( 'NONE', #187007, #88193, #46292, .T. ) ;
#69587 = CARTESIAN_POINT ( 'NONE',  ( 2.205172540517054802, 5.724451730578533848, 1.040834085586084257E-14 ) ) ;
#69588 = CARTESIAN_POINT ( 'NONE',  ( 3.620171223323872756, 0.4232754169638303643, -1.681204106648684693 ) ) ;
#69589 = AXIS2_PLACEMENT_3D ( 'NONE', #13692, #179419, #44090 ) ;
#69590 = CARTESIAN_POINT ( 'NONE',  ( 3.016274402391531773, 2.160936140102893255, -0.2104436154053441199 ) ) ;
#69591 = CARTESIAN_POINT ( 'NONE',  ( 5.118366684358879759, 5.930181538962194132, 1.199719254218462483 ) ) ;
#69592 = CARTESIAN_POINT ( 'NONE',  ( 4.346888830327386266, -1.803415170841724979, -0.9023466997552240798 ) ) ;
#69593 = CARTESIAN_POINT ( 'NONE',  ( 2.531250000000001332, -0.7852924748301189917, -1.895863743164030613 ) ) ;
#69594 = AXIS2_PLACEMENT_3D ( 'NONE', #197029, #114783, #115844 ) ;
#69595 = B_SPLINE_CURVE_WITH_KNOTS ( 'NONE', 3,
 ( #150588, #70354, #187327, #105039, #185182, #54141 ),
 .UNSPECIFIED., .F., .F.,
 ( 4, 2, 4 ),
 ( 0.000000000000000000, 0.001226111284895916318, 0.002452222569791832202 ),
 .UNSPECIFIED. ) ;
#69596 = CARTESIAN_POINT ( 'NONE',  ( -1.500000000000011324, 3.702083334016152971, 0.8660254037844403729 ) ) ;
#69597 = CARTESIAN_POINT ( 'NONE',  ( 1.623919080003157545, -1.068017489352061533, -1.603033266432315918 ) ) ;
#69598 = CARTESIAN_POINT ( 'NONE',  ( 1.499999999999993117, 8.635416667349460340, 0.8660254037844409281 ) ) ;
#69599 = CARTESIAN_POINT ( 'NONE',  ( 4.412477314457364130, -2.220925182493800776, -0.05286738749475486387 ) ) ;
#69600 = EDGE_LOOP ( 'NONE', ( #76078, #165591 ) ) ;
#69602 = CIRCLE ( 'NONE', #211549, 0.07999999999999998779 ) ;
#69601 = CARTESIAN_POINT ( 'NONE',  ( -0.1106856583841060310, -0.002128758811529348188, -1.996853503091333470 ) ) ;
#69603 = CARTESIAN_POINT ( 'NONE',  ( 1.499999999999989120, 1.775000000000019673, 0.000000000000000000 ) ) ;
#69604 = CARTESIAN_POINT ( 'NONE',  ( 4.964256800898067645, 8.943383367689749619, 0.7998128361456462443 ) ) ;
#69605 = CARTESIAN_POINT ( 'NONE',  ( 4.107757354816228279, 6.775838766385488654, -1.082531754730548412 ) ) ;
#69606 = CARTESIAN_POINT ( 'NONE',  ( 0.000000000000000000, -1.246874999522042948, -3.793834371823813445 ) ) ;
#69607 = CARTESIAN_POINT ( 'NONE',  ( 1.067367041543025197, -1.747990651676500029, 1.370551686305313321 ) ) ;
#69608 = CARTESIAN_POINT ( 'NONE',  ( 6.338335788673861160, -1.050647824335379399, 1.656640365463659892 ) ) ;
#69609 = CARTESIAN_POINT ( 'NONE',  ( 8.026063749610047537, 10.38682701267698150, -1.443375672974057666 ) ) ;
#69610 = CARTESIAN_POINT ( 'NONE',  ( 2.359223927328457648E-13, 7.078193277237625480, 2.121339347286388843 ) ) ;
#69611 = CARTESIAN_POINT ( 'NONE',  ( 0.3862812426984676972, -1.019270635400490121, 1.906220128828392646 ) ) ;
#69612 = CARTESIAN_POINT ( 'NONE',  ( 3.555981428534177091, 7.370671776590375757, 0.7998128361456271485 ) ) ;
#69613 = CARTESIAN_POINT ( 'NONE',  ( -3.689227196694341515, 7.318199139536432973, -0.7216878364870458196 ) ) ;
#69614 = CARTESIAN_POINT ( 'NONE',  ( 3.367685602802727551, -0.4050715705573506575, 2.022353529335896294 ) ) ;
#69615 = CARTESIAN_POINT ( 'NONE',  ( -5.766295404513795297, 5.621766148221195358, 0.7998128361456341429 ) ) ;
#69616 = CARTESIAN_POINT ( 'NONE',  ( 1.499999999999990896, 3.556250000682818602, 1.214306433183764966E-14 ) ) ;
#69617 = CARTESIAN_POINT ( 'NONE',  ( -1.364683531249997417, 5.571875000341417916, 1.214306433183764966E-14 ) ) ;
#69618 = CARTESIAN_POINT ( 'NONE',  ( 6.485618507650338316, 1.290063292742931633, 1.354747167150817333 ) ) ;
#69619 = CARTESIAN_POINT ( 'NONE',  ( 5.168516884834092551, 1.170641038942145995, 1.279587065987584982 ) ) ;
#69620 = CARTESIAN_POINT ( 'NONE',  ( 3.684860642351639903, 1.263529365103865709, 1.197186439443503003 ) ) ;
#69621 = CARTESIAN_POINT ( 'NONE',  ( 1.699181366971340701, 1.908771516627869147, 1.269207382326368316 ) ) ;
#69622 = CARTESIAN_POINT ( 'NONE',  ( -0.6823417656250212460, 4.113541667008085767, 1.181850606188767472 ) ) ;
#69623 = CARTESIAN_POINT ( 'NONE',  ( 5.372635804747151411, -0.05242855794247149731, -2.090268718351683930 ) ) ;
#69624 = CARTESIAN_POINT ( 'NONE',  ( -0.02377707250108065939, -0.1326659201078099481, -1.811169398030491928 ) ) ;
#69625 = ADVANCED_FACE ( 'NONE', ( #55431 ), #174308, .T. ) ;
#69626 = DIRECTION ( 'NONE',  ( 1.000000000000000000, -4.985516615831701596E-16, 0.000000000000000000 ) ) ;
#69627 = SHAPE_REPRESENTATION_RELATIONSHIP ( 'NONE' , 'NONE' ,  #188305, #55192 ) ;
#69628 = CARTESIAN_POINT ( 'NONE',  ( 1.986954140179174155, -2.015912935764123670, 0.05229865529512293942 ) ) ;
#69629 = CARTESIAN_POINT ( 'NONE',  ( 0.5159075615763093481, -1.175655012515547160, -1.849222068403690411 ) ) ;
#69630 = CARTESIAN_POINT ( 'NONE',  ( 9.412040618821951199, 14.12872955391332930, -8.482482427019883531 ) ) ;
#69631 = CARTESIAN_POINT ( 'NONE',  ( -6.679363233026820446, 10.94434087183997129, 0.000000000000000000 ) ) ;
#69632 =( BOUNDED_CURVE ( )  B_SPLINE_CURVE ( 2, ( #46116, #112233, #79657, #63413, #195551, #92735, #10377 ),
 .UNSPECIFIED., .F., .T. ) 
 B_SPLINE_CURVE_WITH_KNOTS ( ( 3, 2, 2, 3 ),
 ( 0.01785714285714263064, 0.02380952380952366942, 0.02976190476190470821, 0.03571428571428574700 ),
 .UNSPECIFIED. ) 
 CURVE ( )  GEOMETRIC_REPRESENTATION_ITEM ( )  RATIONAL_B_SPLINE_CURVE ( ( 1.000000000000005107, 0.8660254037844337116, 1.000000000000000000, 0.8660254037844387076, 1.000000000000000000, 0.8660254037844379305, 1.000000000000000666 ) ) 
 REPRESENTATION_ITEM ( '' )  );
#69633 = CARTESIAN_POINT ( 'NONE',  ( 5.120175567455225618, 9.125288595339771547, -0.7998128361456281477 ) ) ;
#69634 = CARTESIAN_POINT ( 'NONE',  ( 2.983181628360128013, -1.960071735995170927, -0.8095406527153581333 ) ) ;
#69635 = CARTESIAN_POINT ( 'NONE',  ( -1.364683531250000748, -1.240624999658580752, 0.000000000000000000 ) ) ;
#69636 = CARTESIAN_POINT ( 'NONE',  ( 5.022008369909983116, -0.9795521577263366364, -1.540466923627185292 ) ) ;
#69637 = VERTEX_POINT ( 'NONE', #156148 ) ;
#69638 = CARTESIAN_POINT ( 'NONE',  ( -5.956828388357799042, 8.042995434541133193, 1.599625672291263179 ) ) ;
#69639 = CARTESIAN_POINT ( 'NONE',  ( -6.520158902582610772, 5.290451655907115303, -2.438235897557448961 ) ) ;
#69640 = CARTESIAN_POINT ( 'NONE',  ( -3.285556943750000514, -0.2260416661887102996, -1.896917185911906500 ) ) ;
#69641 = CARTESIAN_POINT ( 'NONE',  ( -7.152089726408780379, 8.302858421353754181, -1.199719254218446718 ) ) ;
#69642 = CARTESIAN_POINT ( 'NONE',  ( 1.986587785418312047, -1.239364722674634933, 1.594781737346209871 ) ) ;
#69643 = CARTESIAN_POINT ( 'NONE',  ( 6.821333372217227797, -0.1664864972488830641, 2.170661319153658564 ) ) ;
#69644 = CARTESIAN_POINT ( 'NONE',  ( 9.459838494033030898, 12.05956421450382088, 1.599625672291281386 ) ) ;
#69645 = CARTESIAN_POINT ( 'NONE',  ( 4.223391696059366929, 0.2311737859471388323, -1.846484453672825321 ) ) ;
#69646 = CARTESIAN_POINT ( 'NONE',  ( 7.865701674222579598, 12.32840238656838139, -0.7998128361456352531 ) ) ;
#69647 = ADVANCED_FACE ( 'NONE', ( #7730 ), #167329, .T. ) ;
#69648 = DIRECTION ( 'NONE',  ( 0.000000000000000000, 0.000000000000000000, 1.000000000000000000 ) ) ;
#69649 = ORIENTED_EDGE ( 'NONE', *, *, #71209, .T. ) ;
#69650 = CARTESIAN_POINT ( 'NONE',  ( -5.088387723830502196, 4.830873854090670605, -0.7998128361456221525 ) ) ;
#69651 = CARTESIAN_POINT ( 'NONE',  ( -7.588813295347149435, 9.876701482703580837, -1.599625672291263179 ) ) ;
#69652 = CARTESIAN_POINT ( 'NONE',  ( 5.180226163740526246, -1.011166736308216629, 1.519887457628710248 ) ) ;
#69654 = CARTESIAN_POINT ( 'NONE',  ( -4.096253560606756494, 7.689279582349398012, -0.7399548657811344521 ) ) ;
#69653 = CARTESIAN_POINT ( 'NONE',  ( -5.074494633264801990, 9.142270515442742607, 0.7998128361456291469 ) ) ;
#69655 = CARTESIAN_POINT ( 'NONE',  ( 4.913571454530422322, 8.125067815752732514, -1.031885869761673069 ) ) ;
#69656 = CARTESIAN_POINT ( 'NONE',  ( 1.334805274328724867, -1.105471761691357191, 1.335692278477951689 ) ) ;
#69657 = CARTESIAN_POINT ( 'NONE',  ( 6.492148756324659153, -0.4961259030743305209, -1.772972609911625419 ) ) ;
#69659 = CARTESIAN_POINT ( 'NONE',  ( 7.782016984564054773, 10.10210578678999482, 1.443375672974076540 ) ) ;
#69658 = CARTESIAN_POINT ( 'NONE',  ( 5.391387774523593635, 2.037479383949382772, -1.083606018200606869 ) ) ;
#69660 = CARTESIAN_POINT ( 'NONE',  ( 5.415556014015861841, 5.282846535965431300, -0.7998128361456481317 ) ) ;
#69661 = CARTESIAN_POINT ( 'NONE',  ( 1.352885421680804834, -1.626251134426279332, 1.265669239494594311 ) ) ;
#69662 = CARTESIAN_POINT ( 'NONE',  ( 5.982172092127724383, 8.002286745614243912, -1.599625672291262513 ) ) ;
#69663 = CARTESIAN_POINT ( 'NONE',  ( 6.802148291397191571, -2.057678525504004430, 1.024270743344313672 ) ) ;
#69664 = DIRECTION ( 'NONE',  ( 0.000000000000000000, 0.000000000000000000, 1.000000000000000000 ) ) ;
#69665 = CARTESIAN_POINT ( 'NONE',  ( -7.208094944320834863, 8.438474185576302133, -1.199719254218452047 ) ) ;
#69666 = AXIS2_PLACEMENT_3D ( 'NONE', #53504, #155280, #137969 ) ;
#69667 = CARTESIAN_POINT ( 'NONE',  ( 0.1453086613420169204, -1.522338971917249317, -1.252298935284136938 ) ) ;
#69670 = EDGE_CURVE ( 'NONE', #76077, #64117, #53077, .T. ) ;
#69669 = CARTESIAN_POINT ( 'NONE',  ( -6.238160076063538284, 9.331584951165851294, 1.082531754730549967 ) ) ;
#69668 = CARTESIAN_POINT ( 'NONE',  ( 3.972844611716894736, -1.413603510852480927, 1.288168406687495215 ) ) ;
#69671 = CARTESIAN_POINT ( 'NONE',  ( 5.145248760827346501, -1.894204247122273088, 1.132176536499051700 ) ) ;
#69672 = CARTESIAN_POINT ( 'NONE',  ( -1.225000000000038058, 2.083333334016205907, 0.7072540797572697269 ) ) ;
#69673 = CARTESIAN_POINT ( 'NONE',  ( -1.115562610750309283E-14, 9.093750000682799595, 1.500000000000001554 ) ) ;
#69674 = CARTESIAN_POINT ( 'NONE',  ( 4.597623488365603528, 5.496887170248887067, -1.082531754730548412 ) ) ;
#69675 = CARTESIAN_POINT ( 'NONE',  ( -5.112833325684928987, 5.137596099486740897, -0.7216878364870338292 ) ) ;
#69676 = CARTESIAN_POINT ( 'NONE',  ( 5.514351353798126354, -2.120667953778174741, 0.0001357579994532010219 ) ) ;
#69677 = ORIENTED_EDGE ( 'NONE', *, *, #159645, .T. ) ;
#69678 = EDGE_CURVE ( 'NONE', #179460, #158767, #105037, .T. ) ;
#69679 = CARTESIAN_POINT ( 'NONE',  ( 3.470030448073280205, 2.251904571161921442, -0.5032320387977330389 ) ) ;
#69680 = CARTESIAN_POINT ( 'NONE',  ( 4.281663391851794565, -1.878042059144067633, 0.5673916069991248312 ) ) ;
#69681 = CARTESIAN_POINT ( 'NONE',  ( 1.182386158793121256, 1.172985831986381955, -1.572276950389992933 ) ) ;
#69682 = CARTESIAN_POINT ( 'NONE',  ( 11.78331023100045627, 13.79999999999999893, -1.800000000000001155 ) ) ;
#69683 = CARTESIAN_POINT ( 'NONE',  ( 0.07801928546527701902, -7.184999792974072541, -9.499679989893801135 ) ) ;
#69684 = ORIENTED_EDGE ( 'NONE', *, *, #37494, .T. ) ;
#69685 = CARTESIAN_POINT ( 'NONE',  ( 5.225796113160614986, 0.8128206588041908542, -1.845625551132886288 ) ) ;
#69686 = CARTESIAN_POINT ( 'NONE',  ( -8.402302512167102222, 10.82577223566020841, -1.599625672291263179 ) ) ;
#69687 = DIRECTION ( 'NONE',  ( -5.551115123125782702E-17, 0.000000000000000000, 1.000000000000000000 ) ) ;
#69688 = CARTESIAN_POINT ( 'NONE',  ( 3.239314478175295164, -0.1551929672521153158, -2.165549275587749456 ) ) ;
#69689 = CARTESIAN_POINT ( 'NONE',  ( 10.70618812723756719, 9.877096652175534786, -5.429715724251639841 ) ) ;
#69690 = CARTESIAN_POINT ( 'NONE',  ( 0.8969213510382867405, -2.070190491330957006, -0.4589741369691033857 ) ) ;
#69691 = CARTESIAN_POINT ( 'NONE',  ( 0.7499999999999902300, 1.764583334016148086, 1.299038105676657340 ) ) ;
#69692 = CARTESIAN_POINT ( 'NONE',  ( 9.999301985278609806, 11.62460605670194447, 1.199719254218452047 ) ) ;
#69693 = CARTESIAN_POINT ( 'NONE',  ( 9.549638505170030101, -6.527411821100059797, -0.4330238300980903676 ) ) ;
#69694 = CARTESIAN_POINT ( 'NONE',  ( 6.578229047358968629, 6.784305542873760864, 0.2988042929856441488 ) ) ;
#69695 = ORIENTED_EDGE ( 'NONE', *, *, #170541, .T. ) ;
#69696 = CARTESIAN_POINT ( 'NONE',  ( 2.214203678495901606, -0.9685002052983943122, -1.818986401426671229 ) ) ;
#69697 = CIRCLE ( 'NONE', #42074, 3.475000000000000089 ) ;
#69699 = CARTESIAN_POINT ( 'NONE',  ( 4.370663978927085580, 5.060324124126027279, -2.420000000000000373 ) ) ;
#69698 = CARTESIAN_POINT ( 'NONE',  ( 1.419999999999990603, 6.280000000000042881, 2.900000000000001688 ) ) ;
#69700 = CARTESIAN_POINT ( 'NONE',  ( -1.201851678989727383E-14, 1.571875000341420581, 1.575800808251672791 ) ) ;
#69701 = CARTESIAN_POINT ( 'NONE',  ( 0.000000000000000000, 0.000000000000000000, 0.000000000000000000 ) ) ;
#69702 = EDGE_LOOP ( 'NONE', ( #167911, #132865, #64185, #26725, #167796, #43357, #180089, #214044 ) ) ;
#69703 = CARTESIAN_POINT ( 'NONE',  ( 5.057238878282278804, -1.638088962530854786, 0.9864336689310859718 ) ) ;
#69704 = CARTESIAN_POINT ( 'NONE',  ( -3.475000000000000533, -1.049999999999998934, 0.000000000000000000 ) ) ;
#69705 = CARTESIAN_POINT ( 'NONE',  ( -4.613852347352193739, 4.277249248199312071, 1.214306433183764966E-14 ) ) ;
#69706 = CARTESIAN_POINT ( 'NONE',  ( -0.03528172390533482194, -1.455059732361897895, 1.078909735853793794 ) ) ;
#69708 = CARTESIAN_POINT ( 'NONE',  ( 1.024461926017742996, 0.3770999164835596162, 1.878046770817816791 ) ) ;
#69707 = CARTESIAN_POINT ( 'NONE',  ( 3.967483781714987057, 7.780481511976146791, -0.4145792352998460273 ) ) ;
#69709 = CARTESIAN_POINT ( 'NONE',  ( 2.383334800519558705, -0.002349189141126820958, 2.070544812199434315 ) ) ;
#69710 = CARTESIAN_POINT ( 'NONE',  ( 1.364683531249986537, -0.3239583329919163424, 0.7879004041258500513 ) ) ;
#69711 = CIRCLE ( 'NONE', #571, 10.99999999999999112 ) ;
#69712 = CARTESIAN_POINT ( 'NONE',  ( 0.5320225927652595388, 1.015637564890453426, -1.689598002260852772 ) ) ;
#69713 = CARTESIAN_POINT ( 'NONE',  ( 3.158640206316553289, -1.382037546686708973, 1.193037399656725395 ) ) ;
#69715 = CARTESIAN_POINT ( 'NONE',  ( 5.779562687394081522, 7.242644825714458001, 1.188994900607452054 ) ) ;
#69714 = CARTESIAN_POINT ( 'NONE',  ( 6.340462157465731607, 2.182225300935904055, 0.3281612982340698093 ) ) ;
#69716 = CARTESIAN_POINT ( 'NONE',  ( -1.364683531250012516, 1.030208333674754062, 0.7879004041258379498 ) ) ;
#69717 = CARTESIAN_POINT ( 'NONE',  ( 3.648931631147700472, -0.3995851234466942792, -2.023444851274053491 ) ) ;
#69718 = CARTESIAN_POINT ( 'NONE',  ( -5.038826645773246682, 9.030381520044109322, 0.7998128361456481317 ) ) ;
#69719 = CARTESIAN_POINT ( 'NONE',  ( 7.832860060393120882, 10.16142270859057462, 1.599625672291281386 ) ) ;
#69720 = CARTESIAN_POINT ( 'NONE',  ( 3.032219910950674890, 6.689340329417765574, 0.7998128361456321445 ) ) ;
#69721 = CARTESIAN_POINT ( 'NONE',  ( 6.166260936116925606, 6.088392601758203071, 0.7998128361456341429 ) ) ;
#69723 = CARTESIAN_POINT ( 'NONE',  ( -1.201851678989727383E-14, 3.837500000000021227, -1.732050807568863648 ) ) ;
#69722 = CARTESIAN_POINT ( 'NONE',  ( 4.981522283868931034, 1.966010104637575751, -0.7553895412903822715 ) ) ;
#69724 = CARTESIAN_POINT ( 'NONE',  ( 0.1687529456618936941, -0.9278834597439933329, -1.960587321289827267 ) ) ;
#69725 = CARTESIAN_POINT ( 'NONE',  ( -1.364683531250014514, 2.051041667008086655, -0.7879004041258289570 ) ) ;
#69726 = CARTESIAN_POINT ( 'NONE',  ( 5.431013727915853906, 0.1530101862373678123, 2.156222312673663488 ) ) ;
#69727 = CARTESIAN_POINT ( 'NONE',  ( 4.266274442087925500, 2.019191850312745284, -0.05169103710895606163 ) ) ;
#69728 = CARTESIAN_POINT ( 'NONE',  ( 6.620655732516645742, 7.051964633898824886, 2.771890290588132189 ) ) ;
#69731 = CARTESIAN_POINT ( 'NONE',  ( 6.670248388243460447, 6.884303995813253252, -0.7216878364870257245 ) ) ;
#69730 = CARTESIAN_POINT ( 'NONE',  ( -3.285556943750000514, -3.988541666188710089, -1.896917185911906500 ) ) ;
#69729 = CARTESIAN_POINT ( 'NONE',  ( 9.365395945939138045, 13.54490846161957585, -7.373992051513669210 ) ) ;
#69732 = CARTESIAN_POINT ( 'NONE',  ( -5.121948170912633991, 9.197632976031879792, -0.7998128361456362523 ) ) ;
#69733 = CARTESIAN_POINT ( 'NONE',  ( 2.307827663788959871, -1.164988201124015577, -1.645758576239789051 ) ) ;
#69734 = CARTESIAN_POINT ( 'NONE',  ( -9.840520565420403543, 10.37502883594562597, 1.040834085586084257E-14 ) ) ;
#69736 = CARTESIAN_POINT ( 'NONE',  ( -0.9486429539237359876, 3.105410930033766448, 1.028101543438980858 ) ) ;
#69735 = CARTESIAN_POINT ( 'NONE',  ( -5.091250377131585125, 5.898545847196970726, 1.199719254218450271 ) ) ;
#69737 = DIRECTION ( 'NONE',  ( 1.276756478318932585E-15, -1.000000000000000000, 1.665334536937738262E-16 ) ) ;
#69738 = CARTESIAN_POINT ( 'NONE',  ( 6.720655732516659597, 0.5653683226944251627, 2.225905711026022971 ) ) ;
#69740 = CARTESIAN_POINT ( 'NONE',  ( 4.780875152847498200, 1.674876996157638187, -1.122516304564516565 ) ) ;
#69739 = CARTESIAN_POINT ( 'NONE',  ( -7.849807752188049825, 8.260456587081938196, 0.7216878364870578100 ) ) ;
#69741 = CARTESIAN_POINT ( 'NONE',  ( 0.7499999999999902300, 5.566666666666685082, -1.299038105676658228 ) ) ;
#69742 = CARTESIAN_POINT ( 'NONE',  ( 0.4863796390984359008, -0.2058623683223875511, -1.712490539465325146 ) ) ;
#69743 = CARTESIAN_POINT ( 'NONE',  ( 6.574778147984297938, 6.635272358928617997, -0.7998128361456481317 ) ) ;
#69745 = LINE ( 'NONE', #136921, #159989 ) ;
#69744 = CARTESIAN_POINT ( 'NONE',  ( 8.188761592974039161, 10.57664116326830595, -1.443375672974063439 ) ) ;
#69746 = CARTESIAN_POINT ( 'NONE',  ( -11.52494907509597155, 8.147870201683055313, 3.187903436646419397 ) ) ;
#69747 = CARTESIAN_POINT ( 'NONE',  ( 5.571519856497625156, 1.802974293077023393, -0.4980454429602265698 ) ) ;
#69748 = CARTESIAN_POINT ( 'NONE',  ( 6.240495565780414644, 1.155569484861172391, -1.648366056897664800 ) ) ;
#69749 = DIRECTION ( 'NONE',  ( 1.000000000000000000, -0.000000000000000000, -0.000000000000000000 ) ) ;
#69750 = CIRCLE ( 'NONE', #125219, 2.000000000000000000 ) ;
#69751 = CARTESIAN_POINT ( 'NONE',  ( -6.658462837642833421, 8.861568958707010779, 1.443375672974064550 ) ) ;
#69752 = ORIENTED_EDGE ( 'NONE', *, *, #213928, .F. ) ;
#69754 = CARTESIAN_POINT ( 'NONE',  ( 9.042925270190622200, 12.53353466765568669, 1.082531754730546636 ) ) ;
#69753 = STYLED_ITEM ( 'NONE', ( #42438 ), #49851 ) ;
#69755 = CARTESIAN_POINT ( 'NONE',  ( 0.1050925082292548940, -0.09611335402343046397, 2.014234898253919326 ) ) ;
#69756 = CARTESIAN_POINT ( 'NONE',  ( 1.423755586445039745, -1.797672382977614669, 0.2236433623570739382 ) ) ;
#69757 = CARTESIAN_POINT ( 'NONE',  ( 6.984385409695311964, 8.177479728513226576, 1.199719254218452935 ) ) ;
#69758 = CARTESIAN_POINT ( 'NONE',  ( -0.06814526087293248935, -6.511064858252400889, -10.88932262995847822 ) ) ;
#69759 = CARTESIAN_POINT ( 'NONE',  ( 7.687109908824030668, 10.95175007939464606, -1.082531754730543083 ) ) ;
#69760 = CARTESIAN_POINT ( 'NONE',  ( 7.450369105909416589, 8.650851030771185890, -1.199719254218441611 ) ) ;
#69762 = CARTESIAN_POINT ( 'NONE',  ( 0.2510146965912671835, 0.1847738873272772309, -1.906744464555621521 ) ) ;
#69761 = CARTESIAN_POINT ( 'NONE',  ( -5.066996723205291708, 6.934582148538044777, 1.599625672291267398 ) ) ;
#69763 = LINE ( 'NONE', #84970, #173402 ) ;
#69764 = CARTESIAN_POINT ( 'NONE',  ( 6.927853306458752414, 7.184843067064434763, 0.7216878364870317197 ) ) ;
#69765 = CARTESIAN_POINT ( 'NONE',  ( 0.6823417656249864960, -1.011458332991911568, -1.181850606188749264 ) ) ;
#69767 = ORIENTED_EDGE ( 'NONE', *, *, #83695, .T. ) ;
#69766 = CARTESIAN_POINT ( 'NONE',  ( 4.256897045010922476, 5.029096643009940415, -1.082531754730548412 ) ) ;
#69768 = CARTESIAN_POINT ( 'NONE',  ( -2.948008335967658322, 5.526761261015804116, 1.199719254218462483 ) ) ;
#69769 = CARTESIAN_POINT ( 'NONE',  ( 4.329101982860062314, 0.1031891237209987822, 2.159356164053369387 ) ) ;
#69770 = CARTESIAN_POINT ( 'NONE',  ( -6.536439455564198475, 8.719208346281938304, 1.443375672974064550 ) ) ;
#69771 = CARTESIAN_POINT ( 'NONE',  ( 5.058600711674583472, 8.915801573680086634, 0.000000000000000000 ) ) ;
#69772 = CARTESIAN_POINT ( 'NONE',  ( 0.3168469074051638579, -0.7203255543706194031, -1.994627023381766673 ) ) ;
#69773 = CARTESIAN_POINT ( 'NONE',  ( 2.038291622189229546, 1.949329857042367387, 0.2932346777646984148 ) ) ;
#69774 = CARTESIAN_POINT ( 'NONE',  ( 4.500206361630255003, -0.8965733778899236395, 1.689174240301967389 ) ) ;
#69775 = ORIENTED_EDGE ( 'NONE', *, *, #5833, .T. ) ;
#69776 = CARTESIAN_POINT ( 'NONE',  ( 9.491250020638661411, -6.775781654326489267, -0.2167848519283618325 ) ) ;
#69777 = CARTESIAN_POINT ( 'NONE',  ( 5.881302004902690506, -0.04997076178031189392, 1.969097942535046331 ) ) ;
#69778 = CARTESIAN_POINT ( 'NONE',  ( 0.8845914429877841378, 1.712865214261191316, -0.9150308779080836841 ) ) ;
#69779 = ORIENTED_EDGE ( 'NONE', *, *, #28627, .F. ) ;
#69780 = CARTESIAN_POINT ( 'NONE',  ( -3.610214042988883598, 7.433943160120816351, 0.7998128361456352531 ) ) ;
#69782 = CARTESIAN_POINT ( 'NONE',  ( 11.84668730067608600, 12.69999999999999929, -1.400000000000001910 ) ) ;
#69781 = CARTESIAN_POINT ( 'NONE',  ( -2.972980823146582186, 6.690504403638126263, 0.000000000000000000 ) ) ;
#69784 = CARTESIAN_POINT ( 'NONE',  ( 5.180624093753221970, 9.058162186105164437, 0.000000000000000000 ) ) ;
#69783 = CARTESIAN_POINT ( 'NONE',  ( 7.969495366734495434, 8.192166104145387706, 1.040834085586084257E-14 ) ) ;
#69785 = ORIENTED_EDGE ( 'NONE', *, *, #207315, .T. ) ;
#69786 = ADVANCED_FACE ( 'NONE', ( #213382 ), #195008, .T. ) ;
#69787 = CARTESIAN_POINT ( 'NONE',  ( 0.4115098346569624477, 1.921242953230850148, 1.085561749797583797 ) ) ;
#69788 = CARTESIAN_POINT ( 'NONE',  ( -5.586581854188635177, 5.810800913040471194, -0.4357733342581562863 ) ) ;
#69789 = CARTESIAN_POINT ( 'NONE',  ( 0.1703706300211875746, 0.7318840393725855042, 1.766877091004593225 ) ) ;
#69790 = CARTESIAN_POINT ( 'NONE',  ( -0.02338929933909209696, 6.948787603726593431, -2.306014233525994772 ) ) ;
#69791 = DIRECTION ( 'NONE',  ( 0.000000000000000000, 0.000000000000000000, 1.000000000000000000 ) ) ;
#69792 = CARTESIAN_POINT ( 'NONE',  ( 7.002681350352349732, -8.176227052203545398, -6.455298931196944423 ) ) ;
#69793 = CARTESIAN_POINT ( 'NONE',  ( 2.840353284027045344, -1.066491845456703835, 1.774417039089710935 ) ) ;
#69794 = CARTESIAN_POINT ( 'NONE',  ( -5.087333953625788219, 6.958308917361963886, 1.599625672291267398 ) ) ;
#69795 = CARTESIAN_POINT ( 'NONE',  ( -4.964107424972056037, 7.970992240003957008, 1.031144368780096965 ) ) ;
#69797 = CARTESIAN_POINT ( 'NONE',  ( 0.09294085500742564621, -0.4768749645070144982, -2.116232079886640971 ) ) ;
#69796 = CARTESIAN_POINT ( 'NONE',  ( -2.903417451620861289, 6.539070793532962611, 0.7998128361456341429 ) ) ;
#69798 = CARTESIAN_POINT ( 'NONE',  ( 2.947022816757136621, -1.793111998972513277, -1.259777465452505796 ) ) ;
#69799 = CYLINDRICAL_SURFACE ( 'NONE', #90024, 1.500000000000000222 ) ;
#69800 = ADVANCED_FACE ( 'NONE', ( #161483 ), #129384, .T. ) ;
#69801 = CARTESIAN_POINT ( 'NONE',  ( -1.364683531250014514, 13.65104166700806765, -0.7879004041258335089 ) ) ;
#69802 = CARTESIAN_POINT ( 'NONE',  ( -5.712781623311813384, 7.758274208654143855, -1.599625672291271394 ) ) ;
#69803 = ADVANCED_FACE ( 'NONE', ( #79140 ), #185843, .T. ) ;
#69804 = CARTESIAN_POINT ( 'NONE',  ( 5.818968308277153056, 0.8464176696867716787, -1.513466976307031642 ) ) ;
#69805 = VECTOR ( 'NONE', #158681, 1000.000000000000000 ) ;
#69806 = CARTESIAN_POINT ( 'NONE',  ( -3.952365473583647315, 4.569846793057691592, 1.199719254218462483 ) ) ;
#69807 = CARTESIAN_POINT ( 'NONE',  ( 3.168866831888625946, 1.502704456927813403, -1.424286459396295390 ) ) ;
#69808 = CARTESIAN_POINT ( 'NONE',  ( 4.130539392780770314, 0.5663510459464686786, 2.039993263092474418 ) ) ;
#69809 = CARTESIAN_POINT ( 'NONE',  ( 5.425234023762710578, 9.481190127698507553, -0.7998128361456291469 ) ) ;
#69810 = CARTESIAN_POINT ( 'NONE',  ( 1.364683531249990311, 4.613541667008083103, 0.7879004041258499402 ) ) ;
#69811 = CARTESIAN_POINT ( 'NONE',  ( 3.239063133055252841, -0.1400698962470778297, -1.964493882382233991 ) ) ;
#69812 = CARTESIAN_POINT ( 'NONE',  ( 0.8086807686161383568, -0.4671638426185490967, -1.854305266343849734 ) ) ;
#69813 = CARTESIAN_POINT ( 'NONE',  ( 5.173897996269102961, -1.276782452619073860, 1.903577390058891261 ) ) ;
#69814 = CARTESIAN_POINT ( 'NONE',  ( 3.246530741642670748, 0.4443377543969920795, 1.770662692542070760 ) ) ;
#69815 = CARTESIAN_POINT ( 'NONE',  ( 3.555981428534177091, 7.370671776590375757, 0.7998128361456271485 ) ) ;
#69816 = CARTESIAN_POINT ( 'NONE',  ( 6.765155463094761679, 6.995028916473103209, 0.7216878364870317197 ) ) ;
#69817 = CARTESIAN_POINT ( 'NONE',  ( -5.845536785786364931, 9.971543350059432598, 0.000000000000000000 ) ) ;
#69818 = CARTESIAN_POINT ( 'NONE',  ( 3.955341514648374357, -1.749461739742008470, 0.9961098753780948112 ) ) ;
#69819 = CARTESIAN_POINT ( 'NONE',  ( 2.764445781119912127, -0.7462812867886670087, -1.814464804917370166 ) ) ;
#69820 = CARTESIAN_POINT ( 'NONE',  ( -6.672584156219988571, 10.93643194889866521, -0.7998128361456291469 ) ) ;
#69821 = CARTESIAN_POINT ( 'NONE',  ( -6.084912014434944894, 5.993485526462540847, -0.7998128361456291469 ) ) ;
#69822 = CARTESIAN_POINT ( 'NONE',  ( 0.1751657365761703222, 4.087554309226840488, -2.598743260590470783 ) ) ;
#69824 = CARTESIAN_POINT ( 'NONE',  ( 5.875818619555242428, 1.057306330162042451, 1.419162741687775231 ) ) ;
#69823 = CARTESIAN_POINT ( 'NONE',  ( 6.527293198192279711, -1.364605693714017187, -1.583936087800744907 ) ) ;
#69825 = CARTESIAN_POINT ( 'NONE',  ( 3.152240666618498555, 6.104686963247638154, 0.9091918461422390241 ) ) ;
#69826 = CARTESIAN_POINT ( 'NONE',  ( 1.552940555598739891, -1.880887156831068552, -1.124362282834884263 ) ) ;
#69827 = CARTESIAN_POINT ( 'NONE',  ( 0.3447215323711784740, 0.5487897507440896439, -1.651745661738156734 ) ) ;
#69828 = CARTESIAN_POINT ( 'NONE',  ( 7.613066949273408213, 8.840665181362512115, -1.199719254218441611 ) ) ;
#69829 = CARTESIAN_POINT ( 'NONE',  ( 0.2333690889706926119, 0.7157316027301027228, -2.136973218959358434 ) ) ;
#69830 = CARTESIAN_POINT ( 'NONE',  ( 0.5391470445266118849, -1.216214603651460724, -1.223400588829765878 ) ) ;
#69831 = CARTESIAN_POINT ( 'NONE',  ( 0.8260327929942178349, -1.663255926670023976, 1.586464751714482979 ) ) ;
#69832 = CARTESIAN_POINT ( 'NONE',  ( 0.6092356648998223934, -0.3158941238240610128, 2.168550393043596536 ) ) ;
#69833 = CARTESIAN_POINT ( 'NONE',  ( 6.802075984838630518, -1.546572159107060251, 0.7837757703139431875 ) ) ;
#69834 = CARTESIAN_POINT ( 'NONE',  ( 2.789901687333019797, 1.561178712900921584, 1.560079944692857046 ) ) ;
#69835 = CARTESIAN_POINT ( 'NONE',  ( 6.812935010865087015, -1.682745870255862641, 1.371614790115786908 ) ) ;
#69836 = DIRECTION ( 'NONE',  ( 0.000000000000000000, -1.000000000000000000, 0.000000000000000000 ) ) ;
#69837 = CARTESIAN_POINT ( 'NONE',  ( 0.6380961361360514283, 2.114605634092497688, -0.1105060169243020224 ) ) ;
#69838 = CARTESIAN_POINT ( 'NONE',  ( 6.727182134110222478, 4.688348259194305534, 2.751590707055273199 ) ) ;
#69839 = CARTESIAN_POINT ( 'NONE',  ( 5.385741010672205675, 1.293702408046822239, 1.427520146239504184 ) ) ;
#69840 = VERTEX_POINT ( 'NONE', #60894 ) ;
#69842 = CARTESIAN_POINT ( 'NONE',  ( -0.7499999999999972244, 5.358333333333353821, -1.299038105676652011 ) ) ;
#69841 = CARTESIAN_POINT ( 'NONE',  ( 1.206998765908244176, 2.024556473040285187, 1.075228724532976132 ) ) ;
#69843 = CARTESIAN_POINT ( 'NONE',  ( 3.171717870593107058, 5.787755718078879674, -1.199719254218446718 ) ) ;
#69844 = CARTESIAN_POINT ( 'NONE',  ( 5.982172092127724383, 8.002286745614243912, -1.599625672291262513 ) ) ;
#69845 = CARTESIAN_POINT ( 'NONE',  ( 3.826986476844072005, 1.570263387305373737, -1.571374446222243204 ) ) ;
#69846 = CARTESIAN_POINT ( 'NONE',  ( -7.321039761699444703, 10.52466824108257804, 1.082531754730549967 ) ) ;
#69847 = DIRECTION ( 'NONE',  ( 0.6507913734559640506, -0.7592566023653004592, 0.000000000000000000 ) ) ;
#69848 = CARTESIAN_POINT ( 'NONE',  ( 5.883875478650832491, 6.927238148923188454, -1.082531754730543083 ) ) ;
#69849 = B_SPLINE_CURVE_WITH_KNOTS ( 'NONE', 3,
 ( #136523, #120331, #186307, #109149, #37943, #92850, #104016 ),
 .UNSPECIFIED., .F., .F.,
 ( 4, 3, 4 ),
 ( 0.001837494195021906022, 0.002395020826491690066, 0.002588355962777570424 ),
 .UNSPECIFIED. ) ;
#69850 = CARTESIAN_POINT ( 'NONE',  ( -6.995644074527074707, 11.10540915368285475, 0.000000000000000000 ) ) ;
#69851 = CARTESIAN_POINT ( 'NONE',  ( 4.394251184604957672, 8.140727125432173139, -0.7216878364870357165 ) ) ;
#69852 = CARTESIAN_POINT ( 'NONE',  ( 1.565077508395201988, -1.076315722900993643, 1.704939445326451475 ) ) ;
#69854 = CARTESIAN_POINT ( 'NONE',  ( 1.200133799977639137, 0.8395725688425963451, -1.884152621438263342 ) ) ;
#69853 = CARTESIAN_POINT ( 'NONE',  ( 8.925345196497941558, 9.307324238869423283, 1.040834085586084257E-14 ) ) ;
#69855 =( NAMED_UNIT ( * ) PLANE_ANGLE_UNIT ( ) SI_UNIT ( $, .RADIAN. ) );
#69856 = CARTESIAN_POINT ( 'NONE',  ( 5.031484404002878996, 7.923796667095108326, 1.082531754730548412 ) ) ;
#69857 = CARTESIAN_POINT ( 'NONE',  ( 6.585563763084506306, -0.7354652392584435372, 1.576171286539735705 ) ) ;
#69858 = CARTESIAN_POINT ( 'NONE',  ( -3.940069096733920251, 8.986657997193951530, 0.7749999999999996891 ) ) ;
#69859 = CARTESIAN_POINT ( 'NONE',  ( 0.6823417656249882723, 2.926041667008084879, -1.181850606188754593 ) ) ;
#69860 = CARTESIAN_POINT ( 'NONE',  ( 2.600565598370237819, 1.424089007750706237, -1.050482986540713926 ) ) ;
#69861 = CARTESIAN_POINT ( 'NONE',  ( 1.705704151892040832, 1.882474636155605507, 0.7231385473688843879 ) ) ;
#69862 = CARTESIAN_POINT ( 'NONE',  ( 6.409682876116948869, -0.8291888958818021127, -1.530247525868874581 ) ) ;
#69863 = CARTESIAN_POINT ( 'NONE',  ( 5.530919501969752794, -2.073650524585127997, 0.9775372349926645388 ) ) ;
#69864 = CARTESIAN_POINT ( 'NONE',  ( 3.204851553285171573, -0.3583046703147829137, 1.805758307424263354 ) ) ;
#69865 = EDGE_CURVE ( 'NONE', #145094, #159043, #76095, .T. ) ;
#69866 = CARTESIAN_POINT ( 'NONE',  ( 7.425061681778431399, 11.81432239538354345, 0.7998128361456462443 ) ) ;
#69867 = CARTESIAN_POINT ( 'NONE',  ( 3.961776442328440506, 1.811803316853294765, -0.2231971713724384965 ) ) ;
#69868 = CARTESIAN_POINT ( 'NONE',  ( 5.274064633610318076, 1.777012466945230962, -0.9530095070046653571 ) ) ;
#69869 = CARTESIAN_POINT ( 'NONE',  ( -9.691380875670077444, 10.20103253123691189, 0.7998128361456462443 ) ) ;
#69871 = CARTESIAN_POINT ( 'NONE',  ( -5.610041701004606196, 9.767075427805856691, -0.7998128361456362523 ) ) ;
#69870 = CARTESIAN_POINT ( 'NONE',  ( 3.924925821460770514, 2.147445456087885063, 0.7125370657276063335 ) ) ;
#69872 = CARTESIAN_POINT ( 'NONE',  ( 6.299853487814777608, -0.7131585336714525436, 1.981663801677714831 ) ) ;
#69873 = CARTESIAN_POINT ( 'NONE',  ( -15.75000000000000000, 10.19999999999999929, -3.200000000000001510 ) ) ;
#69874 = CARTESIAN_POINT ( 'NONE',  ( 4.070807014193541740, 1.466255041752505539, -1.461937513464212079 ) ) ;
#69875 = CARTESIAN_POINT ( 'NONE',  ( 8.367353357928214663, 12.91366268422496688, 1.040834085586084257E-14 ) ) ;
#69876 = CARTESIAN_POINT ( 'NONE',  ( -4.156403723172807449E-14, 1.859375000341410678, -1.570758158831802254 ) ) ;
#69877 = PRODUCT_CONTEXT ( 'NONE', #156970, 'mechanical' ) ;
#69879 = CARTESIAN_POINT ( 'NONE',  ( 2.455585946167909928, 0.5135756288857267204, -1.856723504524477875 ) ) ;
#69878 = CARTESIAN_POINT ( 'NONE',  ( -8.292783513053063160, 12.82666453187061073, 0.7998128361456481317 ) ) ;
#69880 = CARTESIAN_POINT ( 'NONE',  ( -3.285556943749999625, -0.1103036037021430799, -0.06039377925050889995 ) ) ;
#69881 = CARTESIAN_POINT ( 'NONE',  ( 6.684429667774410611, 1.136775344189003611, -1.608021923639752604 ) ) ;
#69882 = CARTESIAN_POINT ( 'NONE',  ( 3.865483193227626124, 7.523831135491951372, -0.7216878364870338292 ) ) ;
#69883 = CARTESIAN_POINT ( 'NONE',  ( 5.844719547729445353, 6.005894922780862899, -0.3676955087418033452 ) ) ;
#69884 = CARTESIAN_POINT ( 'NONE',  ( -3.195971524519394702, 4.751719416737803847, -1.599625672291262513 ) ) ;
#69885 = CARTESIAN_POINT ( 'NONE',  ( 0.1413017363236251933, 2.128265657893123386, 0.6366465052881072895 ) ) ;
#69886 = CARTESIAN_POINT ( 'NONE',  ( 3.294068349240862226, -0.8549715976811816942, 1.924793576080959578 ) ) ;
#69887 = CARTESIAN_POINT ( 'NONE',  ( -5.749539660647037032, 8.865490816466966351, 1.199719254218454489 ) ) ;
#69888 = CARTESIAN_POINT ( 'NONE',  ( 6.425674737872927089, 9.584038729905381970, -1.199719254218440723 ) ) ;
#69889 = CARTESIAN_POINT ( 'NONE',  ( 0.2735837943700462627, -1.826300444241350851, 0.3570272679806109073 ) ) ;
#69890 = CARTESIAN_POINT ( 'NONE',  ( 6.287230548435207567, 8.358188277972981695, -1.599625672291262513 ) ) ;
#69891 = ADVANCED_FACE ( 'NONE', ( #96624, #127054 ), #178931, .T. ) ;
#69892 = CARTESIAN_POINT ( 'NONE',  ( 5.359550796103802028, 5.147230771742885125, -0.7998128361456231517 ) ) ;
#69893 = CARTESIAN_POINT ( 'NONE',  ( -6.672020991700860826, 7.917017590806697314, 1.082531754730549078 ) ) ;
#69894 = CARTESIAN_POINT ( 'NONE',  ( -7.619319141200077361, 9.912291636198670375, 1.443375672974090751 ) ) ;
#69895 = AXIS2_PLACEMENT_3D ( 'NONE', #59516, #175423, #27008 ) ;
#69896 = CARTESIAN_POINT ( 'NONE',  ( 1.600013431492643745, 1.466117565985028515, 1.532352819790145482 ) ) ;
#69897 = CARTESIAN_POINT ( 'NONE',  ( -6.749980374757255319, 8.968339418673846097, 1.599625672291269396 ) ) ;
#69899 = CARTESIAN_POINT ( 'NONE',  ( 4.228923158279327410, -1.829750178516520442, -0.7082015076659909925 ) ) ;
#69898 = CARTESIAN_POINT ( 'NONE',  ( -0.6125000000000226930, 0.2083333333333242665, -1.060881119635965764 ) ) ;
#69900 = CARTESIAN_POINT ( 'NONE',  ( 3.625982885822197410, -1.285997354380935098, -1.737435825693343094 ) ) ;
#69901 = CARTESIAN_POINT ( 'NONE',  ( 1.839159199666509759, 0.7036077657225292548, -1.701706503975081830 ) ) ;
#69902 = VECTOR ( 'NONE', #11115, 1000.000000000000000 ) ;
#69904 = CARTESIAN_POINT ( 'NONE',  ( -4.409912583257236562, 7.141888050452717351, -1.077592642408040424 ) ) ;
#69903 = CARTESIAN_POINT ( 'NONE',  ( -4.604929450496978660, 5.401447776115099408, -1.199719254218453823 ) ) ;
#69905 = CARTESIAN_POINT ( 'NONE',  ( 5.173663570605946838, -0.9624332111635640619, 1.449765197900940938 ) ) ;
#69906 = CARTESIAN_POINT ( 'NONE',  ( 1.000000047849771034, 14.00000000000001066, -11.64874984998672325 ) ) ;
#69907 = CARTESIAN_POINT ( 'NONE',  ( 5.124618876285529367, 7.962177208099690873, -1.082531754730549078 ) ) ;
#69908 = CARTESIAN_POINT ( 'NONE',  ( -11.14389002924298566, 7.220603907090449525, 3.549113525960188031 ) ) ;
#69909 = CARTESIAN_POINT ( 'NONE',  ( 2.131903390035182255, -1.411712784473453830, -1.637176306262012826 ) ) ;
#69910 = CARTESIAN_POINT ( 'NONE',  ( 3.251327214347735861, -1.985796489957316391, -0.3474142817363470304 ) ) ;
#69911 = CARTESIAN_POINT ( 'NONE',  ( -8.459924664802993988, 12.81373650900478189, 1.040834085586084257E-14 ) ) ;
#69912 = CARTESIAN_POINT ( 'NONE',  ( 1.006953172832128152, 1.636353683469338183, -1.412668763314451903 ) ) ;
#69913 = CARTESIAN_POINT ( 'NONE',  ( 3.485194120740982449, 1.782821823783652837, -0.8418218905394663221 ) ) ;
#69914 = CARTESIAN_POINT ( 'NONE',  ( 6.509000000000010111, 6.037005099786168394, 2.594901386363585694 ) ) ;
#69915 = CARTESIAN_POINT ( 'NONE',  ( 2.876435298317912004, -0.1456031558026495976, -1.936675272211895837 ) ) ;
#69919 = ORIENTED_EDGE ( 'NONE', *, *, #177065, .T. ) ;
#69918 = ADVANCED_FACE ( 'NONE', ( #148555 ), #132332, .F. ) ;
#69917 = CARTESIAN_POINT ( 'NONE',  ( -5.167065940583949413, 5.200867483535597913, 0.000000000000000000 ) ) ;
#69916 = CARTESIAN_POINT ( 'NONE',  ( 6.533470333208203584, -0.1312131129157616261, 1.882018712217728318 ) ) ;
#69920 = CARTESIAN_POINT ( 'NONE',  ( -3.648552735408985725, 7.270745601370182776, -0.7216878364870458196 ) ) ;
#69921 = CARTESIAN_POINT ( 'NONE',  ( 5.737035277238070385, 6.722237907313067140, -1.199719254218452047 ) ) ;
#69922 = CARTESIAN_POINT ( 'NONE',  ( -4.950662367645459305, 5.804802846121667415, -1.199719254218453823 ) ) ;
#69923 = CARTESIAN_POINT ( 'NONE',  ( -5.447343857640614573, 9.577261277214532242, -0.7998128361456362523 ) ) ;
#69924 = CARTESIAN_POINT ( 'NONE',  ( -10.11401940567025548, 10.90203684947788076, 1.040834085586084257E-14 ) ) ;
#69925 = EDGE_CURVE ( 'NONE', #7438, #107724, #83750, .T. ) ;
#69926 = CARTESIAN_POINT ( 'NONE',  ( 6.598638948628339662, -0.6063221841578874116, -2.226463007350306444 ) ) ;
#69927 = CARTESIAN_POINT ( 'NONE',  ( -1.499999999999964029, 8.500000000000000000, 9.886859966642596476 ) ) ;
#69928 = CARTESIAN_POINT ( 'NONE',  ( 4.627759936859944467, 1.903863570041373077, -0.4726564843360381851 ) ) ;
#69929 = CARTESIAN_POINT ( 'NONE',  ( 8.015895134177609904, 10.37496362800581018, 1.599625672291281386 ) ) ;
#69930 = CARTESIAN_POINT ( 'NONE',  ( 2.127577483945505055, 0.4445034925110411539, 1.966644524931899563 ) ) ;
#69931 = VERTEX_POINT ( 'NONE', #1195 ) ;
#69932 = CARTESIAN_POINT ( 'NONE',  ( 3.239577248433673784, 0.5100137816880914166, -2.054909399002705861 ) ) ;
#69933 = CARTESIAN_POINT ( 'NONE',  ( 1.499999999999989120, 2.035416667349480679, 0.8660254037844524744 ) ) ;
#69936 = ORIENTED_EDGE ( 'NONE', *, *, #142608, .T. ) ;
#69935 = CARTESIAN_POINT ( 'NONE',  ( -6.728924311084075960, 6.744833205886536120, 1.040834085586084257E-14 ) ) ;
#69934 = CARTESIAN_POINT ( 'NONE',  ( -10.43625799253330122, 3.019799309333212722, 6.025376361321555407 ) ) ;
#69937 = CARTESIAN_POINT ( 'NONE',  ( 3.644333108393753573, -1.504320797718930791, 1.061230752167609204 ) ) ;
#69938 = ORIENTED_EDGE ( 'NONE', *, *, #124980, .T. ) ;
#69939 = CARTESIAN_POINT ( 'NONE',  ( -7.323375529675950624, 11.69568855126397011, -0.7998128361456291469 ) ) ;
#69940 = CARTESIAN_POINT ( 'NONE',  ( 3.639029512587122372, 2.014767915268770082, 0.6618469929612482705 ) ) ;
#69941 = DIRECTION ( 'NONE',  ( -1.224646799147353207E-16, 1.000000000000000000, -1.301042606982605321E-17 ) ) ;
#69942 = CARTESIAN_POINT ( 'NONE',  ( 6.262976894508937242, 9.394224579314053969, -1.199719254218440723 ) ) ;
#69943 = CARTESIAN_POINT ( 'NONE',  ( 5.184866321732980232, -0.2479502356789231865, -2.045719655484798949 ) ) ;
#69945 = CARTESIAN_POINT ( 'NONE',  ( 2.155570461979210428, 0.7887370375637430264, 1.663910549085621415 ) ) ;
#69944 = CARTESIAN_POINT ( 'NONE',  ( -6.470265622219711688, 8.571729197388226140, -1.599625672291263179 ) ) ;
#69946 = CARTESIAN_POINT ( 'NONE',  ( 9.097684769969825780, 10.57271930550834860, -1.199719254218446718 ) ) ;
#69947 = CARTESIAN_POINT ( 'NONE',  ( 1.364683531249988535, 5.655208333674751842, -0.7879004041258300672 ) ) ;
#69948 = CARTESIAN_POINT ( 'NONE',  ( -6.056815632531343141, 6.015240258500212711, 0.3115616189311651296 ) ) ;
#69949 = PRESENTATION_STYLE_ASSIGNMENT (( #3877 ) ) ;
#69950 = CARTESIAN_POINT ( 'NONE',  ( 1.737499999999999378, -1.472916665710751527, -3.009438278150925683 ) ) ;
#69951 = CARTESIAN_POINT ( 'NONE',  ( 1.805583701156989518, 1.836052299496168771, 1.224139149458243425 ) ) ;
#69952 = CARTESIAN_POINT ( 'NONE',  ( 3.673342012549928981, 0.05998355446043589223, -2.261782774625902714 ) ) ;
#69953 = CARTESIAN_POINT ( 'NONE',  ( -6.534666852106790103, 10.56760239419251590, 0.7216878364870458196 ) ) ;
#69954 = CARTESIAN_POINT ( 'NONE',  ( 4.289189881116685754, -0.006549295265783834294, -1.811767228872669389 ) ) ;
#69955 = CARTESIAN_POINT ( 'NONE',  ( 4.628101268237789334, 1.911029739866540345, 0.1345505791198585988 ) ) ;
#69956 = CARTESIAN_POINT ( 'NONE',  ( -1.364683531250010295, 3.842708333674751398, 0.7879004041258379498 ) ) ;
#69957 = CARTESIAN_POINT ( 'NONE',  ( 3.520352277729906998, 1.251605784994310300, -1.523194303571529185 ) ) ;
#69958 = CARTESIAN_POINT ( 'NONE',  ( 4.662891624058607576, -1.671085903211678270, -0.8408918736509605196 ) ) ;
#69959 = CARTESIAN_POINT ( 'NONE',  ( 3.774305527563319274, 1.280948863717756847, 1.919355958833997233 ) ) ;
#69960 = CARTESIAN_POINT ( 'NONE',  ( 4.580409787399508659, 1.145788356511275863, -1.466404039444089591 ) ) ;
#69961 = CARTESIAN_POINT ( 'NONE',  ( 0.07933194154487849259, -9.900000000000005684, 9.499668754385625746 ) ) ;
#69962 = AXIS2_PLACEMENT_3D ( 'NONE', #29753, #30829, #11341 ) ;
#69963 = AXIS2_PLACEMENT_3D ( 'NONE', #149727, #50094, #162787 ) ;
#69964 = CARTESIAN_POINT ( 'NONE',  ( -0.2351498743046881446, -0.1506043639611966134, -1.983733596389973597 ) ) ;
#69966 = CARTESIAN_POINT ( 'NONE',  ( 2.016375119164611984, -0.9936656701176631579, -1.856918979450744578 ) ) ;
#69965 = CARTESIAN_POINT ( 'NONE',  ( -3.836594282542926226, 5.499112634431936542, 1.443375672974064550 ) ) ;
#69967 = CARTESIAN_POINT ( 'NONE',  ( 8.387690588348714726, 12.93738945304888333, 1.040834085586084257E-14 ) ) ;
#69969 = CARTESIAN_POINT ( 'NONE',  ( -10.50487009249003378, 11.15010328419353947, 0.7998128361456462443 ) ) ;
#69968 = CARTESIAN_POINT ( 'NONE',  ( -1.364683531250010295, 5.301041667008085767, -0.7879004041258300672 ) ) ;
#69970 = CARTESIAN_POINT ( 'NONE',  ( -4.955972296452688219, 4.884889769079732602, -0.3912739104816483349 ) ) ;
#69971 = CARTESIAN_POINT ( 'NONE',  ( 0.3518269803744868418, -1.431374087835567632, -1.425298768015555551 ) ) ;
#69972 = CARTESIAN_POINT ( 'NONE',  ( 1.364683531249986537, 0.9052083336747533959, -0.7879004041258239610 ) ) ;
#69973 = CARTESIAN_POINT ( 'NONE',  ( -2.643476764984671767, 6.027880625883323518, 1.040834085586084257E-14 ) ) ;
#69974 = CARTESIAN_POINT ( 'NONE',  ( 4.871457266011829823, 4.577788319968905562, -0.7998128361456221525 ) ) ;
#69975 = EDGE_LOOP ( 'NONE', ( #71381, #83342, #198970, #92651 ) ) ;
#69976 = CARTESIAN_POINT ( 'NONE',  ( 2.671339989782473001, 0.1089736159370843782, -2.158987078831893669 ) ) ;
#69977 = CARTESIAN_POINT ( 'NONE',  ( 6.610000000000009202, 6.036727194997777879, 2.594899704271665275 ) ) ;
#69980 = CARTESIAN_POINT ( 'NONE',  ( 1.419999999999820739, 7.240846818246208905, -4.154462424328212222 ) ) ;
#69979 = CARTESIAN_POINT ( 'NONE',  ( -5.946383829929366094, 4.757679660040812664, -2.499999999999995559 ) ) ;
#69978 = CARTESIAN_POINT ( 'NONE',  ( 6.384963997392946844, 6.413822516572072807, 0.7998128361456352531 ) ) ;
#69981 = DIRECTION ( 'NONE',  ( -1.000000000000000000, 0.000000000000000000, 0.000000000000000000 ) ) ;
#69982 = CARTESIAN_POINT ( 'NONE',  ( 6.227749967195368441, 0.7672974224810541477, -1.865044430435198741 ) ) ;
#69983 = CARTESIAN_POINT ( 'NONE',  ( -9.341204650135658483, 10.00041963468749984, 1.040834085586084257E-14 ) ) ;
#69984 = CARTESIAN_POINT ( 'NONE',  ( 6.532766951017621615, -1.867387138063754337, 0.9404246163645290091 ) ) ;
#69985 = CARTESIAN_POINT ( 'NONE',  ( -0.4630894006623515469, -6.442483420144702322, -11.24798772015292769 ) ) ;
#69987 = CARTESIAN_POINT ( 'NONE',  ( -1.402160292154681736E-14, 11.42187500034139980, 1.575800808251682339 ) ) ;
#69986 = CARTESIAN_POINT ( 'NONE',  ( 1.516897200560879178, 1.518302048914378588, -1.677564506150258206 ) ) ;
#69988 = CARTESIAN_POINT ( 'NONE',  ( -8.941766003412679353, 10.39081407785832845, -1.199719254218446718 ) ) ;
#69989 = CARTESIAN_POINT ( 'NONE',  ( -5.436456408955534947, 6.405249234278626247, 1.082531754730546636 ) ) ;
#69990 = CARTESIAN_POINT ( 'NONE',  ( -1.364683531250000748, 1.821875000341421913, 0.000000000000000000 ) ) ;
#69991 = CARTESIAN_POINT ( 'NONE',  ( 0.4019237886466816012, 9.426335450315370679, -1.499999999999998668 ) ) ;
#69992 = AXIS2_PLACEMENT_3D ( 'NONE', #149562, #200417, #1147 ) ;
#69993 = CARTESIAN_POINT ( 'NONE',  ( 0.7500000000000006661, 9.083333333333332149, 1.299038105676657340 ) ) ;
#69994 = CARTESIAN_POINT ( 'NONE',  ( 4.564925566169513615, -1.542601567919573258, -0.7719000744037025630 ) ) ;
#69995 = CARTESIAN_POINT ( 'NONE',  ( 3.854260808034858155, 7.718664386007802136, -0.7998128361456362523 ) ) ;
#69996 = CARTESIAN_POINT ( 'NONE',  ( 2.582953972192280734, 1.619985402465830671, -0.7128798769604760555 ) ) ;
#69997 = CARTESIAN_POINT ( 'NONE',  ( 4.858537417550492954, 0.8407558337346630051, 2.040536144146696707 ) ) ;
#69998 = VERTEX_POINT ( 'NONE', #202595 ) ;
#69999 = CARTESIAN_POINT ( 'NONE',  ( 4.570572472720978219, 0.7768735290680817140, 1.864611197846306911 ) ) ;
#70000 = CARTESIAN_POINT ( 'NONE',  ( -5.966470118465691641, 9.118576350588734059, -1.199719254218452047 ) ) ;
#70002 = CARTESIAN_POINT ( 'NONE',  ( 4.587517648402447357, -0.5350702435001615243, 1.944077497823355261 ) ) ;
#70001 = CARTESIAN_POINT ( 'NONE',  ( 4.934296419935967570, -1.134874685878878520, -1.791058398909770588 ) ) ;
#70004 = ORIENTED_EDGE ( 'NONE', *, *, #184537, .F. ) ;
#70003 = CARTESIAN_POINT ( 'NONE',  ( 4.306777863985831623, -0.4033372078124509708, -1.765930869088320865 ) ) ;
#70005 = ORIENTED_EDGE ( 'NONE', *, *, #194044, .F. ) ;
#70006 = CARTESIAN_POINT ( 'NONE',  ( 1.375632740723360836, 1.111493989511678881, 1.504490780774490499 ) ) ;
#70007 = CARTESIAN_POINT ( 'NONE',  ( 5.692136587293062711, 5.855332880448197663, -2.499999999999994671 ) ) ;
#70008 = CARTESIAN_POINT ( 'NONE',  ( 1.459083999156213451, -1.613880964290700160, 1.025699646091532857 ) ) ;
#70009 = CARTESIAN_POINT ( 'NONE',  ( -5.861933645127444414, 6.964938855919925231, 1.092222976013698332 ) ) ;
#70010 = CARTESIAN_POINT ( 'NONE',  ( -10.80887392267048241, 4.296486016114100082, -4.677321330754881323 ) ) ;
#70011 = CARTESIAN_POINT ( 'NONE',  ( 0.4355862708379926174, -6.583980363595115293, 9.606148981167594414 ) ) ;
#70012 = CARTESIAN_POINT ( 'NONE',  ( 1.364683531249988535, 2.967708333674755394, -0.7879004041258239610 ) ) ;
#70013 = FACE_OUTER_BOUND ( 'NONE', #207670, .T. ) ;
#70014 = CARTESIAN_POINT ( 'NONE',  ( 4.719646871332936477, 8.520355426614829142, -0.7216878364870357165 ) ) ;
#70015 = CARTESIAN_POINT ( 'NONE',  ( 2.242563829109287088, -1.923402688547710904, -0.3857071251459272543 ) ) ;
#70016 = DIRECTION ( 'NONE',  ( -0.6507913734559640506, -0.7592566023653004592, 0.000000000000000000 ) ) ;
#70017 = CARTESIAN_POINT ( 'NONE',  ( -6.459533842268148973, 6.500820668926428958, 0.000000000000000000 ) ) ;
#70018 = CARTESIAN_POINT ( 'NONE',  ( 4.025719079702368752, -0.3592959752154977204, 2.089770972018199835 ) ) ;
#70020 = CARTESIAN_POINT ( 'NONE',  ( -11.14389002924298566, 7.220603907090449525, 3.549113525960188031 ) ) ;
#70019 = CARTESIAN_POINT ( 'NONE',  ( 9.908311333488716954, 10.45411806535867782, 0.7998128361456462443 ) ) ;
#70021 = CARTESIAN_POINT ( 'NONE',  ( 5.096930449404251107, 1.640577245564038389, -1.092763768510503608 ) ) ;
#70022 = CARTESIAN_POINT ( 'NONE',  ( 0.6823417656249899377, 1.342708333674752508, 1.181850606188755259 ) ) ;
#70023 = CARTESIAN_POINT ( 'NONE',  ( 0.9494776711209992337, -1.818202237497710483, 0.8646994008154506028 ) ) ;
#70024 = ORIENTED_EDGE ( 'NONE', *, *, #121129, .F. ) ;
#70025 = CARTESIAN_POINT ( 'NONE',  ( 0.9841680404778062607, -2.117403155482136423, 0.004310642112759220310 ) ) ;
#70026 = B_SPLINE_CURVE_WITH_KNOTS ( 'NONE', 3,
 ( #178231, #194465, #111156, #95929, #98056, #177155 ),
 .UNSPECIFIED., .F., .F.,
 ( 4, 2, 4 ),
 ( 0.000000000000000000, 0.0003767643964918268649, 0.0007535287929836534046 ),
 .UNSPECIFIED. ) ;
#70027 = CARTESIAN_POINT ( 'NONE',  ( 11.75000478245984503, 6.934949167590856334, -2.448457861207594455 ) ) ;
#70028 = CARTESIAN_POINT ( 'NONE',  ( 2.682155120989743402, -1.190029146579720587, -1.693995171316540427 ) ) ;
#70029 = CARTESIAN_POINT ( 'NONE',  ( 3.217027588192558074, 6.975225629525113824, -1.734723475976807094E-15 ) ) ;
#70030 = CARTESIAN_POINT ( 'NONE',  ( 6.398522151006641678, 6.429640362454684954, 0.000000000000000000 ) ) ;
#70031 = ORIENTED_EDGE ( 'NONE', *, *, #10962, .T. ) ;
#70033 = CARTESIAN_POINT ( 'NONE',  ( 6.356075086708249167, 6.309842444114747373, -0.7998128361456281477 ) ) ;
#70032 = CARTESIAN_POINT ( 'NONE',  ( 5.015614203636001633, -1.117866415629315435, -1.766478577331761723 ) ) ;
#70036 = VERTEX_POINT ( 'NONE', #34776 ) ;
#70035 = CARTESIAN_POINT ( 'NONE',  ( 1.453448513857479973, -1.311971142947904401, -1.249319819763055950 ) ) ;
#70034 = CARTESIAN_POINT ( 'NONE',  ( 2.660947563312371589, -1.587261545009664765, -0.9017329732442300738 ) ) ;
#70037 = CARTESIAN_POINT ( 'NONE',  ( 0.3275200278799236253, 3.116672424413495790, -0.4674645318178084485 ) ) ;
#70038 = CARTESIAN_POINT ( 'NONE',  ( 3.850147086611925396, 5.981400113484194314, 1.344841084984424562 ) ) ;
#70039 = CARTESIAN_POINT ( 'NONE',  ( 9.392804560491793353, 11.17150285567701928, -6.982157407287515660 ) ) ;
#70040 = CARTESIAN_POINT ( 'NONE',  ( 4.858537417550492954, 0.8407558337346630051, 2.040536144146696707 ) ) ;
#70042 =( BOUNDED_SURFACE ( )  B_SPLINE_SURFACE ( 3, 2, ( 
 ( #162265, #214153, #196883 ),
 ( #65779, #113578, #46385 ),
 ( #63686, #181683, #197939 ),
 ( #116759, #166522, #99395 ) ),
 .UNSPECIFIED., .F., .F., .T. ) 
 B_SPLINE_SURFACE_WITH_KNOTS ( ( 4, 4 ),
 ( 3, 3 ),
 ( -6.071532165918824830E-18, 0.002003486994853880768 ),
 ( 0.000000000000000000, 1.000000000000000000 ),
 .UNSPECIFIED. ) 
 GEOMETRIC_REPRESENTATION_ITEM ( )  RATIONAL_B_SPLINE_SURFACE ( (
 ( 1.000000000000000000, 0.7779734834199515392, 1.000000000000000000),
 ( 1.000000000000000000, 0.7856061901475719367, 1.000000000000000000),
 ( 1.000000000000000000, 0.7951961705782245593, 1.000000000000000000),
 ( 1.000000000000000000, 0.8104931255419017821, 1.000000000000000000) ) ) 
 REPRESENTATION_ITEM ( '' )  SURFACE ( )  );
#70041 = CARTESIAN_POINT ( 'NONE',  ( 0.6823417656249969321, 9.588541667008065872, -1.181850606188757036 ) ) ;
#70043 = ORIENTED_EDGE ( 'NONE', *, *, #166950, .T. ) ;
#70044 = CARTESIAN_POINT ( 'NONE',  ( 4.318947422894989785, 1.476084237994702786, -1.215703867470045774 ) ) ;
#70045 = CARTESIAN_POINT ( 'NONE',  ( -4.620631424159025613, 4.285158171140619032, -0.7998128361456221525 ) ) ;
#70046 = CIRCLE ( 'NONE', #83834, 0.08000000000000050127 ) ;
#70047 = CARTESIAN_POINT ( 'NONE',  ( 8.015895134177609904, 10.37496362800581018, 1.599625672291281386 ) ) ;
#70048 = CARTESIAN_POINT ( 'NONE',  ( 6.320769956279724155, -1.466918727022303193, 1.461273828345016845 ) ) ;
#70049 = CARTESIAN_POINT ( 'NONE',  ( -2.788906526875773208E-15, 10.21875000068279782, -1.499999999999998446 ) ) ;
#70050 = CARTESIAN_POINT ( 'NONE',  ( 5.970311429539967740, -2.080533979117826782, -0.6889730390344513955 ) ) ;
#70051 = CARTESIAN_POINT ( 'NONE',  ( 5.763319317650291040, 7.363698819737331647, -1.304181885133362195 ) ) ;
#70052 = CARTESIAN_POINT ( 'NONE',  ( -1.539565250226320312E-10, 15.46908218388475831, -12.00000000000000533 ) ) ;
#70053 = ORIENTED_EDGE ( 'NONE', *, *, #7244, .T. ) ;
#70054 = ORIENTED_EDGE ( 'NONE', *, *, #56757, .T. ) ;
#70055 = EDGE_CURVE ( 'NONE', #116248, #54188, #132726, .T. ) ;
#70056 = CARTESIAN_POINT ( 'NONE',  ( -11.92619526913699879, 12.69999999999999929, -1.328859060402686199 ) ) ;
#70057 = CARTESIAN_POINT ( 'NONE',  ( 3.989402248074361612, 1.353031944225962624, 1.291829963354161892 ) ) ;
#70058 = CARTESIAN_POINT ( 'NONE',  ( 0.000000000000000000, 3.481540744127368914, 0.000000000000000000 ) ) ;
#70059 = DIRECTION ( 'NONE',  ( -9.436895709313856232E-16, 0.8656921114426506803, 0.5005768354468324022 ) ) ;
#70060 = CARTESIAN_POINT ( 'NONE',  ( -6.371969008742801144, 10.37778824360119145, 0.7216878364870458196 ) ) ;
#70061 = CARTESIAN_POINT ( 'NONE',  ( 3.088225128862704949, 6.824956093640315302, 0.7998128361456281477 ) ) ;
#70062 = CARTESIAN_POINT ( 'NONE',  ( 5.880485940025228508, 7.883652901494672349, 1.599625672291267398 ) ) ;
#70063 = CARTESIAN_POINT ( 'NONE',  ( 6.842638490404138629, -2.029097751484234546, -0.4099019697717393163 ) ) ;
#70064 = CARTESIAN_POINT ( 'NONE',  ( 0.8785300617164049086, -0.4926655378557908138, -1.955167820405806056 ) ) ;
#70065 = CARTESIAN_POINT ( 'NONE',  ( -9.297140650669053485, 11.86975006391249643, 1.599625672291281386 ) ) ;
#70066 = CARTESIAN_POINT ( 'NONE',  ( 6.690022453700429139, 6.769724048930809701, 0.7998128361456331437 ) ) ;
#70067 = DIRECTION ( 'NONE',  ( 1.000000000000000000, -0.000000000000000000, -0.000000000000000000 ) ) ;
#70068 = CARTESIAN_POINT ( 'NONE',  ( 1.922082643403967506, 1.260107670313360240, -1.792737600334909365 ) ) ;
#70069 = CARTESIAN_POINT ( 'NONE',  ( 3.834746474454188013E-15, 13.09375000068279959, 1.500000000000001554 ) ) ;
#70070 = CARTESIAN_POINT ( 'NONE',  ( -2.761056838677368397, 6.372983411765559048, 0.7998128361456341429 ) ) ;
#70071 = CARTESIAN_POINT ( 'NONE',  ( 4.963693636378940788, 5.923969009597785274, -1.082531754730548412 ) ) ;
#70072 = CARTESIAN_POINT ( 'NONE',  ( 8.211434591371064684, 12.73175745657494851, -0.7998128361456352531 ) ) ;
#70073 = EDGE_CURVE ( 'NONE', #24729, #70347, #96843, .T. ) ;
#70074 = CARTESIAN_POINT ( 'NONE',  ( 4.878236342818665250, 4.585697242910212523, 1.040834085586084257E-14 ) ) ;
#70075 = CARTESIAN_POINT ( 'NONE',  ( 6.373741612200160667, 9.489763409991955001, 1.082531754730549078 ) ) ;
#70076 = ORIENTED_EDGE ( 'NONE', *, *, #148167, .F. ) ;
#70078 = CARTESIAN_POINT ( 'NONE',  ( 1.154940503102233729, 0.3948395466160973255, 1.973830874585213113 ) ) ;
#70077 = CARTESIAN_POINT ( 'NONE',  ( 3.597050949361340511, -0.5310884314010614338, 1.763007376093472800 ) ) ;
#70079 = CARTESIAN_POINT ( 'NONE',  ( 2.390373184264094952, -0.001117755346285650552, 2.298542322714514530 ) ) ;
#70081 = CARTESIAN_POINT ( 'NONE',  ( 1.094327318609791710, 1.832149372150039479, 0.3252389950085340375 ) ) ;
#70080 = CARTESIAN_POINT ( 'NONE',  ( 5.178851490740207453, 5.144340948726102702, 0.7216878364870317197 ) ) ;
#70082 = CARTESIAN_POINT ( 'NONE',  ( 1.001543065824772753E-15, -0.2624999999999988454, 4.012584370867899430 ) ) ;
#70083 = CARTESIAN_POINT ( 'NONE',  ( -3.405069135326500351, 7.124331091189553433, 1.040834085586084257E-14 ) ) ;
#70084 = CARTESIAN_POINT ( 'NONE',  ( 3.990413957267644474, -1.096855775730350757, 1.566394476586838724 ) ) ;
#70085 = CARTESIAN_POINT ( 'NONE',  ( -8.676328237741483207, 12.20980114641871062, -1.199719254218446718 ) ) ;
#70086 = CARTESIAN_POINT ( 'NONE',  ( 6.400493444083267036, 6.807005473012165631, 0.5116258143813920967 ) ) ;
#70087 = CARTESIAN_POINT ( 'NONE',  ( -4.442231607132987925, 5.211633625523774960, -1.199719254218453823 ) ) ;
#70089 = CARTESIAN_POINT ( 'NONE',  ( 2.729206520949432946, -1.746158693253213379, 0.6715030345267187784 ) ) ;
#70088 = CARTESIAN_POINT ( 'NONE',  ( 3.280887763456251882, 1.889169395226503401, -0.8960188238960642426 ) ) ;
#70090 = CARTESIAN_POINT ( 'NONE',  ( 7.293923454472069245, 11.45340176361870199, 0.7216878364870438212 ) ) ;
#70091 = CARTESIAN_POINT ( 'NONE',  ( -0.6823417656249969321, 5.030208333674755394, -1.181850606188749264 ) ) ;
#70092 = CARTESIAN_POINT ( 'NONE',  ( 3.456370904947672074, -1.536751586138744852, -0.8169772437159742440 ) ) ;
#70093 = CARTESIAN_POINT ( 'NONE',  ( 4.172158584703322681, 5.890604320285754980, -1.599625672291256295 ) ) ;
#70095 =( NAMED_UNIT ( * ) PLANE_ANGLE_UNIT ( ) SI_UNIT ( $, .RADIAN. ) );
#70094 = CARTESIAN_POINT ( 'NONE',  ( -1.225000000000005640, 1.387778780781445676E-14, -1.387778780781445676E-14 ) ) ;
#70096 = CARTESIAN_POINT ( 'NONE',  ( 3.545241905100663615, -1.307145164029408502, -1.125523404956897178 ) ) ;
#70097 = CARTESIAN_POINT ( 'NONE',  ( 3.509492838045696672, -2.158849082856160173, 0.3763758916049686487 ) ) ;
#70098 = CARTESIAN_POINT ( 'NONE',  ( 5.848300530743933301, 2.204158087718602221, 0.1119919437090263481 ) ) ;
#70099 =( BOUNDED_SURFACE ( )  B_SPLINE_SURFACE ( 3, 2, ( 
 ( #164131, #16773, #181422 ),
 ( #115431, #1578, #97016 ),
 ( #148933, #196623, #15715 ),
 ( #132716, #81800, #147883 ) ),
 .UNSPECIFIED., .F., .F., .T. ) 
 B_SPLINE_SURFACE_WITH_KNOTS ( ( 4, 4 ),
 ( 3, 3 ),
 ( 0.01090155471707265726, 0.01336979040894267258 ),
 ( 0.000000000000000000, 1.000000000000000000 ),
 .UNSPECIFIED. ) 
 GEOMETRIC_REPRESENTATION_ITEM ( )  RATIONAL_B_SPLINE_SURFACE ( (
 ( 1.000000000000000000, 0.6967468848055777819, 1.000000000000000000),
 ( 1.000000000000000000, 0.6961913616436821162, 1.000000000000000000),
 ( 1.000000000000000000, 0.6955505937926295124, 1.000000000000000000),
 ( 1.000000000000000000, 0.6947640035364029965, 1.000000000000000000) ) ) 
 REPRESENTATION_ITEM ( '' )  SURFACE ( )  );
#70100 = CARTESIAN_POINT ( 'NONE',  ( 3.239314478175295164, -0.1551929672521153158, -2.165549275587749456 ) ) ;
#70101 = CARTESIAN_POINT ( 'NONE',  ( 2.666400811807769777, -1.259032629953384719, 1.322343945743660543 ) ) ;
#70102 = CARTESIAN_POINT ( 'NONE',  ( -0.7500000000000006661, 9.239583334016129967, -1.299038105676657340 ) ) ;
#70104 = CARTESIAN_POINT ( 'NONE',  ( 5.014918053075636095, 0.1589874617720990202, 2.111459674661147368 ) ) ;
#70103 = B_SPLINE_CURVE_WITH_KNOTS ( 'NONE', 3,
 ( #78251, #128170, #177902, #210374 ),
 .UNSPECIFIED., .F., .F.,
 ( 4, 4 ),
 ( 0.000000000000000000, 0.0002909236271752606252 ),
 .UNSPECIFIED. ) ;
#70105 = ORIENTED_EDGE ( 'NONE', *, *, #24424, .T. ) ;
#70107 = CARTESIAN_POINT ( 'NONE',  ( -1.364683531250012516, 2.342708333674752286, 0.7879004041258379498 ) ) ;
#70106 = CARTESIAN_POINT ( 'NONE',  ( 4.599361256383265761, -0.6123007911535255365, 2.209042870082494225 ) ) ;
#70108 = CARTESIAN_POINT ( 'NONE',  ( 6.620655732516651071, 1.309889148221474509, 1.844503626996786938 ) ) ;
#70109 = CARTESIAN_POINT ( 'NONE',  ( 9.836604141914616406, 11.43479190611061647, 1.199719254218452047 ) ) ;
#70110 = CARTESIAN_POINT ( 'NONE',  ( -0.004992717928550480244, -2.057963470346049650, -0.5107951590591561786 ) ) ;
#70111 = CARTESIAN_POINT ( 'NONE',  ( -3.931501358282937009, 7.530575984731317618, 0.7216878364870317197 ) ) ;
#70112 = FACE_OUTER_BOUND ( 'NONE', #94121, .T. ) ;
#70113 = AXIS2_PLACEMENT_3D ( 'NONE', #202948, #104417, #108481 ) ;
#70114 = CARTESIAN_POINT ( 'NONE',  ( -4.229780737339226881, 7.878568593630327577, 1.040834085586084257E-14 ) ) ;
#70115 = AXIS2_PLACEMENT_3D ( 'NONE', #103555, #36405, #102483 ) ;
#70117 = CARTESIAN_POINT ( 'NONE',  ( 1.499999999999993117, 11.63541666734946745, 0.8660254037844409281 ) ) ;
#70116 = CARTESIAN_POINT ( 'NONE',  ( 5.346851039111009563, 6.199209027673978412, 1.092492203018504471 ) ) ;
#70118 = EDGE_LOOP ( 'NONE', ( #100372, #30464, #71104, #169663 ) ) ;
#70119 = CARTESIAN_POINT ( 'NONE',  ( 5.467422714486909641, -1.967887220244109558, -0.4390321945699494632 ) ) ;
#70121 = CARTESIAN_POINT ( 'NONE',  ( 4.276276908810595856, -1.056066993903046924, -1.771547272865436673 ) ) ;
#70120 = CARTESIAN_POINT ( 'NONE',  ( 4.150767584078112193, 7.994312614733129152, 0.7998128361456321445 ) ) ;
#70123 = CARTESIAN_POINT ( 'NONE',  ( -0.2411972340276282434, 2.878796387150697633, -2.389097370654146513 ) ) ;
#70122 = CARTESIAN_POINT ( 'NONE',  ( 5.885121196783658526, 9.023669275293071834, 1.199719254218452047 ) ) ;
#70124 = CARTESIAN_POINT ( 'NONE',  ( 5.528692779322568640, 9.672168352510192690, 0.7998128361456341429 ) ) ;
#70125 = CARTESIAN_POINT ( 'NONE',  ( 1.001543065824772753E-15, -1.771874999522040861, 3.793834371823811669 ) ) ;
#70126 = CARTESIAN_POINT ( 'NONE',  ( 0.000000000000000000, 3.079999999999999183, 6.250000000000000000 ) ) ;
#70127 = CARTESIAN_POINT ( 'NONE',  ( 0.8145359132093257237, 1.932373828749304856, 0.7984225692715187783 ) ) ;
#70128 = CARTESIAN_POINT ( 'NONE',  ( 4.781875055470904634, 1.674888562130649960, -1.122497055794105192 ) ) ;
#70129 = CARTESIAN_POINT ( 'NONE',  ( 3.843160323004328305, 0.6166970922517557296, -1.735048075492843456 ) ) ;
#70130 = EDGE_CURVE ( 'NONE', #62722, #205506, #202670, .T. ) ;
#70131 = CARTESIAN_POINT ( 'NONE',  ( 7.156006149914539982, 7.243095351188763686, 1.040834085586084257E-14 ) ) ;
#70132 = CARTESIAN_POINT ( 'NONE',  ( 0.4985095413094174921, 1.438046592433483761, -0.9519660005063760311 ) ) ;
#70133 = VECTOR ( 'NONE', #184778, 1000.000000000000000 ) ;
#70134 = CARTESIAN_POINT ( 'NONE',  ( -4.288456660624211381, 3.897620947016656956, 1.214306433183764966E-14 ) ) ;
#70135 = CARTESIAN_POINT ( 'NONE',  ( 0.8272591630335036639, 0.9250671760404407529, -2.104501483148725427 ) ) ;
#70136 = CARTESIAN_POINT ( 'NONE',  ( -5.052384799386910430, 9.046199365926717917, 1.214306433183764966E-14 ) ) ;
#70137 = CARTESIAN_POINT ( 'NONE',  ( 0.7028506612886147309, -0.7633063118723592000, -2.129901512202157399 ) ) ;
#70138 = CARTESIAN_POINT ( 'NONE',  ( 2.807361190694975139, 1.779531611039061767, 1.126096823879179754 ) ) ;
#70139 = CARTESIAN_POINT ( 'NONE',  ( -3.959863383643135393, 6.777535159962392086, 1.199719254218452935 ) ) ;
#70140 = CARTESIAN_POINT ( 'NONE',  ( 7.396136491454752715, 8.587579647240744407, 1.199719254218462483 ) ) ;
#70141 = CARTESIAN_POINT ( 'NONE',  ( 6.089020385868848528, 8.197219431637373432, -1.443375672974078761 ) ) ;
#70142 =( NAMED_UNIT ( * ) PLANE_ANGLE_UNIT ( ) SI_UNIT ( $, .RADIAN. ) );
#70143 = CARTESIAN_POINT ( 'NONE',  ( -5.377780486114890124, 9.425827667109372143, 0.000000000000000000 ) ) ;
#70144 = CARTESIAN_POINT ( 'NONE',  ( 7.578644679914718019, 7.944099669429731669, 0.7216878364870317197 ) ) ;
#70145 = CARTESIAN_POINT ( 'NONE',  ( 5.497327176576959573, 6.424397595302826502, 1.252573174869066941 ) ) ;
#70146 = CIRCLE ( 'NONE', #66734, 0.07999999999999969635 ) ;
#70147 = CARTESIAN_POINT ( 'NONE',  ( -4.192495815123836955, 5.914331089109674089, -1.599625672291256295 ) ) ;
#70148 = CARTESIAN_POINT ( 'NONE',  ( 5.256174644204150148, 0.8999736644031709476, -2.031094499404682008 ) ) ;
#70149 = CARTESIAN_POINT ( 'NONE',  ( 2.256057974219495499, 0.9384471748680022207, 1.980482673072603284 ) ) ;
#70150 = CARTESIAN_POINT ( 'NONE',  ( -4.577849422908604637, 8.492574760035358494, -0.7998128361456281477 ) ) ;
#70151 = CARTESIAN_POINT ( 'NONE',  ( -3.984117037569407938, 5.741498858621315371, 1.599625672291270506 ) ) ;
#70152 = CARTESIAN_POINT ( 'NONE',  ( 5.178158156489047315, -1.047961880893449882, -1.658324637040713867 ) ) ;
#70153 = CARTESIAN_POINT ( 'NONE',  ( -1.402160292154681736E-14, 1.946875000341422579, -1.575800808251660134 ) ) ;
#70154 = CARTESIAN_POINT ( 'NONE',  ( 6.890000000000025437, 2.478461836817289043, 2.104748632312344103 ) ) ;
#70156 = ORIENTED_EDGE ( 'NONE', *, *, #73625, .T. ) ;
#70155 = CARTESIAN_POINT ( 'NONE',  ( -4.107757355260591936, 7.736207981205250661, 1.040834085586084257E-14 ) ) ;
#70157 = CARTESIAN_POINT ( 'NONE',  ( 4.869442314738527067, -1.792836814666173062, -1.132239877606910472 ) ) ;
#70158 = CARTESIAN_POINT ( 'NONE',  ( -5.157951095356222204, 4.982307464195829816, 0.000000000000000000 ) ) ;
#70159 = ORIENTED_EDGE ( 'NONE', *, *, #143150, .F. ) ;
#70161 = CARTESIAN_POINT ( 'NONE',  ( 6.332923096303629151, 0.2067577541180857514, 2.151790036905242953 ) ) ;
#70160 = CARTESIAN_POINT ( 'NONE',  ( -5.804299160426242388, 6.904675454319632699, -1.082531754730549967 ) ) ;
#70162 = CARTESIAN_POINT ( 'NONE',  ( 6.226218857173709154, 8.287007971501239467, 1.599625672291281386 ) ) ;
#70163 = CARTESIAN_POINT ( 'NONE',  ( 4.862772069579198941, 0.1752732939881325724, -1.832877676746891726 ) ) ;
#70164 =( LENGTH_UNIT ( ) NAMED_UNIT ( * ) SI_UNIT ( .MILLI., .METRE. ) );
#70165 = CARTESIAN_POINT ( 'NONE',  ( -1.201851678989727383E-14, 2.884375000341418804, 1.575800808251672791 ) ) ;
#70166 = CARTESIAN_POINT ( 'NONE',  ( 0.7842107965865081631, 1.535900883440274090, -0.8186502264825399333 ) ) ;
#70167 = CARTESIAN_POINT ( 'NONE',  ( -0.9999999999999965583, 6.400000000000024336, 1.226552901175238481E-14 ) ) ;
#70168 = FACE_OUTER_BOUND ( 'NONE', #41501, .T. ) ;
#70169 = CARTESIAN_POINT ( 'NONE',  ( -1.225000000000026512, 1.750000000000015543, -1.734723475976807094E-14 ) ) ;
#70170 = CARTESIAN_POINT ( 'NONE',  ( 4.961884481312108797, 2.138711985806662330, -0.3135959325617638238 ) ) ;
#70171 = CARTESIAN_POINT ( 'NONE',  ( -2.785310492603665367, 5.336947110424484109, 1.199719254218462483 ) ) ;
#70172 = CARTESIAN_POINT ( 'NONE',  ( -7.673551755210395342, 8.054824590608001600, 1.040834085586084257E-14 ) ) ;
#70173 = CARTESIAN_POINT ( 'NONE',  ( 4.416967121957662279, 1.975198431823081302, 0.8787980929093119897 ) ) ;
#70174 = CARTESIAN_POINT ( 'NONE',  ( -1.201851678989727383E-14, 1.071875000341418138, 1.575800808251672791 ) ) ;
#70175 = CARTESIAN_POINT ( 'NONE',  ( 5.026621361268301946, 1.885657091993764745, 0.5748499752153258813 ) ) ;
#70176 = CARTESIAN_POINT ( 'NONE',  ( 4.358545522520183013, -0.6637924119957930857, 1.601953373104019418 ) ) ;
#70177 = CARTESIAN_POINT ( 'NONE',  ( 1.066276686178056377, -1.386418637449363889, 1.697306931840412370 ) ) ;
#70178 = CARTESIAN_POINT ( 'NONE',  ( 2.362750734746793757, 0.9868518204677073635, 2.086042234993300770 ) ) ;
#70179 = CARTESIAN_POINT ( 'NONE',  ( 3.427077464676528074, 0.04692547926744317088, 2.060408731095995094 ) ) ;
#70180 = CARTESIAN_POINT ( 'NONE',  ( 6.339402847020720877, 0.7390441267520877489, -1.796137868246181046 ) ) ;
#70182 = EDGE_CURVE ( 'NONE', #65240, #2249, #89167, .T. ) ;
#70181 = CARTESIAN_POINT ( 'NONE',  ( -7.822691444960716112, 8.228820895316715678, -0.7216878364870267237 ) ) ;
#70183 = CARTESIAN_POINT ( 'NONE',  ( -6.656127069666307072, 6.730179434224282886, 0.7998128361456341429 ) ) ;
#70184 = CARTESIAN_POINT ( 'NONE',  ( 0.3866913795912775842, 3.974415841077574285, -11.53480748357603858 ) ) ;
#70185 = CARTESIAN_POINT ( 'NONE',  ( -5.544921637864820951, 9.412899644243539754, -0.7216878364870207285 ) ) ;
#70186 = CARTESIAN_POINT ( 'NONE',  ( 3.856632026064894525, 0.7917978285330304900, 2.060012427959257764 ) ) ;
#70187 = CARTESIAN_POINT ( 'NONE',  ( 1.642778471875000035, -2.413541666188709911, -2.845375778867859751 ) ) ;
#70188 = ORIENTED_EDGE ( 'NONE', *, *, #36376, .T. ) ;
#70189 = CARTESIAN_POINT ( 'NONE',  ( 0.8482322855925720217, -1.845984902429298025, -0.2351823381797259749 ) ) ;
#70190 = CARTESIAN_POINT ( 'NONE',  ( -0.1290005225502433017, 7.629137130509076492, -2.773995091683974401 ) ) ;
#70191 = CARTESIAN_POINT ( 'NONE',  ( 0.7499999999999902300, 5.347916667349482012, -1.299038105676658228 ) ) ;
#70192 = FACE_OUTER_BOUND ( 'NONE', #38936, .T. ) ;
#70194 = CARTESIAN_POINT ( 'NONE',  ( 6.925078400183531713, 7.629137130509035636, 2.844348168701658075 ) ) ;
#70193 = CARTESIAN_POINT ( 'NONE',  ( -4.593509350353649268, 8.487843406384373068, -0.1931319778552646749 ) ) ;
#70195 = ORIENTED_EDGE ( 'NONE', *, *, #162297, .F. ) ;
#70196 = CARTESIAN_POINT ( 'NONE',  ( 2.817317228389113470, -0.2032538945386449802, 2.050847873933867138 ) ) ;
#70197 = CARTESIAN_POINT ( 'NONE',  ( -4.957638175832625493E-14, 2.078125000341435769, -1.570758158831802254 ) ) ;
#70198 = EDGE_CURVE ( 'NONE', #32144, #84441, #35899, .T. ) ;
#70199 = CARTESIAN_POINT ( 'NONE',  ( -6.742482464697739708, 6.760651051769146491, 0.7998128361456341429 ) ) ;
#70200 = CARTESIAN_POINT ( 'NONE',  ( 2.719404001658455527, 1.707403962800517316, 1.078498517531191858 ) ) ;
#70201 = SURFACE_STYLE_USAGE ( .BOTH. , #122278 ) ;
#70202 = CARTESIAN_POINT ( 'NONE',  ( 5.359550796103802028, 5.147230771742885125, -0.7998128361456231517 ) ) ;
#70203 = CARTESIAN_POINT ( 'NONE',  ( 2.500915792353772815, 1.655931770628838784, -1.226644000274518476 ) ) ;
#70205 = CARTESIAN_POINT ( 'NONE',  ( -8.012344526598182026E-15, 13.79687500034139624, -1.575800808251669460 ) ) ;
#70204 = CARTESIAN_POINT ( 'NONE',  ( -9.604686356149279902, 3.481548657788669843, -7.193747284969073341 ) ) ;
#70206 = CARTESIAN_POINT ( 'NONE',  ( 6.470265622219697477, 8.571729197388226140, -1.599625672291262513 ) ) ;
#70207 = AXIS2_PLACEMENT_3D ( 'NONE', #6450, #175392, #56298 ) ;
#70208 = CARTESIAN_POINT ( 'NONE',  ( 3.578681416171143770, 3.551814636441959383, 2.500000000000000444 ) ) ;
#70209 = AXIS2_PLACEMENT_3D ( 'NONE', #63910, #178747, #96447 ) ;
#70210 = CARTESIAN_POINT ( 'NONE',  ( 5.883472226557855400, 2.040502603023553796, -0.8411249186189362348 ) ) ;
#70211 = CARTESIAN_POINT ( 'NONE',  ( 1.335488691732108046, -1.954760257947166568, 0.9229496955955732718 ) ) ;
#70212 = CARTESIAN_POINT ( 'NONE',  ( -4.107757355260591936, 7.736207981205250661, 1.040834085586084257E-14 ) ) ;
#70213 = CARTESIAN_POINT ( 'NONE',  ( 0.9543149826918421175, -1.275552737861269437, 1.561884623745241951 ) ) ;
#70214 = EDGE_CURVE ( 'NONE', #79190, #115058, #166639, .T. ) ;
#70215 = CARTESIAN_POINT ( 'NONE',  ( 1.933413756328787869, 1.181669745456917830, 1.971221161662185528 ) ) ;
#70216 = CARTESIAN_POINT ( 'NONE',  ( 4.599659039672021166, 8.466119764437587847, 0.4625730637407374779 ) ) ;
#70217 = CARTESIAN_POINT ( 'NONE',  ( 6.621744163077868173, -0.4141588628726756149, 1.873750786029332316 ) ) ;
#70218 = CARTESIAN_POINT ( 'NONE',  ( 1.909527279894939422, 8.998253746724575564, -0.7749999999999996891 ) ) ;
#70219 = EDGE_CURVE ( 'NONE', #9929, #157346, #135577, .T. ) ;
#70220 = CARTESIAN_POINT ( 'NONE',  ( 1.920565142479381038, 1.744437793965779582, 0.6759427408406930571 ) ) ;
#70221 = CARTESIAN_POINT ( 'NONE',  ( 3.467982673848205355, -0.9896861206786079501, 1.756853968756578066 ) ) ;
#70223 = DIRECTION ( 'NONE',  ( -0.1510067114093955887, 0.000000000000000000, 0.9885327375000383388 ) ) ;
#70222 = CARTESIAN_POINT ( 'NONE',  ( 1.364683531249988535, 1.613541667008084879, 0.7879004041258500513 ) ) ;
#70225 = CARTESIAN_POINT ( 'NONE',  ( 5.197925827040419833, -0.7590715138193807610, 1.964706065220876541 ) ) ;
#70224 = CARTESIAN_POINT ( 'NONE',  ( -7.178152263431422320, 10.46192917639026554, 1.199719254218453823 ) ) ;
#70226 = CARTESIAN_POINT ( 'NONE',  ( 5.282873410819217241, 9.315102745931094219, -0.7998128361456281477 ) ) ;
#70228 = CARTESIAN_POINT ( 'NONE',  ( -7.901704598666176693, 8.113076874732334076, 0.7998128361456602331 ) ) ;
#70227 = CARTESIAN_POINT ( 'NONE',  ( 4.441177836928239309, 7.339068688795062911, 1.199719254218452047 ) ) ;
#70229 = CARTESIAN_POINT ( 'NONE',  ( 5.502215278945715937, -0.9042992897083046433, 1.806084391566422198 ) ) ;
#70230 = CARTESIAN_POINT ( 'NONE',  ( -1.402160292154681736E-14, -1.006249999317181620, 1.732050807568877637 ) ) ;
#70231 = CARTESIAN_POINT ( 'NONE',  ( 0.8485701241471826917, -2.046539366587364572, -0.2563945212397024109 ) ) ;
#70232 = CARTESIAN_POINT ( 'NONE',  ( 8.188761592974039161, 10.57664116326830595, -1.443375672974063439 ) ) ;
#70233 = CARTESIAN_POINT ( 'NONE',  ( 5.870447946289019114, -1.376328297836002301, 1.666777564274177781 ) ) ;
#70234 = CARTESIAN_POINT ( 'NONE',  ( 7.225569521440261767, 7.394528961293920233, -0.7998128361456341429 ) ) ;
#70235 = CARTESIAN_POINT ( 'NONE',  ( -1.402160292154681736E-14, -0.2406249996585799189, -1.575800808251665908 ) ) ;
#70236 = CARTESIAN_POINT ( 'NONE',  ( 5.204350862799327793, 7.165104988056252289, -1.599625672291281386 ) ) ;
#70237 = CARTESIAN_POINT ( 'NONE',  ( 8.229436053370676518, 9.663725486096376827, 1.082531754730558626 ) ) ;
#70239 = CARTESIAN_POINT ( 'NONE',  ( 0.000000000000000000, 0.08000000000000020983, 0.000000000000000000 ) ) ;
#70238 = CARTESIAN_POINT ( 'NONE',  ( 3.438082271139299539, 1.374976351402785513, 1.680335591205921908 ) ) ;
#70241 = CARTESIAN_POINT ( 'NONE',  ( 2.225889136967126536, 1.786374552192676823, 0.4457033907802817052 ) ) ;
#70240 = CARTESIAN_POINT ( 'NONE',  ( -5.504247177468192476, 7.444707678511436555, 1.443375672974064550 ) ) ;
#70242 = CARTESIAN_POINT ( 'NONE',  ( -1.364683531249997417, 3.259375000341423245, 1.214306433183764966E-14 ) ) ;
#70243 = CARTESIAN_POINT ( 'NONE',  ( 4.142245973918059043, 0.5854081421233224836, 2.111838497463234710 ) ) ;
#70244 = CARTESIAN_POINT ( 'NONE',  ( 6.883263157960330503, 2.417872181280413812, 2.534681901920758929 ) ) ;
#70245 = CARTESIAN_POINT ( 'NONE',  ( 4.487383681424582882, 2.022794180288649990, -1.013680454646571638 ) ) ;
#70246 = CARTESIAN_POINT ( 'NONE',  ( -4.557512192488103686, 8.468847991211438497, -0.7998128361456281477 ) ) ;
#70247 = B_SPLINE_CURVE_WITH_KNOTS ( 'NONE', 3,
 ( #64085, #96610, #112904, #79266, #46790, #113975 ),
 .UNSPECIFIED., .F., .F.,
 ( 4, 2, 4 ),
 ( 0.000000000000000000, 0.0003779448103413554443, 0.0007558896206827108886 ),
 .UNSPECIFIED. ) ;
#70248 = CARTESIAN_POINT ( 'NONE',  ( -11.78331023100045627, 9.799999999999982947, 1.799999999999999600 ) ) ;
#70249 = CARTESIAN_POINT ( 'NONE',  ( 4.985841187518467166, 7.931359929992748192, -1.059499378661461710 ) ) ;
#70250 = VECTOR ( 'NONE', #146610, 1000.000000000000000 ) ;
#70251 = CARTESIAN_POINT ( 'NONE',  ( 1.499999999999993117, 13.35416666666667140, 0.8660254037844409281 ) ) ;
#70252 = CARTESIAN_POINT ( 'NONE',  ( -4.950135482320918712, 7.828889591799445213, -1.082531754730549967 ) ) ;
#70253 = CARTESIAN_POINT ( 'NONE',  ( 5.180624094197585627, 8.097792972322238825, -1.082531754730548412 ) ) ;
#70254 = CARTESIAN_POINT ( 'NONE',  ( 5.114393831954183511, 1.220379059178023695, -1.281870188591783588 ) ) ;
#70255 = CARTESIAN_POINT ( 'NONE',  ( 6.598014311344812199, 10.84943379654430906, 1.040834085586084257E-14 ) ) ;
#70256 = CARTESIAN_POINT ( 'NONE',  ( 1.589043446250279601, -0.3083810453359912551, -2.083120927691509916 ) ) ;
#70258 = CARTESIAN_POINT ( 'NONE',  ( 1.499999999999989120, 2.775000000000020339, 1.214306433183764966E-14 ) ) ;
#70257 = CARTESIAN_POINT ( 'NONE',  ( -1.364683531250000748, 12.35937500034139980, 0.000000000000000000 ) ) ;
#70259 = CARTESIAN_POINT ( 'NONE',  ( 2.277737068081890914, -1.911112558508936354, 0.4757300241334978530 ) ) ;
#70260 = CARTESIAN_POINT ( 'NONE',  ( -2.823841133396259639, 6.516508098929413961, -0.7998128361456481317 ) ) ;
#70261 = CARTESIAN_POINT ( 'NONE',  ( 3.658644423338138107, 7.354739799217567153, 0.2810151790806048044 ) ) ;
#70263 = EDGE_LOOP ( 'NONE', ( #136147, #185439, #21183 ) ) ;
#70262 = CARTESIAN_POINT ( 'NONE',  ( 6.134996530155978789, 1.693739186514784167, 0.6432786700914516764 ) ) ;
#70264 = CARTESIAN_POINT ( 'NONE',  ( 5.002595493762530765, 8.780185809457538681, 1.040834085586084257E-14 ) ) ;
#70265 = CARTESIAN_POINT ( 'NONE',  ( -1.402160292154681736E-14, -0.1156249996585793222, 1.575800808251672791 ) ) ;
#70266 = CARTESIAN_POINT ( 'NONE',  ( 6.420764531294745225, 1.746252128813120086, 0.6712297951826234899 ) ) ;
#70267 = AXIS2_PLACEMENT_3D ( 'NONE', #108690, #172566, #123899 ) ;
#70268 = CARTESIAN_POINT ( 'NONE',  ( 6.034052368894809781, 1.228512962337786174, 1.666229478724051027 ) ) ;
#70269 = CARTESIAN_POINT ( 'NONE',  ( -0.6125000000000123679, 2.958333333333326820, -1.060881119635965764 ) ) ;
#70270 = CARTESIAN_POINT ( 'NONE',  ( -5.438229012412903352, 6.477593614970734492, -1.082531754730549967 ) ) ;
#70271 = CARTESIAN_POINT ( 'NONE',  ( 0.2564123431100414074, -2.069877475643782994, -0.05227228806716639753 ) ) ;
#70272 = CARTESIAN_POINT ( 'NONE',  ( -1.500000000000001332, -0.09999999999997510880, 0.000000000000000000 ) ) ;
#70273 = CARTESIAN_POINT ( 'NONE',  ( 8.613507663383630941, 8.943513783569379427, -0.7998128361456221525 ) ) ;
#70274 = CARTESIAN_POINT ( 'NONE',  ( -8.208571938070008400, 11.66408546346865016, -1.199719254218446718 ) ) ;
#70275 = CARTESIAN_POINT ( 'NONE',  ( 6.879836604291781121, 6.991173891287354003, -0.7998128361456341429 ) ) ;
#70276 = CARTESIAN_POINT ( 'NONE',  ( 1.364683531249986537, 0.4052083336747511200, -0.7879004041258309554 ) ) ;
#70277 = CARTESIAN_POINT ( 'NONE',  ( 1.499999999999987121, 1.295833333333353377, -0.8660254037844253849 ) ) ;
#70279 = CARTESIAN_POINT ( 'NONE',  ( 6.471319392424407901, 6.444294134116939077, 0.7998128361456341429 ) ) ;
#70278 = CARTESIAN_POINT ( 'NONE',  ( 5.213317179658601752, -1.656387821537348426, -1.051046178410528942 ) ) ;
#70280 = CARTESIAN_POINT ( 'NONE',  ( 3.233749808020690342, -1.861731463674856979, -0.7741979076196571219 ) ) ;
#70281 = CARTESIAN_POINT ( 'NONE',  ( 3.063600739116902449, 1.219304168433880564, 1.477546071989847665 ) ) ;
#70282 = DIRECTION ( 'NONE',  ( -0.7978120914393174168, 0.6029061840396252592, 6.536721945407052908E-15 ) ) ;
#70283 = AXIS2_PLACEMENT_3D ( 'NONE', #38529, #186897, #91574 ) ;
#70284 = CARTESIAN_POINT ( 'NONE',  ( -0.005964567173097347699, -2.191213315851054944, -0.04726126812268362232 ) ) ;
#70285 = CARTESIAN_POINT ( 'NONE',  ( 0.2333690889706682703, 1.352610664630080839, -2.308230059406161772 ) ) ;
#70286 = CARTESIAN_POINT ( 'NONE',  ( 1.827212670807505379, -1.763035892288829620, 0.6254473451912796467 ) ) ;
#70287 = CARTESIAN_POINT ( 'NONE',  ( 1.364683531249990311, 5.363541667008086655, 0.7879004041258500513 ) ) ;
#70288 = CARTESIAN_POINT ( 'NONE',  ( 4.605731108040309607, 1.494732351555028371, 1.348829144277723824 ) ) ;
#70289 = CARTESIAN_POINT ( 'NONE',  ( -8.857554428429624593, 9.228235009456373206, 0.7998128361456462443 ) ) ;
#70291 = CARTESIAN_POINT ( 'NONE',  ( 5.009417666957850734, -2.010078760914670859, 0.6651486602928055047 ) ) ;
#70290 = CARTESIAN_POINT ( 'NONE',  ( -5.097502569058215194, 6.970172302033127210, -1.443375672974053447 ) ) ;
#70292 = FACE_OUTER_BOUND ( 'NONE', #93832, .T. ) ;
#70293 = CARTESIAN_POINT ( 'NONE',  ( 6.566853775770633561, 1.536883091774071453, -1.387433097640700774 ) ) ;
#70295 = CARTESIAN_POINT ( 'NONE',  ( 4.064230490221667935, 7.507048082629879104, -0.5272979928686331030 ) ) ;
#70294 = CARTESIAN_POINT ( 'NONE',  ( 0.7145361118556601276, 1.933244891618046024, 0.7966077499205433954 ) ) ;
#70297 = ORIENTED_EDGE ( 'NONE', *, *, #47358, .F. ) ;
#70296 = CARTESIAN_POINT ( 'NONE',  ( 6.106453908201667780, -0.6597477751954274883, -1.702385593799011110 ) ) ;
#70298 = CARTESIAN_POINT ( 'NONE',  ( 8.749089199520284410, 9.101692242395490240, 0.7998128361456481317 ) ) ;
#70299 = CIRCLE ( 'NONE', #56425, 8.300000000000000711 ) ;
#70300 = CARTESIAN_POINT ( 'NONE',  ( -2.788906526875773208E-15, 11.96875000068279604, -1.499999999999998446 ) ) ;
#70301 = CARTESIAN_POINT ( 'NONE',  ( -10.41980074470002648, 5.020554563858687480, 5.279403930596816785 ) ) ;
#70302 = CARTESIAN_POINT ( 'NONE',  ( 7.090551149822739596, 8.335026431957096804, 1.082531754730558626 ) ) ;
#70303 = CARTESIAN_POINT ( 'NONE',  ( 1.364683531249997417, 13.04687500034139980, 2.602085213965210642E-15 ) ) ;
#70305 = CARTESIAN_POINT ( 'NONE',  ( 0.8733459280946423986, 0.3543511941397787801, -1.776278655377810489 ) ) ;
#70304 = CARTESIAN_POINT ( 'NONE',  ( 5.820193082016415609, 10.01225203898631655, 0.000000000000000000 ) ) ;
#70306 = CARTESIAN_POINT ( 'NONE',  ( -7.995557903757128493, 10.35123685918189729, 1.599625672291295375 ) ) ;
#70307 = CARTESIAN_POINT ( 'NONE',  ( 4.143988507271280319, 7.986403691791820414, -0.7998128361456221525 ) ) ;
#70308 = DIRECTION ( 'NONE',  ( 0.000000000000000000, 0.000000000000000000, 1.000000000000000000 ) ) ;
#70309 = CARTESIAN_POINT ( 'NONE',  ( -11.41381675112459959, 10.89999999999999325, 3.704697986577257129 ) ) ;
#70310 = CARTESIAN_POINT ( 'NONE',  ( 8.595506201383999567, 12.97191496834930113, 0.7216878364870438212 ) ) ;
#70311 = ORIENTED_EDGE ( 'NONE', *, *, #201380, .F. ) ;
#70312 = ADVANCED_FACE ( 'NONE', ( #57444 ), #105147, .F. ) ;
#70313 = CARTESIAN_POINT ( 'NONE',  ( 6.064077406165095496, -1.076301619396256237, 1.704949653848472302 ) ) ;
#70314 = CARTESIAN_POINT ( 'NONE',  ( 0.03014954708456181465, -2.078685333231004684, 0.4181070283913386199 ) ) ;
#70315 = CARTESIAN_POINT ( 'NONE',  ( 1.208258962943321357, -6.100893924328829751E-15, -0.5075860003171979162 ) ) ;
#70316 = CARTESIAN_POINT ( 'NONE',  ( 2.275435306267621804, 5.643409308550367598, 0.5316758947214432762 ) ) ;
#70317 = CARTESIAN_POINT ( 'NONE',  ( 7.004500933659072892, -6.920331743269710678, 7.004500933659049799 ) ) ;
#70318 = CARTESIAN_POINT ( 'NONE',  ( -4.500943810056945438, 5.313817868896925312, 1.082531754730560403 ) ) ;
#70319 = CARTESIAN_POINT ( 'NONE',  ( 9.246297574839974942, 11.81043314211192019, 1.443375672974076540 ) ) ;
#70320 = CARTESIAN_POINT ( 'NONE',  ( 3.063290813078624719, 1.661244007368352982, 1.057527034793050547 ) ) ;
#70321 = CARTESIAN_POINT ( 'NONE',  ( 4.411732571322396268, -1.242743209197882059, -1.587826168943158089 ) ) ;
#70322 = CARTESIAN_POINT ( 'NONE',  ( -5.506582945444718824, 9.576097202994168001, 0.7998128361456481317 ) ) ;
#70323 = CARTESIAN_POINT ( 'NONE',  ( -3.253593677155282471, 6.739683690082376444, 1.040834085586084257E-14 ) ) ;
#70324 = CARTESIAN_POINT ( 'NONE',  ( 0.4355862708379926174, -6.583980363595115293, 9.606148981167594414 ) ) ;
#70325 = CARTESIAN_POINT ( 'NONE',  ( 5.173855182012670362, -1.219361875273092366, 1.820681821249593657 ) ) ;
#70326 = FACE_OUTER_BOUND ( 'NONE', #127608, .T. ) ;
#70327 = CARTESIAN_POINT ( 'NONE',  ( 3.557566385928968788, 0.4691178692100838599, -1.868274323828737371 ) ) ;
#70328 = CARTESIAN_POINT ( 'NONE',  ( -8.369460898337653276, 8.658792557682392754, 0.7998128361456462443 ) ) ;
#70329 = CARTESIAN_POINT ( 'NONE',  ( -0.02988540731103071432, 0.005807295984020746475, -1.726291166677936362 ) ) ;
#70330 = CARTESIAN_POINT ( 'NONE',  ( 7.334597915313080918, 9.580116872663850813, 1.040834085586084257E-14 ) ) ;
#70331 = DIRECTION ( 'NONE',  ( 0.000000000000000000, -1.000000000000000000, 0.000000000000000000 ) ) ;
#70332 = ORIENTED_EDGE ( 'NONE', *, *, #158186, .F. ) ;
#70333 = CARTESIAN_POINT ( 'NONE',  ( 4.909461021924254709, 5.860697626067345567, 1.082531754730549078 ) ) ;
#70334 = CARTESIAN_POINT ( 'NONE',  ( 4.733233314711627671, 0.004152288854553880422, -1.969629310717621040 ) ) ;
#70336 = CARTESIAN_POINT ( 'NONE',  ( 3.545567672969043294, -1.859159518717553139, 0.7725093927312511877 ) ) ;
#70335 = CARTESIAN_POINT ( 'NONE',  ( 0.1166052997346351955, -0.09441621361710265947, 1.939868080593883048 ) ) ;
#70337 = CARTESIAN_POINT ( 'NONE',  ( 5.185072832991014735, -1.223605693886620438, -1.945460884747321151 ) ) ;
#70339 = CARTESIAN_POINT ( 'NONE',  ( 3.854231730816888302, -1.858662791824859051, -0.09517680055876918954 ) ) ;
#70338 = FACE_OUTER_BOUND ( 'NONE', #139530, .T. ) ;
#70340 = CARTESIAN_POINT ( 'NONE',  ( 5.189738938980948291, 9.276722205444929870, 0.000000000000000000 ) ) ;
#70341 = CARTESIAN_POINT ( 'NONE',  ( -0.4019237886466802689, 11.44866454968463110, -1.500000000000002887 ) ) ;
#70342 = DIRECTION ( 'NONE',  ( 1.000000000000000000, 1.725633230170963762E-31, 8.638326563840814399E-31 ) ) ;
#70343 = CARTESIAN_POINT ( 'NONE',  ( -6.775324078527193983, 8.927630729746953264, -1.599625672291263179 ) ) ;
#70344 = CARTESIAN_POINT ( 'NONE',  ( -4.177320726786319049, 6.927272377009067839, -1.082531754730551743 ) ) ;
#70345 = CARTESIAN_POINT ( 'NONE',  ( 0.1522426329377546128, 0.8445714516599597266, 2.022489037641273857 ) ) ;
#70346 = CARTESIAN_POINT ( 'NONE',  ( 5.666945020832177882, 6.674152614801420746, 1.082531754730558626 ) ) ;
#70347 = VERTEX_POINT ( 'NONE', #122540 ) ;
#70348 = DIRECTION ( 'NONE',  ( -0.000000000000000000, 1.000000000000000000, 0.000000000000000000 ) ) ;
#70349 = CARTESIAN_POINT ( 'NONE',  ( 0.4917504562594980921, 10.46609003534429405, 2.420000000000000373 ) ) ;
#70350 = CARTESIAN_POINT ( 'NONE',  ( 0.6447967512687136082, -1.567379569643694515, 0.9359695128687425258 ) ) ;
#70351 = CARTESIAN_POINT ( 'NONE',  ( -2.788173145904702555, 6.404619103530779789, -0.7998128361456281477 ) ) ;
#70352 = AXIS2_PLACEMENT_3D ( 'NONE', #34232, #632, #181547 ) ;
#70353 = CARTESIAN_POINT ( 'NONE',  ( 2.830371795882984820, 0.6218406304432465559, -1.619021885657184745 ) ) ;
#70354 = CARTESIAN_POINT ( 'NONE',  ( -10.39230484541328181, 3.038454817776199857, -5.999999999999975131 ) ) ;
#70355 = CARTESIAN_POINT ( 'NONE',  ( -4.955918092712652268, 4.886086657537050293, 0.4932186882876873901 ) ) ;
#70356 = CARTESIAN_POINT ( 'NONE',  ( -0.7499999999999972244, 3.358333333333359150, -1.299038105676652011 ) ) ;
#70357 = AXIS2_PLACEMENT_3D ( 'NONE', #135803, #20944, #154185 ) ;
#70358 = CARTESIAN_POINT ( 'NONE',  ( 5.725187622324654946, -0.04035785615889506128, 1.825416780793003069 ) ) ;
#70359 = CARTESIAN_POINT ( 'NONE',  ( 3.819154011256303161, -1.728040176127441763, -0.9287006429716244682 ) ) ;
#70360 = CARTESIAN_POINT ( 'NONE',  ( 1.224999999999969225, -0.8333333326504639427, 0.7072540797572596238 ) ) ;
#70361 = CARTESIAN_POINT ( 'NONE',  ( -9.179033691651859783, 10.66762638080401260, 1.199719254218462483 ) ) ;
#70362 = CARTESIAN_POINT ( 'NONE',  ( 6.252281394196331554, 10.44607872653774372, 1.040834085586084257E-14 ) ) ;
#70363 = CARTESIAN_POINT ( 'NONE',  ( 5.268275487455277073, 2.118052368503114291, -0.1043780312826799589 ) ) ;
#70364 = CARTESIAN_POINT ( 'NONE',  ( 7.828907357248368726, 8.098423103070084395, 0.7998128361456281477 ) ) ;
#70365 = CARTESIAN_POINT ( 'NONE',  ( -10.13488352141530768, 11.78278451552804817, 1.199719254218462483 ) ) ;
#70366 = CARTESIAN_POINT ( 'NONE',  ( 1.534126288888465917, 1.230018689141991306, 1.665114864061276734 ) ) ;
#70368 = CARTESIAN_POINT ( 'NONE',  ( -1.364683531250014514, 0.3427083336747508424, 0.7879004041258379498 ) ) ;
#70367 = CARTESIAN_POINT ( 'NONE',  ( -11.86145016429273191, 10.90000000000000036, 1.099999999999996980 ) ) ;
#70370 = ORIENTED_EDGE ( 'NONE', *, *, #86369, .T. ) ;
#70369 = CARTESIAN_POINT ( 'NONE',  ( 4.283969606688295961, 2.154612580813870082, -0.5396949931109666920 ) ) ;
#70371 = CARTESIAN_POINT ( 'NONE',  ( 1.864337758866913441, -0.1181282521124735752, -2.295782230965204285 ) ) ;
#70372 = CARTESIAN_POINT ( 'NONE',  ( 9.585251415181632595, 10.28514086057449184, 0.000000000000000000 ) ) ;
#70374 = CARTESIAN_POINT ( 'NONE',  ( 1.642778471875001811, -3.142708332855375986, 2.845375778867859751 ) ) ;
#70373 = CARTESIAN_POINT ( 'NONE',  ( 7.851580356089786328, 8.332800968292465527, 0.000000000000000000 ) ) ;
#70375 = SURFACE_STYLE_FILL_AREA ( #67177 ) ;
#70376 = CARTESIAN_POINT ( 'NONE',  ( 6.509000000000016328, 0.001920477310516919547, 2.100274754360693219 ) ) ;
#70377 = DIRECTION ( 'NONE',  ( 0.000000000000000000, -1.000000000000000000, 0.000000000000000000 ) ) ;
#70378 = CARTESIAN_POINT ( 'NONE',  ( 2.795058504854182946, -0.1448928079688660830, -1.906987441340234568 ) ) ;
#70379 = CARTESIAN_POINT ( 'NONE',  ( 1.394453263437886604E-15, -1.312499999999999556, 3.474999999999999645 ) ) ;
#70380 = CARTESIAN_POINT ( 'NONE',  ( 4.225434206992398245, -1.650187577572001629, 0.5017251585606904429 ) ) ;
#70381 = CARTESIAN_POINT ( 'NONE',  ( 2.044158018538293042, 0.8666093899718421145, 1.820985203412978093 ) ) ;
#70382 = CARTESIAN_POINT ( 'NONE',  ( 4.201969167805962968, 2.101520711257957252, 0.9317802909727909144 ) ) ;
#70383 = CARTESIAN_POINT ( 'NONE',  ( -11.41381676900480713, 12.56958039977600983, -3.704697931490059215 ) ) ;
#70384 = CARTESIAN_POINT ( 'NONE',  ( 6.006491595720174104, -0.7565722652288708883, -1.965664901909335738 ) ) ;
#70385 = CARTESIAN_POINT ( 'NONE',  ( -4.665414256878293031, 7.496714828783040296, -1.082531754730549967 ) ) ;
#70386 = CARTESIAN_POINT ( 'NONE',  ( 4.288192095134175652, -1.750260269857591755, -0.2610086191854649740 ) ) ;
#70388 = CARTESIAN_POINT ( 'NONE',  ( 0.3402841477759439570, 2.286568017602428338, 0.1625022809590911665 ) ) ;
#70387 = CARTESIAN_POINT ( 'NONE',  ( 8.011942431032855083, 8.311964022485323511, 0.7998128361456291469 ) ) ;
#70389 = CARTESIAN_POINT ( 'NONE',  ( 0.02286245922865359423, -1.065969982613410583, -1.375977130364250955 ) ) ;
#70390 = CARTESIAN_POINT ( 'NONE',  ( 0.4339420102923677303, 3.986509213895420345, -0.4852232617283462335 ) ) ;
#70391 = CARTESIAN_POINT ( 'NONE',  ( 5.806613533822880591, 1.931179984464112653, 1.035834350304319695 ) ) ;
#70392 = CARTESIAN_POINT ( 'NONE',  ( -6.005335696210345020, 5.970922831858983315, 0.7998128361456281477 ) ) ;
#70393 = CARTESIAN_POINT ( 'NONE',  ( 1.360316468749989793, -0.4322916663252800995, -0.7853790794158961308 ) ) ;
#70394 = CARTESIAN_POINT ( 'NONE',  ( 3.920443345323491258, 7.328669659756545940, -0.8660684152334082730 ) ) ;
#70395 = CARTESIAN_POINT ( 'NONE',  ( 0.1393978552833140261, -0.1497620924123649333, -2.137132186964474378 ) ) ;
#70396 = CARTESIAN_POINT ( 'NONE',  ( 1.499232818411553536, -0.2420282084563407654, 2.001858358113464575 ) ) ;
#70397 = CARTESIAN_POINT ( 'NONE',  ( -0.7500000000000249800, -0.7770833326505161009, 1.299038105676659116 ) ) ;
#70398 = CARTESIAN_POINT ( 'NONE',  ( 4.494702926938664689, -0.4234472454235098104, -1.879237243589318318 ) ) ;
#70399 = CARTESIAN_POINT ( 'NONE',  ( 1.364683531250000303, 11.75520833367473017, -0.7879004041258355073 ) ) ;
#70400 = CARTESIAN_POINT ( 'NONE',  ( 1.090412635922506368, 1.328748260410139492, 1.780047631856091606 ) ) ;
#70402 = VERTEX_POINT ( 'NONE', #91030 ) ;
#70401 = CARTESIAN_POINT ( 'NONE',  ( 8.204655514564224816, 12.72384853363364066, 1.040834085586084257E-14 ) ) ;
#70404 = CARTESIAN_POINT ( 'NONE',  ( -1.230728480726522411, 3.230010058876359835, 0.7750000000000100142 ) ) ;
#70403 = DIRECTION ( 'NONE',  ( 0.9632918427306580433, 0.000000000000000000, 0.2684563758389303945 ) ) ;
#70405 = CARTESIAN_POINT ( 'NONE',  ( 4.162516854595432747, 4.815023404238158555, 1.199719254218464037 ) ) ;
#70406 = CARTESIAN_POINT ( 'NONE',  ( -0.7500000000000006661, 8.989583334016129967, -1.299038105676657340 ) ) ;
#70407 = FILL_AREA_STYLE_COLOUR ( '', #197785 ) ;
#70408 = CARTESIAN_POINT ( 'NONE',  ( 3.843067196288481480, 0.5821562417002418277, -1.640339850388317089 ) ) ;
#70409 = CARTESIAN_POINT ( 'NONE',  ( 2.506241959165692812, 1.961374882610424919, 0.05109738790698423877 ) ) ;
#70411 = CARTESIAN_POINT ( 'NONE',  ( 0.6823417656249899377, 2.405208333674753618, 1.181850606188767472 ) ) ;
#70410 = CARTESIAN_POINT ( 'NONE',  ( 5.311043488251262268, 7.219303374425030562, -1.599625672291256295 ) ) ;
#70412 = CARTESIAN_POINT ( 'NONE',  ( -5.845765802024414981, 6.039811503853035113, 0.4322504083978280232 ) ) ;
#70413 = CARTESIAN_POINT ( 'NONE',  ( -0.9311234436981532525, -1.984380368602567835, 3.474999999999999201 ) ) ;
#70414 = CIRCLE ( 'NONE', #191495, 0.08000000000000014044 ) ;
#70415 = CIRCLE ( 'NONE', #122497, 1.500000000000000222 ) ;
#70416 = CARTESIAN_POINT ( 'NONE',  ( 0.3794369086736723018, -0.1030016517138358095, 2.060237976199934984 ) ) ;
#70417 = CARTESIAN_POINT ( 'NONE',  ( -8.355902744723985975, 8.642974711799791265, 1.040834085586084257E-14 ) ) ;
#70418 = CARTESIAN_POINT ( 'NONE',  ( -5.572037945092175981, 5.603058478803387032, 0.7216878364870317197 ) ) ;
#70419 = CARTESIAN_POINT ( 'NONE',  ( 0.8314075926023238861, 0.1693486111025067908, 2.256218002396610522 ) ) ;
#70421 = VERTEX_POINT ( 'NONE', #154948 ) ;
#70420 = CARTESIAN_POINT ( 'NONE',  ( -6.718228810771495141, 7.796687353110217877, 1.199719254218450271 ) ) ;
#70422 = CARTESIAN_POINT ( 'NONE',  ( -1.402160292154681736E-14, -0.1312499993171854229, -1.732050807568870754 ) ) ;
#70423 = ADVANCED_FACE ( 'NONE', ( #171187 ), #21700, .T. ) ;
#70424 = CARTESIAN_POINT ( 'NONE',  ( 1.985418980784030119, 1.286400883397397221, 1.358229366437320618 ) ) ;
#70425 = CARTESIAN_POINT ( 'NONE',  ( -0.03512515232485542011, -1.681152455970882809, -0.4250410675877940303 ) ) ;
#70426 = AXIS2_PLACEMENT_3D ( 'NONE', #63878, #33507, #214339 ) ;
#70427 = CARTESIAN_POINT ( 'NONE',  ( 4.493798347139664529, -2.191065130646638437, -0.05333993539427539510 ) ) ;
#70428 = CARTESIAN_POINT ( 'NONE',  ( 5.684705870536221894, -2.249774798156725986, -0.5126945500162644054 ) ) ;
#70429 = CARTESIAN_POINT ( 'NONE',  ( 0.7255486961553169190, -1.957115920898297112, 0.6459669076722980297 ) ) ;
#70430 = CARTESIAN_POINT ( 'NONE',  ( 3.890518024738118807, 1.639914603359222456, -1.039847546996591765 ) ) ;
#70431 = CARTESIAN_POINT ( 'NONE',  ( -3.592547517496935683, 6.174760622846296343, -1.082531754730548412 ) ) ;
#70432 = CARTESIAN_POINT ( 'NONE',  ( 5.852782322939766857, -1.474943281369223147, 1.150351685248012457 ) ) ;
#70433 = LINE ( 'NONE', #170088, #74829 ) ;
#70434 = CARTESIAN_POINT ( 'NONE',  ( -0.6801582343750438575, 1.932291667008062541, 1.178068619123787908 ) ) ;
#70435 = CARTESIAN_POINT ( 'NONE',  ( 5.115861365725078436, 0.1511377038382749338, 2.010826595755777824 ) ) ;
#70436 = CARTESIAN_POINT ( 'NONE',  ( -3.267151830768952880, 5.795132321663641228, -1.082531754730549078 ) ) ;
#70437 = CARTESIAN_POINT ( 'NONE',  ( -5.956828388357799042, 8.042995434541133193, 1.599625672291263179 ) ) ;
#70438 = CARTESIAN_POINT ( 'NONE',  ( 9.610031953988080744, 10.10612545594124967, -0.7998128361456281477 ) ) ;
#70440 = CARTESIAN_POINT ( 'NONE',  ( 7.836017471263539313, -5.361065518611640712, -7.720011280421980260 ) ) ;
#70439 = CARTESIAN_POINT ( 'NONE',  ( 1.312830284664792790, 1.609138963534262778, 0.8624270714618911260 ) ) ;
#70441 = CARTESIAN_POINT ( 'NONE',  ( -6.296835998904160014, 6.311006518335105397, 0.000000000000000000 ) ) ;
#70442 = CARTESIAN_POINT ( 'NONE',  ( -5.819596349002143398, 5.754226926782749274, -0.5594349688150419553 ) ) ;
#70443 = CARTESIAN_POINT ( 'NONE',  ( -11.16150260363039060, 4.727604019697102977, 6.014961758122009172 ) ) ;
#70444 = EDGE_LOOP ( 'NONE', ( #49165, #171834, #143387, #134105 ) ) ;
#70445 = CARTESIAN_POINT ( 'NONE',  ( 6.825078400183568483, -0.002763825414428457399, 2.044262525762724270 ) ) ;
#70446 = CARTESIAN_POINT ( 'NONE',  ( -6.305950843687521790, 7.489935751457798219, 1.082531754730548412 ) ) ;
#70447 = EDGE_CURVE ( 'NONE', #213959, #135649, #92102, .T. ) ;
#70448 = CARTESIAN_POINT ( 'NONE',  ( -1.313174662617411670, 8.310476012147654856, 10.86148356754324595 ) ) ;
#70449 = CARTESIAN_POINT ( 'NONE',  ( -4.785408264436112447, 4.881506149194969169, -0.5627276081983053624 ) ) ;
#70450 = CARTESIAN_POINT ( 'NONE',  ( 6.182287216677275765, 1.039997956529638889, 1.731187096421077376 ) ) ;
#70452 = ORIENTED_EDGE ( 'NONE', *, *, #35454, .F. ) ;
#70451 = CARTESIAN_POINT ( 'NONE',  ( 0.4695848928168535608, -1.793611485386744420, -1.130822890709509254 ) ) ;
#70453 = CARTESIAN_POINT ( 'NONE',  ( -5.250750630242457362, 9.347902511916677426, 0.000000000000000000 ) ) ;
#70454 = CARTESIAN_POINT ( 'NONE',  ( 5.412729640353754590, 7.337937218544611895, 1.599625672291267398 ) ) ;
#70455 = CARTESIAN_POINT ( 'NONE',  ( 5.190332118341006051, -2.045072267241864861, -0.2543341860123843334 ) ) ;
#70456 = CARTESIAN_POINT ( 'NONE',  ( 3.885388821667290493, -0.6351983117205138862, -1.913803978180687482 ) ) ;
#70457 = ORIENTED_EDGE ( 'NONE', *, *, #200070, .T. ) ;
#70458 = CARTESIAN_POINT ( 'NONE',  ( 10.62873463776380056, 11.29999999999999893, -3.200000000000001510 ) ) ;
#70459 = CARTESIAN_POINT ( 'NONE',  ( 4.715538499454675403, 4.395883092318884522, 1.214306433183764966E-14 ) ) ;
#70461 = ORIENTED_EDGE ( 'NONE', *, *, #154010, .T. ) ;
#70460 = CARTESIAN_POINT ( 'NONE',  ( -7.795011973214244883, 8.058878488363559356, 0.7998128361456341429 ) ) ;
#70462 = CARTESIAN_POINT ( 'NONE',  ( 5.141188686642438554, 7.897460914975725998, 1.230089993873971999 ) ) ;
#70463 = CARTESIAN_POINT ( 'NONE',  ( 4.358749857130030492, -0.7741967591250037417, 1.861731939633674893 ) ) ;
#70464 = CARTESIAN_POINT ( 'NONE',  ( 3.257574473681293270, 0.8286728953739975756, 1.644182576024610265 ) ) ;
#70465 = CARTESIAN_POINT ( 'NONE',  ( 5.765600714192121501, 7.067438534624141511, 2.440103264412639472 ) ) ;
#70466 = CARTESIAN_POINT ( 'NONE',  ( 2.350585845863040646, 2.307203942772034111, 0.05475910514858049749 ) ) ;
#70467 = CARTESIAN_POINT ( 'NONE',  ( 3.400062661977048428, 7.188766548940353829, -1.734723475976807094E-15 ) ) ;
#70468 = CARTESIAN_POINT ( 'NONE',  ( 4.499409293453607184, 1.733128992574247684, 1.291583502853070886 ) ) ;
#70469 = CARTESIAN_POINT ( 'NONE',  ( 7.690499447449630210, 9.995335326823163058, 1.599625672291281386 ) ) ;
#70471 = CARTESIAN_POINT ( 'NONE',  ( 2.764861550476094276, -0.1531697945360478985, -2.010801143277194392 ) ) ;
#70470 = CARTESIAN_POINT ( 'NONE',  ( 0.2396544122938427390, 1.936909983681795344, 0.1419545801408238772 ) ) ;
#70472 = CARTESIAN_POINT ( 'NONE',  ( -3.899941742225307539, 7.701682465904834629, 0.7998128361456341429 ) ) ;
#70473 = CARTESIAN_POINT ( 'NONE',  ( -9.342889098753607513, 14.55305243632841616, -7.460114340563301916 ) ) ;
#70474 = CARTESIAN_POINT ( 'NONE',  ( -4.568734577680888087, 6.353276312092901890, -1.443375672974051449 ) ) ;
#70475 = CARTESIAN_POINT ( 'NONE',  ( 1.797508989346347619, -0.6330400025267440833, 1.760413054629046625 ) ) ;
#70476 = EDGE_CURVE ( 'NONE', #103981, #15788, #204726, .T. ) ;
#70477 = CARTESIAN_POINT ( 'NONE',  ( 0.1925371440497048448, -0.4299567264692584212, -1.931277891087788579 ) ) ;
#70479 = CARTESIAN_POINT ( 'NONE',  ( -6.587282531393266360, 8.778525268082516320, 1.599625672291269396 ) ) ;
#70478 = CARTESIAN_POINT ( 'NONE',  ( -1.500000000000001332, -1.068749999317178290, 0.000000000000000000 ) ) ;
#70480 = CARTESIAN_POINT ( 'NONE',  ( 1.752831059180045115, 0.6944836804415283060, 2.094827981560241970 ) ) ;
#70481 = VERTEX_POINT ( 'NONE', #73687 ) ;
#70482 = CARTESIAN_POINT ( 'NONE',  ( 5.027376032568989572, 4.759693547618927489, 0.7998128361456341429 ) ) ;
#70483 = CARTESIAN_POINT ( 'NONE',  ( -4.843287188579803448, 6.673587691474970107, -1.599625672291256295 ) ) ;
#70484 = CARTESIAN_POINT ( 'NONE',  ( 11.88234649872613602, 13.75660782916751579, 0.9090484974825158160 ) ) ;
#70485 = CARTESIAN_POINT ( 'NONE',  ( 6.139525842074132100, -1.427670353879314957, -1.359795004109279004 ) ) ;
#70486 = CARTESIAN_POINT ( 'NONE',  ( 6.428381082836107652, 1.334599446741807638, -1.882477381066828936 ) ) ;
#70487 = CARTESIAN_POINT ( 'NONE',  ( 6.549252741683062595, 1.618575325784047392, -0.9183544947665848168 ) ) ;
#70488 = CARTESIAN_POINT ( 'NONE',  ( 4.188373618524662056, 1.107674127198258196, -1.739744320567500280 ) ) ;
#70489 = CARTESIAN_POINT ( 'NONE',  ( 5.124618876285529367, 7.962177208099690873, -1.082531754730549078 ) ) ;
#70490 = CARTESIAN_POINT ( 'NONE',  ( 5.505492895601038938, 8.580769590579979678, -1.199719254218452047 ) ) ;
#70491 = ORIENTED_EDGE ( 'NONE', *, *, #58107, .T. ) ;
#70492 = CARTESIAN_POINT ( 'NONE',  ( 8.283668667825342169, 9.726996869626816533, -1.082531754730543083 ) ) ;
#70493 = CARTESIAN_POINT ( 'NONE',  ( -0.6823417656249969321, 3.780208333674754506, -1.181850606188749264 ) ) ;
#70494 = CARTESIAN_POINT ( 'NONE',  ( -10.24908409314513236, 3.786466850380959759, -6.156910069284049492 ) ) ;
#70495 = CARTESIAN_POINT ( 'NONE',  ( 3.673896439178911066, 7.230036912443299713, 0.7216878364870317197 ) ) ;
#70496 = CARTESIAN_POINT ( 'NONE',  ( 0.2335667940002684184, 0.001055507091213009818, -2.153566573614831281 ) ) ;
#70498 = CARTESIAN_POINT ( 'NONE',  ( 5.073706409418358376, -1.018251046719556685, 1.533866337327425278 ) ) ;
#70497 = CARTESIAN_POINT ( 'NONE',  ( 9.603221262331027575, -9.439766061754880866, -0.1988025308400224733 ) ) ;
#70499 = CARTESIAN_POINT ( 'NONE',  ( -2.020417662918760016, 3.956598013261175772, 11.36521191596583336 ) ) ;
#70500 = CARTESIAN_POINT ( 'NONE',  ( 6.392587740394330531, -6.532648833121157850, 6.999862025036990509 ) ) ;
#70501 = CARTESIAN_POINT ( 'NONE',  ( 0.5263522483448194178, 1.788089326329355577, 0.5492086291003297482 ) ) ;
#70502 = CARTESIAN_POINT ( 'NONE',  ( -4.612682051294048513, 7.132468998681293471, 1.371008595254997964 ) ) ;
#70503 = DIRECTION ( 'NONE',  ( 0.000000000000000000, 0.000000000000000000, 1.000000000000000000 ) ) ;
#70504 = CARTESIAN_POINT ( 'NONE',  ( 5.911136963822321455, 7.250628055112136039, -1.245581879728396846 ) ) ;
#70505 = CARTESIAN_POINT ( 'NONE',  ( 1.383307607624170155, 0.1396965592646744470, -1.907218110473147155 ) ) ;
#70506 = VECTOR ( 'NONE', #56718, 1000.000000000000000 ) ;
#70507 = CARTESIAN_POINT ( 'NONE',  ( 1.744620744215353625, -1.497317806218407599, 0.9432750629611782456 ) ) ;
#70508 = CARTESIAN_POINT ( 'NONE',  ( 6.633470333208185465, -0.1360683555875797923, 1.981904614263108266 ) ) ;
#70510 = CARTESIAN_POINT ( 'NONE',  ( 4.429236352518686637, -1.483253864829991775, -1.212251590588450112 ) ) ;
#70509 = CARTESIAN_POINT ( 'NONE',  ( -8.642432853707342488, 12.17025653171218558, 1.199719254218462483 ) ) ;
#70511 = CARTESIAN_POINT ( 'NONE',  ( 0.000000000000000000, -1.000000000000000888, 0.000000000000000000 ) ) ;
#70512 = CARTESIAN_POINT ( 'NONE',  ( 5.195741393986025969, -1.391442517743620710, -1.394189886649561227 ) ) ;
#70513 = CARTESIAN_POINT ( 'NONE',  ( 0.1586465271753433603, 2.115359532055087310, 0.1496401998123952359 ) ) ;
#70514 = CARTESIAN_POINT ( 'NONE',  ( -4.295235737431041478, 3.905529869957963029, -0.7998128361456221525 ) ) ;
#70515 = CARTESIAN_POINT ( 'NONE',  ( 4.469519713540137218, 1.814478506493342191, -0.4545110902946307152 ) ) ;
#70517 = ORIENTED_EDGE ( 'NONE', *, *, #202346, .F. ) ;
#70516 = CARTESIAN_POINT ( 'NONE',  ( 6.428329371266205072, 0.9864720512241608175, -1.414751289540659318 ) ) ;
#70519 = CARTESIAN_POINT ( 'NONE',  ( 3.768803514918948938, 4.459654191235965293, -1.082531754730543083 ) ) ;
#70518 = CARTESIAN_POINT ( 'NONE',  ( 4.020313978404310262, -1.133593497508533110, -1.893353337301090233 ) ) ;
#70520 = CARTESIAN_POINT ( 'NONE',  ( -1.364683531249997417, 3.071875000341423245, 1.214306433183764966E-14 ) ) ;
#70521 = CARTESIAN_POINT ( 'NONE',  ( 0.6079712386793578727, 0.6485803912554971573, -1.958102696269433673 ) ) ;
#70522 = CARTESIAN_POINT ( 'NONE',  ( 6.775324078527185989, 8.927630729746953264, -1.599625672291262513 ) ) ;
#70523 = CARTESIAN_POINT ( 'NONE',  ( -9.287498920561160887, 10.79416914786490089, -1.199719254218441611 ) ) ;
#70524 = CARTESIAN_POINT ( 'NONE',  ( -3.090415204605499344, 15.44821195424843019, -11.55764624973227228 ) ) ;
#70525 = CARTESIAN_POINT ( 'NONE',  ( 0.1747926744264668986, 7.629137130509083597, -2.455305974604498953 ) ) ;
#70526 = CARTESIAN_POINT ( 'NONE',  ( -5.384964389648357219, 7.561047897801473461, -1.247881146202101776 ) ) ;
#70527 = EDGE_LOOP ( 'NONE', ( #22245, #209205, #205261, #150083 ) ) ;
#70528 = CARTESIAN_POINT ( 'NONE',  ( 2.822784111170244525, -1.429543836668966561, 1.497820115680066344 ) ) ;
#70529 = CARTESIAN_POINT ( 'NONE',  ( -1.499999999999997780, 4.900000000000022560, 1.214306433183764966E-14 ) ) ;
#70530 = CARTESIAN_POINT ( 'NONE',  ( 4.364835388595708743, 7.179726155748598515, 1.199719254218462483 ) ) ;
#70531 = CARTESIAN_POINT ( 'NONE',  ( -6.458928793950097891, 6.861006557743732692, 0.6885227102202008398 ) ) ;
#70532 = CARTESIAN_POINT ( 'NONE',  ( 1.295575897195440307, 1.865243415117883385, -0.7750591016795584931 ) ) ;
#70533 = CARTESIAN_POINT ( 'NONE',  ( 1.436838838544731267, 7.449283400311756509, 4.203727439823562229 ) ) ;
#70534 = CARTESIAN_POINT ( 'NONE',  ( -1.364683531250010295, 4.030208333674751842, 0.7879004041258379498 ) ) ;
#70535 = ORIENTED_EDGE ( 'NONE', *, *, #101745, .F. ) ;
#70537 = CARTESIAN_POINT ( 'NONE',  ( 8.242994207428692377, 12.56065097540143327, -0.7216878364870328300 ) ) ;
#70536 = CARTESIAN_POINT ( 'NONE',  ( 0.07499057489260964326, 4.092262291754148684, -2.510514182268712702 ) ) ;
#70538 = CARTESIAN_POINT ( 'NONE',  ( 6.397814513887354337, 0.1948139983735352188, 2.006652364629394114 ) ) ;
#70539 = CARTESIAN_POINT ( 'NONE',  ( 6.403544266003773799, -1.856299428965903164, 0.4729442951737494183 ) ) ;
#70540 = FACE_BOUND ( 'NONE', #88471, .T. ) ;
#70541 = CARTESIAN_POINT ( 'NONE',  ( 3.245827600587628758, 2.191739723504753101, -0.002129563554123526260 ) ) ;
#70542 = CARTESIAN_POINT ( 'NONE',  ( -1.500000000000013101, 3.410416667349487785, -0.8660254037844313801 ) ) ;
#70543 = CARTESIAN_POINT ( 'NONE',  ( 2.777492966359981441, 0.2764497561681695803, -1.892163382976944419 ) ) ;
#70544 = CARTESIAN_POINT ( 'NONE',  ( -5.413783410558481002, 5.210502155273325720, -0.7998128361456221525 ) ) ;
#70545 = CARTESIAN_POINT ( 'NONE',  ( 3.009546912109283934, 6.454962464195385330, 0.000000000000000000 ) ) ;
#70547 = CARTESIAN_POINT ( 'NONE',  ( 1.458611474731505986, -1.915607644094442064, -0.6298556652749932594 ) ) ;
#70546 = CARTESIAN_POINT ( 'NONE',  ( 1.734723475976807094E-15, 14.99962766111844736, 11.68000013863625774 ) ) ;
#70548 = CARTESIAN_POINT ( 'NONE',  ( -1.364683531250000748, 10.92187500034139802, 0.000000000000000000 ) ) ;
#70550 = CARTESIAN_POINT ( 'NONE',  ( -5.387385936583832802, 7.378645907471495846, -1.599625672291271394 ) ) ;
#70549 = CARTESIAN_POINT ( 'NONE',  ( 6.444889499930222421, -1.758869480593090673, -1.307235502039267860 ) ) ;
#70552 = ORIENTED_EDGE ( 'NONE', *, *, #70219, .T. ) ;
#70551 = CARTESIAN_POINT ( 'NONE',  ( 3.328823242065849008, 0.04121275867331047893, 1.724443917160731976 ) ) ;
#70553 = CARTESIAN_POINT ( 'NONE',  ( 0.1399997263886003374, 7.629137130509076492, -2.599723212958489516 ) ) ;
#70554 = CARTESIAN_POINT ( 'NONE',  ( 8.308449207076147758, 8.587612251210650527, -0.7998128361456281477 ) ) ;
#70555 = CARTESIAN_POINT ( 'NONE',  ( 5.847644326195776010, 5.716673223516856694, -0.7998128361456281477 ) ) ;
#70556 = SURFACE_STYLE_FILL_AREA ( #21802 ) ;
#70557 = CARTESIAN_POINT ( 'NONE',  ( 1.012071980069819910, 1.959787197952606252, -0.09269708818125664551 ) ) ;
#70558 = CARTESIAN_POINT ( 'NONE',  ( -0.1236583036082171405, 1.000000000000000888, 11.99936284241579898 ) ) ;
#70559 = CARTESIAN_POINT ( 'NONE',  ( 4.005544317833563461, 6.760553239859419250, -1.199719254218452047 ) ) ;
#70560 = LINE ( 'NONE', #87912, #30061 ) ;
#70561 = ORIENTED_EDGE ( 'NONE', *, *, #109845, .F. ) ;
#70562 = EDGE_LOOP ( 'NONE', ( #6885, #92366, #120595, #163922 ) ) ;
#70563 = CARTESIAN_POINT ( 'NONE',  ( 4.213381321868588714, 1.457370398675205569, 1.075660112967236737 ) ) ;
#70564 = ORIENTED_EDGE ( 'NONE', *, *, #211272, .F. ) ;
#70565 = CARTESIAN_POINT ( 'NONE',  ( 7.879259827836241570, 12.34422023245099176, 1.040834085586084257E-14 ) ) ;
#70566 = CARTESIAN_POINT ( 'NONE',  ( 4.167152111353856547, 5.955039778036558040, 1.599625672291262513 ) ) ;
#70567 = CARTESIAN_POINT ( 'NONE',  ( 4.635318128526639825, -0.08385371298775616544, 1.809651570580686819 ) ) ;
#70568 = CARTESIAN_POINT ( 'NONE',  ( 6.658462837642789012, 9.821938173008357253, 1.082531754730549078 ) ) ;
#70569 = DIRECTION ( 'NONE',  ( 0.000000000000000000, 0.000000000000000000, 1.000000000000000000 ) ) ;
#70570 = CARTESIAN_POINT ( 'NONE',  ( 5.048403365090235795, 6.545034038527520082, -1.227034678662905609 ) ) ;
#70571 = EDGE_CURVE ( 'NONE', #92214, #69090, #3719, .T. ) ;
#70573 = CARTESIAN_POINT ( 'NONE',  ( 10.24048609702354717, 10.84165528948263457, -0.7998128361456281477 ) ) ;
#70572 = CARTESIAN_POINT ( 'NONE',  ( 5.318752605461887661, -1.348013374683079135, 1.283375817886179826 ) ) ;
#70574 = CARTESIAN_POINT ( 'NONE',  ( 3.198755040744692302, 1.733147561012362559, 0.8161988141396243623 ) ) ;
#70575 = AXIS2_PLACEMENT_3D ( 'NONE', #126739, #12881, #46481 ) ;
#70576 = CARTESIAN_POINT ( 'NONE',  ( -6.438543648255500962, 6.869506004301173085, 0.7833520578412848101 ) ) ;
#70577 = CARTESIAN_POINT ( 'NONE',  ( -5.761852096127856981, 5.824508321678349532, 0.000000000000000000 ) ) ;
#70578 = CARTESIAN_POINT ( 'NONE',  ( 0.7499999999999902300, 3.233333333333352044, 1.299038105676669330 ) ) ;
#70579 = DIRECTION ( 'NONE',  ( 1.276756478318932585E-15, -1.000000000000000000, 1.665334536937738262E-16 ) ) ;
#70580 = VECTOR ( 'NONE', #36443, 1000.000000000000000 ) ;
#70581 = CARTESIAN_POINT ( 'NONE',  ( 5.666945020832170776, 7.634521829102760115, 1.443375672974062551 ) ) ;
#70582 = CARTESIAN_POINT ( 'NONE',  ( -2.930533758848195447, 6.570706485298192234, -0.7998128361456281477 ) ) ;
#70583 = CYLINDRICAL_SURFACE ( 'NONE', #204205, 1.500000000000000222 ) ;
#70584 = CARTESIAN_POINT ( 'NONE',  ( -5.088052786878465739, 9.158088361325352977, 0.000000000000000000 ) ) ;
#70585 = ADVANCED_FACE ( 'NONE', ( #8680 ), #10700, .T. ) ;
#70586 = CARTESIAN_POINT ( 'NONE',  ( 1.289138792185164251, 1.584031432202914313, 1.364508995882382170 ) ) ;
#70587 = CARTESIAN_POINT ( 'NONE',  ( 4.667750024854814050, 8.667735138964429709, -0.7998128361456381397 ) ) ;
#70588 = CARTESIAN_POINT ( 'NONE',  ( 6.124042008734975617, -1.070608276503826950, -1.601302156493543905 ) ) ;
#70589 = CARTESIAN_POINT ( 'NONE',  ( -5.766295404513795297, 5.621766148221195358, 0.7998128361456341429 ) ) ;
#70590 = CARTESIAN_POINT ( 'NONE',  ( 2.783998052563033010, -0.9402290988879957734, 1.564698673013890984 ) ) ;
#70591 = CARTESIAN_POINT ( 'NONE',  ( 11.57394138716773213, 8.953477593029530723, 4.723522898263817993 ) ) ;
#70592 = CARTESIAN_POINT ( 'NONE',  ( 1.810667312839256304, -0.5133170510521027907, -1.842115474350584980 ) ) ;
#70593 = CARTESIAN_POINT ( 'NONE',  ( 2.049204468142644231, 1.715183525312633517, -0.9679544390571446222 ) ) ;
#70595 = B_SPLINE_CURVE_WITH_KNOTS ( 'NONE', 3,
 ( #86893, #54399, #51199, #167086, #183319, #200614 ),
 .UNSPECIFIED., .F., .F.,
 ( 4, 2, 4 ),
 ( 1.052505139324892547E-16, 0.002037829324722971718, 0.004075658649445837618 ),
 .UNSPECIFIED. ) ;
#70594 = CARTESIAN_POINT ( 'NONE',  ( 4.142085694530703854, 0.5209831505245207106, 1.870798910701749973 ) ) ;
#70596 = ORIENTED_EDGE ( 'NONE', *, *, #40853, .T. ) ;
#70597 = CARTESIAN_POINT ( 'NONE',  ( 1.284279953904121641, 3.284610286488902187, 0.7750000000000135669 ) ) ;
#70598 = CARTESIAN_POINT ( 'NONE',  ( -5.601453741101424022, 6.564059448486966986, -1.199719254218453823 ) ) ;
#70600 = CARTESIAN_POINT ( 'NONE',  ( 3.937823072884456099, -2.028283017459261650, 0.6187693826033290323 ) ) ;
#70599 = CARTESIAN_POINT ( 'NONE',  ( 5.273195401072370281, 5.116759154198018855, -0.7998128361456481317 ) ) ;
#70601 = CARTESIAN_POINT ( 'NONE',  ( 6.457408393014330450, -6.713678229394961505, 6.956254272497509383 ) ) ;
#70602 = CARTESIAN_POINT ( 'NONE',  ( 9.447334110624092673, 9.916311305349925220, -0.7998128361456281477 ) ) ;
#70603 = CARTESIAN_POINT ( 'NONE',  ( 6.108949960370312127, 6.019453914259918825, -0.1454340903971618193 ) ) ;
#70604 = SURFACE_SIDE_STYLE ('',( #105294 ) ) ;
#70605 = CARTESIAN_POINT ( 'NONE',  ( 5.040599249230596435, 9.102725900736217568, 0.7998128361456341429 ) ) ;
#70606 = CARTESIAN_POINT ( 'NONE',  ( -4.161989969715274462, 4.726297878971393196, -2.500000000000000444 ) ) ;
#70607 = CARTESIAN_POINT ( 'NONE',  ( 4.266095019097836172, 0.8626762044917112293, 1.609013669381313294 ) ) ;
#70608 = DIRECTION ( 'NONE',  ( 0.6507913734559640506, -0.7592566023653004592, 0.000000000000000000 ) ) ;
#70609 = CARTESIAN_POINT ( 'NONE',  ( -8.487040972474682476, 12.84537220128841817, 0.7216878364870338292 ) ) ;
#70610 = CARTESIAN_POINT ( 'NONE',  ( -4.618765760061220860, 8.456409177651165621, 0.3783674834792974950 ) ) ;
#70611 = DIRECTION ( 'NONE',  ( -1.000000000000000000, -3.451266460341926649E-31, 0.000000000000000000 ) ) ;
#70612 = CARTESIAN_POINT ( 'NONE',  ( 4.539837415608827698, 0.7997722286730184482, -1.691214532891088362 ) ) ;
#70613 = CARTESIAN_POINT ( 'NONE',  ( 6.265839547809997079, 10.46189657242035587, 0.7998128361456462443 ) ) ;
#70615 = ADVANCED_FACE ( 'NONE', ( #54247 ), #39061, .T. ) ;
#70614 = CARTESIAN_POINT ( 'NONE',  ( 1.875490933414716288, 1.843686865663298091, -0.5587569667290130937 ) ) ;
#70616 = CARTESIAN_POINT ( 'NONE',  ( 6.666857073735664052, 1.455856877570887109, -1.315125143065517532 ) ) ;
#70617 = CARTESIAN_POINT ( 'NONE',  ( -8.012344526598182026E-15, 8.859375000341405126, -1.575800808251669460 ) ) ;
#70618 = CARTESIAN_POINT ( 'NONE',  ( -5.713871673155502151, 8.753601821068331290, 1.199719254218452047 ) ) ;
#70619 = CARTESIAN_POINT ( 'NONE',  ( 5.281064527722868718, 6.119995689553514140, 1.199719254218462483 ) ) ;
#70620 = CARTESIAN_POINT ( 'NONE',  ( -4.462041952228944730, 7.259447140025469203, -1.082531754730549967 ) ) ;
#70621 =( BOUNDED_CURVE ( )  B_SPLINE_CURVE ( 2, ( #135946, #200902, #18965, #85049, #88257, #2703, #102365 ),
 .UNSPECIFIED., .F., .T. ) 
 B_SPLINE_CURVE_WITH_KNOTS ( ( 3, 2, 2, 3 ),
 ( 0.2678571428571428492, 0.2738095238095239470, 0.2797619047619049337, 0.2857142857142859760 ),
 .UNSPECIFIED. ) 
 CURVE ( )  GEOMETRIC_REPRESENTATION_ITEM ( )  RATIONAL_B_SPLINE_CURVE ( ( 1.000000000000000000, 0.8660254037844387076, 1.000000000000000000, 0.8660254037844387076, 1.000000000000000000, 0.8660254037844324904, 1.000000000000006217 ) ) 
 REPRESENTATION_ITEM ( '' )  );
#70622 = CARTESIAN_POINT ( 'NONE',  ( 1.634521315757204940, 0.6676430208681031209, 2.009258352967583150 ) ) ;
#70623 = VECTOR ( 'NONE', #197970, 1000.000000000000000 ) ;
#70624 = CARTESIAN_POINT ( 'NONE',  ( 9.836604141914616406, 11.43479190611061647, 1.199719254218452047 ) ) ;
#70626 = EDGE_CURVE ( 'NONE', #102463, #28948, #205366, .T. ) ;
#70625 = CARTESIAN_POINT ( 'NONE',  ( -1.802380875475197541, 2.439898602870748778, 2.460315029152825961 ) ) ;
#70627 = CARTESIAN_POINT ( 'NONE',  ( 5.418829850390409320, -1.503349927839289002, 1.423607673449282851 ) ) ;
#70629 = CARTESIAN_POINT ( 'NONE',  ( 4.001130546182508851, 7.826233022050814725, 0.1222016466962717873 ) ) ;
#70628 = CARTESIAN_POINT ( 'NONE',  ( 0.3625324912872701089, 0.1813134127766780901, -1.832273687604975665 ) ) ;
#70630 = CARTESIAN_POINT ( 'NONE',  ( 6.205746375452622310, 2.143286971341977765, 0.8312943217957665665 ) ) ;
#70631 = CARTESIAN_POINT ( 'NONE',  ( 6.155038550924155416, 6.283225852274053835, 0.7216878364870317197 ) ) ;
#70633 =( NAMED_UNIT ( * ) SI_UNIT ( $, .STERADIAN. ) SOLID_ANGLE_UNIT ( ) );
#70632 = CARTESIAN_POINT ( 'NONE',  ( 5.234856708652235291, 5.279956712948652431, 0.7216878364870338292 ) ) ;
#70634 = CARTESIAN_POINT ( 'NONE',  ( 1.676131343691760645, -1.223425685817343789, 1.938311714834321631 ) ) ;
#70635 = DIRECTION ( 'NONE',  ( 0.000000000000000000, -1.000000000000000000, 0.000000000000000000 ) ) ;
#70636 = CARTESIAN_POINT ( 'NONE',  ( -6.459533842268148973, 6.500820668926428958, 0.000000000000000000 ) ) ;
#70637 = CARTESIAN_POINT ( 'NONE',  ( 6.281195871053392388, 1.340900550492612364, 1.404911987746715774 ) ) ;
#70638 = ORIENTED_EDGE ( 'NONE', *, *, #73270, .F. ) ;
#70639 = CARTESIAN_POINT ( 'NONE',  ( 8.473482818416664841, 10.90881592628469932, -1.443375672974063439 ) ) ;
#70640 = EDGE_LOOP ( 'NONE', ( #170498, #171264, #74068, #81768 ) ) ;
#70641 = CARTESIAN_POINT ( 'NONE',  ( 6.469012471580376733, -1.473683540339595810, 1.218514635347216046 ) ) ;
#70642 = CARTESIAN_POINT ( 'NONE',  ( -4.955918092712652268, 4.886086657537050293, 0.4932186882876873901 ) ) ;
#70644 = CARTESIAN_POINT ( 'NONE',  ( -1.349890321011286476, 8.200329036966257590, -10.79298809153609540 ) ) ;
#70643 = CARTESIAN_POINT ( 'NONE',  ( -8.259941899223614215, 10.65968485389279508, -1.599625672291263179 ) ) ;
#70645 = CARTESIAN_POINT ( 'NONE',  ( -3.285556943750000514, -0.2260416661887102996, -1.896917185911906500 ) ) ;
#70647 = CARTESIAN_POINT ( 'NONE',  ( 1.164531557977426912, -1.597865870565655877, -0.7613500884297589311 ) ) ;
#70646 = CARTESIAN_POINT ( 'NONE',  ( 2.783241352837596327, 1.478939484563842610, 1.477931775543766202 ) ) ;
#70648 = CARTESIAN_POINT ( 'NONE',  ( 6.539686446881147752, -1.556848207870220602, 1.281141925495055123 ) ) ;
#70650 = CARTESIAN_POINT ( 'NONE',  ( 4.400488903878751579, 1.773513045242902209, -1.452268937634313417 ) ) ;
#70649 = CARTESIAN_POINT ( 'NONE',  ( 5.110497557708379546, 4.926945003606695295, -0.7998128361456481317 ) ) ;
#70651 = CARTESIAN_POINT ( 'NONE',  ( 3.362975788648288944, 1.697558991927169192, -0.3826393865087075463 ) ) ;
#70652 = B_SPLINE_CURVE_WITH_KNOTS ( 'NONE', 3,
 ( #129027, #196081, #126895, #46636, #30383, #96469, #80181, #31447, #97525, #142027, #143103, #208041, #109569, #175573 ),
 .UNSPECIFIED., .F., .F.,
 ( 4, 2, 2, 2, 2, 2, 4 ),
 ( 0.000000000000000000, 0.0006738968695872706808, 0.001010845304380905913, 0.001347793739174541362, 0.001684742173968175943, 0.002021690608761810524, 0.002695587478349080121 ),
 .UNSPECIFIED. ) ;
#70653 = CARTESIAN_POINT ( 'NONE',  ( 4.539282502477016479, 4.190251095844947926, 0.7998128361456341429 ) ) ;
#70654 = CARTESIAN_POINT ( 'NONE',  ( 0.000000000000000000, 0.000000000000000000, -1.500000000000000222 ) ) ;
#70655 = CARTESIAN_POINT ( 'NONE',  ( 2.952174690553764691, 1.223825555390768871, 1.228469256970601498 ) ) ;
#70656 = CARTESIAN_POINT ( 'NONE',  ( 3.438082271139299539, 1.374976351402785513, 1.680335591205921908 ) ) ;
#70657 = CARTESIAN_POINT ( 'NONE',  ( 4.253507506385319381, 5.985511395581417204, 1.599625672291267398 ) ) ;
#70658 = CARTESIAN_POINT ( 'NONE',  ( 4.821500071095637274, -1.429446227384461032, -1.422610148874188463 ) ) ;
#70659 = CARTESIAN_POINT ( 'NONE',  ( 1.531250000000001110, -0.7852924748300684765, -1.895863743164053927 ) ) ;
#70660 = CARTESIAN_POINT ( 'NONE',  ( 0.7499999999999902300, 2.264583334016148530, 1.299038105676669330 ) ) ;
#70661 = CARTESIAN_POINT ( 'NONE',  ( 1.149297380808786517, -1.516923518071541910, -1.187294353726556562 ) ) ;
#70662 = CARTESIAN_POINT ( 'NONE',  ( -1.500000000000001110, 8.802083334016133520, 0.8660254037844419273 ) ) ;
#70663 = CARTESIAN_POINT ( 'NONE',  ( 4.008219027074312990, -0.8479933951243652235, 2.053374474559205520 ) ) ;
#70664 = ORIENTED_EDGE ( 'NONE', *, *, #19949, .F. ) ;
#70665 = CARTESIAN_POINT ( 'NONE',  ( -0.2108831679770960255, -0.001785917861228669690, -1.896958272444612792 ) ) ;
#70666 = CARTESIAN_POINT ( 'NONE',  ( -0.7500000000000006661, 1.608333333333357373, -1.299038105676652011 ) ) ;
#70667 = CARTESIAN_POINT ( 'NONE',  ( 6.425674737872927089, 9.584038729905381970, -1.199719254218440723 ) ) ;
#70668 = CARTESIAN_POINT ( 'NONE',  ( 3.836594282542902246, 7.419851063034623273, 0.7216878364870317197 ) ) ;
#70669 = CARTESIAN_POINT ( 'NONE',  ( 5.355107487717867265, 5.349972945200037522, 1.040834085586084257E-14 ) ) ;
#70670 = CARTESIAN_POINT ( 'NONE',  ( 0.2061412868327249515, 1.650399489264813502, 1.486927644236696766 ) ) ;
#70671 = CARTESIAN_POINT ( 'NONE',  ( 5.617619635959271385, 0.3843197845415853853, -1.923678648292715732 ) ) ;
#70672 = CARTESIAN_POINT ( 'NONE',  ( 10.38518247838791986, 11.21839376764850726, 0.7216878364870438212 ) ) ;
#70673 = CARTESIAN_POINT ( 'NONE',  ( -0.1033001855874529917, 3.400480225852400729, 1.999524373000333144 ) ) ;
#70674 = CARTESIAN_POINT ( 'NONE',  ( 6.520815820410102326, 2.107438871474434983, 0.8233813407293107955 ) ) ;
#70675 = CLOSED_SHELL ( 'NONE', ( #79519, #91112, #203731, #183898, #23463, #194422, #169621, #213186 ) ) ;
#70676 = CARTESIAN_POINT ( 'NONE',  ( -6.143253000767895600, 6.339752387083549934, 0.000000000000000000 ) ) ;
#70677 = CARTESIAN_POINT ( 'NONE',  ( 3.666515279890161239, -0.8333913613888814798, -1.886988505759807921 ) ) ;
#70678 = CARTESIAN_POINT ( 'NONE',  ( -4.554649539187067830, 7.401175998105142817, 1.199719254218464037 ) ) ;
#70679 = CARTESIAN_POINT ( 'NONE',  ( 1.499999999999989120, 4.535416667349484676, 0.8660254037844524744 ) ) ;
#70680 = CARTESIAN_POINT ( 'NONE',  ( 1.364683531249988535, 4.967708333674756283, -0.7879004041258300672 ) ) ;
#70681 = CARTESIAN_POINT ( 'NONE',  ( 5.132044594934622062, 0.9627672477196843603, -1.603626212978970900 ) ) ;
#70682 = CARTESIAN_POINT ( 'NONE',  ( 3.902719751800659775, -0.8955246652143248332, -1.484863070527132622 ) ) ;
#70683 = CARTESIAN_POINT ( 'NONE',  ( 3.175097308692858444, 1.106666961078702771, 1.343256515094106041 ) ) ;
#70684 = CARTESIAN_POINT ( 'NONE',  ( 0.5391474206018737059, -1.962199071191613964, 1.185045521927590162 ) ) ;
#70685 = CARTESIAN_POINT ( 'NONE',  ( -1.364683531250012516, 3.342708333674756727, 0.7879004041258379498 ) ) ;
#70686 = CARTESIAN_POINT ( 'NONE',  ( 4.230081496780574213, 2.050754116127400106, 0.4060544076584340356 ) ) ;
#70687 = CARTESIAN_POINT ( 'NONE',  ( 0.2164228883963260908, -0.09351453081237262599, 1.838880455306932227 ) ) ;
#70688 = CARTESIAN_POINT ( 'NONE',  ( 0.09999999999990051569, -10.00000000000009592, 10.91954211494245008 ) ) ;
#70689 = CARTESIAN_POINT ( 'NONE',  ( 1.195935645703485539, 1.779627574718087635, 0.9480385367472210500 ) ) ;
#70690 = CARTESIAN_POINT ( 'NONE',  ( 0.1643758432304382178, -1.428106194732338352, 1.662303017507735570 ) ) ;
#70691 = FACE_OUTER_BOUND ( 'NONE', #77394, .T. ) ;
#70692 = CARTESIAN_POINT ( 'NONE',  ( -8.525379664894808585, 8.840697785332414682, -0.7998128361456291469 ) ) ;
#70693 = CARTESIAN_POINT ( 'NONE',  ( 6.226218857173709154, 8.287007971501239467, 1.599625672291281386 ) ) ;
#70694 = CARTESIAN_POINT ( 'NONE',  ( 2.297662419472700002, 1.937625723843895864, -0.8618613456389671024 ) ) ;
#70695 = CARTESIAN_POINT ( 'NONE',  ( 5.988856447087389512, -0.2726756491404982441, -1.805090154579996442 ) ) ;
#70696 = VERTEX_POINT ( 'NONE', #61708 ) ;
#70697 = CARTESIAN_POINT ( 'NONE',  ( -6.740338644649361832, 7.892758502626242567, -1.199719254218452047 ) ) ;
#70698 = EDGE_CURVE ( 'NONE', #35130, #124966, #76428, .T. ) ;
#70699 = CARTESIAN_POINT ( 'NONE',  ( -4.907068755522976389, 4.827261090972641000, -0.03298405530800324614 ) ) ;
#70700 = CARTESIAN_POINT ( 'NONE',  ( 0.000000000000000000, -1.334374999522042859, -3.793834371823813001 ) ) ;
#70701 = CARTESIAN_POINT ( 'NONE',  ( -8.355902744723985975, 8.642974711799791265, 1.040834085586084257E-14 ) ) ;
#70702 = CARTESIAN_POINT ( 'NONE',  ( 1.758075477673838982, 0.7690763710625804217, -1.867840884567156357 ) ) ;
#70703 = CARTESIAN_POINT ( 'NONE',  ( 6.651417122894856426, -1.768357563224710605, -1.319949637914811458 ) ) ;
#70704 = CARTESIAN_POINT ( 'NONE',  ( 8.866142388332804103, 12.43125098877526113, -1.199719254218446718 ) ) ;
#70705 = CARTESIAN_POINT ( 'NONE',  ( 4.487043221128726778, 0.08799343497551150028, 1.858965402599630723 ) ) ;
#70706 = CARTESIAN_POINT ( 'NONE',  ( 9.565441069641300587, 11.11843498845840905, -1.199719254218440723 ) ) ;
#70707 = CARTESIAN_POINT ( 'NONE',  ( 11.92619526913699701, 13.40000000000000036, -1.328859060402686199 ) ) ;
#70708 = ORIENTED_EDGE ( 'NONE', *, *, #178139, .T. ) ;
#70709 = CARTESIAN_POINT ( 'NONE',  ( -5.766295404513795297, 5.621766148221195358, 0.7998128361456341429 ) ) ;
#70710 =( BOUNDED_CURVE ( )  B_SPLINE_CURVE ( 3, ( #172357, #156110, #41307, #56468 ),
 .UNSPECIFIED., .F., .T. ) 
 B_SPLINE_CURVE_WITH_KNOTS ( ( 4, 4 ),
 ( 0.4999999999999993894, 1.000000000000000000 ),
 .UNSPECIFIED. ) 
 CURVE ( )  GEOMETRIC_REPRESENTATION_ITEM ( )  RATIONAL_B_SPLINE_CURVE ( ( 1.000000000000000888, 0.3333333333333334259, 0.3333333333333325932, 1.000000000000000000 ) ) 
 REPRESENTATION_ITEM ( '' )  );
#70711 = CARTESIAN_POINT ( 'NONE',  ( -6.997979842947967377, 11.31606025008131233, -0.7998128361456291469 ) ) ;
#70712 = CARTESIAN_POINT ( 'NONE',  ( 5.215394836314163562, -0.2642288504575221464, 1.806346989861665087 ) ) ;
#70714 = CARTESIAN_POINT ( 'NONE',  ( -4.172464037091858202, 7.595707080679858336, -0.9154354581521230161 ) ) ;
#70713 = CARTESIAN_POINT ( 'NONE',  ( -2.979759899953417612, 6.698413326579433225, 0.7998128361456352531 ) ) ;
#70715 = CARTESIAN_POINT ( 'NONE',  ( 5.092389439195339484, 7.944299729584391123, -1.199137415704543130 ) ) ;
#70716 = CARTESIAN_POINT ( 'NONE',  ( 1.967715241700284556, 1.438441333088829266, 0.9676545092154006378 ) ) ;
#70717 = CARTESIAN_POINT ( 'NONE',  ( 6.474545096729185545, -0.09562278402284159207, -1.838781726270556804 ) ) ;
#70718 = CARTESIAN_POINT ( 'NONE',  ( 5.004635055918612352, -0.7736033420917761694, -2.174287598079288841 ) ) ;
#70719 = CARTESIAN_POINT ( 'NONE',  ( 3.067887898442204442, 6.801229324816399746, 0.7998128361456271485 ) ) ;
#70720 = CARTESIAN_POINT ( 'NONE',  ( 1.686866501761717263, -0.2992900534812113489, -2.038785687196064789 ) ) ;
#70721 = CARTESIAN_POINT ( 'NONE',  ( 6.331821432781979730, 7.345878745455822312, -1.199719254218445830 ) ) ;
#70722 = CARTESIAN_POINT ( 'NONE',  ( 0.2982036909132765867, -1.844429998007334648, 0.8144978490535054183 ) ) ;
#70723 = CARTESIAN_POINT ( 'NONE',  ( 0.000000000000000000, -0.5000000000000004441, 0.000000000000000000 ) ) ;
#70725 = CIRCLE ( 'NONE', #105422, 11.99999999999999112 ) ;
#70724 = CARTESIAN_POINT ( 'NONE',  ( -5.074494633264801990, 9.142270515442742607, 0.7998128361456291469 ) ) ;
#70726 = CARTESIAN_POINT ( 'NONE',  ( 5.998880656844745474, 1.528293836345222312, -1.078463600801618405 ) ) ;
#70727 = TOROIDAL_SURFACE ( 'NONE', #191810, 4.899999999999999467, 0.4000000000000000222 ) ;
#70729 = CARTESIAN_POINT ( 'NONE',  ( -3.637330350216213759, 7.465578851886037093, -0.7998128361456481317 ) ) ;
#70728 = CARTESIAN_POINT ( 'NONE',  ( 3.621269620730773298, 1.642686141288721480, 0.9789267784374030557 ) ) ;
#70730 = CARTESIAN_POINT ( 'NONE',  ( 5.338574060078519423, 2.173733305800494175, 0.3801736985692484305 ) ) ;
#70731 = CARTESIAN_POINT ( 'NONE',  ( -1.225000000000006084, 2.041666667349461672, -0.7072540797572977045 ) ) ;
#70732 = CARTESIAN_POINT ( 'NONE',  ( 6.061904079085887354, 6.244845311787889486, 0.000000000000000000 ) ) ;
#70733 = CARTESIAN_POINT ( 'NONE',  ( 4.055297343818933697, 5.824542549245813383, 1.443375672974058777 ) ) ;
#70734 = CARTESIAN_POINT ( 'NONE',  ( -5.275531169048909952, 7.248148678680751189, -1.443375672974066548 ) ) ;
#70735 = CARTESIAN_POINT ( 'NONE',  ( 6.270199134133584096, 2.114857618286110075, -0.1555134818699496213 ) ) ;
#70736 = ORIENTED_EDGE ( 'NONE', *, *, #85807, .F. ) ;
#70737 = EDGE_CURVE ( 'NONE', #157709, #64278, #63048, .T. ) ;
#70738 = CARTESIAN_POINT ( 'NONE',  ( 3.575485986712009456, 0.05928947047922557279, -2.306987226281012049 ) ) ;
#70739 = CARTESIAN_POINT ( 'NONE',  ( 3.824618516750320385, -1.319357783791510697, 1.452116237791359010 ) ) ;
#70740 = CARTESIAN_POINT ( 'NONE',  ( 7.487360338304411833, -6.465328379374277290, 7.487360338304385188 ) ) ;
#70741 = CARTESIAN_POINT ( 'NONE',  ( 0.3386216902839487841, -1.901412053528793722, -0.4823507731460881520 ) ) ;
#70742 = CARTESIAN_POINT ( 'NONE',  ( 2.738383840280328663, 5.178236332760252303, 1.082531754730548412 ) ) ;
#70743 = CARTESIAN_POINT ( 'NONE',  ( -11.92619526913699524, 13.52780024161488370, 1.328859060402684866 ) ) ;
#70744 = ORIENTED_EDGE ( 'NONE', *, *, #66045, .F. ) ;
#70745 = CARTESIAN_POINT ( 'NONE',  ( 6.227749967195368441, 0.7672974224810541477, -1.865044430435198741 ) ) ;
#70746 = CARTESIAN_POINT ( 'NONE',  ( -8.483651433849100698, 10.92067931095586886, 1.599625672291269396 ) ) ;
#70748 = CARTESIAN_POINT ( 'NONE',  ( 0.1461044202776436429, -1.480667811789614818, 1.094048858351577724 ) ) ;
#70747 = AXIS2_PLACEMENT_3D ( 'NONE', #109621, #129084, #61859 ) ;
#70749 = CARTESIAN_POINT ( 'NONE',  ( 2.782273231148081116, -1.246650745954593464, -1.777310168556520464 ) ) ;
#70750 = CARTESIAN_POINT ( 'NONE',  ( 5.499767588998890844, 6.445425604367387429, 1.199719254218451159 ) ) ;
#70751 = CARTESIAN_POINT ( 'NONE',  ( 0.3871773095200456982, -1.998849835692744659, -0.7086421328065874992 ) ) ;
#70752 = CARTESIAN_POINT ( 'NONE',  ( -1.499999999999997780, 1.931250000682817269, 0.000000000000000000 ) ) ;
#70753 = CARTESIAN_POINT ( 'NONE',  ( 10.22692794340986921, 10.82583744360002243, 0.000000000000000000 ) ) ;
#70754 = CARTESIAN_POINT ( 'NONE',  ( 11.86239285000045740, 13.88000000000000078, -1.812080536912752837 ) ) ;
#70755 = CARTESIAN_POINT ( 'NONE',  ( 6.148788998471866662, 7.076870205577955986, 1.084632487400632339 ) ) ;
#70756 = CARTESIAN_POINT ( 'NONE',  ( 0.8431279278494309137, -1.768909939683245058, 1.056965710194081920 ) ) ;
#70758 = CARTESIAN_POINT ( 'NONE',  ( 6.727182134110201162, 0.003007720480356981373, 1.910970182385363092 ) ) ;
#70757 = CARTESIAN_POINT ( 'NONE',  ( -10.15522075183580419, 11.80651128435196462, 1.199719254218462483 ) ) ;
#70759 = CARTESIAN_POINT ( 'NONE',  ( -1.402160292154681736E-14, 1.446875000341420137, -1.575800808251659024 ) ) ;
#70760 = CARTESIAN_POINT ( 'NONE',  ( 7.204675194429079505E-15, -1.137499999999999512, -3.475000000000000089 ) ) ;
#70761 = ORIENTED_EDGE ( 'NONE', *, *, #80621, .F. ) ;
#70762 = CARTESIAN_POINT ( 'NONE',  ( 4.072844535355981677, -1.414876986328793329, 1.286614418101794444 ) ) ;
#70763 = CARTESIAN_POINT ( 'NONE',  ( 5.013482942003290255, 9.071090208970993274, -0.7998128361456481317 ) ) ;
#70764 = CARTESIAN_POINT ( 'NONE',  ( -8.487040972474682476, 12.84537220128841817, 0.7216878364870338292 ) ) ;
#70765 = CARTESIAN_POINT ( 'NONE',  ( 0.4569037783100584060, -1.553534471429316666, 0.9316326570649158256 ) ) ;
#70767 = CARTESIAN_POINT ( 'NONE',  ( 0.6025738811294746311, 1.771267034891465642, 0.7302799438476501592 ) ) ;
#70766 = CARTESIAN_POINT ( 'NONE',  ( -6.777910281175750562, -7.189645481333823085, 6.776323679500811714 ) ) ;
#70768 = CARTESIAN_POINT ( 'NONE',  ( 1.557173632797459684, 1.693725193156172315, -1.190412882225246438 ) ) ;
#70769 = CARTESIAN_POINT ( 'NONE',  ( -1.402160292154681736E-14, 0.5093750003414236893, -1.575800808251659024 ) ) ;
#70770 = CARTESIAN_POINT ( 'NONE',  ( 0.4089732319989903275, 1.714023354001862787, 0.9739579164984181192 ) ) ;
#70771 = CARTESIAN_POINT ( 'NONE',  ( 2.930095790256614485, 1.013914413367119627, -1.518051517300327502 ) ) ;
#70772 = EDGE_CURVE ( 'NONE', #123959, #166540, #207944, .T. ) ;
#70774 = CARTESIAN_POINT ( 'NONE',  ( 6.426609430950597890, 6.789993649951097332, 0.4362094596595481599 ) ) ;
#70773 = CARTESIAN_POINT ( 'NONE',  ( 0.1359762249627448627, -2.107041879058098033, 0.9415998322012062438 ) ) ;
#70775 = CARTESIAN_POINT ( 'NONE',  ( 1.364683531249986537, 0.6552083336747522857, -0.7879004041258239610 ) ) ;
#70776 = CARTESIAN_POINT ( 'NONE',  ( 4.105966297347532823, 0.6976637339557908435, -1.941222516249243579 ) ) ;
#70777 = CARTESIAN_POINT ( 'NONE',  ( -5.713871673155502151, 8.753601821068331290, 1.199719254218452047 ) ) ;
#70778 = CARTESIAN_POINT ( 'NONE',  ( 6.564118927310645724, 10.80988918183778225, -0.7998128361456291469 ) ) ;
#70779 = CARTESIAN_POINT ( 'NONE',  ( 5.192936529234042808, 6.017179691316550283, -1.199719254218452047 ) ) ;
#70780 = CARTESIAN_POINT ( 'NONE',  ( 5.575427483717746213, 7.527751369135936343, 1.599625672291267398 ) ) ;
#70783 = CARTESIAN_POINT ( 'NONE',  ( 0.7499999999999885647, 3.316666666666689967, -1.299038105676658228 ) ) ;
#70782 = MECHANICAL_DESIGN_GEOMETRIC_PRESENTATION_REPRESENTATION (  '', ( #198792 ), #195290 ) ;
#70781 = CARTESIAN_POINT ( 'NONE',  ( 5.016683434392706253, 1.454383057171860116, -1.523333715015115608 ) ) ;
#70784 = CARTESIAN_POINT ( 'NONE',  ( 6.707487347292075519, -1.660346423639452951, -1.236579608897829363 ) ) ;
#70785 = CARTESIAN_POINT ( 'NONE',  ( 0.6823417656249899377, 1.155208333674752286, 1.181850606188755259 ) ) ;
#70786 = CARTESIAN_POINT ( 'NONE',  ( 3.216266648612066792, -1.062311135343798618, -1.882447817163131587 ) ) ;
#70787 = CARTESIAN_POINT ( 'NONE',  ( 4.635418745873795210, -0.09682320349532060055, 2.017468490573450346 ) ) ;
#70788 =( LENGTH_UNIT ( ) NAMED_UNIT ( * ) SI_UNIT ( .MILLI., .METRE. ) );
#70789 = CIRCLE ( 'NONE', #84577, 3.970406073902761790 ) ;
#70792 = CARTESIAN_POINT ( 'NONE',  ( 5.016153647376201619, 7.835634441038803466, 1.082531754730558626 ) ) ;
#70791 = CARTESIAN_POINT ( 'NONE',  ( 1.642778471875000035, -3.726041666188707691, -2.845375778867859751 ) ) ;
#70790 = DIRECTION ( 'NONE',  ( 1.000000000000000000, 0.000000000000000000, 0.000000000000000000 ) ) ;
#70793 = CARTESIAN_POINT ( 'NONE',  ( -6.479871072688648148, 6.524547437750345402, 0.000000000000000000 ) ) ;
#70794 = CARTESIAN_POINT ( 'NONE',  ( 2.923064838257955156, -1.776166165677966591, 0.9548571111624851726 ) ) ;
#70795 = CARTESIAN_POINT ( 'NONE',  ( -9.176171038350775078, 9.599954387697719582, -0.7998128361456291469 ) ) ;
#70797 = LINE ( 'NONE', #136910, #91710 ) ;
#70796 = CARTESIAN_POINT ( 'NONE',  ( -2.930533758848195447, 6.570706485298192234, -0.7998128361456281477 ) ) ;
#70798 = CARTESIAN_POINT ( 'NONE',  ( 1.499999999999990896, 8.627523663848661428, 2.580000000000000515 ) ) ;
#70799 = CARTESIAN_POINT ( 'NONE',  ( 5.607647405131535479, 1.452367144367059826, 1.244281684088063944 ) ) ;
#70800 = CARTESIAN_POINT ( 'NONE',  ( 6.720655732516665815, 3.683894443391816154, 2.687682123607849416 ) ) ;
#70802 = CARTESIAN_POINT ( 'NONE',  ( 4.271111354109316416, 1.799915745204151429, -0.9091612155255476280 ) ) ;
#70801 = CARTESIAN_POINT ( 'NONE',  ( -7.497295758232720431, 10.73030023703809555, -1.082531754730543083 ) ) ;
#70803 = CARTESIAN_POINT ( 'NONE',  ( 1.499999999999987121, 4.545833333333352932, -0.8660254037844323793 ) ) ;
#70804 = CARTESIAN_POINT ( 'NONE',  ( 1.364683531249996529, 15.27604166700806587, 0.7879004041258405033 ) ) ;
#70805 = CARTESIAN_POINT ( 'NONE',  ( 6.036138234293757954, 0.8456279901550376454, -1.503183349252550371 ) ) ;
#70806 = CARTESIAN_POINT ( 'NONE',  ( 5.875479466675786355, 7.948088359245467416, -1.599625672291283607 ) ) ;
#70808 = CARTESIAN_POINT ( 'NONE',  ( 1.637338291174485510E-15, -6.530144695498204754, 11.00000000000000178 ) ) ;
#70807 = CARTESIAN_POINT ( 'NONE',  ( 9.747949258545622442, 10.47495501116581984, 0.000000000000000000 ) ) ;
#70809 = LINE ( 'NONE', #50330, #12487 ) ;
#70810 = CARTESIAN_POINT ( 'NONE',  ( 5.096879011283717453, 1.555924861325823416, -1.037969726935553005 ) ) ;
#70811 = CARTESIAN_POINT ( 'NONE',  ( 0.02993902094421736770, -1.973830418800892161, 0.3948085296872869687 ) ) ;
#70812 = DIRECTION ( 'NONE',  ( 0.000000000000000000, 1.000000000000000000, 0.000000000000000000 ) ) ;
#70813 = CARTESIAN_POINT ( 'NONE',  ( -7.146556367734805626, 9.431011410480991231, 1.443375672974064550 ) ) ;
#70814 = VERTEX_POINT ( 'NONE', #94235 ) ;
#70815 = CARTESIAN_POINT ( 'NONE',  ( 0.9312678054614745848, -1.591333336790928366, -1.238303555203337680 ) ) ;
#70816 = CARTESIAN_POINT ( 'NONE',  ( 0.8788404743438563704, -1.638286771785288254, -0.7734350870383081000 ) ) ;
#70817 = EDGE_CURVE ( 'NONE', #66793, #9078, #124918, .T. ) ;
#70818 = CARTESIAN_POINT ( 'NONE',  ( 4.543390873910906791, 6.393985001019784953, 1.443375672974065660 ) ) ;
#70819 = CARTESIAN_POINT ( 'NONE',  ( 5.607077132713799372, 5.680974216569005364, -0.2743783134233104826 ) ) ;
#70820 = CARTESIAN_POINT ( 'NONE',  ( 7.063434842595398777, 11.18449838309590483, -0.7216878364870267237 ) ) ;
#70821 = CARTESIAN_POINT ( 'NONE',  ( 5.937581207780954884, 9.014596278131406848, -1.199719254218440723 ) ) ;
#70823 = CARTESIAN_POINT ( 'NONE',  ( 5.782812685692425347, 1.563071972524389786, -1.107110302061852236 ) ) ;
#70822 = CARTESIAN_POINT ( 'NONE',  ( -5.253948220495577637, 6.088359997788290734, 1.199719254218450271 ) ) ;
#70824 = CARTESIAN_POINT ( 'NONE',  ( -11.97929049433705373, 9.719999999999998863, -0.7046979865771834106 ) ) ;
#70825 = FACE_OUTER_BOUND ( 'NONE', #165371, .T. ) ;
#70826 = CARTESIAN_POINT ( 'NONE',  ( 0.6823417656249864960, -0.5114583329919111243, -1.181850606188749264 ) ) ;
#70828 = ORIENTED_EDGE ( 'NONE', *, *, #95161, .T. ) ;
#70827 = CARTESIAN_POINT ( 'NONE',  ( 4.392478581147586603, 4.226905887534702977, -0.7216878364870188411 ) ) ;
#70829 = CARTESIAN_POINT ( 'NONE',  ( -3.297657676621885692, 4.870353260857385180, 1.599625672291267398 ) ) ;
#70830 = CARTESIAN_POINT ( 'NONE',  ( 2.536181837661064087, 1.019768383293401248, -1.906060392209196763 ) ) ;
#70831 = CARTESIAN_POINT ( 'NONE',  ( -7.431277594066152403, 8.802816960232885179, -1.082531754730549967 ) ) ;
#70832 = ADVANCED_FACE ( 'NONE', ( #11876 ), #30280, .T. ) ;
#70833 = CARTESIAN_POINT ( 'NONE',  ( 5.831415467653547680, 8.857049574687536619, -1.082531754730548412 ) ) ;
#70834 = CARTESIAN_POINT ( 'NONE',  ( 0.8617730121942971389, -1.675286201960282995, -1.300076073212981242 ) ) ;
#70835 = CARTESIAN_POINT ( 'NONE',  ( 5.790036952090301448, -0.8187086143041850672, 1.631793460665123208 ) ) ;
#70836 = CARTESIAN_POINT ( 'NONE',  ( 2.548066081221173729, 1.970837879163300332, 0.05219120132928834616 ) ) ;
#70837 = CARTESIAN_POINT ( 'NONE',  ( 4.570513122935188299, 0.7371126809179430195, 1.764830652192488580 ) ) ;
#70838 = ORIENTED_EDGE ( 'NONE', *, *, #190098, .F. ) ;
#70839 = DIRECTION ( 'NONE',  ( 0.000000000000000000, -1.000000000000000000, 0.000000000000000000 ) ) ;
#70840 = CARTESIAN_POINT ( 'NONE',  ( 4.668383401541156275, -0.8401123053542228769, -1.781513398035587281 ) ) ;
#70841 = CARTESIAN_POINT ( 'NONE',  ( 0.7615419678954943317, 0.9566914028362738520, 1.689878795569139891 ) ) ;
#70842 = ORIENTED_EDGE ( 'NONE', *, *, #208497, .T. ) ;
#70843 = CARTESIAN_POINT ( 'NONE',  ( -5.984998465789844069, 5.947196063035064206, 0.7998128361456281477 ) ) ;
#70845 = DIRECTION ( 'NONE',  ( 1.000000000000000000, 0.000000000000000000, 0.000000000000000000 ) ) ;
#70844 = CARTESIAN_POINT ( 'NONE',  ( -5.307090785106547415, 5.156303768904543894, -0.7998128361456362523 ) ) ;
#70848 = VECTOR ( 'NONE', #85725, 1000.000000000000000 ) ;
#70847 = CARTESIAN_POINT ( 'NONE',  ( 4.529832720297257254, 8.298905583739861314, 0.000000000000000000 ) ) ;
#70846 = CARTESIAN_POINT ( 'NONE',  ( 8.444030743212801227, 8.745790710036752458, 0.7998128361456462443 ) ) ;
#70850 = ORIENTED_EDGE ( 'NONE', *, *, #77409, .F. ) ;
#70849 = CARTESIAN_POINT ( 'NONE',  ( 5.356085673312771966, 0.7711821229579116643, -1.750063228584404440 ) ) ;
#70851 = CARTESIAN_POINT ( 'NONE',  ( 1.413402608508182556, 1.946665536341249503, 1.039416302365432587 ) ) ;
#70852 = CARTESIAN_POINT ( 'NONE',  ( 7.778383330260375317, -5.907420853759296264, 7.778383330260354001 ) ) ;
#70853 = CARTESIAN_POINT ( 'NONE',  ( 6.358070405704149941, 0.7683137238208622710, -1.860897411154702530 ) ) ;
#70854 = CARTESIAN_POINT ( 'NONE',  ( -9.984936468205201976, 4.580882523742140222, 6.662390435242588893 ) ) ;
#70855 = CARTESIAN_POINT ( 'NONE',  ( -0.04705280706217805642, 15.48512687740116611, 11.99263203770169817 ) ) ;
#70856 = CARTESIAN_POINT ( 'NONE',  ( -6.457408393014387293, -6.713678229394907326, -6.956254272497591096 ) ) ;
#70857 = CARTESIAN_POINT ( 'NONE',  ( 2.541538742049511246, 1.893869637037654208, -0.8368498079355383146 ) ) ;
#70858 = CARTESIAN_POINT ( 'NONE',  ( -3.927058049452637700, 7.733318157670055371, -0.7998128361456281477 ) ) ;
#70859 = CARTESIAN_POINT ( 'NONE',  ( -4.626128544448885549, 8.355821839108529048, -0.2988314032242797569 ) ) ;
#70861 = CARTESIAN_POINT ( 'NONE',  ( 0.4093245661422850734, 1.881582470445356314, 1.064130679222355491 ) ) ;
#70860 = CARTESIAN_POINT ( 'NONE',  ( -4.440459003675619520, 5.139289244831666714, 1.199719254218462483 ) ) ;
#70862 = CARTESIAN_POINT ( 'NONE',  ( -2.788906526875773208E-15, 11.18749999999999822, -1.499999999999998446 ) ) ;
#70863 = CARTESIAN_POINT ( 'NONE',  ( 4.584065335196271462, 5.481069324884694005, 1.082531754730549078 ) ) ;
#70864 = CARTESIAN_POINT ( 'NONE',  ( -9.604686356149274573, 3.481540744127369802, 7.193747284969079558 ) ) ;
#70865 = CARTESIAN_POINT ( 'NONE',  ( 0.6823417656249969321, 12.58854166700806942, -1.181850606188757036 ) ) ;
#70867 = CARTESIAN_POINT ( 'NONE',  ( -4.308458954092677651, 8.248562223075252220, -0.7998128361456362523 ) ) ;
#70866 = DIRECTION ( 'NONE',  ( -0.000000000000000000, 1.000000000000000000, -0.000000000000000000 ) ) ;
#70868 = CARTESIAN_POINT ( 'NONE',  ( 5.467320813769629417, -1.693630324315539726, -0.3718415804769247268 ) ) ;
#70869 = CARTESIAN_POINT ( 'NONE',  ( -2.605138072120212200, 6.191078184115536232, -0.7998128361456281477 ) ) ;
#70870 = CARTESIAN_POINT ( 'NONE',  ( 3.625891163443736520, 2.020865133175090644, -0.4488579359705275329 ) ) ;
#70871 = CARTESIAN_POINT ( 'NONE',  ( 4.569977310993092345, -0.9968198436792906625, 1.867865768302608531 ) ) ;
#70872 = AXIS2_PLACEMENT_3D ( 'NONE', #100459, #214166, #64760 ) ;
#70873 = CARTESIAN_POINT ( 'NONE',  ( 6.751070424600909448, 9.963667031088037973, -1.199719254218441611 ) ) ;
#70875 = EDGE_CURVE ( 'NONE', #169159, #113379, #97426, .T. ) ;
#70874 = CARTESIAN_POINT ( 'NONE',  ( -0.6823417656250212460, 4.301041667008085767, 1.181850606188767472 ) ) ;
#70876 = CARTESIAN_POINT ( 'NONE',  ( 2.940244962816233265, -1.016462931258435010, 1.686739332702111405 ) ) ;
#70877 = CARTESIAN_POINT ( 'NONE',  ( 0.7735182334044669039, 0.3705173918269571431, -1.875978362188877036 ) ) ;
#70878 = CARTESIAN_POINT ( 'NONE',  ( 4.418134799529137346, 1.412088972526281072, -1.805610035947482039 ) ) ;
#70879 = CARTESIAN_POINT ( 'NONE',  ( 2.191784710619415044, -0.7813054520266484726, 1.650194661559079456 ) ) ;
#70880 = EDGE_CURVE ( 'NONE', #205992, #9073, #55705, .T. ) ;
#70881 = CARTESIAN_POINT ( 'NONE',  ( 3.705121118284530279, 7.544668081299086282, -1.734723475976807094E-15 ) ) ;
#70882 = CARTESIAN_POINT ( 'NONE',  ( 4.636525345749193505, 8.353103970108639587, 1.040834085586084257E-14 ) ) ;
#70883 = CARTESIAN_POINT ( 'NONE',  ( -7.832860060393135093, 10.16142270859057462, 1.599625672291295375 ) ) ;
#70884 =( BOUNDED_CURVE ( )  B_SPLINE_CURVE ( 2, ( #39857, #102719, #152529, #4114, #72323, #7323, #170908 ),
 .UNSPECIFIED., .F., .T. ) 
 B_SPLINE_CURVE_WITH_KNOTS ( ( 3, 2, 2, 3 ),
 ( 0.3780836810543342641, 0.3809523809523809312, 0.3869047619047619180, 0.3897734618028085851 ),
 .UNSPECIFIED. ) 
 CURVE ( )  GEOMETRIC_REPRESENTATION_ITEM ( )  RATIONAL_B_SPLINE_CURVE ( ( 0.9331000818465633451, 0.9354320710352566071, 1.000000000000000000, 0.8660254037844387076, 1.000000000000000000, 0.9354320710352564960, 0.9331000818465632340 ) ) 
 REPRESENTATION_ITEM ( '' )  );
#70885 = CARTESIAN_POINT ( 'NONE',  ( 2.795184176893855899, -0.1524655061851394322, -2.007514041822997086 ) ) ;
#70886 = CARTESIAN_POINT ( 'NONE',  ( 3.397265449134680981, -1.732261247800225279, 0.9206733083975682241 ) ) ;
#70887 = CARTESIAN_POINT ( 'NONE',  ( -8.505042434474312074, 8.816971016508505343, -0.7998128361456291469 ) ) ;
#70888 = B_SPLINE_CURVE_WITH_KNOTS ( 'NONE', 3,
 ( #92805, #64543, #60272, #44047, #76519, #62407 ),
 .UNSPECIFIED., .F., .F.,
 ( 4, 2, 4 ),
 ( 0.000000000000000000, 0.0003844267940947831432, 0.0007688535881895662864 ),
 .UNSPECIFIED. ) ;
#70889 = CARTESIAN_POINT ( 'NONE',  ( -6.735703387890906946, 6.752742128827836865, -0.7998128361456291469 ) ) ;
#70890 = CARTESIAN_POINT ( 'NONE',  ( -10.91804383151481339, -8.407420853759283830, 0.1905751639681794174 ) ) ;
#70892 = CARTESIAN_POINT ( 'NONE',  ( 5.014393912088591421, 1.219005865285277546, -1.283338120600298726 ) ) ;
#70891 = CARTESIAN_POINT ( 'NONE',  ( 6.123005977957785007, -1.968908147963293942, 0.7033269742807277680 ) ) ;
#70893 = CARTESIAN_POINT ( 'NONE',  ( -3.796053574492273874, 15.00000000000182077, 12.24940615670316468 ) ) ;
#70894 = CARTESIAN_POINT ( 'NONE',  ( 0.4631483011842302266, 0.2107759881739781904, -2.181290363801504650 ) ) ;
#70895 = CARTESIAN_POINT ( 'NONE',  ( 0.2744473674479709913, 1.625014162249105443, -0.6237133657705071776 ) ) ;
#70896 = CARTESIAN_POINT ( 'NONE',  ( 7.182068686937156166, 9.402166106225269715, 1.599625672291281386 ) ) ;
#70897 = DIRECTION ( 'NONE',  ( 0.000000000000000000, -1.000000000000000000, 0.000000000000000000 ) ) ;
#70898 = CARTESIAN_POINT ( 'NONE',  ( 0.3339538366646053191, -1.498446967350696379, 1.742810101306817794 ) ) ;
#70899 = CARTESIAN_POINT ( 'NONE',  ( 0.04676574305502099321, -1.756316032869180921, 1.310637071781264984 ) ) ;
#70900 = CARTESIAN_POINT ( 'NONE',  ( 6.503290690126083184, 1.715628873550764988, 0.2497197086974659863 ) ) ;
#70901 = CARTESIAN_POINT ( 'NONE',  ( 2.983271218942393332, -0.1628219013674602478, -2.200934326520533446 ) ) ;
#70902 = CARTESIAN_POINT ( 'NONE',  ( 6.408646267151912213, 0.6747503738608184864, 2.063755040143978370 ) ) ;
#70903 = DIRECTION ( 'NONE',  ( 0.000000000000000000, -1.000000000000000000, -0.000000000000000000 ) ) ;
#70904 = CARTESIAN_POINT ( 'NONE',  ( 1.587271696126206111, 1.763578281176042761, 1.171447882250826522 ) ) ;
#70906 = AXIS2_PLACEMENT_3D ( 'NONE', #77759, #30083, #96175 ) ;
#70905 = CARTESIAN_POINT ( 'NONE',  ( 3.343750000000002220, 1.895863743164157178, 0.7852924748298092394 ) ) ;
#70907 = CARTESIAN_POINT ( 'NONE',  ( 6.727182134110195832, 2.427649464305783322, 2.470530574517680655 ) ) ;
#70908 = CARTESIAN_POINT ( 'NONE',  ( 6.018570082959111112, 1.293320673360508488, -1.427839425051903532 ) ) ;
#70909 = ORIENTED_EDGE ( 'NONE', *, *, #129470, .T. ) ;
#70911 = CARTESIAN_POINT ( 'NONE',  ( 1.364683531249984538, -1.032291666325247714, -0.7879004041258309554 ) ) ;
#70910 = CARTESIAN_POINT ( 'NONE',  ( 1.541004877621090507, -1.933652123512133114, 1.230999918854805975 ) ) ;
#70912 = CARTESIAN_POINT ( 'NONE',  ( 2.510230996824538430, 6.080353262937265413, 0.000000000000000000 ) ) ;
#70913 = CARTESIAN_POINT ( 'NONE',  ( 4.171104814498611368, 8.018039383557042044, 0.7998128361456321445 ) ) ;
#70914 = CARTESIAN_POINT ( 'NONE',  ( 3.194184678167404368, 1.410462778303589015, 1.716012817976236171 ) ) ;
#70915 = CARTESIAN_POINT ( 'NONE',  ( -9.327646496521992958, 9.984601788804893019, -0.7216878364870267237 ) ) ;
#70916 = CARTESIAN_POINT ( 'NONE',  ( 6.371969008742804697, 7.496680600697164465, -1.082531754730543083 ) ) ;
#70917 = CARTESIAN_POINT ( 'NONE',  ( -8.853111119599343937, 10.39134639669645566, 1.082531754730558626 ) ) ;
#70918 = CARTESIAN_POINT ( 'NONE',  ( 6.875393295905841917, 7.193916064744513506, 0.000000000000000000 ) ) ;
#70919 = ORIENTED_EDGE ( 'NONE', *, *, #175809, .T. ) ;
#70920 = CARTESIAN_POINT ( 'NONE',  ( 1.986954140179174155, -2.015912935764123670, 0.05229865529512293942 ) ) ;
#70922 = CARTESIAN_POINT ( 'NONE',  ( 6.285603487943992818, -1.943538462464271088, 0.6912672899390749359 ) ) ;
#70921 = CARTESIAN_POINT ( 'NONE',  ( 6.740374924288304648, 11.01552117831172062, 1.040834085586084257E-14 ) ) ;
#70923 = FACE_OUTER_BOUND ( 'NONE', #1953, .T. ) ;
#70924 = CARTESIAN_POINT ( 'NONE',  ( 6.007671464186825183, 8.102312356341712984, 1.443375672974064550 ) ) ;
#70925 = B_SPLINE_CURVE_WITH_KNOTS ( 'NONE', 3,
 ( #141047, #5625, #203838, #91206, #21878, #172445, #57623 ),
 .UNSPECIFIED., .F., .F.,
 ( 4, 3, 4 ),
 ( 0.0001135037246152992285, 0.0006245292469112881514, 0.002007692286193846990 ),
 .UNSPECIFIED. ) ;
#70926 = CARTESIAN_POINT ( 'NONE',  ( 6.040530583712122592, -1.465329908677007742, 0.9388326107527265041 ) ) ;
#70927 = SURFACE_STYLE_FILL_AREA ( #4847 ) ;
#70928 = CARTESIAN_POINT ( 'NONE',  ( 0.6823417656249882723, 2.426041667008084435, -1.181850606188749264 ) ) ;
#70929 = CARTESIAN_POINT ( 'NONE',  ( 1.616075582413665002, 1.193477697079999178, -1.306907023524202183 ) ) ;
#70930 = CARTESIAN_POINT ( 'NONE',  ( 0.4576579978108759050, -1.899619568183811058, -0.6767110947205197125 ) ) ;
#70931 = CARTESIAN_POINT ( 'NONE',  ( 0.2570343420702363435, 1.821350608449383124, -0.2692129421619017804 ) ) ;
#70932 = CARTESIAN_POINT ( 'NONE',  ( 3.597495906037956992, -0.6642907406799610781, 2.194031518130711067 ) ) ;
#70933 = CARTESIAN_POINT ( 'NONE',  ( 3.767381502543519112, 1.024135474229198151, 1.529801857347697025 ) ) ;
#70934 = CARTESIAN_POINT ( 'NONE',  ( 9.447334110624092673, 9.916311305349925220, -0.7998128361456281477 ) ) ;
#70935 = DIRECTION ( 'NONE',  ( 0.000000000000000000, 0.000000000000000000, -1.000000000000000000 ) ) ;
#70936 = CARTESIAN_POINT ( 'NONE',  ( 4.295794115256676982, -0.6985059363485807138, 1.686860163339451990 ) ) ;
#70937 = CARTESIAN_POINT ( 'NONE',  ( 5.238907797441370029, 2.013986022392059816, -0.1017483359899013229 ) ) ;
#70938 = CARTESIAN_POINT ( 'NONE',  ( -9.287498920561160887, 10.79416914786490089, -1.199719254218441611 ) ) ;
#70940 = CARTESIAN_POINT ( 'NONE',  ( -6.312203035614172286, 9.521931420595302953, -1.199719254218452047 ) ) ;
#70939 = CARTESIAN_POINT ( 'NONE',  ( 2.940562510593609513, 2.245292490812002661, 0.2782218841625680450 ) ) ;
#70941 = CARTESIAN_POINT ( 'NONE',  ( 0.03009625396771432870, -1.297761387203050232, -1.659265549802463546 ) ) ;
#70942 = CARTESIAN_POINT ( 'NONE',  ( 3.473154722801426786, 1.870513717286937494, 0.8877811045280564750 ) ) ;
#70943 = CARTESIAN_POINT ( 'NONE',  ( 3.083589872104280705, 5.684939719841914929, 1.199719254218450271 ) ) ;
#70944 = CARTESIAN_POINT ( 'NONE',  ( -1.360316468750062846, 1.401041667008104508, -0.7853790794158941324 ) ) ;
#70945 = CARTESIAN_POINT ( 'NONE',  ( 5.707716976326653757, 1.605689621071492601, 1.385122894465253829 ) ) ;
#70946 = APPLICATION_PROTOCOL_DEFINITION ( 'draft international standard', 'automotive_design', 1998, #141817 ) ;
#70948 = CARTESIAN_POINT ( 'NONE',  ( 1.576654987853912449, -1.829214484822901055, -0.6046830185306437677 ) ) ;
#70947 = CARTESIAN_POINT ( 'NONE',  ( -10.15235809853472126, 10.73883929124566983, -0.7998128361456291469 ) ) ;
#70949 = UNCERTAINTY_MEASURE_WITH_UNIT (LENGTH_MEASURE( 1.000000000000000082E-05 ), #108005, 'distance_accuracy_value', 'NONE');
#70950 = CARTESIAN_POINT ( 'NONE',  ( 8.718062746983862965, 13.27486625357122563, -8.129070176819260141 ) ) ;
#70951 = CARTESIAN_POINT ( 'NONE',  ( 0.2562226757886588713, -1.969045882358761101, -0.05199970915584737480 ) ) ;
#70952 = CARTESIAN_POINT ( 'NONE',  ( 4.299344108864946890, 6.109263775132799168, -1.443375672974068769 ) ) ;
#70953 = CARTESIAN_POINT ( 'NONE',  ( 5.463439706979909438, 6.248932391672394893, 1.002290858133829010 ) ) ;
#70954 = CARTESIAN_POINT ( 'NONE',  ( 10.48884024596648601, 1.000000000000000888, -5.608780650328974104 ) ) ;
#70955 = CARTESIAN_POINT ( 'NONE',  ( -5.278201874421821316, 5.052323696447222900, 0.7998128361456341429 ) ) ;
#70956 = CARTESIAN_POINT ( 'NONE',  ( 0.08853117554794007193, 1.285972019905703201, 1.811169930398129013 ) ) ;
#70957 = CARTESIAN_POINT ( 'NONE',  ( 3.206187942969561000, -2.103625563118251218, 0.1016139793386036383 ) ) ;
#70958 = CARTESIAN_POINT ( 'NONE',  ( -4.142898457427624415, 6.991076079377632091, 1.199719254218452935 ) ) ;
#70959 = CARTESIAN_POINT ( 'NONE',  ( 6.693975156845185737, 8.832723654451292816, 1.599625672291281386 ) ) ;
#70960 = CARTESIAN_POINT ( 'NONE',  ( 0.4669691663035968054, 1.616376026143636624, 0.9223025969757200349 ) ) ;
#70961 = CARTESIAN_POINT ( 'NONE',  ( 5.126954644262057492, 9.133197518281081173, 0.7998128361456462443 ) ) ;
#70962 = CARTESIAN_POINT ( 'NONE',  ( 5.996784015946103885, 5.890669528225568996, 1.040834085586084257E-14 ) ) ;
#70963 = CARTESIAN_POINT ( 'NONE',  ( -5.641601317062233001, 9.595968946632336127, -0.7216878364870338292 ) ) ;
#70964 = CARTESIAN_POINT ( 'NONE',  ( -8.568389894156720032, 10.05917163368005163, 1.082531754730558626 ) ) ;
#70965 = CARTESIAN_POINT ( 'NONE',  ( 1.582450481569739331, 1.094613367649547309, 1.816135667671102016 ) ) ;
#70966 = CARTESIAN_POINT ( 'NONE',  ( -6.668631453075260396, 8.873432343378178544, -1.599625672291271394 ) ) ;
#70968 = CARTESIAN_POINT ( 'NONE',  ( 3.596105239937871456, 0.8843387906064968940, -1.751336483779348585 ) ) ;
#70967 = CARTESIAN_POINT ( 'NONE',  ( 0.6124999999999932720, 0.9166666666666906105, -1.060881119635955327 ) ) ;
#70969 = CARTESIAN_POINT ( 'NONE',  ( 2.676834871759771417, -2.068302492614528365, -0.6285112194897370941 ) ) ;
#70970 = CARTESIAN_POINT ( 'NONE',  ( 1.223879446662301307, 1.774596971308094018, 0.4907264878865265634 ) ) ;
#70972 = CARTESIAN_POINT ( 'NONE',  ( -4.447391987980185313, 7.103198448885253313, -1.107391122544647333 ) ) ;
#70971 = FACE_OUTER_BOUND ( 'NONE', #84667, .T. ) ;
#70973 = CARTESIAN_POINT ( 'NONE',  ( 3.820004643325402238, 1.653240603489447569, 0.5438404159014453843 ) ) ;
#70974 = DIRECTION ( 'NONE',  ( 0.000000000000000000, -1.000000000000000000, 0.000000000000000000 ) ) ;
#70975 = CARTESIAN_POINT ( 'NONE',  ( 5.504247177468179153, 7.444707678511436555, 1.443375672974062551 ) ) ;
#70976 = CARTESIAN_POINT ( 'NONE',  ( -9.986107380900749675, 5.615474669794299878, -5.966265754238714969 ) ) ;
#70977 = CARTESIAN_POINT ( 'NONE',  ( 0.8312129145573650124, 0.1600495679085281175, 2.155820468135719814 ) ) ;
#70978 = CARTESIAN_POINT ( 'NONE',  ( 3.725935337077026510, -1.776739457207517248, -0.9528653653038119398 ) ) ;
#70979 = CARTESIAN_POINT ( 'NONE',  ( 0.000000000000000000, 8.980740528189222971, 0.000000000000000000 ) ) ;
#70980 = CARTESIAN_POINT ( 'NONE',  ( -4.496464221587651799, 5.274905009054215554, 1.199719254218452935 ) ) ;
#70981 = CARTESIAN_POINT ( 'NONE',  ( 3.045733664408939223, 0.7109379216812520275, -1.838982635421481993 ) ) ;
#70982 = CARTESIAN_POINT ( 'NONE',  ( 6.509000000000016328, 7.053097208480951785, 2.498154145070859311 ) ) ;
#70983 = CARTESIAN_POINT ( 'NONE',  ( 2.050241756059832721, -1.499988152044306133, 1.233518166440790598 ) ) ;
#70986 = VERTEX_POINT ( 'NONE', #177601 ) ;
#70985 = CARTESIAN_POINT ( 'NONE',  ( -5.994113311017573054, 6.165756082374834079, 0.7216878364870257245 ) ) ;
#70984 = CARTESIAN_POINT ( 'NONE',  ( -11.06305611892948448, 9.842384604456084318, 0.9079708613958296093 ) ) ;
#70987 = CARTESIAN_POINT ( 'NONE',  ( -4.082413651046300274, 6.816547455312373494, 1.082531754730549967 ) ) ;
#70988 = CARTESIAN_POINT ( 'NONE',  ( 5.357406976055401948, 6.279338222599979424, 1.199719254218452935 ) ) ;
#70989 = CARTESIAN_POINT ( 'NONE',  ( -4.980641328173854632, 6.904110530993182948, 1.599625672291263179 ) ) ;
#70990 = CARTESIAN_POINT ( 'NONE',  ( -6.119526231721793330, 8.232809585132461194, 1.599625672291263179 ) ) ;
#70991 = DIRECTION ( 'NONE',  ( -0.000000000000000000, -1.000000000000000000, 0.000000000000000000 ) ) ;
#70992 = CARTESIAN_POINT ( 'NONE',  ( 6.510760317505348560, 1.716126801009032032, -1.542884448788630625 ) ) ;
#70993 = CARTESIAN_POINT ( 'NONE',  ( 6.478960399985357554, 1.830089090633261417, 0.7073212282268787066 ) ) ;
#70994 = CARTESIAN_POINT ( 'NONE',  ( 4.399235598239510381, -1.708881994454291675, 0.9632455365647660805 ) ) ;
#70995 = CARTESIAN_POINT ( 'NONE',  ( 7.365103760721646076, 9.615707025640515937, 1.599625672291281386 ) ) ;
#70996 = CARTESIAN_POINT ( 'NONE',  ( 2.162732623366144136, 1.242727809108796322, 1.587836805404294171 ) ) ;
#70997 = ORIENTED_EDGE ( 'NONE', *, *, #78986, .F. ) ;
#70998 = CARTESIAN_POINT ( 'NONE',  ( 2.255205753237074617, 0.09875464746901543855, -2.115135400419057010 ) ) ;
#70999 = CARTESIAN_POINT ( 'NONE',  ( -1.402160292154681736E-14, 1.618750000682814827, -1.732050807568863648 ) ) ;
#71001 = CARTESIAN_POINT ( 'NONE',  ( -5.368138756007025947, 8.350246751061767725, 1.199719254218452047 ) ) ;
#71000 = CARTESIAN_POINT ( 'NONE',  ( -3.297657676621885692, 4.870353260857385180, 1.599625672291267398 ) ) ;
#71002 = CARTESIAN_POINT ( 'NONE',  ( 3.222423357234116992, 0.04607595322191247039, 1.840729346561786439 ) ) ;
#71003 = EDGE_LOOP ( 'NONE', ( #112281, #122181, #83097, #35722 ) ) ;
#71004 = CARTESIAN_POINT ( 'NONE',  ( -9.134442807305063639, 11.67993591332117376, 1.599625672291281386 ) ) ;
#71005 = CARTESIAN_POINT ( 'NONE',  ( 10.72102920343737331, 9.918789484241997911, 5.400078146547925506 ) ) ;
#71006 = CARTESIAN_POINT ( 'NONE',  ( 4.271814301144261528, 0.4616217191124799002, -2.069597271375968273 ) ) ;
#71007 = DIRECTION ( 'NONE',  ( 0.2684563758389248433, 0.000000000000000000, -0.9632918427306597087 ) ) ;
#71008 = CARTESIAN_POINT ( 'NONE',  ( 6.856673000209174695, 9.022537805042615489, 1.599625672291281386 ) ) ;
#71009 = CARTESIAN_POINT ( 'NONE',  ( 4.727839713825126466, -1.264755334911156881, -1.626962714342747196 ) ) ;
#71011 = CARTESIAN_POINT ( 'NONE',  ( 2.014959344526063845, -1.785600367564584179, 0.4486904387498573676 ) ) ;
#71010 = CARTESIAN_POINT ( 'NONE',  ( -5.526920175865215334, 9.599823971818089774, 0.7998128361456481317 ) ) ;
#71012 = CARTESIAN_POINT ( 'NONE',  ( 9.420217803396747414, 9.884675613584706255, 0.7998128361456462443 ) ) ;
#71013 = CARTESIAN_POINT ( 'NONE',  ( 6.115102234889607580, 6.015626655811740164, -0.1465594925542352267 ) ) ;
#71014 = CARTESIAN_POINT ( 'NONE',  ( -5.698619510900288176, 7.404755683226262875, -1.372140228778085502 ) ) ;
#71015 = CARTESIAN_POINT ( 'NONE',  ( -1.499999999998296696, 8.673756432004703143, 2.614717076620993730 ) ) ;
#71016 = DIRECTION ( 'NONE',  ( 0.000000000000000000, 1.000000000000000000, 0.000000000000000000 ) ) ;
#71017 = CARTESIAN_POINT ( 'NONE',  ( 2.227434312139275896, 0.001603268854937638837, 2.207063162490217056 ) ) ;
#71018 = CARTESIAN_POINT ( 'NONE',  ( 3.392113076582465858, -0.9204767452889413004, 2.066876591271109120 ) ) ;
#71019 = CARTESIAN_POINT ( 'NONE',  ( -7.619319141200077361, 9.912291636198670375, 1.443375672974090751 ) ) ;
#71020 = CARTESIAN_POINT ( 'NONE',  ( 3.304753640158542893, -0.3582801770840525757, -1.775609565582184191 ) ) ;
#71021 = CARTESIAN_POINT ( 'NONE',  ( 3.960093407954877520, -1.098340823217320184, 1.569403885630010320 ) ) ;
#71022 = ADVANCED_FACE ( 'NONE', ( #43346 ), #27061, .T. ) ;
#71023 = CARTESIAN_POINT ( 'NONE',  ( -1.001543065824772872E-14, 4.634375000341418804, 1.575800808251672791 ) ) ;
#71024 = CARTESIAN_POINT ( 'NONE',  ( 3.784019197727214401, -0.9729451851334305346, 1.714598810357757630 ) ) ;
#71025 = CARTESIAN_POINT ( 'NONE',  ( 0.9559316444634465837, 1.924326902252432081, -0.09161688492189544453 ) ) ;
#71026 = CARTESIAN_POINT ( 'NONE',  ( 5.489076674590072535, 1.649195787720953987, -0.8828566466120502110 ) ) ;
#71027 = EDGE_CURVE ( 'NONE', #44793, #142253, #156293, .T. ) ;
#71028 = CARTESIAN_POINT ( 'NONE',  ( 3.141587237543626454, -2.035091569058588679, 1.088060180353218165 ) ) ;
#71029 = CARTESIAN_POINT ( 'NONE',  ( 4.334314691326750513, -1.072585289120084440, 1.520660633866082634 ) ) ;
#71030 = CARTESIAN_POINT ( 'NONE',  ( 1.364683531249990311, 5.613541667008087543, 0.7879004041258500513 ) ) ;
#71031 = AXIS2_PLACEMENT_3D ( 'NONE', #207065, #60826, #190809 ) ;
#71032 = CARTESIAN_POINT ( 'NONE',  ( 10.91914056351824414, 3.934209603697785607, -3.813461610468072749 ) ) ;
#71034 = CARTESIAN_POINT ( 'NONE',  ( 2.244876548131835126, 0.4624279887704956238, 2.054504457251419502 ) ) ;
#71033 = CARTESIAN_POINT ( 'NONE',  ( -4.894130264408878439, 4.812166184672871161, -0.7216878364870197293 ) ) ;
#71035 = AXIS2_PLACEMENT_3D ( 'NONE', #101531, #35452, #99404 ) ;
#71036 = CARTESIAN_POINT ( 'NONE',  ( 2.846849068745292755, 6.265148313604064434, 0.000000000000000000 ) ) ;
#71038 = CARTESIAN_POINT ( 'NONE',  ( 11.86239285000045740, 9.719999999999998863, -1.812080536912752837 ) ) ;
#71037 = CYLINDRICAL_SURFACE ( 'NONE', #11254, 1.250000000000000000 ) ;
#71039 = CARTESIAN_POINT ( 'NONE',  ( 3.410498715577559015, -2.118327196165440185, -0.1003008382433126094 ) ) ;
#71040 = CARTESIAN_POINT ( 'NONE',  ( 0.6154972907393120307, 1.653649208057221598, 1.159462664468139614 ) ) ;
#71041 = CARTESIAN_POINT ( 'NONE',  ( -1.364683531250014514, 0.4885416670080875434, -0.7879004041258289570 ) ) ;
#71042 = CARTESIAN_POINT ( 'NONE',  ( -4.297571505851936813, 4.116180966356429494, 1.214306433183764966E-14 ) ) ;
#71043 = CARTESIAN_POINT ( 'NONE',  ( 5.983225862332436584, 5.874851682342960402, 0.7998128361456341429 ) ) ;
#71044 = ORIENTED_EDGE ( 'NONE', *, *, #126447, .T. ) ;
#71045 = CARTESIAN_POINT ( 'NONE',  ( 2.390102426918311540, -0.9266024157483061519, 1.953076554623616401 ) ) ;
#71046 = CARTESIAN_POINT ( 'NONE',  ( 6.610000000000010090, 0.5825982378308904863, 2.053072689460200273 ) ) ;
#71049 = CARTESIAN_POINT ( 'NONE',  ( 6.539320575229289112, 0.004092658091040711314, 2.003502637948689102 ) ) ;
#71048 = CARTESIAN_POINT ( 'NONE',  ( 6.925078400183553029, 6.037155338232472523, 2.550556537725846340 ) ) ;
#71047 = CARTESIAN_POINT ( 'NONE',  ( 6.412080304620304538, 6.445458208337293549, -0.7998128361456481317 ) ) ;
#71050 = DIRECTION ( 'NONE',  ( 0.000000000000000000, -1.000000000000000000, 0.000000000000000000 ) ) ;
#71051 = CARTESIAN_POINT ( 'NONE',  ( 6.298064597363540074, -0.9548514761729166578, -1.776169100128288658 ) ) ;
#71052 = CARTESIAN_POINT ( 'NONE',  ( -7.022760382198764084, 11.13704484596649635, 0.7216878364870458196 ) ) ;
#71053 = CARTESIAN_POINT ( 'NONE',  ( 6.497611715980437630, -2.090283427287362272, 0.05178676472679385329 ) ) ;
#71054 = CARTESIAN_POINT ( 'NONE',  ( 10.91005274787795720, -6.893137084989842123, -0.4659925305415656971 ) ) ;
#71056 = CARTESIAN_POINT ( 'NONE',  ( 1.364683531250000748, 12.50520833367473550, -0.7879004041258355073 ) ) ;
#71055 = CARTESIAN_POINT ( 'NONE',  ( 0.3743661609300020232, 1.305675439620108458, 1.847588536312362972 ) ) ;
#71057 = CARTESIAN_POINT ( 'NONE',  ( -7.784352752540590004, 12.23349531127272094, 0.7998128361456481317 ) ) ;
#71058 = CARTESIAN_POINT ( 'NONE',  ( -6.534666851662457532, 6.726125536468730459, 1.040834085586084257E-14 ) ) ;
#71059 = CARTESIAN_POINT ( 'NONE',  ( -1.201851678989727383E-14, 2.134375000341423689, 1.575800808251672791 ) ) ;
#71060 = CARTESIAN_POINT ( 'NONE',  ( 0.000000000000000000, 1.000000000000000888, 0.000000000000000000 ) ) ;
#71061 = CARTESIAN_POINT ( 'NONE',  ( -1.500000000000008216, 10.25000000000000178, 3.469446951953614189E-15 ) ) ;
#71062 = CARTESIAN_POINT ( 'NONE',  ( 2.578358533787118212, -1.650418691300073570, -0.5013113332296408320 ) ) ;
#71063 = CARTESIAN_POINT ( 'NONE',  ( 3.555981428534177091, 7.370671776590375757, 0.7998128361456271485 ) ) ;
#71064 = CARTESIAN_POINT ( 'NONE',  ( 1.950134490391452369, 0.5496875458596857111, 1.682295776093334139 ) ) ;
#71065 = CARTESIAN_POINT ( 'NONE',  ( 2.983067126429808091, -1.860865636787402577, -0.7683904602088088565 ) ) ;
#71066 = CARTESIAN_POINT ( 'NONE',  ( 10.57266086055835075, 11.22919251360659310, 0.000000000000000000 ) ) ;
#71068 = COLOUR_RGB ( '', 0.72549020, 0.75294118, 0.79215686) ;
#71067 = CARTESIAN_POINT ( 'NONE',  ( 5.421004802376033993, 2.037064969303593820, 0.8491359902737596332 ) ) ;
#71069 = VERTEX_POINT ( 'NONE', #129993 ) ;
#71070 = CARTESIAN_POINT ( 'NONE',  ( -6.936931872047518155, 8.122117267924091166, 1.199719254218452047 ) ) ;
#71072 = CARTESIAN_POINT ( 'NONE',  ( 4.359000025081374297, -0.002827702239943663542, -2.016598147179492262 ) ) ;
#71071 = CARTESIAN_POINT ( 'NONE',  ( 4.776102292387626846, 2.097323840013893381, -0.3118266106481304423 ) ) ;
#71073 = EDGE_LOOP ( 'NONE', ( #152504, #24156, #140977, #110899 ) ) ;
#71074 = CARTESIAN_POINT ( 'NONE',  ( 3.711900195091365262, 7.552577004240394132, -0.7998128361456362523 ) ) ;
#71075 = ORIENTED_EDGE ( 'NONE', *, *, #60772, .T. ) ;
#71076 = CARTESIAN_POINT ( 'NONE',  ( 0.9361565222895779081, 1.842281575443193375, 0.3236747858033904302 ) ) ;
#71077 = CARTESIAN_POINT ( 'NONE',  ( -10.91962425643199808, -9.999999999999994671, 0.09058751758333691284 ) ) ;
#71078 = CARTESIAN_POINT ( 'NONE',  ( 6.041655779063732190, -1.703243848673033023, 0.6171442250446981248 ) ) ;
#71080 = CIRCLE ( 'NONE', #129952, 0.5000000000000013323 ) ;
#71079 = CARTESIAN_POINT ( 'NONE',  ( -1.452583904633382383, -1.374772708486751593, 1.500000000000001332 ) ) ;
#71081 = CARTESIAN_POINT ( 'NONE',  ( -10.32224513571693869, 3.007486591634276341, -7.366906358548013678 ) ) ;
#71082 = CARTESIAN_POINT ( 'NONE',  ( 4.028181036591608866, 7.713645286083285590, -0.7216878364870253915 ) ) ;
#71083 = CARTESIAN_POINT ( 'NONE',  ( -0.6823417656250212460, 3.613541667008085767, 1.181850606188767472 ) ) ;
#71084 = CYLINDRICAL_SURFACE ( 'NONE', #202202, 0.09999999999999986677 ) ;
#71085 = STYLED_ITEM ( 'NONE', ( #4014 ), #136888 ) ;
#71086 = CARTESIAN_POINT ( 'NONE',  ( 4.733205024946604667, 8.536173272497439513, 0.000000000000000000 ) ) ;
#71087 = CARTESIAN_POINT ( 'NONE',  ( 1.433958818539453395, 1.165882187713672247, 1.577721859592796205 ) ) ;
#71088 = CARTESIAN_POINT ( 'NONE',  ( -5.017926250833627755, 5.026871178826882947, 0.7216878364870257245 ) ) ;
#71089 = EDGE_CURVE ( 'NONE', #17872, #77955, #93779, .T. ) ;
#71090 = CARTESIAN_POINT ( 'NONE',  ( -6.635789839245807897, 6.706452665400368218, 0.7998128361456341429 ) ) ;
#71091 = CARTESIAN_POINT ( 'NONE',  ( 3.639029512587122372, 2.014767915268770082, 0.6618469929612482705 ) ) ;
#71093 = DIRECTION ( 'NONE',  ( -0.000000000000000000, -1.000000000000000000, -0.000000000000000000 ) ) ;
#71092 = CARTESIAN_POINT ( 'NONE',  ( 2.425588855776289687, 2.974000657016989901, -11.41149836408899709 ) ) ;
#71094 = CARTESIAN_POINT ( 'NONE',  ( 5.641858350889248364, 0.8014469270729590589, -1.801278572543635326 ) ) ;
#71095 = CARTESIAN_POINT ( 'NONE',  ( -1.364683531250012516, 1.030208333674754062, 0.7879004041258379498 ) ) ;
#71096 = CARTESIAN_POINT ( 'NONE',  ( 0.7385399849154888896, 1.195762776690506790, -1.619497776973168213 ) ) ;
#71097 = VERTEX_POINT ( 'NONE', #145130 ) ;
#71098 = CARTESIAN_POINT ( 'NONE',  ( 1.370887597065591823, -0.3147031148599331307, -2.093612404753260492 ) ) ;
#71099 = CARTESIAN_POINT ( 'NONE',  ( 11.48869292188783753, 7.332629663034461842, 3.321605222796156998 ) ) ;
#71100 = CARTESIAN_POINT ( 'NONE',  ( 3.191909353267761151, -1.388477207968623839, -1.535938721777901472 ) ) ;
#71101 = ORIENTED_EDGE ( 'NONE', *, *, #41850, .T. ) ;
#71102 = CARTESIAN_POINT ( 'NONE',  ( 3.867818961648523235, 7.734482231890414283, 1.040834085586084257E-14 ) ) ;
#71103 = CARTESIAN_POINT ( 'NONE',  ( 4.050854035433010480, 7.948023151305657841, 0.000000000000000000 ) ) ;
#71104 = ORIENTED_EDGE ( 'NONE', *, *, #213238, .F. ) ;
#71106 = CARTESIAN_POINT ( 'NONE',  ( 4.008406971134620633, 7.828225232965717595, 0.7998128361456321445 ) ) ;
#71105 = CARTESIAN_POINT ( 'NONE',  ( 4.611325087297634795, -2.050354119209703008, 0.4075000692524420876 ) ) ;
#71109 = VERTEX_POINT ( 'NONE', #62759 ) ;
#71108 = CARTESIAN_POINT ( 'NONE',  ( 1.506221797076849889, -1.802732806890252837, -0.1774259793663693907 ) ) ;
#71107 = CARTESIAN_POINT ( 'NONE',  ( 3.135583521505393545, -1.224952879796761041, -1.353777129306121818 ) ) ;
#71110 = CARTESIAN_POINT ( 'NONE',  ( 6.481111342790009999, -0.1036386110354891726, -2.204582208980155222 ) ) ;
#71111 = CARTESIAN_POINT ( 'NONE',  ( -8.917737905728751358, 3.499999999999989342, -8.029567276306261547 ) ) ;
#71112 = CARTESIAN_POINT ( 'NONE',  ( 4.278500955059440614, -1.273273528111932063, 1.802203266693293893 ) ) ;
#71113 = CARTESIAN_POINT ( 'NONE',  ( 7.121056995675668411, 9.330985799753529264, -1.599625672291262513 ) ) ;
#71114 = CARTESIAN_POINT ( 'NONE',  ( -8.012344526598182026E-15, 9.359375000341396245, -1.575800808251669460 ) ) ;
#71115 = EDGE_CURVE ( 'NONE', #128668, #86318, #41982, .T. ) ;
#71116 = CARTESIAN_POINT ( 'NONE',  ( 3.088426618631805454, -1.137173348016347063, 1.537276688398482083 ) ) ;
#71117 = CARTESIAN_POINT ( 'NONE',  ( -3.918470089549458635, 4.530302178351167441, -1.199719254218452047 ) ) ;
#71118 = CARTESIAN_POINT ( 'NONE',  ( 8.178592977541601527, 10.56477777859713463, 1.599625672291281386 ) ) ;
#71119 = DIRECTION ( 'NONE',  ( 1.000000000000000000, 0.000000000000000000, 0.000000000000000000 ) ) ;
#71120 = CARTESIAN_POINT ( 'NONE',  ( -1.953008978358306879E-14, 0.2343750003414031002, 1.570758158831794260 ) ) ;
#71121 = CARTESIAN_POINT ( 'NONE',  ( 5.812113132715003516, 1.472855484078567700, -1.623034594306454137 ) ) ;
#71122 = CARTESIAN_POINT ( 'NONE',  ( 5.494857653270467601, 7.581134149042087600, -1.337725346733337872 ) ) ;
#71123 = CARTESIAN_POINT ( 'NONE',  ( -3.101842508592871361, 15.51993578035203569, -11.60075130052193337 ) ) ;
#71124 = ORIENTED_EDGE ( 'NONE', *, *, #58112, .F. ) ;
#71125 = CARTESIAN_POINT ( 'NONE',  ( 11.41267819554179042, 3.447199233515649386, -3.708203932499494648 ) ) ;
#71126 = CARTESIAN_POINT ( 'NONE',  ( 3.075316773429651818, 1.777364689479765003, -0.5833007003755164011 ) ) ;
#71127 = CARTESIAN_POINT ( 'NONE',  ( 1.001543065824772753E-15, -1.159374999522043703, 3.793834371823810780 ) ) ;
#71128 = CARTESIAN_POINT ( 'NONE',  ( 4.746763178560250651, 7.591621904078704297, 1.082531754730549078 ) ) ;
#71129 = CARTESIAN_POINT ( 'NONE',  ( -8.351459436338048548, 8.845716885256940998, -0.7216878364870278340 ) ) ;
#71130 = CARTESIAN_POINT ( 'NONE',  ( 3.711900195091365262, 7.552577004240394132, -0.7998128361456362523 ) ) ;
#71131 = CARTESIAN_POINT ( 'NONE',  ( 0.2683110675134177669, -0.8374301267611580224, -1.781048649993026700 ) ) ;
#71132 = CARTESIAN_POINT ( 'NONE',  ( 1.317982704262925520, 0.9913799330133237220, -1.755781447868165257 ) ) ;
#71133 = CARTESIAN_POINT ( 'NONE',  ( -8.676328237741483207, 12.20980114641871062, -1.199719254218446718 ) ) ;
#71134 = CARTESIAN_POINT ( 'NONE',  ( 6.481679955784983349, 9.719654494127929922, -1.199719254218452047 ) ) ;
#71135 = EDGE_CURVE ( 'NONE', #99531, #156687, #38391, .T. ) ;
#71136 = CARTESIAN_POINT ( 'NONE',  ( 1.693587955360946529, -0.7361150630936144079, 2.064250245950305374 ) ) ;
#71137 = CARTESIAN_POINT ( 'NONE',  ( 6.305291373979137859, 1.520805759102666910, 1.009792402853857185 ) ) ;
#71138 = CARTESIAN_POINT ( 'NONE',  ( -3.541704441667874903, 5.155074486744371853, -1.599625672291256295 ) ) ;
#71139 = EDGE_CURVE ( 'NONE', #193812, #178469, #118240, .T. ) ;
#71140 = CARTESIAN_POINT ( 'NONE',  ( 4.909461021924240498, 7.781436054670031410, 1.082531754730549078 ) ) ;
#71141 = CARTESIAN_POINT ( 'NONE',  ( 10.72180055030867329, 11.40318881831530540, 0.7998128361456341429 ) ) ;
#71142 = CARTESIAN_POINT ( 'NONE',  ( 5.217190183160311356, 4.981143389975473568, -0.7998128361456211532 ) ) ;
#71143 = CARTESIAN_POINT ( 'NONE',  ( 3.040771591214902259, 6.769593633051179005, -0.7998128361456362523 ) ) ;
#71144 = ORIENTED_EDGE ( 'NONE', *, *, #4772, .T. ) ;
#71146 = CARTESIAN_POINT ( 'NONE',  ( 0.2057266557286231146, 1.493221433009199517, 1.350316897416648843 ) ) ;
#71145 = CARTESIAN_POINT ( 'NONE',  ( 3.526749072549471453, -1.699942963128863838, 0.7078653300200200560 ) ) ;
#71147 = CARTESIAN_POINT ( 'NONE',  ( 2.320019640604139788, -1.777541238149564107, 1.457059784348129217 ) ) ;
#71149 = CARTESIAN_POINT ( 'NONE',  ( 6.209812062937981381, 0.5727486527220859713, -1.876249287704085722 ) ) ;
#71148 = CARTESIAN_POINT ( 'NONE',  ( 4.541618270897912701, 4.400902192243413502, 1.214306433183764966E-14 ) ) ;
#71150 = CARTESIAN_POINT ( 'NONE',  ( -3.242371291962510504, 6.934516940598226320, 1.040834085586084257E-14 ) ) ;
#71151 = DIRECTION ( 'NONE',  ( -1.000000000000000000, 0.000000000000000000, 0.000000000000000000 ) ) ;
#71152 = CARTESIAN_POINT ( 'NONE',  ( 4.517770118113122457, -0.5046507728132009207, 1.844564425022446885 ) ) ;
#71153 = CARTESIAN_POINT ( 'NONE',  ( -10.62011439820619429, 11.28455497419572318, -0.7998128361456221525 ) ) ;
#71154 = CARTESIAN_POINT ( 'NONE',  ( 5.997574213172828905, 7.082153300894140635, -1.064076030282636420 ) ) ;
#71155 = CARTESIAN_POINT ( 'NONE',  ( -3.634467696915153034, 6.397906858779740524, 1.199719254218452935 ) ) ;
#71157 = CARTESIAN_POINT ( 'NONE',  ( 0.9361565222895779081, 1.842281575443193375, 0.3236747858033904302 ) ) ;
#71156 = CARTESIAN_POINT ( 'NONE',  ( 3.157844376090960026, 0.9421199074126384021, 1.866540799821286845 ) ) ;
#71158 = CARTESIAN_POINT ( 'NONE',  ( 1.739611019359630584, -1.913509794028777522, -0.6351045200190530426 ) ) ;
#71159 = CARTESIAN_POINT ( 'NONE',  ( 6.805829924380097040, 10.88395931184472154, 0.7216878364870438212 ) ) ;
#71160 = CARTESIAN_POINT ( 'NONE',  ( -1.364683531250010740, 3.842708333674751398, 0.7879004041258379498 ) ) ;
#71161 = CARTESIAN_POINT ( 'NONE',  ( 2.735604107484723269, 1.727544688213778601, 0.2106955661135938018 ) ) ;
#71162 = CARTESIAN_POINT ( 'NONE',  ( 5.335297142177534369, 6.183267073083954735, -1.199719254218452047 ) ) ;
#71164 = CARTESIAN_POINT ( 'NONE',  ( 0.4608211143923647835, 2.871031678985719537, -1.947158891359296540 ) ) ;
#71163 = CARTESIAN_POINT ( 'NONE',  ( 1.499999999999990896, 3.775000000000021227, 1.214306433183764966E-14 ) ) ;
#71165 = CARTESIAN_POINT ( 'NONE',  ( 3.439825841515719240, 0.7741550462027242396, -1.541462414610708764 ) ) ;
#71166 = CARTESIAN_POINT ( 'NONE',  ( 3.421585747727782678, -1.306972202059282218, -1.759028276249123168 ) ) ;
#71167 = CARTESIAN_POINT ( 'NONE',  ( 6.287735281038357549, 1.518688880046001444, 1.601449620450722700 ) ) ;
#71168 = DIRECTION ( 'NONE',  ( -0.000000000000000000, 1.000000000000000000, 9.023263958591317418E-17 ) ) ;
#71169 = CARTESIAN_POINT ( 'NONE',  ( 3.819318941869216388, -1.912159422281418220, -1.028266076255865968 ) ) ;
#71170 = CARTESIAN_POINT ( 'NONE',  ( 2.349991895876184511, 1.825291697999480434, 0.04531359951509549705 ) ) ;
#71171 = CARTESIAN_POINT ( 'NONE',  ( 0.2331563151865486683, 0.005903526429595904942, -1.945944850731482934 ) ) ;
#71172 = CARTESIAN_POINT ( 'NONE',  ( 5.067619284625084930, 1.424172025040346679, 1.566925857267987832 ) ) ;
#71173 = CARTESIAN_POINT ( 'NONE',  ( 3.798255590122798342, 7.583048621785260401, -0.7998128361456221525 ) ) ;
#71174 = ORIENTED_EDGE ( 'NONE', *, *, #113105, .F. ) ;
#71176 = CARTESIAN_POINT ( 'NONE',  ( -0.6823417656250212460, 2.363541667008084435, 1.181850606188767472 ) ) ;
#71175 = CARTESIAN_POINT ( 'NONE',  ( 5.232074500395570205, 2.258064205686944437, 0.3942454582816708464 ) ) ;
#71177 = CARTESIAN_POINT ( 'NONE',  ( 6.620655732516659064, 6.039214117936751336, 2.421170424969817603 ) ) ;
#71178 = CARTESIAN_POINT ( 'NONE',  ( 3.379006598303866848, 4.965260336153046516, -1.599625672291262513 ) ) ;
#71179 = CARTESIAN_POINT ( 'NONE',  ( 0.6980877996264934771, 1.427081234210248573, 1.568565553304770877 ) ) ;
#71180 = CARTESIAN_POINT ( 'NONE',  ( -5.260200412422213923, 6.199617238323108737, -1.082531754730544860 ) ) ;
#71181 = AXIS2_PLACEMENT_3D ( 'NONE', #111032, #62222, #213761 ) ;
#71182 = DIRECTION ( 'NONE',  ( 0.000000000000000000, -1.000000000000000000, 0.000000000000000000 ) ) ;
#71183 = CARTESIAN_POINT ( 'NONE',  ( -4.216222583725562245, 7.862750747747711877, 0.7216878364870317197 ) ) ;
#71184 = CARTESIAN_POINT ( 'NONE',  ( -1.387358672527355008, 7.251968950354660493, 4.302625267139497112 ) ) ;
#71186 = VERTEX_POINT ( 'NONE', #36656 ) ;
#71185 =( GEOMETRIC_REPRESENTATION_CONTEXT ( 3 ) GLOBAL_UNCERTAINTY_ASSIGNED_CONTEXT ( ( #5154 ) ) GLOBAL_UNIT_ASSIGNED_CONTEXT ( ( #1434, #85919, #4627 ) ) REPRESENTATION_CONTEXT ( 'NONE', 'WORKASPACE' ) );
#71187 = CARTESIAN_POINT ( 'NONE',  ( 4.887342357109405455, -0.6819942819097268849, -1.897698409216505233 ) ) ;
#71189 = CARTESIAN_POINT ( 'NONE',  ( 3.133693747638730098, 1.960048766001153631, -0.6424893143618380931 ) ) ;
#71188 = CARTESIAN_POINT ( 'NONE',  ( 4.364835388595708743, 7.179726155748598515, 1.199719254218462483 ) ) ;
#71191 = CARTESIAN_POINT ( 'NONE',  ( -0.1411974294642124317, 6.947781193150396994, -2.495311724135263809 ) ) ;
#71190 = CARTESIAN_POINT ( 'NONE',  ( 7.367930134383754215, 7.560616343061329125, -0.7998128361456341429 ) ) ;
#71192 = CARTESIAN_POINT ( 'NONE',  ( 5.905458427204159477, 9.047396044116986502, 1.199719254218452047 ) ) ;
#71193 = CARTESIAN_POINT ( 'NONE',  ( -1.642778471874998480, -2.151041666188707957, 2.845375778867863303 ) ) ;
#71194 = CARTESIAN_POINT ( 'NONE',  ( 8.500000000000000000, 6.120000000000034746, -2.580000000000001403 ) ) ;
#71195 = CARTESIAN_POINT ( 'NONE',  ( 6.720655732516648939, -0.004400176169771368405, 2.173773060281408487 ) ) ;
#71196 = CARTESIAN_POINT ( 'NONE',  ( 4.887342357109405455, -0.6819942819097268849, -1.897698409216505233 ) ) ;
#71197 = CARTESIAN_POINT ( 'NONE',  ( 3.350949008998193257, 0.4442310927498266948, -1.786741727165648497 ) ) ;
#71198 = CARTESIAN_POINT ( 'NONE',  ( 5.144429221381498607, 8.089252293998699272, -1.199719254218452047 ) ) ;
#71199 =( NAMED_UNIT ( * ) SI_UNIT ( $, .STERADIAN. ) SOLID_ANGLE_UNIT ( ) );
#71200 = CARTESIAN_POINT ( 'NONE',  ( 0.9555556167152472469, 1.723134239262851475, -0.07815038326265508206 ) ) ;
#71201 = CARTESIAN_POINT ( 'NONE',  ( -2.656508033273816238, 5.186677574539687363, -1.199719254218446718 ) ) ;
#71202 = CARTESIAN_POINT ( 'NONE',  ( 0.5636314131802122596, -1.270468259257762966, 1.915555708879124852 ) ) ;
#71203 = CARTESIAN_POINT ( 'NONE',  ( -5.900823170445743671, 7.907379670318584353, 1.599625672291269396 ) ) ;
#71204 = CARTESIAN_POINT ( 'NONE',  ( 0.1813603024932753938, -0.1560989159599696641, -2.227174003853182871 ) ) ;
#71205 = CARTESIAN_POINT ( 'NONE',  ( 2.842513320990670778, 2.090244732995512944, 0.2570852942500467808 ) ) ;
#71206 = CARTESIAN_POINT ( 'NONE',  ( -3.461074353238556167, 7.259946855412102273, 0.000000000000000000 ) ) ;
#71207 = CARTESIAN_POINT ( 'NONE',  ( 5.750629710490689384, 9.860818428881154674, -0.7998128361456291469 ) ) ;
#71209 = EDGE_CURVE ( 'NONE', #36899, #25291, #59113, .T. ) ;
#71208 = CARTESIAN_POINT ( 'NONE',  ( 6.387299765369506055, 7.584842826753462219, -1.082531754730548412 ) ) ;
#71210 = CARTESIAN_POINT ( 'NONE',  ( -7.725448601688521322, 7.907444878258402809, 1.040834085586084257E-14 ) ) ;
#71211 = CARTESIAN_POINT ( 'NONE',  ( 6.982085920913413624, 8.208483664896217391, -1.082531754730543971 ) ) ;
#71212 = CARTESIAN_POINT ( 'NONE',  ( 4.556571072163061231, 7.192851904033680910, 1.311937382574361877 ) ) ;
#71213 = CARTESIAN_POINT ( 'NONE',  ( -5.382750679825375251, 6.238629533673094585, -1.199719254218446718 ) ) ;
#71214 = CARTESIAN_POINT ( 'NONE',  ( 4.289451472217206351, -0.001904023060144560469, -2.221583672334653148 ) ) ;
#71215 = CARTESIAN_POINT ( 'NONE',  ( 2.765787700092982693, 1.173089151190203294, 1.850848517565194751 ) ) ;
#71216 = CARTESIAN_POINT ( 'NONE',  ( -4.903245109636583443, 8.872203061218007392, -0.7998128361456281477 ) ) ;
#71217 = CARTESIAN_POINT ( 'NONE',  ( -5.285699784481336927, 7.260012063351913625, 1.599625672291263179 ) ) ;
#71218 = CARTESIAN_POINT ( 'NONE',  ( 5.441838459065293065, 1.316327937319297758, 1.454900926449454124 ) ) ;
#71219 = CARTESIAN_POINT ( 'NONE',  ( -1.364683531250012516, 2.280208333674751842, 0.7879004041258379498 ) ) ;
#71220 = EDGE_CURVE ( 'NONE', #30003, #12895, #43548, .T. ) ;
#71221 = CARTESIAN_POINT ( 'NONE',  ( -4.828112100242303306, 4.805421336470338645, -0.7216878364870338292 ) ) ;
#71223 = CARTESIAN_POINT ( 'NONE',  ( -4.934804725694224459, 6.780358151441803649, -1.443375672974053447 ) ) ;
#71222 = AXIS2_PLACEMENT_3D ( 'NONE', #164300, #148060, #214068 ) ;
#71224 = CARTESIAN_POINT ( 'NONE',  ( 4.553055379497691568, 0.3652949536288411791, 2.088752307168060707 ) ) ;
#71225 = CARTESIAN_POINT ( 'NONE',  ( -5.093022980588950865, 5.970890227889075419, -1.199719254218453823 ) ) ;
#71226 = ORIENTED_EDGE ( 'NONE', *, *, #74380, .T. ) ;
#71228 = CARTESIAN_POINT ( 'NONE',  ( 5.963787895669664607, 2.130530397400759668, -0.3648857593604309391 ) ) ;
#71227 = CARTESIAN_POINT ( 'NONE',  ( -6.183927461608886844, 7.347575139032721303, 1.082531754730548412 ) ) ;
#71229 = CARTESIAN_POINT ( 'NONE',  ( 4.659198344590585350, 8.587481835331020719, 0.7998128361456462443 ) ) ;
#71230 = CARTESIAN_POINT ( 'NONE',  ( 5.495603940606402560, -1.841430844871448258, 0.006098274996368944698 ) ) ;
#71231 = CARTESIAN_POINT ( 'NONE',  ( -5.901845825571131243, 6.006233656505717278, 0.1738135011533047114 ) ) ;
#71232 = CARTESIAN_POINT ( 'NONE',  ( 0.6823417656249882723, 1.488541667008083547, -1.181850606188749264 ) ) ;
#71233 = CARTESIAN_POINT ( 'NONE',  ( 6.351467175048743918, 1.735110083250133162, -0.1355937802150069815 ) ) ;
#71234 = CARTESIAN_POINT ( 'NONE',  ( -9.578206935422372226, -9.900000000000074962, 0.1671882239537618997 ) ) ;
#71235 = CARTESIAN_POINT ( 'NONE',  ( 0.6823417656249864960, -0.7614583329919113464, -1.181850606188749264 ) ) ;
#71236 = CARTESIAN_POINT ( 'NONE',  ( 4.871153761480781164, 8.051123856976298399, 0.9350251597124116243 ) ) ;
#71237 = CARTESIAN_POINT ( 'NONE',  ( 3.590839768554392908, -0.4196827604958653923, -2.120402733634827452 ) ) ;
#71238 = CARTESIAN_POINT ( 'NONE',  ( -5.111587607552082524, 5.922272616020886282, 1.199719254218450271 ) ) ;
#71239 = PRESENTATION_LAYER_ASSIGNMENT (  '', '', ( #36620 ) ) ;
#71240 = CARTESIAN_POINT ( 'NONE',  ( -7.090551149822745813, 9.295395646258437949, 1.443375672974078761 ) ) ;
#71241 = CARTESIAN_POINT ( 'NONE',  ( 3.661132068870280420, -1.905464569931826446, -1.020879743040298271 ) ) ;
#71242 = CARTESIAN_POINT ( 'NONE',  ( 4.639890180388304586, 0.8457560770286243201, -1.780867954887039417 ) ) ;
#71243 = CARTESIAN_POINT ( 'NONE',  ( 3.831122626782780927, -1.165689738437695189, 1.283648893705439331 ) ) ;
#71244 = CARTESIAN_POINT ( 'NONE',  ( 1.329895901633147748, 1.076045675571284166, -1.909117696414885934 ) ) ;
#71245 = CARTESIAN_POINT ( 'NONE',  ( 2.327567518148494941, 0.0001997265634129384874, 2.307758715027211416 ) ) ;
#71246 = CARTESIAN_POINT ( 'NONE',  ( 3.216142984300340846, -1.012526663717785214, -1.794778392713367587 ) ) ;
#71247 = CARTESIAN_POINT ( 'NONE',  ( 5.776890131463271238, 1.792767593593114439, -0.7471807142077312447 ) ) ;
#71249 = ORIENTED_EDGE ( 'NONE', *, *, #9318, .T. ) ;
#71248 = CARTESIAN_POINT ( 'NONE',  ( -7.659993601596710278, 10.92011438762942355, -1.082531754730543083 ) ) ;
#71250 = CIRCLE ( 'NONE', #192316, 0.07999999999999993228 ) ;
#71251 = CARTESIAN_POINT ( 'NONE',  ( -6.143779885648060102, 7.196773283791382703, 1.199719254218452047 ) ) ;
#71252 = FILL_AREA_STYLE_COLOUR ( '', #123459 ) ;
#71253 = CARTESIAN_POINT ( 'NONE',  ( -4.004454267989906668, 5.765225627445230927, 1.599625672291270506 ) ) ;
#71254 = CARTESIAN_POINT ( 'NONE',  ( -7.998947441938374148, 8.434452891790657603, 1.040834085586084257E-14 ) ) ;
#71255 = EDGE_CURVE ( 'NONE', #134733, #213643, #167735, .T. ) ;
#71256 = CARTESIAN_POINT ( 'NONE',  ( 3.505080564089088746, 1.740947047783932611, -1.355986173033681075 ) ) ;
#71257 = CARTESIAN_POINT ( 'NONE',  ( 3.285556943750000514, -2.851041666188706802, 1.896917185911906500 ) ) ;
#71258 = ORIENTED_EDGE ( 'NONE', *, *, #121971, .F. ) ;
#71259 = CARTESIAN_POINT ( 'NONE',  ( 1.111883761159220496, 1.859168010044176311, -0.08395930885315286418 ) ) ;
#71260 = CARTESIAN_POINT ( 'NONE',  ( -0.02900071798683095947, 5.719935618195115978, -2.767867108847458901 ) ) ;
#71261 = PRESENTATION_STYLE_ASSIGNMENT (( #103800 ) ) ;
#71263 = CARTESIAN_POINT ( 'NONE',  ( 6.825078400183582694, 7.052246674313852992, 2.642498189888539795 ) ) ;
#71262 = CARTESIAN_POINT ( 'NONE',  ( -6.026230196168996578, 7.163122537909742071, -1.192248477780058380 ) ) ;
#71264 = CARTESIAN_POINT ( 'NONE',  ( 6.509700743154069436, -0.8726169035938921015, -1.621212818125779220 ) ) ;
#71265 = EDGE_LOOP ( 'NONE', ( #168377, #162085, #147301, #182738 ) ) ;
#71266 = CARTESIAN_POINT ( 'NONE',  ( 3.168876024238317601, -1.903602637213364979, -0.7901525784780991657 ) ) ;
#71267 = CARTESIAN_POINT ( 'NONE',  ( 0.6801582343749935644, -0.02604166632526327962, 1.178068619123817218 ) ) ;
#71268 = CARTESIAN_POINT ( 'NONE',  ( -4.934277840369690971, 7.844075682818238526, -1.199719254218452047 ) ) ;
#71269 = CARTESIAN_POINT ( 'NONE',  ( 0.07680821025391608436, 0.2560392329899116026, -1.846278364303982178 ) ) ;
#71270 = CARTESIAN_POINT ( 'NONE',  ( 4.253507506385319381, 5.985511395581417204, 1.599625672291267398 ) ) ;
#71271 = EDGE_CURVE ( 'NONE', #170224, #172377, #59972, .T. ) ;
#71272 = CARTESIAN_POINT ( 'NONE',  ( 2.430605206563386300, 1.998658846558550195, 0.5020661504441750189 ) ) ;
#71274 = CARTESIAN_POINT ( 'NONE',  ( -1.364683531250010295, 12.63020833367473372, 0.7879004041258445001 ) ) ;
#71273 = CARTESIAN_POINT ( 'NONE',  ( -0.7500000000000179856, 12.54166666666666607, 1.299038105676658228 ) ) ;
#71275 = CARTESIAN_POINT ( 'NONE',  ( 7.467843683028853263, 7.606905806488803101, 0.7998128361456341429 ) ) ;
#71276 = DIRECTION ( 'NONE',  ( 0.8660254037844327124, 0.000000000000000000, -0.5000000000000102141 ) ) ;
#71277 = CARTESIAN_POINT ( 'NONE',  ( 5.426482453889071245, 1.317083479513626587, -1.770629405693980640 ) ) ;
#71278 = CARTESIAN_POINT ( 'NONE',  ( 0.6499751493908960676, 0.6786997614584532323, -2.052318101833712660 ) ) ;
#71279 = CARTESIAN_POINT ( 'NONE',  ( -4.446711195602245148, 7.171284913969171448, -1.082531754730549967 ) ) ;
#71280 = CARTESIAN_POINT ( 'NONE',  ( 0.2336117360935245635, 0.6279853779636718203, -1.916355031878452797 ) ) ;
#71281 = CARTESIAN_POINT ( 'NONE',  ( 1.494008433901512278, 2.215370577347621328, 0.6118545706256629524 ) ) ;
#71282 = CARTESIAN_POINT ( 'NONE',  ( 4.641416471958547341, 8.415375545968219129, 0.6158420707860997600 ) ) ;
#71283 = EDGE_CURVE ( 'NONE', #128332, #96549, #29692, .T. ) ;
#71284 = CARTESIAN_POINT ( 'NONE',  ( 6.199862383955294654, 1.322219258337012704, 1.381733411008022383 ) ) ;
#71285 = CARTESIAN_POINT ( 'NONE',  ( 2.969872605471104876, 6.605953636086679737, -0.06813560672779371552 ) ) ;
#71286 = CARTESIAN_POINT ( 'NONE',  ( 1.709613803025863188, -1.856884215550944850, 0.2259493607114013147 ) ) ;
#71287 = CARTESIAN_POINT ( 'NONE',  ( 3.415250174187448362, -1.861344788686780438, 0.7762291900053899241 ) ) ;
#71289 = CARTESIAN_POINT ( 'NONE',  ( 2.286103771890017011, 5.558832614202657396, -0.5700755669254429225 ) ) ;
#71288 = CARTESIAN_POINT ( 'NONE',  ( 1.364683531249988757, 0.6343750003414208027, 0.000000000000000000 ) ) ;
#71291 = CARTESIAN_POINT ( 'NONE',  ( 4.934254457356054502, 1.083321712992061814, -1.805932085151832789 ) ) ;
#71290 = CARTESIAN_POINT ( 'NONE',  ( -7.004758919754800139, 11.32396917302262018, 0.000000000000000000 ) ) ;
#71292 = CARTESIAN_POINT ( 'NONE',  ( 6.421758314367153275, 10.64380180007036891, -0.7998128361456291469 ) ) ;
#71294 = CARTESIAN_POINT ( 'NONE',  ( -7.739006755302186846, 7.923262724141010516, 0.7998128361456462443 ) ) ;
#71293 = CARTESIAN_POINT ( 'NONE',  ( 5.910428620914669473, 5.860197910680708944, 0.000000000000000000 ) ) ;
#71295 = CARTESIAN_POINT ( 'NONE',  ( -0.2167848519283963049, -6.775781654326366699, -9.491250020638732465 ) ) ;
#71296 = CARTESIAN_POINT ( 'NONE',  ( 4.289322773248661846, -0.004189350761124934451, -2.019972750201783906 ) ) ;
#71297 = CARTESIAN_POINT ( 'NONE',  ( -0.6823417656249969321, 4.967708333674755394, -1.181850606188749264 ) ) ;
#71298 = CARTESIAN_POINT ( 'NONE',  ( 6.830530959611283315, -1.272493244265305634, 1.624195267664030995 ) ) ;
#71299 = CARTESIAN_POINT ( 'NONE',  ( 10.23604278863759909, 11.04439746293979496, 0.000000000000000000 ) ) ;
#71300 = CARTESIAN_POINT ( 'NONE',  ( 5.220075184997099882, -1.151474455836385857, -1.829185309946822713 ) ) ;
#71301 = CARTESIAN_POINT ( 'NONE',  ( 6.068156270568149324, 9.237210194708310951, 1.199719254218452047 ) ) ;
#71302 = CARTESIAN_POINT ( 'NONE',  ( -1.364683531250014514, -0.9489583329919112353, -0.7879004041258359514 ) ) ;
#71304 = CYLINDRICAL_SURFACE ( 'NONE', #51751, 2.025000000000006573 ) ;
#71303 = CARTESIAN_POINT ( 'NONE',  ( 6.690022453700429139, 6.769724048930809701, 0.7998128361456331437 ) ) ;
#71305 = CARTESIAN_POINT ( 'NONE',  ( 8.283668667825342169, 9.726996869626816533, -1.082531754730543083 ) ) ;
#71307 = CARTESIAN_POINT ( 'NONE',  ( 2.065456695249153540, 8.523797939977239224, 2.459872958007392807 ) ) ;
#71306 = CARTESIAN_POINT ( 'NONE',  ( 2.594372030776093574, 1.025359171358769306, -1.913825152921688311 ) ) ;
#71309 = CARTESIAN_POINT ( 'NONE',  ( 1.856743374925871715, 0.3135980649527739250, -1.814175028193690808 ) ) ;
#71308 = CARTESIAN_POINT ( 'NONE',  ( -6.127922243696855453, 7.211959374810172463, 1.082531754730549967 ) ) ;
#71310 = STYLED_ITEM ( 'NONE', ( #153162 ), #16025 ) ;
#71311 = CARTESIAN_POINT ( 'NONE',  ( -0.6823417656250003738, 2.967708333674754062, -1.181850606188749264 ) ) ;
#71312 = CARTESIAN_POINT ( 'NONE',  ( 3.720431430916489646, 2.081484170424623859, 0.6860852429351402826 ) ) ;
#71313 = CARTESIAN_POINT ( 'NONE',  ( 6.983263157960363010, 6.034173670577698267, 2.748703042679788044 ) ) ;
#71314 = CARTESIAN_POINT ( 'NONE',  ( 4.241306175801488720, -1.970289653591940970, 1.112044505652502346 ) ) ;
#71315 = CARTESIAN_POINT ( 'NONE',  ( -5.961834861707238531, 7.978559976790334574, -1.599625672291263179 ) ) ;
#71316 = LINE ( 'NONE', #101708, #139012 ) ;
#71317 = CARTESIAN_POINT ( 'NONE',  ( 6.423677080210483226, 6.791898735554919853, -0.4454198846488600649 ) ) ;
#71318 = CARTESIAN_POINT ( 'NONE',  ( 1.500000000000001332, 13.87499999999999822, 0.000000000000000000 ) ) ;
#71319 = CARTESIAN_POINT ( 'NONE',  ( 4.855228407469603269, 7.718164671139588151, -1.082531754730548412 ) ) ;
#71320 =( BOUNDED_CURVE ( )  B_SPLINE_CURVE ( 2, ( #189543, #41191, #124641, #105123, #88870, #92076, #91006, #154924, #157068 ),
 .UNSPECIFIED., .F., .T. ) 
 B_SPLINE_CURVE_WITH_KNOTS ( ( 3, 2, 2, 2, 3 ),
 ( 0.01562500000000013531, 0.02083333333333333218, 0.03125000000000000000, 0.04166666666666666435, 0.04687499999999977796 ),
 .UNSPECIFIED. ) 
 CURVE ( )  GEOMETRIC_REPRESENTATION_ITEM ( )  RATIONAL_B_SPLINE_CURVE ( ( 0.9330127018922194093, 0.9330127018922211857, 1.000000000000000000, 0.8660254037844387076, 1.000000000000000000, 0.8660254037844387076, 1.000000000000000000, 0.9330127018922221849, 0.9330127018922194093 ) ) 
 REPRESENTATION_ITEM ( '' )  );
#71321 = CARTESIAN_POINT ( 'NONE',  ( 5.483597806724121781, 1.189268614677735592, 1.310771863001722437 ) ) ;
#71322 = CARTESIAN_POINT ( 'NONE',  ( 7.853197290813620945, 10.18514947741448573, 1.599625672291281386 ) ) ;
#71323 = CARTESIAN_POINT ( 'NONE',  ( 1.360533241671294746, 0.8531190763820644118, 1.925603555557230617 ) ) ;
#71325 = CARTESIAN_POINT ( 'NONE',  ( 1.499999999999989120, 2.275000000000019895, 1.214306433183764966E-14 ) ) ;
#71324 = CARTESIAN_POINT ( 'NONE',  ( 1.364683531249996529, 12.46354166700806054, 0.7879004041258405033 ) ) ;
#71326 = CARTESIAN_POINT ( 'NONE',  ( 1.715229078707868782, -1.687648322675440626, -1.015142298990583614 ) ) ;
#71327 = CARTESIAN_POINT ( 'NONE',  ( -3.471769853551161411, 6.208092708188416076, 1.199719254218452935 ) ) ;
#71328 = CARTESIAN_POINT ( 'NONE',  ( 1.250000000000037526, 8.500000000000000000, -10.97907099895068583 ) ) ;
#71330 = VERTEX_POINT ( 'NONE', #213266 ) ;
#71329 = CARTESIAN_POINT ( 'NONE',  ( 5.677939507029830857, 1.783257022268599723, -0.3182440143107477248 ) ) ;
#71331 = CARTESIAN_POINT ( 'NONE',  ( 7.293923454472091450, 7.611924906413328529, 0.7216878364870317197 ) ) ;
#71332 = CARTESIAN_POINT ( 'NONE',  ( 0.4437637753827078924, 3.174217730513756663, -1.950200034575564123 ) ) ;
#71334 = CARTESIAN_POINT ( 'NONE',  ( 5.067206508511894469, 0.1826785619755930679, -1.861722072867748823 ) ) ;
#71333 = COLOUR_RGB ( '', 0.66274510, 0.83137255, 0.94901961) ;
#71335 = CARTESIAN_POINT ( 'NONE',  ( 5.102424979711988051, 2.064335680360945169, 0.1577259720206558580 ) ) ;
#71336 = CARTESIAN_POINT ( 'NONE',  ( 1.224999999999959233, 2.104166666666714480, 0.7072540797572757221 ) ) ;
#71337 = CARTESIAN_POINT ( 'NONE',  ( -5.817857313595549584, 6.920493299683823096, 1.082531754730549078 ) ) ;
#71338 = CARTESIAN_POINT ( 'NONE',  ( 1.683015768249133348, -0.9661576380125261876, 2.984288236375972403 ) ) ;
#71340 = CARTESIAN_POINT ( 'NONE',  ( 1.499999999999987121, 1.004166666666687968, 0.8660254037844524744 ) ) ;
#71339 = CIRCLE ( 'NONE', #33315, 0.08000000000000020983 ) ;
#71341 = CARTESIAN_POINT ( 'NONE',  ( 6.588372581236919601, 9.773852880496709972, -1.199719254218440723 ) ) ;
#71342 = CARTESIAN_POINT ( 'NONE',  ( -7.980945979938748103, 12.46285407657057220, 0.000000000000000000 ) ) ;
#71343 = CARTESIAN_POINT ( 'NONE',  ( 6.638652492546827766, 7.774124658506663010, 1.199719254218452047 ) ) ;
#71344 = CARTESIAN_POINT ( 'NONE',  ( 0.6823417656249882723, 0.3427083336747516196, 1.181850606188755259 ) ) ;
#71345 = CARTESIAN_POINT ( 'NONE',  ( 1.499999999999987121, 1.504166666666690411, 0.8660254037844524744 ) ) ;
#71347 = CARTESIAN_POINT ( 'NONE',  ( 3.798255590122797898, 7.583048621785260401, -0.7998128361456221525 ) ) ;
#71346 = CARTESIAN_POINT ( 'NONE',  ( 4.650807877244386823, -0.4278111053654386486, -1.914496481071884970 ) ) ;
#71348 = CARTESIAN_POINT ( 'NONE',  ( 1.950545848857932807, 1.388271641964162084, 1.462223312268404074 ) ) ;
#71349 = EDGE_CURVE ( 'NONE', #24990, #82008, #125069, .T. ) ;
#71350 = CARTESIAN_POINT ( 'NONE',  ( 2.342874207364954220, -1.669023557642179467, -0.9401844802782586275 ) ) ;
#71351 = CARTESIAN_POINT ( 'NONE',  ( -1.084637062511542016, 2.898878807974804239, -1.105835307554790647 ) ) ;
#71352 = CARTESIAN_POINT ( 'NONE',  ( 0.4334776158547505864, -1.553986563932317377, -1.545601477622601472 ) ) ;
#71353 = CARTESIAN_POINT ( 'NONE',  ( 6.539320575229252697, 0.01001626003939219342, 1.796977979958066518 ) ) ;
#71354 = CARTESIAN_POINT ( 'NONE',  ( 2.424885678431305092, -0.004389691185376768875, 1.870726058193001196 ) ) ;
#71355 = CARTESIAN_POINT ( 'NONE',  ( -0.6823417656249969321, 5.467708333674756283, -1.181850606188749264 ) ) ;
#71356 = CARTESIAN_POINT ( 'NONE',  ( 4.429943789601535009, -1.973532241649661678, 0.3969061482532297291 ) ) ;
#71357 = CARTESIAN_POINT ( 'NONE',  ( -9.020252271793614440, 9.418049160047695878, 0.7998128361456462443 ) ) ;
#71359 = CARTESIAN_POINT ( 'NONE',  ( 4.657876698301413043, 1.220176935102987636, 1.730081886799080593 ) ) ;
#71358 = CARTESIAN_POINT ( 'NONE',  ( -6.412643469583822586, 6.583764924043652655, 1.040834085586084257E-14 ) ) ;
#71360 = CARTESIAN_POINT ( 'NONE',  ( 9.579665964948882007, -7.325744180092283564, 1.734723475976807094E-15 ) ) ;
#71361 = CARTESIAN_POINT ( 'NONE',  ( 5.828598057497599960, -1.316348130051235410, 1.597988563933512074 ) ) ;
#71363 = CARTESIAN_POINT ( 'NONE',  ( 6.720655732516624070, 2.949086357957014570, 2.625980845328681923 ) ) ;
#71362 = CARTESIAN_POINT ( 'NONE',  ( 1.153981415136243527, 0.8505622500237058903, 1.910110313709513674 ) ) ;
#71365 = ORIENTED_EDGE ( 'NONE', *, *, #162949, .T. ) ;
#71364 = CARTESIAN_POINT ( 'NONE',  ( 6.616225513087798049, -0.8637638766970030524, -1.608286988965562214 ) ) ;
#71366 = CARTESIAN_POINT ( 'NONE',  ( 6.564118927310645724, 10.80988918183778225, -0.7998128361456291469 ) ) ;
#71367 = CARTESIAN_POINT ( 'NONE',  ( -6.056815632531343141, 6.015240258500212711, 0.3115616189311651296 ) ) ;
#71368 = CARTESIAN_POINT ( 'NONE',  ( 9.729489633724101694, 13.21513059140455759, -8.104625967152696120 ) ) ;
#71369 = CARTESIAN_POINT ( 'NONE',  ( -10.73969341588288628, 4.108126672274917013, 4.807887712954548753 ) ) ;
#71370 = CARTESIAN_POINT ( 'NONE',  ( 7.592202833528386208, 7.959917515312338487, 1.040834085586084257E-14 ) ) ;
#71371 = CARTESIAN_POINT ( 'NONE',  ( 1.364683531250000748, 13.06770833367473372, -0.7879004041258355073 ) ) ;
#71372 = CARTESIAN_POINT ( 'NONE',  ( 0.8381711186948238579, 1.079942214367535680, -1.454201162973115524 ) ) ;
#71374 = CARTESIAN_POINT ( 'NONE',  ( -7.802881099864745984, 9.062115023719057305, -1.199719254218446718 ) ) ;
#71373 = COLOUR_RGB ( '', 0.40784314, 0.44705882, 0.49803922) ;
#71375 =( BOUNDED_SURFACE ( )  B_SPLINE_SURFACE ( 3, 2, ( 
 ( #93745, #76395, #77463 ),
 ( #13527, #192263, #44992 ),
 ( #10321, #79599, #29797 ),
 ( #126304, #145718, #212783 ),
 ( #129511, #158724, #142504 ),
 ( #208512, #112177, #211716 ),
 ( #12450, #11385, #143581 ),
 ( #180307, #28723, #176052 ),
 ( #159783, #63353, #43925 ),
 ( #177107, #195492, #61219 ),
 ( #210661, #127376, #160858 ),
 ( #130564, #60146, #110040 ),
 ( #27645, #209574, #193348 ),
 ( #14579, #111101, #47127 ),
 ( #94809, #78528, #144645 ),
 ( #62287, #48196, #128447 ),
 ( #162998, #179247, #178182 ),
 ( #194414, #46056, #95881 ) ),
 .UNSPECIFIED., .F., .F., .T. ) 
 B_SPLINE_SURFACE_WITH_KNOTS ( ( 4, 2, 2, 2, 2, 2, 2, 2, 4 ),
 ( 3, 3 ),
 ( 0.001893572594152293821, 0.002130269168421383350, 0.002366965742690472444, 0.002603662316959561539, 0.002840358891228651067, 0.003077055465497740595, 0.003313752039766830124, 0.003550448614035919652, 0.003787145188305008747 ),
 ( 0.000000000000000000, 1.000000000000000000 ),
 .UNSPECIFIED. ) 
 GEOMETRIC_REPRESENTATION_ITEM ( )  RATIONAL_B_SPLINE_SURFACE ( (
 ( 1.000000000000000000, 0.5649783097559765155, 1.000000000000000000),
 ( 1.000000000000000000, 0.5467450299869772712, 1.000000000000000000),
 ( 1.000000000000000000, 0.5350701846666650052, 1.000000000000000000),
 ( 1.000000000000000000, 0.5340147030925761484, 1.000000000000000000),
 ( 1.000000000000000000, 0.5447811154896697872, 1.000000000000000000),
 ( 1.000000000000000000, 0.5795975317820121209, 1.000000000000000000),
 ( 1.000000000000000000, 0.6028840214606389081, 1.000000000000000000),
 ( 1.000000000000000000, 0.6474634991924413940, 1.000000000000000000),
 ( 1.000000000000000000, 0.6683065367292350123, 1.000000000000000000),
 ( 1.000000000000000000, 0.6980320384851331772, 1.000000000000000000),
 ( 1.000000000000000000, 0.7066998895408397319, 1.000000000000000000),
 ( 1.000000000000000000, 0.7074845257686436240, 1.000000000000000000),
 ( 1.000000000000000000, 0.6995439292594691771, 1.000000000000000000),
 ( 1.000000000000000000, 0.6710262760327128095, 1.000000000000000000),
 ( 1.000000000000000000, 0.6504357685074378947, 1.000000000000000000),
 ( 1.000000000000000000, 0.6062099919889085697, 1.000000000000000000),
 ( 1.000000000000000000, 0.5828135443829817186, 1.000000000000000000),
 ( 1.000000000000000000, 0.5647844906712726765, 1.000000000000000000) ) ) 
 REPRESENTATION_ITEM ( '' )  SURFACE ( )  );
#71376 = CARTESIAN_POINT ( 'NONE',  ( 5.656776405399742025, 7.622658444431597680, -1.599625672291262513 ) ) ;
#71377 = CARTESIAN_POINT ( 'NONE',  ( -6.595517585942705985, -7.896420114628011078, -7.253242555595321939 ) ) ;
#71378 = CARTESIAN_POINT ( 'NONE',  ( 3.890826896997583884, 4.602014803661035103, -1.082531754730543083 ) ) ;
#71379 = CARTESIAN_POINT ( 'NONE',  ( -2.255140518769849223E-14, 3.249999999999988898, -4.336808689942017736E-14 ) ) ;
#71380 = CARTESIAN_POINT ( 'NONE',  ( 3.816783937446950770, 4.411668334231586996, 1.199719254218464037 ) ) ;
#71381 = ORIENTED_EDGE ( 'NONE', *, *, #57852, .T. ) ;
#71382 = CIRCLE ( 'NONE', #185652, 0.08000000000000020983 ) ;
#71383 = CARTESIAN_POINT ( 'NONE',  ( 6.538686444676896414, -1.556836737174282836, 1.281159629702780078 ) ) ;
#71384 = CARTESIAN_POINT ( 'NONE',  ( 3.009610312849396951, 6.452363523749469643, -0.06592220986071165023 ) ) ;
#71385 = CARTESIAN_POINT ( 'NONE',  ( -9.305047016969982820, 15.51845925588232333, 7.450000000803896683 ) ) ;
#71386 = CARTESIAN_POINT ( 'NONE',  ( 2.274666334179356930, 5.653847144074187980, 0.5136602295931251838 ) ) ;
#71387 = CARTESIAN_POINT ( 'NONE',  ( -5.585596099150193616, 6.579245539505756746, -1.082531754730544860 ) ) ;
#71388 = CARTESIAN_POINT ( 'NONE',  ( 9.788623719386617239, 11.48277776311499387, -1.082531754730537088 ) ) ;
#71389 = CARTESIAN_POINT ( 'NONE',  ( 3.502752968683011225, 0.4741538486671539876, 1.911403532405174133 ) ) ;
#71390 = CARTESIAN_POINT ( 'NONE',  ( 4.306267660493944049, 1.238306454277863677, -1.591331080693689781 ) ) ;
#71391 = CARTESIAN_POINT ( 'NONE',  ( -5.520141099058386125, 9.591915048876776595, 0.000000000000000000 ) ) ;
#71393 = EDGE_CURVE ( 'NONE', #92178, #25559, #156067, .T. ) ;
#71392 = CARTESIAN_POINT ( 'NONE',  ( -1.500000000000001110, 10.27083333333332860, 0.8660254037844418162 ) ) ;
#71394 = CARTESIAN_POINT ( 'NONE',  ( 4.822331674454460426, 2.096538211656114647, 0.6379635903819569354 ) ) ;
#71395 = CARTESIAN_POINT ( 'NONE',  ( 5.974410882859532812, 4.760127796209649098, 2.438793965253449159 ) ) ;
#71396 = CARTESIAN_POINT ( 'NONE',  ( 3.504829168241951898, 1.519505285488613744, -1.184012928881588822 ) ) ;
#71397 = CARTESIAN_POINT ( 'NONE',  ( -6.008234629150358330, 10.16135750065076060, 0.000000000000000000 ) ) ;
#71398 = CARTESIAN_POINT ( 'NONE',  ( -0.1296875068448125057, 7.629137130509072939, -2.426516348560475933 ) ) ;
#71399 = CARTESIAN_POINT ( 'NONE',  ( 0.06543086261080394150, -1.973449318085427340, -0.9880335165917543128 ) ) ;
#71400 = CARTESIAN_POINT ( 'NONE',  ( 1.364683531250000748, 13.25520833367473017, -0.7879004041258355073 ) ) ;
#71401 = ORIENTED_EDGE ( 'NONE', *, *, #33667, .F. ) ;
#71402 = CARTESIAN_POINT ( 'NONE',  ( 4.746763178560254204, 6.631252689777363152, 1.443375672974065660 ) ) ;
#71403 = CARTESIAN_POINT ( 'NONE',  ( 5.137539950512164388, 1.839066438578255136, -0.7051811603524612559 ) ) ;
#71404 = VERTEX_POINT ( 'NONE', #201273 ) ;
#71406 = CARTESIAN_POINT ( 'NONE',  ( 4.459639246686514902, -1.557681092447872784, -1.275236256583739403 ) ) ;
#71405 = CARTESIAN_POINT ( 'NONE',  ( 0.3451281418221859854, 0.6079892978090885025, -1.844522312511005957 ) ) ;
#71407 = CARTESIAN_POINT ( 'NONE',  ( 5.694729993868760332, -1.451380474000956156, -1.782189233907914838 ) ) ;
#71409 = CARTESIAN_POINT ( 'NONE',  ( 3.326847623520872155, -1.717698991579403422, -0.7164791247627964044 ) ) ;
#71408 = CARTESIAN_POINT ( 'NONE',  ( -6.933015448541747006, 9.181880338089085214, 1.599625672291269396 ) ) ;
#71410 = CARTESIAN_POINT ( 'NONE',  ( 6.875920180786008196, 8.050936961452347163, -1.199719254218452047 ) ) ;
#71412 = EDGE_CURVE ( 'NONE', #207604, #185122, #150912, .T. ) ;
#71411 = CARTESIAN_POINT ( 'NONE',  ( 6.938893903907228378E-15, 10.64264068711930733, 1.214306433183764966E-14 ) ) ;
#71413 = FILL_AREA_STYLE_COLOUR ( '', #105951 ) ;
#71414 = CARTESIAN_POINT ( 'NONE',  ( -7.379715684540041565, 7.504089808251839244, 1.040834085586084257E-14 ) ) ;
#71415 = CARTESIAN_POINT ( 'NONE',  ( -3.987506576194992824, 7.666191748953863794, 0.7216878364870338292 ) ) ;
#71416 = CARTESIAN_POINT ( 'NONE',  ( 6.093324021728765416, -0.7037842761165017391, 1.968882989559454622 ) ) ;
#71417 = CARTESIAN_POINT ( 'NONE',  ( 4.853455804012212660, 7.645820290447483458, 1.082531754730558626 ) ) ;
#71418 = EDGE_LOOP ( 'NONE', ( #9061, #111989, #131824, #27172 ) ) ;
#71419 = CARTESIAN_POINT ( 'NONE',  ( -2.081668171172168513E-14, 6.487495393664096888, 3.100011470320013451 ) ) ;
#71420 = DIRECTION ( 'NONE',  ( 1.561251128379126077E-17, 1.301042606982605475E-17, 1.000000000000000000 ) ) ;
#71421 = CARTESIAN_POINT ( 'NONE',  ( -0.005637892868452093476, -0.3948761927005627337, -1.788892068844874395 ) ) ;
#71422 = CARTESIAN_POINT ( 'NONE',  ( -5.599681137644054729, 6.491715067794862293, 1.199719254218450271 ) ) ;
#71423 = CARTESIAN_POINT ( 'NONE',  ( 2.232704217388951751, 1.733830997258398066, 0.04099941454244887540 ) ) ;
#71424 = CARTESIAN_POINT ( 'NONE',  ( 0.3282377607281107279, 1.988835450998174492, -1.225000000000013411 ) ) ;
#71425 = CARTESIAN_POINT ( 'NONE',  ( 6.509000000000037645, 2.054060622569788386, 2.307050226316338382 ) ) ;
#71426 = CARTESIAN_POINT ( 'NONE',  ( -6.718228810771495141, 7.796687353110217877, 1.199719254218450271 ) ) ;
#71427 = CARTESIAN_POINT ( 'NONE',  ( -5.911302602197302747, 6.000609024624352195, 0.1125370128407701259 ) ) ;
#71428 = CARTESIAN_POINT ( 'NONE',  ( 0.4442981077158770775, -0.9790059121952739973, 1.824179074426744762 ) ) ;
#71429 = CARTESIAN_POINT ( 'NONE',  ( 5.162654993523497993, -1.319871331358621669, 1.261628347558927166 ) ) ;
#71430 = CARTESIAN_POINT ( 'NONE',  ( 3.326955106232618586, -1.810811308836293598, -0.7551016064811162387 ) ) ;
#71431 = CARTESIAN_POINT ( 'NONE',  ( -1.225000000000026512, -0.6874999993171926338, -2.428612866367529932E-14 ) ) ;
#71432 = CARTESIAN_POINT ( 'NONE',  ( -8.157201976916404362, 12.66848607304450702, -0.7998128361456281477 ) ) ;
#71433 = CARTESIAN_POINT ( 'NONE',  ( 7.287671262545424966, 8.461036880179857889, -1.199719254218451159 ) ) ;
#71434 = CARTESIAN_POINT ( 'NONE',  ( 3.826904873358004888, 1.498484187726952799, -1.500593194838243605 ) ) ;
#71435 = CARTESIAN_POINT ( 'NONE',  ( 6.210516883511641772, 9.403297576475722508, 1.199719254218452047 ) ) ;
#71436 = CARTESIAN_POINT ( 'NONE',  ( -8.123306592882240551, 12.62894145833798376, 0.000000000000000000 ) ) ;
#71437 = EDGE_CURVE ( 'NONE', #61441, #198330, #18263, .T. ) ;
#71438 = CARTESIAN_POINT ( 'NONE',  ( 1.288034235163344254, -1.310400469390052836, -1.602789277989056238 ) ) ;
#71440 = CARTESIAN_POINT ( 'NONE',  ( 0.7500000000000006661, 14.61458333401613530, 1.299038105676657340 ) ) ;
#71439 = CARTESIAN_POINT ( 'NONE',  ( -11.94105721839851952, 11.02698343341132947, 1.187919402540718927 ) ) ;
#71442 = ORIENTED_EDGE ( 'NONE', *, *, #95883, .F. ) ;
#71441 = CARTESIAN_POINT ( 'NONE',  ( 4.565202069552391606, -1.784334575089935981, 1.322790477621762051 ) ) ;
#71443 = CARTESIAN_POINT ( 'NONE',  ( 1.389710824352110574, -0.8328434156393785814, -2.142668459815112669 ) ) ;
#71445 = CARTESIAN_POINT ( 'NONE',  ( 0.4792544977638459880, -0.1021076105021078151, 1.959249876678282209 ) ) ;
#71444 = CARTESIAN_POINT ( 'NONE',  ( 8.758204044747994743, 12.20135990463928266, 1.082531754730546636 ) ) ;
#71447 = CARTESIAN_POINT ( 'NONE',  ( 0.000000000000000000, -0.4374999999999981126, -4.012584370867899430 ) ) ;
#71446 = CARTESIAN_POINT ( 'NONE',  ( 6.211043768836170820, 9.299949259400630552, 1.082531754730549967 ) ) ;
#71448 = CARTESIAN_POINT ( 'NONE',  ( -1.734723475976807094E-15, 2.999999999999988898, -6.938893903907228378E-15 ) ) ;
#71449 = CARTESIAN_POINT ( 'NONE',  ( 6.321814700078944860, 1.054209175812788502, -1.509406368332133930 ) ) ;
#71450 = CARTESIAN_POINT ( 'NONE',  ( -5.558128722462742033, 6.219596756869237630, -0.9274318607392477709 ) ) ;
#71451 = CARTESIAN_POINT ( 'NONE',  ( 2.865378420500460876, -1.565876230000915692, -1.097592462808501645 ) ) ;
#71452 = CARTESIAN_POINT ( 'NONE',  ( -0.4997071982806468582, 6.813474644879237374, -3.717966193172169920 ) ) ;
#71453 = CARTESIAN_POINT ( 'NONE',  ( 3.680403716343355836, -1.662106674541915075, -0.4603510507015916020 ) ) ;
#71454 = CARTESIAN_POINT ( 'NONE',  ( 2.589077643123653072, 1.706113014995232380, 1.074661422923957055 ) ) ;
#71455 = CARTESIAN_POINT ( 'NONE',  ( 3.692236332591435577, 1.971970683719068695, 1.181021729054130054 ) ) ;
#71456 = CARTESIAN_POINT ( 'NONE',  ( 3.163607282743227334, 0.3354078767881124024, -2.237311900363625483 ) ) ;
#71457 = CARTESIAN_POINT ( 'NONE',  ( 6.568975480045090798, -1.924755568788787397, -0.8553139683228675461 ) ) ;
#71458 = CARTESIAN_POINT ( 'NONE',  ( -4.611181642423629157, 7.433443445252599702, 1.082531754730549967 ) ) ;
#71459 = CARTESIAN_POINT ( 'NONE',  ( 4.358513420383302694, -1.312205524322278549, 1.187683162289454142 ) ) ;
#71461 = CARTESIAN_POINT ( 'NONE',  ( 1.148812421071528256, -1.804313360470580108, 1.413740901141118611 ) ) ;
#71460 = CARTESIAN_POINT ( 'NONE',  ( 5.677832469072920496, 9.846164657218904992, 0.000000000000000000 ) ) ;
#71462 = CARTESIAN_POINT ( 'NONE',  ( 5.560457619783242933, -1.666209093894938764, -0.7835883864039174806 ) ) ;
#71463 = CARTESIAN_POINT ( 'NONE',  ( -2.774614992291035698, 6.388801257648172971, 1.040834085586084257E-14 ) ) ;
#71464 = CARTESIAN_POINT ( 'NONE',  ( 6.140607899229071798, -1.853288307406484536, 1.169240172944140621 ) ) ;
#71465 = CARTESIAN_POINT ( 'NONE',  ( -3.630551273409382329, 7.457669928944732796, 0.7998128361456352531 ) ) ;
#71466 = CARTESIAN_POINT ( 'NONE',  ( -3.810004860640155311, 4.403759411290286252, 1.199719254218462483 ) ) ;
#71467 = DIRECTION ( 'NONE',  ( -1.224646799147353207E-16, 1.000000000000000000, 0.000000000000000000 ) ) ;
#71468 = CARTESIAN_POINT ( 'NONE',  ( 5.371561628297467195, -0.3073141173523045167, 2.047320497149993646 ) ) ;
#71469 = CARTESIAN_POINT ( 'NONE',  ( 1.024625454658374624, 0.3981145430279106057, 1.976669095394629982 ) ) ;
#71470 = B_SPLINE_CURVE_WITH_KNOTS ( 'NONE', 3,
 ( #197194, #150601, #15235, #46713, #112826, #178842, #31520, #96539 ),
 .UNSPECIFIED., .F., .F.,
 ( 4, 2, 2, 4 ),
 ( 0.000000000000000000, 0.001562990337899492670, 0.003125980675798985340, 0.006251961351597973282 ),
 .UNSPECIFIED. ) ;
#71471 = CARTESIAN_POINT ( 'NONE',  ( 1.499999999999985123, -0.6729166659838520248, -0.8660254037844323793 ) ) ;
#71472 = CARTESIAN_POINT ( 'NONE',  ( 4.705647360784301014, -0.5120751438620478879, 1.857136557572524715 ) ) ;
#71473 = EDGE_CURVE ( 'NONE', #145305, #897, #114544, .T. ) ;
#71474 = CARTESIAN_POINT ( 'NONE',  ( -1.402160292154681736E-14, 10.42187500034139447, 1.575800808251682339 ) ) ;
#71475 = CARTESIAN_POINT ( 'NONE',  ( 1.037687956146810198, -0.04753379745526563338, 2.221059295257783006 ) ) ;
#71477 = VERTEX_POINT ( 'NONE', #134200 ) ;
#71476 = CARTESIAN_POINT ( 'NONE',  ( -0.7807912181424305764, 13.24045051524828942, -1.280767376876722041 ) ) ;
#71479 = CARTESIAN_POINT ( 'NONE',  ( -7.767011945534285644, -7.169578370797520250, 7.110792111438891894 ) ) ;
#71478 = SURFACE_SIDE_STYLE ('',( #119249 ) ) ;
#71480 = CARTESIAN_POINT ( 'NONE',  ( 6.549078289569722600, -6.948428148671506932, 6.549078289569701283 ) ) ;
#71481 = CARTESIAN_POINT ( 'NONE',  ( 2.758194185376297902, 5.305311418659259814, 1.199719254218452047 ) ) ;
#71482 = CARTESIAN_POINT ( 'NONE',  ( -11.01135777277262129, 10.19999999999998153, 1.399999999999998579 ) ) ;
#71483 = CARTESIAN_POINT ( 'NONE',  ( 4.634162599488286460, 0.3036646131651790093, 1.713576892981442557 ) ) ;
#71484 = CARTESIAN_POINT ( 'NONE',  ( 2.031626174157370457, 1.878314540015123102, -0.5664888411779643862 ) ) ;
#71486 = CARTESIAN_POINT ( 'NONE',  ( 1.364683531249986537, 2.217708333674751398, -0.7879004041258239610 ) ) ;
#71485 = CARTESIAN_POINT ( 'NONE',  ( 3.798255590122797898, 7.583048621785260401, -0.7998128361456221525 ) ) ;
#71487 = CARTESIAN_POINT ( 'NONE',  ( -5.386593377506219582, 6.333579893170925068, 1.078181536478119762 ) ) ;
#71488 = CARTESIAN_POINT ( 'NONE',  ( 8.516493047678546091, 13.08765898893368629, -0.7998128361456352531 ) ) ;
#71489 = AXIS2_PLACEMENT_3D ( 'NONE', #73368, #105932, #124361 ) ;
#71490 = CARTESIAN_POINT ( 'NONE',  ( 6.180128940399614912, -1.088687182605744042, -1.631870318916525120 ) ) ;
#71491 = CARTESIAN_POINT ( 'NONE',  ( -8.670602931139386627, 10.07445716020612103, 1.199719254218462483 ) ) ;
#71492 = CARTESIAN_POINT ( 'NONE',  ( -4.894130264408873110, 5.772535398974209642, -1.082531754730543971 ) ) ;
#71493 = CARTESIAN_POINT ( 'NONE',  ( 4.891814693739657827, -2.006371927678828104, 0.2024599332275459629 ) ) ;
#71494 = AXIS2_PLACEMENT_3D ( 'NONE', #5925, #200924, #21103 ) ;
#71495 = CARTESIAN_POINT ( 'NONE',  ( 0.7435140528431654072, -1.938958340150579662, 1.165708873083745045 ) ) ;
#71497 = VERTEX_POINT ( 'NONE', #200210 ) ;
#71496 = CARTESIAN_POINT ( 'NONE',  ( -4.934277840369690971, 7.844075682818238526, -1.199719254218452047 ) ) ;
#71498 = CARTESIAN_POINT ( 'NONE',  ( 1.499999999999987121, -0.9645833326505173222, 0.8660254037844524744 ) ) ;
#71499 = CARTESIAN_POINT ( 'NONE',  ( 1.264687732342294701, -1.688641954842164283, -0.8049673154429252131 ) ) ;
#71500 = CARTESIAN_POINT ( 'NONE',  ( 0.7383815455153321938, 1.732312080274291732, -0.08293238807991276662 ) ) ;
#71502 = CARTESIAN_POINT ( 'NONE',  ( 3.737968522918270864, 2.181131050170285857, 0.2133239450496857148 ) ) ;
#71501 = CARTESIAN_POINT ( 'NONE',  ( -1.360316468750026875, 2.140625000341400685, -4.857225732735059864E-14 ) ) ;
#71503 = CARTESIAN_POINT ( 'NONE',  ( 5.385860071389879877, 1.544758419828775153, 1.714431625121175751 ) ) ;
#71504 = CARTESIAN_POINT ( 'NONE',  ( 0.6025036485793239249, -0.6938342907959176298, -1.940726168717278322 ) ) ;
#71505 = CARTESIAN_POINT ( 'NONE',  ( 2.958853767740171392, 0.2844919188511252917, -1.920881014358867489 ) ) ;
#71506 = CARTESIAN_POINT ( 'NONE',  ( -4.053524740361572398, 7.672936597156388316, 0.7216878364870317197 ) ) ;
#71507 = CARTESIAN_POINT ( 'NONE',  ( -1.408489644583400535, 7.311701683604569624, -4.382268911472688266 ) ) ;
#71508 = CARTESIAN_POINT ( 'NONE',  ( 3.580761967785000888, 7.191656372475549119, -0.7216878364870338292 ) ) ;
#71509 = CARTESIAN_POINT ( 'NONE',  ( 2.971327447312217984, -1.987046587055636637, -0.3419355124290662240 ) ) ;
#71510 = CARTESIAN_POINT ( 'NONE',  ( -4.894130264408878439, 4.812166184672871161, -0.7216878364870197293 ) ) ;
#71511 = CARTESIAN_POINT ( 'NONE',  ( -5.108390017298964914, 9.181815130149269422, 0.000000000000000000 ) ) ;
#71512 = CARTESIAN_POINT ( 'NONE',  ( 9.121938423896107651, 9.536683004167278099, -0.7998128361456221525 ) ) ;
#71514 = CARTESIAN_POINT ( 'NONE',  ( 7.770158002575686673, -5.767087321558989288, -7.786489011998996901 ) ) ;
#71513 = CARTESIAN_POINT ( 'NONE',  ( 1.295219883412350503, 1.381147610352757127, 1.194082977437810333 ) ) ;
#71515 = CARTESIAN_POINT ( 'NONE',  ( -5.971440312176176768, 5.931378217152456500, 0.000000000000000000 ) ) ;
#71516 = CARTESIAN_POINT ( 'NONE',  ( -5.514013019825418915, 5.994650414344389056, -0.9619886414689112764 ) ) ;
#71517 = CARTESIAN_POINT ( 'NONE',  ( -9.979842676043658045, 5.589819607760296627, 5.978770845575332338 ) ) ;
#71518 = ORIENTED_EDGE ( 'NONE', *, *, #106930, .T. ) ;
#71519 = CARTESIAN_POINT ( 'NONE',  ( 6.350472301779563900, 0.6441285046014081361, 1.957720813820832850 ) ) ;
#71520 = CARTESIAN_POINT ( 'NONE',  ( -7.241463443030476732, 7.620997903056574430, 0.000000000000000000 ) ) ;
#71521 = CARTESIAN_POINT ( 'NONE',  ( 7.824464048418096951, 8.301165276008827476, -0.7216878364870317197 ) ) ;
#71522 = CARTESIAN_POINT ( 'NONE',  ( -2.428882075142555497, 5.985446187641602300, 1.040834085586084257E-14 ) ) ;
#71523 = CARTESIAN_POINT ( 'NONE',  ( -10.29471871147821282, 10.90492667301307605, -0.7998128361456291469 ) ) ;
#71524 = CARTESIAN_POINT ( 'NONE',  ( 5.356120063770971385, 0.8164924478912498618, -1.847455861782754782 ) ) ;
#71526 = ORIENTED_EDGE ( 'NONE', *, *, #155462, .T. ) ;
#71525 = CARTESIAN_POINT ( 'NONE',  ( 5.479204513921561492, -2.007303783262293972, -0.9515056986081956714 ) ) ;
#71527 = CARTESIAN_POINT ( 'NONE',  ( -6.749980374757255319, 8.968339418673846097, 1.599625672291269396 ) ) ;
#71528 = CARTESIAN_POINT ( 'NONE',  ( 5.900823170445728572, 7.907379670318584353, 1.599625672291267398 ) ) ;
#71529 = CARTESIAN_POINT ( 'NONE',  ( 5.120021580010623907, -1.100570584753908454, -1.742215132906791641 ) ) ;
#71530 = CARTESIAN_POINT ( 'NONE',  ( 3.902970337090125419, -1.038992709432768891, -1.728002613881730376 ) ) ;
#71531 = ORIENTED_EDGE ( 'NONE', *, *, #149705, .F. ) ;
#71532 = CARTESIAN_POINT ( 'NONE',  ( 1.913201741516656895, 3.249623237789923902, -0.4478572873796519138 ) ) ;
#71533 = CARTESIAN_POINT ( 'NONE',  ( -1.869747205843177662, 2.481503150524173140, 2.472679675789646314 ) ) ;
#71534 = TOROIDAL_SURFACE ( 'NONE', #199556, 10.89999999999920988, 0.2000000000000000111 ) ;
#71536 = VERTEX_POINT ( 'NONE', #117984 ) ;
#71535 = CARTESIAN_POINT ( 'NONE',  ( -7.632314129850253259, 7.869064337772231355, 0.7998128361456341429 ) ) ;
#71537 = CARTESIAN_POINT ( 'NONE',  ( 4.628438946891473726, 8.448539137754004003, 0.3726521946380862427 ) ) ;
#71538 = CARTESIAN_POINT ( 'NONE',  ( 4.376327261493318410, -0.3474131038204917310, 1.985796694155849362 ) ) ;
#71539 = CARTESIAN_POINT ( 'NONE',  ( 3.081803158279991628, -1.813988701161291628, -0.3140598505507880556 ) ) ;
#71540 = LINE ( 'NONE', #103003, #60292 ) ;
#71541 = CARTESIAN_POINT ( 'NONE',  ( 2.526355290359350025, -1.329941221805782892, -1.885751665715528880 ) ) ;
#71542 = CARTESIAN_POINT ( 'NONE',  ( 4.329849954717849947, 6.144853928627882489, 1.599625672291262513 ) ) ;
#71543 = CARTESIAN_POINT ( 'NONE',  ( 3.198656860129048152, -0.6241516536032962748, -2.069545307505623821 ) ) ;
#71544 = CARTESIAN_POINT ( 'NONE',  ( 7.262363838414439776, 11.62450824479221900, 0.7998128361456462443 ) ) ;
#71545 = CARTESIAN_POINT ( 'NONE',  ( -6.274726165026268454, 6.214935368819085149, 0.7998128361456341429 ) ) ;
#71547 = ADVANCED_FACE ( 'NONE', ( #35587, #19335 ), #87558, .T. ) ;
#71546 = AXIS2_PLACEMENT_3D ( 'NONE', #195968, #82195, #200200 ) ;
#71548 = PRODUCT_RELATED_PRODUCT_CATEGORY ( 'part', '', ( #59182 ) ) ;
#71549 = CARTESIAN_POINT ( 'NONE',  ( -9.585855168744716437, 14.76561575556795347, -7.219146574477996126 ) ) ;
#71550 = CARTESIAN_POINT ( 'NONE',  ( 1.144815873399098738, 2.850330900256261568, 0.7749999999993786304 ) ) ;
#71551 = CARTESIAN_POINT ( 'NONE',  ( 2.377632874612686020, 1.149002834218125102, 1.476114537088555112 ) ) ;
#71552 = CARTESIAN_POINT ( 'NONE',  ( 0.6144489392437714192, 1.362578290646492718, -1.424861684082868063 ) ) ;
#71554 = CARTESIAN_POINT ( 'NONE',  ( -5.752402313948099533, 9.933162809573264695, -0.7998128361456362523 ) ) ;
#71553 = CARTESIAN_POINT ( 'NONE',  ( -1.364683531249997417, 5.009375000341425022, 1.214306433183764966E-14 ) ) ;
#71555 = CARTESIAN_POINT ( 'NONE',  ( 1.823171247573553311, 2.059948494222668014, 0.7922594597074559264 ) ) ;
#71556 = ORIENTED_EDGE ( 'NONE', *, *, #135726, .F. ) ;
#71557 = CARTESIAN_POINT ( 'NONE',  ( -1.485618637124742625, 7.335443175656797266, -4.255655007286210711 ) ) ;
#71558 = CARTESIAN_POINT ( 'NONE',  ( 3.408985558832261731, 6.064568021024562938, 1.199719254218462483 ) ) ;
#71559 = CARTESIAN_POINT ( 'NONE',  ( -4.761938266897808525, 6.578680616179308771, 1.599625672291267398 ) ) ;
#71560 = MECHANICAL_DESIGN_GEOMETRIC_PRESENTATION_REPRESENTATION (  '', ( #175337 ), #92341 ) ;
#71561 = DIRECTION ( 'NONE',  ( 0.000000000000000000, 1.000000000000000000, 0.000000000000000000 ) ) ;
#71562 = CARTESIAN_POINT ( 'NONE',  ( 6.034049845351773023, 0.9722699467793812778, -1.714982496439126924 ) ) ;
#71563 = CARTESIAN_POINT ( 'NONE',  ( 6.006511608602003172, -0.8246739634825739351, -2.155485180906725251 ) ) ;
#71564 = CARTESIAN_POINT ( 'NONE',  ( 0.7308173252688826560, -1.846041318942293286, -0.6644482084196751126 ) ) ;
#71565 = CARTESIAN_POINT ( 'NONE',  ( 3.625881544801349055, 2.013384979781565942, -0.4471371585693607598 ) ) ;
#71566 = CARTESIAN_POINT ( 'NONE',  ( 6.317736394288147039, 6.473040002865377396, 0.7216878364870317197 ) ) ;
#71567 = CARTESIAN_POINT ( 'NONE',  ( 4.004454267989866700, 5.765225627445230927, 1.599625672291262513 ) ) ;
#71568 = CARTESIAN_POINT ( 'NONE',  ( 8.880227426826646564, 9.462612874160329923, 0.7216878364870458196 ) ) ;
#71569 = CARTESIAN_POINT ( 'NONE',  ( -1.364683531250010295, 3.842708333674751398, 0.7879004041258379498 ) ) ;
#71570 = CARTESIAN_POINT ( 'NONE',  ( -9.902774762303035772, 3.558546654280230204, -6.781965751223174799 ) ) ;
#71571 = CARTESIAN_POINT ( 'NONE',  ( 4.161989969270892153, 6.839110149915929249, 1.082531754730558626 ) ) ;
#71572 = CARTESIAN_POINT ( 'NONE',  ( 5.986835238096758438, 2.090873126042319896, 0.5847848357620232251 ) ) ;
#71574 = CARTESIAN_POINT ( 'NONE',  ( 4.774869596704574448, 1.716175909155163382, -0.6674964387535023969 ) ) ;
#71573 = DIRECTION ( 'NONE',  ( 0.000000000000000000, -1.000000000000000000, 0.000000000000000000 ) ) ;
#71575 = DIRECTION ( 'NONE',  ( 2.168404344971003188E-14, 1.000000000000000000, 0.000000000000000000 ) ) ;
#71576 = CARTESIAN_POINT ( 'NONE',  ( 6.110890996357365879, -0.2699588104537915534, 2.174781792473476472 ) ) ;
#71577 = CARTESIAN_POINT ( 'NONE',  ( -11.92619526913700057, 10.07218333338755301, 1.328859060402684644 ) ) ;
#71578 = CARTESIAN_POINT ( 'NONE',  ( -4.181557753866925964, 7.584876391898649928, 0.9328056193420256603 ) ) ;
#71579 = CARTESIAN_POINT ( 'NONE',  ( -10.91970695577495931, -6.134628647623513231, 0.000000000000000000 ) ) ;
#71580 = CARTESIAN_POINT ( 'NONE',  ( 6.440439394220377700, 6.875545743132385645, 0.7017714770480776298 ) ) ;
#71581 = CARTESIAN_POINT ( 'NONE',  ( 11.41176686791169104, 13.75950803486853680, -3.404018756831829418 ) ) ;
#71582 = CARTESIAN_POINT ( 'NONE',  ( 1.920411955722916453, 1.650032497218676397, 0.6405850872945593188 ) ) ;
#71583 = CARTESIAN_POINT ( 'NONE',  ( 6.428391161641624940, -0.9511404050406097044, -1.774240594045069841 ) ) ;
#71585 = CARTESIAN_POINT ( 'NONE',  ( 3.919475720687201736, -1.323675617205988475, -1.384941642318695987 ) ) ;
#71584 = CARTESIAN_POINT ( 'NONE',  ( -10.64045162862669081, 11.30828174301964140, -0.7998128361456221525 ) ) ;
#71586 = CARTESIAN_POINT ( 'NONE',  ( -2.974862185324181674, 6.692333939762660222, -0.03304652273056766371 ) ) ;
#71587 = CARTESIAN_POINT ( 'NONE',  ( 5.406690398188211510, 0.5700869393594419909, 1.885254869494409791 ) ) ;
#71588 = CARTESIAN_POINT ( 'NONE',  ( 0.3695850531008069706, -1.794773754367712693, -1.129184308951653781 ) ) ;
#71589 = CARTESIAN_POINT ( 'NONE',  ( -1.527869225950100107, -1.291745156262765759, 1.495028600074747027 ) ) ;
#71590 = CARTESIAN_POINT ( 'NONE',  ( 2.764352523130030548, -1.291370965961564421, 1.353630663414123969 ) ) ;
#71592 = ORIENTED_EDGE ( 'NONE', *, *, #157187, .F. ) ;
#71591 = CARTESIAN_POINT ( 'NONE',  ( 6.621745524129793559, -1.670984818007285266, 0.4274731708342211500 ) ) ;
#71594 = CARTESIAN_POINT ( 'NONE',  ( 4.053524740805938720, 3.831459740469437936, 1.214306433183764966E-14 ) ) ;
#71593 = CARTESIAN_POINT ( 'NONE',  ( 3.141465813989018141, -1.946189201368169641, 1.040519825639886431 ) ) ;
#71595 = CARTESIAN_POINT ( 'NONE',  ( 1.364683531249990311, 2.946875000341416140, 1.214306433183764966E-14 ) ) ;
#71596 = CARTESIAN_POINT ( 'NONE',  ( 1.064971659385913316, 1.563282549206745475, -1.345778378556292676 ) ) ;
#71597 = CARTESIAN_POINT ( 'NONE',  ( 5.926885707468349196, 10.06645042535509660, 1.040834085586084257E-14 ) ) ;
#71598 = CARTESIAN_POINT ( 'NONE',  ( -6.766604819867126253, -7.256397064628592020, 6.766604819867148457 ) ) ;
#71599 = CARTESIAN_POINT ( 'NONE',  ( 0.000000000000000000, 0.000000000000000000, 0.000000000000000000 ) ) ;
#71600 = CARTESIAN_POINT ( 'NONE',  ( -4.497554271431319250, 6.270232621468402989, -1.599625672291256517 ) ) ;
#71601 = CARTESIAN_POINT ( 'NONE',  ( -7.668547801473484249, -6.765616048178583419, -7.886602582589878452 ) ) ;
#71602 = ORIENTED_EDGE ( 'NONE', *, *, #169931, .F. ) ;
#71603 = CARTESIAN_POINT ( 'NONE',  ( 3.367693471486675083, -0.4065805204805824635, 2.029877954327436118 ) ) ;
#71604 = CARTESIAN_POINT ( 'NONE',  ( 0.7499999999999920064, 4.983333333333353821, 1.299038105676669330 ) ) ;
#71605 = CARTESIAN_POINT ( 'NONE',  ( 3.798255590122797898, 7.583048621785260401, -0.7998128361456221525 ) ) ;
#71606 = CARTESIAN_POINT ( 'NONE',  ( -5.939261241470221719, 7.227352081167748743, 1.243796156610659454 ) ) ;
#71607 = CARTESIAN_POINT ( 'NONE',  ( 0.5572930201490761126, -1.731111387009228952, 1.040124062761533352 ) ) ;
#71608 = CARTESIAN_POINT ( 'NONE',  ( -1.364683531249997417, 3.259375000341423245, 1.214306433183764966E-14 ) ) ;
#71609 = VERTEX_POINT ( 'NONE', #56123 ) ;
#71611 = CARTESIAN_POINT ( 'NONE',  ( 9.246297574839974942, 11.81043314211192019, 1.443375672974076540 ) ) ;
#71610 = CARTESIAN_POINT ( 'NONE',  ( 0.1745949693968693039, 7.629137130509094256, -2.355306170041113756 ) ) ;
#71612 = CARTESIAN_POINT ( 'NONE',  ( 6.028672669474048007, 1.986741788447304646, -0.3418859329693338944 ) ) ;
#71613 = CARTESIAN_POINT ( 'NONE',  ( 5.717977451880697615, 0.9379096786080630688, -1.670315906950563534 ) ) ;
#71614 = SPHERICAL_SURFACE ( 'NONE', #186581, 0.08000000000000000167 ) ;
#71615 = CARTESIAN_POINT ( 'NONE',  ( 3.562233144267571650, -1.470601008620987749, 1.625073949779440419 ) ) ;
#71617 = STYLED_ITEM ( 'NONE', ( #16875 ), #19216 ) ;
#71616 = CARTESIAN_POINT ( 'NONE',  ( -1.402160292154681736E-14, 2.618750000682819490, -1.732050807568863648 ) ) ;
#71618 = CARTESIAN_POINT ( 'NONE',  ( 2.636851627972558454, 1.802111047976437508, 0.6404684511054498097 ) ) ;
#71619 = CARTESIAN_POINT ( 'NONE',  ( -5.018489415352746619, 9.006654751220198207, 0.7998128361456481317 ) ) ;
#71620 = CARTESIAN_POINT ( 'NONE',  ( 4.731432421044862835, 6.543090462684225450, -1.443375672974051449 ) ) ;
#71622 = CARTESIAN_POINT ( 'NONE',  ( 0.8082205221912192039, 1.198841770460257194, -1.621197638953228548 ) ) ;
#71621 = SURFACE_STYLE_USAGE ( .BOTH. , #152896 ) ;
#71623 = CARTESIAN_POINT ( 'NONE',  ( 0.6823417656249934904, 11.25520833367473017, 1.181850606188764807 ) ) ;
#71625 = CARTESIAN_POINT ( 'NONE',  ( -5.108390017298964914, 9.181815130149269422, 0.000000000000000000 ) ) ;
#71624 = CARTESIAN_POINT ( 'NONE',  ( 6.023007056224171762, -2.064090639567913499, 0.7368321019862942300 ) ) ;
#71627 = ORIENTED_EDGE ( 'NONE', *, *, #134258, .T. ) ;
#71626 = CARTESIAN_POINT ( 'NONE',  ( 3.574969364760666846, 0.04275877055364904478, -1.724416222950067690 ) ) ;
#71628 = CARTESIAN_POINT ( 'NONE',  ( 0.1399997263886037790, 2.025166351305721868, -2.415484119839182320 ) ) ;
#71629 = CARTESIAN_POINT ( 'NONE',  ( 8.620286740190458374, 8.951422706510690830, 1.040834085586084257E-14 ) ) ;
#71630 = CARTESIAN_POINT ( 'NONE',  ( 4.741601036477289810, 6.554953847355395880, 1.599625672291267398 ) ) ;
#71631 = DIRECTION ( 'NONE',  ( 2.949029909160572061E-17, 1.000000000000000000, -8.673600428462616880E-15 ) ) ;
#71632 = CARTESIAN_POINT ( 'NONE',  ( 0.4495626703563436743, 1.451167377975391304, 1.320406988977901985 ) ) ;
#71633 = CARTESIAN_POINT ( 'NONE',  ( -4.229020061460118107, 7.343517960532633282, -0.8650006913940473385 ) ) ;
#71634 = CARTESIAN_POINT ( 'NONE',  ( 4.813308228051395687, 5.574280006603454574, 1.199719254218462483 ) ) ;
#71635 = CARTESIAN_POINT ( 'NONE',  ( -10.91944002402978775, -9.999999999999994671, 0.1105873483556694958 ) ) ;
#71636 = VERTEX_POINT ( 'NONE', #73424 ) ;
#71637 = CARTESIAN_POINT ( 'NONE',  ( -10.43059700200766216, 5.377693802073528317, 5.769666037277090709 ) ) ;
#71638 = VERTEX_POINT ( 'NONE', #187176 ) ;
#71639 = CARTESIAN_POINT ( 'NONE',  ( 3.668453237830204827, 0.6552377326864079476, 1.688991677562341920 ) ) ;
#71640 = ORIENTED_EDGE ( 'NONE', *, *, #16540, .T. ) ;
#71641 = CARTESIAN_POINT ( 'NONE',  ( 9.378489572351044856, 11.96465713920816043, -1.599625672291262513 ) ) ;
#71642 = CARTESIAN_POINT ( 'NONE',  ( 3.736153849017632922, 6.516540702899320081, -1.199719254218453823 ) ) ;
#71643 = CARTESIAN_POINT ( 'NONE',  ( 4.477109312160544974, -1.620259271022955305, -0.8101795318041657978 ) ) ;
#71644 = CARTESIAN_POINT ( 'NONE',  ( 5.994113310573177422, 10.00723293906178846, 0.000000000000000000 ) ) ;
#71645 = CARTESIAN_POINT ( 'NONE',  ( 5.320181785876097358, 6.346852008952179602, 1.110229221197155169 ) ) ;
#71647 = CARTESIAN_POINT ( 'NONE',  ( 1.364683531250000303, 14.00520833367473195, -0.7879004041258355073 ) ) ;
#71646 = CARTESIAN_POINT ( 'NONE',  ( 5.441811508714582857, 1.250024229543914567, 1.378945535785504051 ) ) ;
#71648 = CARTESIAN_POINT ( 'NONE',  ( 3.233901216830310954, 1.915793140838128572, -0.003097617167701141160 ) ) ;
#71649 = CARTESIAN_POINT ( 'NONE',  ( 6.777182134110200096, 7.629137130509070275, 2.410944104600750038 ) ) ;
#71650 = CARTESIAN_POINT ( 'NONE',  ( -11.50375155617990686, 6.427325993555151662, 3.051984382272954210 ) ) ;
#71651 = CIRCLE ( 'NONE', #26670, 12.00000000000000178 ) ;
#71652 = CARTESIAN_POINT ( 'NONE',  ( -1.201851678989727383E-14, 3.212500000000018119, 1.732050807568877637 ) ) ;
#71653 = DIRECTION ( 'NONE',  ( -0.000000000000000000, -1.000000000000000000, -0.000000000000000000 ) ) ;
#71654 = CARTESIAN_POINT ( 'NONE',  ( 6.304178240674458422, 10.29869901418813782, 1.040834085586084257E-14 ) ) ;
#71655 = CARTESIAN_POINT ( 'NONE',  ( -4.627410500965859264, 4.293067094081919777, 0.7998128361456341429 ) ) ;
#71656 = CARTESIAN_POINT ( 'NONE',  ( 6.663994888585877518, -7.154544010627095219, -6.770610912236881163 ) ) ;
#71657 = CARTESIAN_POINT ( 'NONE',  ( 1.007895156502825573, -0.9414231642565270564, -1.866751856443664037 ) ) ;
#71658 = CARTESIAN_POINT ( 'NONE',  ( 5.017399365509065845, 8.011327138806002779, -1.199719254218450271 ) ) ;
#71659 = CARTESIAN_POINT ( 'NONE',  ( 6.053727987682750999, 0.5585614288021992779, -1.843621721047507878 ) ) ;
#71660 = CARTESIAN_POINT ( 'NONE',  ( -3.581325132304157943, 7.329963087663487364, -0.7998128361456281477 ) ) ;
#71661 = CARTESIAN_POINT ( 'NONE',  ( 2.907047201455061014, 1.541221212934189344, 0.9781624729086123571 ) ) ;
#71662 = CARTESIAN_POINT ( 'NONE',  ( 9.728550251279687089, 13.21449840343153426, 8.106492410889076794 ) ) ;
#71663 = CARTESIAN_POINT ( 'NONE',  ( 2.408343312057196872, -1.907530749141531423, -0.1368029246449145864 ) ) ;
#71664 = CARTESIAN_POINT ( 'NONE',  ( 1.750388463564346075, -1.959780499145358679, -0.1960735186044142708 ) ) ;
#71665 = CARTESIAN_POINT ( 'NONE',  ( 3.403789896209925114, -0.7897705758606025084, -1.774406015287466332 ) ) ;
#71666 = ORIENTED_EDGE ( 'NONE', *, *, #76499, .T. ) ;
#71667 = CARTESIAN_POINT ( 'NONE',  ( -0.7500000000000215383, 3.222916667349487341, 1.299038105676671107 ) ) ;
#71668 = CARTESIAN_POINT ( 'NONE',  ( -4.817943484809863008, 6.714296380401858499, 1.599625672291263179 ) ) ;
#71670 = CARTESIAN_POINT ( 'NONE',  ( 3.726904977748810133, 1.497142547446396410, -1.502090761940577002 ) ) ;
#71669 = CARTESIAN_POINT ( 'NONE',  ( 4.085803189671889157, 5.860132702740892263, -1.599625672291273171 ) ) ;
#71672 = EDGE_CURVE ( 'NONE', #22347, #12842, #201016, .T. ) ;
#71671 = CARTESIAN_POINT ( 'NONE',  ( 1.836970198721030181E-16, 13.49999999999999822, 1.500000000000000222 ) ) ;
#71673 = CARTESIAN_POINT ( 'NONE',  ( 8.422639742587595180, 10.84949900448412130, -1.599625672291268286 ) ) ;
#71674 = CARTESIAN_POINT ( 'NONE',  ( -4.936050443827081580, 7.916420063510339666, 1.199719254218452935 ) ) ;
#71675 = CARTESIAN_POINT ( 'NONE',  ( 2.236732156574683827, 5.553345249405011508, 1.040834085586084257E-14 ) ) ;
#71676 = EDGE_LOOP ( 'NONE', ( #49855, #61456, #136671, #159206 ) ) ;
#71677 = CARTESIAN_POINT ( 'NONE',  ( 7.198453214212898743, 7.362893269528701268, 0.7998128361456291469 ) ) ;
#71678 = DIRECTION ( 'NONE',  ( 1.000000000000000000, -0.000000000000000000, -0.000000000000000000 ) ) ;
#71679 = CARTESIAN_POINT ( 'NONE',  ( 3.404746562951189937, 1.438594061741470753, -1.123979961188771304 ) ) ;
#71680 = CARTESIAN_POINT ( 'NONE',  ( 0.1333692844072559280, 0.001398348041498076455, -2.053671342968105051 ) ) ;
#71681 = CARTESIAN_POINT ( 'NONE',  ( -8.337901282724359930, 12.67137589657970409, 1.040834085586084257E-14 ) ) ;
#71682 = STYLED_ITEM ( 'NONE', ( #121220 ), #101631 ) ;
#71683 = CARTESIAN_POINT ( 'NONE',  ( -5.586845290032572464, 7.502486493224762576, 1.347716017753825879 ) ) ;
#71684 = FACE_OUTER_BOUND ( 'NONE', #113054, .T. ) ;
#71685 = CARTESIAN_POINT ( 'NONE',  ( 4.627732503263369601, -1.150995203733524930, -1.474563928533303869 ) ) ;
#71686 = CARTESIAN_POINT ( 'NONE',  ( 8.589254009457354400, 9.979550084910457031, -1.199719254218446718 ) ) ;
#71687 = CARTESIAN_POINT ( 'NONE',  ( 2.402848698864976207, 1.547341197487204001, -1.147474368762817498 ) ) ;
#71688 = CARTESIAN_POINT ( 'NONE',  ( 6.403176761927252159, -1.659045864033869666, 1.046607237317781269 ) ) ;
#71689 = AXIS2_PLACEMENT_3D ( 'NONE', #39876, #104882, #154688 ) ;
#71690 = CARTESIAN_POINT ( 'NONE',  ( 0.6823417656249969321, 8.588541667008065872, -1.181850606188757036 ) ) ;
#71691 = CARTESIAN_POINT ( 'NONE',  ( -5.388475986427523345, 8.373973519885682393, 1.199719254218452047 ) ) ;
#71692 = CARTESIAN_POINT ( 'NONE',  ( 4.253507506385319381, 5.985511395581417204, 1.599625672291267398 ) ) ;
#71693 = CARTESIAN_POINT ( 'NONE',  ( -6.251718229232867685, 6.466295153626015590, -0.7216878364870338292 ) ) ;
#71694 = EDGE_CURVE ( 'NONE', #206450, #23400, #121207, .T. ) ;
#71695 = CARTESIAN_POINT ( 'NONE',  ( 0.7204975843347528608, 2.086673352822054461, 0.3575386888887230885 ) ) ;
#71696 = CARTESIAN_POINT ( 'NONE',  ( 9.890836756369282057, 11.49806328964105617, -1.199719254218440723 ) ) ;
#71698 = ORIENTED_EDGE ( 'NONE', *, *, #57396, .F. ) ;
#71697 = CARTESIAN_POINT ( 'NONE',  ( -3.145128448690323264, 4.692402494937224056, -1.443375672974059665 ) ) ;
#71699 = CARTESIAN_POINT ( 'NONE',  ( 5.682505902380680318, 1.237739610710282046, -1.659335868388504220 ) ) ;
#71701 = CARTESIAN_POINT ( 'NONE',  ( 0.6823417656249899377, 2.155208333674753174, 1.181850606188767472 ) ) ;
#71700 = CARTESIAN_POINT ( 'NONE',  ( 0.1867156058280826092, 1.363667594142993877, 1.237386390646778578 ) ) ;
#71702 = CARTESIAN_POINT ( 'NONE',  ( 5.432396523169654934, -1.810675156642663541, -1.416092387804610553 ) ) ;
#71703 = CARTESIAN_POINT ( 'NONE',  ( 6.155038550924144758, 8.203964280876741455, 1.443375672974076540 ) ) ;
#71704 = CARTESIAN_POINT ( 'NONE',  ( -0.7499999999999972244, 4.639583334016150751, -1.299038105676652899 ) ) ;
#71705 = CARTESIAN_POINT ( 'NONE',  ( 0.9203736287852108955, 1.361359823012283865, -1.844092865855660124 ) ) ;
#71706 = CARTESIAN_POINT ( 'NONE',  ( 5.040435666063417308, 4.901720900707255524, -0.1634480055122013165 ) ) ;
#71707 = CARTESIAN_POINT ( 'NONE',  ( -4.274563570058511175, 8.209017608368725405, 0.000000000000000000 ) ) ;
#71708 = CARTESIAN_POINT ( 'NONE',  ( 5.349535142863500070, 1.939630122921351729, -0.09734604192479337503 ) ) ;
#71709 = ORIENTED_EDGE ( 'NONE', *, *, #175445, .T. ) ;
#71710 = CARTESIAN_POINT ( 'NONE',  ( 7.090551149822722721, 11.21613407486112379, 0.7216878364870438212 ) ) ;
#71711 = VERTEX_POINT ( 'NONE', #122281 ) ;
#71712 = CARTESIAN_POINT ( 'NONE',  ( 6.170165192347925931, 1.906784905861274693, -0.1475879885542986936 ) ) ;
#71713 = CARTESIAN_POINT ( 'NONE',  ( 5.173064673083394460, 1.776168143800487043, -0.9548534231369476544 ) ) ;
#71715 = DIRECTION ( 'NONE',  ( 0.000000000000000000, -1.000000000000000000, 0.000000000000000000 ) ) ;
#71714 = CARTESIAN_POINT ( 'NONE',  ( -7.828943636887387925, 11.22118577875556156, 1.199719254218453823 ) ) ;
#71716 = CARTESIAN_POINT ( 'NONE',  ( -1.642778471875000035, -1.655208332855377051, -2.845375778867859751 ) ) ;
#71718 = CARTESIAN_POINT ( 'NONE',  ( 1.744620744215353625, -1.497317806218407599, 0.9432750629611782456 ) ) ;
#71717 = CARTESIAN_POINT ( 'NONE',  ( 2.220754083240178645, 0.001034992482759621978, 2.090823719040376893 ) ) ;
#71719 = CARTESIAN_POINT ( 'NONE',  ( 0.3999999999999819811, 3.049942316455271474, -0.4288785890452975202 ) ) ;
#71721 = CARTESIAN_POINT ( 'NONE',  ( 3.662334778960428139, -1.540015086033737601, 1.698051401694438800 ) ) ;
#71720 =( LENGTH_UNIT ( ) NAMED_UNIT ( * ) SI_UNIT ( .MILLI., .METRE. ) );
#71722 = B_SPLINE_CURVE_WITH_KNOTS ( 'NONE', 3,
 ( #174172, #140617, #96116, #125479, #25744, #161097, #78762, #76633, #124416, #190375, #209820 ),
 .UNSPECIFIED., .F., .F.,
 ( 4, 1, 1, 1, 1, 1, 1, 1, 4 ),
 ( 0.000000000000000000, 0.2255619619413396781, 0.3975297875667437308, 0.5250373104567740423, 0.6172314665434700531, 0.6832587661106447330, 0.7322037845459880012, 0.7729093456892226488, 1.000000000000000000 ),
 .UNSPECIFIED. ) ;
#71723 = CARTESIAN_POINT ( 'NONE',  ( 2.431276410161122392, 0.8208083392724160321, -1.534589408508793440 ) ) ;
#71724 = CARTESIAN_POINT ( 'NONE',  ( 2.855963913973019963, 6.483708332943829866, 0.000000000000000000 ) ) ;
#71725 = DIRECTION ( 'NONE',  ( 0.5000000000000001110, 0.000000000000000000, -0.8660254037844385966 ) ) ;
#71726 = CARTESIAN_POINT ( 'NONE',  ( 2.231429653443087080, -1.583367121652721421, -0.7069697159475217818 ) ) ;
#71727 = CARTESIAN_POINT ( 'NONE',  ( 2.945941647375094785, 1.533668492858210497, 1.537084210998492795 ) ) ;
#71728 = CARTESIAN_POINT ( 'NONE',  ( 3.310162060030825248, 7.013606170011280838, -0.7998128361456291469 ) ) ;
#71729 = CARTESIAN_POINT ( 'NONE',  ( 5.085172837459294826, 1.651341431264556014, 1.157102043685846793 ) ) ;
#71730 = CARTESIAN_POINT ( 'NONE',  ( 1.500000000000001110, -8.632537233970167800E-14, -2.052068128417951165 ) ) ;
#71731 = CARTESIAN_POINT ( 'NONE',  ( -1.201851678989727383E-14, 3.493750000682815493, 1.732050807568877637 ) ) ;
#71732 = CARTESIAN_POINT ( 'NONE',  ( 0.6922523098862876090, -1.911435030786556855, -0.2391616053641909545 ) ) ;
#71733 = CARTESIAN_POINT ( 'NONE',  ( 0.6823417656249934904, 15.19270833367473372, 1.181850606188764807 ) ) ;
#71734 = CARTESIAN_POINT ( 'NONE',  ( 4.236746486948286261, 1.365021424349493584, -1.752494286840690085 ) ) ;
#71735 = VERTEX_POINT ( 'NONE', #154692 ) ;
#71736 = CARTESIAN_POINT ( 'NONE',  ( -0.2106854629475062024, 1.349218558350977260, -2.248994321313985800 ) ) ;
#71737 = CARTESIAN_POINT ( 'NONE',  ( -1.500000000000015099, -0.1208333333333093396, -0.8660254037844383745 ) ) ;
#71738 = CARTESIAN_POINT ( 'NONE',  ( 7.130698725783555680, 10.40656671580112658, 1.199719254218460707 ) ) ;
#71739 = CARTESIAN_POINT ( 'NONE',  ( 5.707619481228810798, 7.681975366232176583, -1.443375672974057666 ) ) ;
#71740 = CARTESIAN_POINT ( 'NONE',  ( -3.285556943749998737, -1.480208332855375453, 1.896917185911908721 ) ) ;
#71741 = CARTESIAN_POINT ( 'NONE',  ( 0.6455721646590365514, 0.1693206843514388493, 2.214916916779915201 ) ) ;
#71742 = CARTESIAN_POINT ( 'NONE',  ( 5.582460749670235423, 1.169929261559121247, -1.574690175210855747 ) ) ;
#71743 = CARTESIAN_POINT ( 'NONE',  ( 8.758204044747994743, 12.20135990463928266, 1.082531754730546636 ) ) ;
#71744 =( LENGTH_UNIT ( ) NAMED_UNIT ( * ) SI_UNIT ( .MILLI., .METRE. ) );
#71745 = CARTESIAN_POINT ( 'NONE',  ( 0.2456851981432126020, -1.670693100197045977, -1.371219901248825535 ) ) ;
#71746 = CARTESIAN_POINT ( 'NONE',  ( -4.123088112331656951, 6.864000993478624579, 1.082531754730549967 ) ) ;
#71747 = CARTESIAN_POINT ( 'NONE',  ( 3.314939881033797331, -1.563807569242671613, 1.345168064507019423 ) ) ;
#71748 = CARTESIAN_POINT ( 'NONE',  ( -6.715366157470410435, 6.729015360003925750, -0.7998128361456291469 ) ) ;
#71749 = CARTESIAN_POINT ( 'NONE',  ( -1.499999999999997780, 2.931250000682818158, 1.214306433183764966E-14 ) ) ;
#71750 = CARTESIAN_POINT ( 'NONE',  ( 0.6823417656249882723, -1.157291666325249713, 1.181850606188755259 ) ) ;
#71751 = CARTESIAN_POINT ( 'NONE',  ( 4.973830807571049561, 1.075732564348480746, 1.530087412091485799 ) ) ;
#71752 = CARTESIAN_POINT ( 'NONE',  ( 3.428057853464313798, -1.315526611184931527, -1.130013928329278494 ) ) ;
#71753 = CARTESIAN_POINT ( 'NONE',  ( 3.210250486799534286, 1.574880741971116827, 0.7411356085459307463 ) ) ;
#71754 = CARTESIAN_POINT ( 'NONE',  ( 0.6621918981609349331, 1.136352663792916662, 1.990853321008963395 ) ) ;
#71755 = CARTESIAN_POINT ( 'NONE',  ( -1.364683531249997417, 4.571875000341417028, 1.214306433183764966E-14 ) ) ;
#71756 = CARTESIAN_POINT ( 'NONE',  ( 4.898031494525131535, -0.7058569028579181337, -1.968109489924846356 ) ) ;
#71757 = CARTESIAN_POINT ( 'NONE',  ( 6.597608361038971303, -1.941456323438792042, 0.05037571119943275166 ) ) ;
#71758 = EDGE_LOOP ( 'NONE', ( #125060, #102993, #172363, #8330, #84491 ) ) ;
#71759 = SHAPE_REPRESENTATION_RELATIONSHIP ( 'NONE' , 'NONE' ,  #189584, #166452 ) ;
#71760 = CARTESIAN_POINT ( 'NONE',  ( 0.4049229342097167006, -1.081068455937021611, -1.701946057285643743 ) ) ;
#71761 = CARTESIAN_POINT ( 'NONE',  ( 1.318772358905948794, -0.7683209907942339933, -1.976687055281033611 ) ) ;
#71762 = LINE ( 'NONE', #142158, #24524 ) ;
#71763 = DIRECTION ( 'NONE',  ( 0.000000000000000000, -1.000000000000000000, 0.000000000000000000 ) ) ;
#71764 = CARTESIAN_POINT ( 'NONE',  ( -8.701635661872465732, 9.046329781806354831, 1.040834085586084257E-14 ) ) ;
#71765 = CARTESIAN_POINT ( 'NONE',  ( 6.993308306550549247, 7.053281200597435685, 1.040834085586084257E-14 ) ) ;
#71766 = CARTESIAN_POINT ( 'NONE',  ( 2.104293207771616991, -0.9040658786637757460, 1.918231223523607865 ) ) ;
#71767 = CARTESIAN_POINT ( 'NONE',  ( 0.4288785890452437299, 3.049942316455264812, -0.4196807566835009662 ) ) ;
#71768 = CARTESIAN_POINT ( 'NONE',  ( 4.600122369450095228, -1.825375079466069694, -0.04201004182294298950 ) ) ;
#71769 = ORIENTED_EDGE ( 'NONE', *, *, #57451, .T. ) ;
#71770 = CARTESIAN_POINT ( 'NONE',  ( -6.967964602780620353, 7.093989889524320525, 0.000000000000000000 ) ) ;
#71771 = CARTESIAN_POINT ( 'NONE',  ( -1.364683531250000748, 8.390625000341399797, 0.000000000000000000 ) ) ;
#71772 = CARTESIAN_POINT ( 'NONE',  ( 7.797347741190739256, 8.269529584243604958, 0.7216878364870267237 ) ) ;
#71773 = CARTESIAN_POINT ( 'NONE',  ( 3.285556943750000514, -0.4010416661887095113, 1.896917185911906500 ) ) ;
#71774 = CARTESIAN_POINT ( 'NONE',  ( -6.018930129462987999, 9.109503353427070849, 1.199719254218452047 ) ) ;
#71775 = CARTESIAN_POINT ( 'NONE',  ( 1.863541707127059688, -1.624685865379692506, -1.199789887509305597 ) ) ;
#71776 = CARTESIAN_POINT ( 'NONE',  ( 5.948300505803370442, 2.203960110721484789, 0.1139900122707343255 ) ) ;
#71777 = CARTESIAN_POINT ( 'NONE',  ( -3.474632506852224356, 7.275764701294714420, -0.7998128361456481317 ) ) ;
#71778 = CARTESIAN_POINT ( 'NONE',  ( 4.539814342829402882, 1.213294893355709503, 1.411164879910733472 ) ) ;
#71779 = CARTESIAN_POINT ( 'NONE',  ( 8.269583629331492602, 11.73526576994040482, 1.199719254218450271 ) ) ;
#71780 = CARTESIAN_POINT ( 'NONE',  ( 11.52460864928264783, 9.719999999999982876, 3.346683403123522638 ) ) ;
#71781 = VERTEX_POINT ( 'NONE', #6275 ) ;
#71782 = CARTESIAN_POINT ( 'NONE',  ( -3.391510981712833939, 7.108513245306943062, 0.7998128361456341429 ) ) ;
#71783 = CARTESIAN_POINT ( 'NONE',  ( -8.565000355531095622, 11.01558638625153286, -1.599625672291263179 ) ) ;
#71784 = CARTESIAN_POINT ( 'NONE',  ( 4.529811765687052016, -1.125283923072720071, -1.437579299059896343 ) ) ;
#71786 = CARTESIAN_POINT ( 'NONE',  ( -4.002466101043451019, 7.812316210466456745, 0.3644823170804913914 ) ) ;
#71785 = CARTESIAN_POINT ( 'NONE',  ( -6.050681693448748177, 10.28115541899069463, 0.7998128361456291469 ) ) ;
#71787 = CARTESIAN_POINT ( 'NONE',  ( -1.364683531250014514, -0.7197916663252461600, 0.7879004041258379498 ) ) ;
#71788 = CARTESIAN_POINT ( 'NONE',  ( 0.4383029422423733168, 0.9912079340955775031, 1.422354019259955304 ) ) ;
#71789 = CARTESIAN_POINT ( 'NONE',  ( 0.1283017097272065865, -1.593451896579937355, 0.7002181395190426594 ) ) ;
#71790 = CARTESIAN_POINT ( 'NONE',  ( 5.567085169132608868, -2.083932277878234096, -0.9915751667191848862 ) ) ;
#71791 = CARTESIAN_POINT ( 'NONE',  ( 4.797606254389322089, 6.690569611577942943, 1.599625672291268286 ) ) ;
#71792 = CARTESIAN_POINT ( 'NONE',  ( 0.9837496482606482573, 1.382075509872608299, 1.528818673835147024 ) ) ;
#71793 = CARTESIAN_POINT ( 'NONE',  ( 7.006866460164219212, 7.069099046480051385, -0.7998128361456281477 ) ) ;
#71794 = ADVANCED_FACE ( 'NONE', ( #204470 ), #105990, .F. ) ;
#71795 = CARTESIAN_POINT ( 'NONE',  ( 6.520923251934013898, 2.292922446452568597, -0.1593734864932250250 ) ) ;
#71796 = CARTESIAN_POINT ( 'NONE',  ( 5.946383829931009224, 4.757679660038602876, 2.499999999987512656 ) ) ;
#71797 = CARTESIAN_POINT ( 'NONE',  ( -7.110325215724114578, 7.260077271291732082, 0.000000000000000000 ) ) ;
#71798 = CARTESIAN_POINT ( 'NONE',  ( 6.192256348250350761, -1.861847689568534081, -0.1814220289034565448 ) ) ;
#71799 = CIRCLE ( 'NONE', #147908, 0.8299999999999999600 ) ;
#71800 = EDGE_CURVE ( 'NONE', #32497, #143111, #140351, .T. ) ;
#71802 = CARTESIAN_POINT ( 'NONE',  ( -5.469788628470539926, 5.346117919495872783, -0.7998128361456362523 ) ) ;
#71801 = CARTESIAN_POINT ( 'NONE',  ( 3.234525475359388391, 1.209690070866603406, -1.481213593849866950 ) ) ;
#71803 = CARTESIAN_POINT ( 'NONE',  ( 5.514374426699260923, -0.9893691592960799364, -1.972764877262770833 ) ) ;
#71804 = CARTESIAN_POINT ( 'NONE',  ( -1.225000000000045386, 1.312500000682802259, -4.336808689942017736E-14 ) ) ;
#71805 = CARTESIAN_POINT ( 'NONE',  ( 1.782949938078044916, -3.499999999999999556, -2.093702347113241213 ) ) ;
#71806 = CARTESIAN_POINT ( 'NONE',  ( 3.702785349863636277, 7.334016984900627811, -0.7216878364870338292 ) ) ;
#71807 = CARTESIAN_POINT ( 'NONE',  ( -3.946832114909637479, 7.618738210787614484, 0.7216878364870338292 ) ) ;
#71808 = CARTESIAN_POINT ( 'NONE',  ( 5.725269513181780567, 1.870077439114096629, 0.9995941271150191598 ) ) ;
#71809 = CARTESIAN_POINT ( 'NONE',  ( 2.679136956247138546, -2.208066087050132520, -0.6703273527271095267 ) ) ;
#71810 = CARTESIAN_POINT ( 'NONE',  ( 3.648837080137564470, -0.3802854374791163616, -1.924481129451253603 ) ) ;
#71811 = CARTESIAN_POINT ( 'NONE',  ( -5.743814354044916470, 6.730146830254374990, -1.199719254218453823 ) ) ;
#71812 = CARTESIAN_POINT ( 'NONE',  ( 0.7253527386562284018, 0.1980078388067410544, -1.951770168129369543 ) ) ;
#71813 = CARTESIAN_POINT ( 'NONE',  ( 7.594853421417097294, 15.38634441068472469, 9.235122635145186720 ) ) ;
#71814 = CARTESIAN_POINT ( 'NONE',  ( 5.713835393516482952, 5.630839145382857680, 0.7998128361456352531 ) ) ;
#71815 = VERTEX_POINT ( 'NONE', #39879 ) ;
#71816 = CARTESIAN_POINT ( 'NONE',  ( 5.700407750362016301, 1.350738941191354625, -1.497498989668680114 ) ) ;
#71817 = CARTESIAN_POINT ( 'NONE',  ( 0.1812672858593766811, -0.8707521589867758260, 1.622202602641155345 ) ) ;
#71818 = DIRECTION ( 'NONE',  ( -0.5005768354468330683, -0.8656921114426503472, 1.942890293094028284E-15 ) ) ;
#71819 = CARTESIAN_POINT ( 'NONE',  ( 3.485384773837760353, 0.04839624821431457585, 2.170676210889192603 ) ) ;
#71820 = CARTESIAN_POINT ( 'NONE',  ( 6.052789233858158369, 6.026285292448116948, 0.000000000000000000 ) ) ;
#71821 = CARTESIAN_POINT ( 'NONE',  ( 0.6684183810189650021, 2.117893379942568988, -0.1100008709709817956 ) ) ;
#71822 = CARTESIAN_POINT ( 'NONE',  ( -0.7500000000000006661, 1.139583334016154526, -1.299038105676652011 ) ) ;
#71823 = CARTESIAN_POINT ( 'NONE',  ( 10.40318394038753702, 11.03146944007395724, -0.7998128361456281477 ) ) ;
#71824 =( NAMED_UNIT ( * ) SI_UNIT ( $, .STERADIAN. ) SOLID_ANGLE_UNIT ( ) );
#71825 = CARTESIAN_POINT ( 'NONE',  ( 5.803742400754204667, 7.332416669035665358, 1.290654366993408297 ) ) ;
#71826 = EDGE_LOOP ( 'NONE', ( #153450, #168788, #18589 ) ) ;
#71827 = CARTESIAN_POINT ( 'NONE',  ( 1.458354148090333258, 0.8324554894755629153, 1.885337613027091352 ) ) ;
#71829 = CARTESIAN_POINT ( 'NONE',  ( 1.499999999999993117, 8.385416667349467446, 0.8660254037844408170 ) ) ;
#71828 = CARTESIAN_POINT ( 'NONE',  ( -8.319899820280397762, 12.85830022363583147, -0.7998128361456281477 ) ) ;
#71830 = CARTESIAN_POINT ( 'NONE',  ( -1.364683531250012516, 0.7802083336747528408, 0.7879004041258379498 ) ) ;
#71831 = CARTESIAN_POINT ( 'NONE',  ( -1.500000000000021316, 5.420833333333356485, 0.8660254037844343777 ) ) ;
#71832 = ORIENTED_EDGE ( 'NONE', *, *, #189245, .T. ) ;
#71833 = CARTESIAN_POINT ( 'NONE',  ( 3.264218543254516103, 1.912461472423479192, -0.002497826895729581952 ) ) ;
#71834 = AXIS2_PLACEMENT_3D ( 'NONE', #6265, #72336, #116899 ) ;
#71835 = CARTESIAN_POINT ( 'NONE',  ( 5.840640841166978348, 0.3488620263497018703, 1.734928340252988033 ) ) ;
#71836 = CARTESIAN_POINT ( 'NONE',  ( 4.864343252252968597, 8.897093904262280972, 0.000000000000000000 ) ) ;
#71837 = CARTESIAN_POINT ( 'NONE',  ( -4.548924232584923288, 5.265832011892554121, -1.199719254218446718 ) ) ;
#71839 = EDGE_CURVE ( 'NONE', #111999, #10691, #104118, .T. ) ;
#71838 = CARTESIAN_POINT ( 'NONE',  ( 0.6503002719215627003, 1.784868618687754926, 0.3088405841149675091 ) ) ;
#71841 = CARTESIAN_POINT ( 'NONE',  ( 0.5674276921618210956, 1.288973137450568407, 1.417358193720698933 ) ) ;
#71840 = CARTESIAN_POINT ( 'NONE',  ( 1.249999999999999334, 8.500000000000000000, -3.469446951953614189E-15 ) ) ;
#71842 = CARTESIAN_POINT ( 'NONE',  ( 1.979048004138800998, 1.930994533390210544, 0.7472069620131777112 ) ) ;
#71843 = CARTESIAN_POINT ( 'NONE',  ( -1.402160292154681736E-14, -0.2406249996585799189, -1.575800808251665908 ) ) ;
#71844 = TOROIDAL_SURFACE ( 'NONE', #109988, 0.1600000000000000033, 0.08000000000000000167 ) ;
#71845 = CARTESIAN_POINT ( 'NONE',  ( 6.631728656526095556, -1.223761959379562114, -1.414937998750566361 ) ) ;
#71846 = CARTESIAN_POINT ( 'NONE',  ( 2.912524513316586461, 1.322148455168963510, -1.259233298254287536 ) ) ;
#71848 = CARTESIAN_POINT ( 'NONE',  ( 6.162627863271451290, 6.966383021533493647, 0.9102919922300183320 ) ) ;
#71847 = CARTESIAN_POINT ( 'NONE',  ( 0.06561565146986823860, -2.064482179495107150, -1.031447015078267304 ) ) ;
#71849 = CARTESIAN_POINT ( 'NONE',  ( -1.402160292154681736E-14, -0.3031249996585801965, -1.575800808251665908 ) ) ;
#71850 = CARTESIAN_POINT ( 'NONE',  ( 3.824720269693319796, -1.387356309220557193, 1.526538889744559313 ) ) ;
#71851 = CARTESIAN_POINT ( 'NONE',  ( -6.039267359883488950, 9.133230122250985517, 1.199719254218452047 ) ) ;
#71852 = CARTESIAN_POINT ( 'NONE',  ( 7.293396569147545527, 10.59638086639245280, 1.199719254218460707 ) ) ;
#71853 = CARTESIAN_POINT ( 'NONE',  ( 5.867981556616276073, 5.740399992340776691, -0.7998128361456282587 ) ) ;
#71854 = CARTESIAN_POINT ( 'NONE',  ( 0.4214394802095830506, -0.1064560406111268731, 2.159113264384164399 ) ) ;
#71855 = ADVANCED_FACE ( 'NONE', ( #120128 ), #28033, .T. ) ;
#71856 = CARTESIAN_POINT ( 'NONE',  ( 0.1862956123577602652, -1.336862347539343965, -1.711682565949741885 ) ) ;
#71857 = CARTESIAN_POINT ( 'NONE',  ( -0.6823417656250003738, 1.530208333674752730, -1.181850606188749264 ) ) ;
#71858 = CARTESIAN_POINT ( 'NONE',  ( 3.567792053227138105, 2.109782723108716063, -0.4697668898906853796 ) ) ;
#71859 = CARTESIAN_POINT ( 'NONE',  ( 3.985024733980116363, -1.885273983189727831, -0.7249480779877092163 ) ) ;
#71862 = CARTESIAN_POINT ( 'NONE',  ( 6.534666852106798096, 7.686494751288491578, -1.082531754730543083 ) ) ;
#71861 = CARTESIAN_POINT ( 'NONE',  ( 1.642778471875001811, -3.842708332855375275, 2.845375778867859751 ) ) ;
#71860 = CARTESIAN_POINT ( 'NONE',  ( 0.000000000000000000, 7.250000000000006217, 0.000000000000000000 ) ) ;
#71863 = CARTESIAN_POINT ( 'NONE',  ( -6.469175572376043348, 7.576401584974034265, 1.199719254218452047 ) ) ;
#71864 = CARTESIAN_POINT ( 'NONE',  ( 2.272673044126482189, -0.3494851828299732621, -1.985868527484459634 ) ) ;
#71865 = CARTESIAN_POINT ( 'NONE',  ( -6.581593504430098385, 9.765943957555402122, -1.199719254218440723 ) ) ;
#71867 = CARTESIAN_POINT ( 'NONE',  ( -1.201851678989727383E-14, 3.134375000341420137, 1.575800808251672791 ) ) ;
#71866 = CARTESIAN_POINT ( 'NONE',  ( -3.255929445576174697, 6.950334786480840243, -0.7998128361456281477 ) ) ;
#71868 = CARTESIAN_POINT ( 'NONE',  ( -3.721290253490582955, 7.355952296265487078, 0.5966894627213925606 ) ) ;
#71869 = CARTESIAN_POINT ( 'NONE',  ( 5.871340715825056122, -1.643613990083541143, -0.9773822251149253404 ) ) ;
#71870 = LINE ( 'NONE', #136913, #167082 ) ;
#71871 = CARTESIAN_POINT ( 'NONE',  ( 6.629573926958101993, 6.836850457647000390, -0.7216878364870257245 ) ) ;
#71873 = CARTESIAN_POINT ( 'NONE',  ( 3.989861366179075386, -2.010826228832915508, 0.1511578083489423796 ) ) ;
#71872 = CARTESIAN_POINT ( 'NONE',  ( -7.741342523278709642, 10.05465224862374285, 1.443375672974090751 ) ) ;
#71874 = CARTESIAN_POINT ( 'NONE',  ( -1.500000000000011324, 4.420833333333352044, 0.8660254037844403729 ) ) ;
#71875 = CARTESIAN_POINT ( 'NONE',  ( 1.364683531249996529, 15.02604166700806587, 0.7879004041258405033 ) ) ;
#71876 = CARTESIAN_POINT ( 'NONE',  ( 6.194358799569198659, -1.717016665659231167, -0.1635641229304989064 ) ) ;
#71877 = CARTESIAN_POINT ( 'NONE',  ( 4.389807875774629942, 8.343469298370917997, 0.7998128361456271485 ) ) ;
#71879 = CARTESIAN_POINT ( 'NONE',  ( -0.7500000000000006661, 10.48958333401613174, -1.299038105676657340 ) ) ;
#71878 = CARTESIAN_POINT ( 'NONE',  ( 8.432808358020016826, 10.86136238915529084, 1.443375672974076540 ) ) ;
#71880 = FACE_OUTER_BOUND ( 'NONE', #100318, .T. ) ;
#71881 = CARTESIAN_POINT ( 'NONE',  ( 5.589076619078012342, 1.650032040524500143, -0.8810306647013477210 ) ) ;
#71882 = CARTESIAN_POINT ( 'NONE',  ( -0.1047997906430510606, -0.1421793342430139606, -1.981047221590222840 ) ) ;
#71883 = CARTESIAN_POINT ( 'NONE',  ( -9.617648866954029430, -9.063431457505044975, 0.6035590660249372519 ) ) ;
#71884 = CARTESIAN_POINT ( 'NONE',  ( 1.920843890195075510, -1.466934385316904343, 1.461102248941518855 ) ) ;
#71885 = CARTESIAN_POINT ( 'NONE',  ( -2.276824562219559311E-15, -8.605993949662213538, -10.72098668450194303 ) ) ;
#71886 = ORIENTED_EDGE ( 'NONE', *, *, #165463, .F. ) ;
#71887 = CARTESIAN_POINT ( 'NONE',  ( 4.415115299905642665, 5.179997933758551554, -1.199719254218450271 ) ) ;
#71888 = CARTESIAN_POINT ( 'NONE',  ( 0.4039230143318903177, -1.081087622585241714, -1.701935196855845822 ) ) ;
#71889 = CARTESIAN_POINT ( 'NONE',  ( 1.353448696812571850, -1.313440895511051032, -1.247944760566013223 ) ) ;
#71890 = CARTESIAN_POINT ( 'NONE',  ( 4.923019175093585886, 5.876515471431535076, -1.082531754730548412 ) ) ;
#71891 = AXIS2_PLACEMENT_3D ( 'NONE', #33030, #486, #127428 ) ;
#71892 = DIRECTION ( 'NONE',  ( -0.000000000000000000, -1.000000000000000000, -0.000000000000000000 ) ) ;
#71893 = CARTESIAN_POINT ( 'NONE',  ( 8.120970824461352322, 9.537182719035495637, -1.082531754730543083 ) ) ;
#71894 = CARTESIAN_POINT ( 'NONE',  ( 6.265839547809997079, 10.46189657242035587, 0.7998128361456462443 ) ) ;
#71896 = CARTESIAN_POINT ( 'NONE',  ( 6.064071300241554496, -1.020233025338047383, 1.621115200587377014 ) ) ;
#71895 = CARTESIAN_POINT ( 'NONE',  ( -5.530836599371015794, 8.540060901653093950, 1.199719254218452047 ) ) ;
#71897 = DIRECTION ( 'NONE',  ( 1.000000000000000000, -0.000000000000000000, -0.000000000000000000 ) ) ;
#71898 = DIRECTION ( 'NONE',  ( 7.993605777301127091E-15, 0.000000000000000000, 1.000000000000000000 ) ) ;
#71899 =( BOUNDED_SURFACE ( )  B_SPLINE_SURFACE ( 3, 2, ( 
 ( #82901, #47246, #113360 ),
 ( #180418, #97062, #164174 ),
 ( #30987, #78640, #115475 ),
 ( #61340, #45114, #32036 ) ),
 .UNSPECIFIED., .F., .F., .T. ) 
 B_SPLINE_SURFACE_WITH_KNOTS ( ( 4, 4 ),
 ( 3, 3 ),
 ( 0.005330693667047291598, 0.008357081610771106145 ),
 ( 0.000000000000000000, 1.000000000000000000 ),
 .UNSPECIFIED. ) 
 GEOMETRIC_REPRESENTATION_ITEM ( )  RATIONAL_B_SPLINE_SURFACE ( (
 ( 1.000000000000000000, 0.7187737999613688089, 1.000000000000000000),
 ( 1.000000000000000000, 0.7186585579880990782, 1.000000000000000000),
 ( 1.000000000000000000, 0.7185467277397579178, 1.000000000000000000),
 ( 1.000000000000000000, 0.7184380228464051221, 1.000000000000000000) ) ) 
 REPRESENTATION_ITEM ( '' )  SURFACE ( )  );
#71900 = CARTESIAN_POINT ( 'NONE',  ( 1.419999999999822737, 7.204077025658621736, 4.238769367544763966 ) ) ;
#71902 = ORIENTED_EDGE ( 'NONE', *, *, #204332, .T. ) ;
#71901 = CARTESIAN_POINT ( 'NONE',  ( 4.907688418466886304, 5.788353245375237321, -1.082531754730548412 ) ) ;
#71903 = CARTESIAN_POINT ( 'NONE',  ( -6.697364695470783502, 10.75741654478384035, 0.7216878364870458196 ) ) ;
#71904 = CARTESIAN_POINT ( 'NONE',  ( 2.870174731959000525, 1.155358403710282866, 1.826860881501219280 ) ) ;
#71905 = CARTESIAN_POINT ( 'NONE',  ( -7.322812365156824654, 8.676274193172000437, 1.082531754730549078 ) ) ;
#71906 = CARTESIAN_POINT ( 'NONE',  ( 6.373741612200162443, 8.529394195690610303, 1.443375672974065660 ) ) ;
#71907 = CARTESIAN_POINT ( 'NONE',  ( 0.4926326669930108371, -1.172979896111199904, 1.766458537607276336 ) ) ;
#71908 = CARTESIAN_POINT ( 'NONE',  ( 5.526323803393727196, 1.085782926936417425, -1.467421699745217190 ) ) ;
#71909 = CARTESIAN_POINT ( 'NONE',  ( 2.301971997355524824, -1.971002988154029412, 0.04462483508816358219 ) ) ;
#71910 = CARTESIAN_POINT ( 'NONE',  ( 4.218947473185084007, 1.474887410857337100, -1.217315437338606365 ) ) ;
#71911 = ORIENTED_EDGE ( 'NONE', *, *, #181109, .T. ) ;
#71912 = CARTESIAN_POINT ( 'NONE',  ( -11.41381675112459781, 10.19999999999998863, -3.704697986577260682 ) ) ;
#71913 = CARTESIAN_POINT ( 'NONE',  ( 4.475032023839897732, 1.799880929630924165, 0.8001706733358445733 ) ) ;
#71914 = CARTESIAN_POINT ( 'NONE',  ( 0.7966981359470609592, 1.587242811699969725, 1.118599961973030021 ) ) ;
#71915 = VERTEX_POINT ( 'NONE', #189317 ) ;
#71916 = CARTESIAN_POINT ( 'NONE',  ( -4.274563570058511175, 8.209017608368725405, 0.000000000000000000 ) ) ;
#71917 = CARTESIAN_POINT ( 'NONE',  ( -4.472210567661380587, 6.310941310395290493, 1.599625672291270506 ) ) ;
#71920 = EDGE_CURVE ( 'NONE', #100909, #19519, #213034, .T. ) ;
#71919 = CARTESIAN_POINT ( 'NONE',  ( 5.628043163004202931, 8.619781885929965526, -1.082531754730548412 ) ) ;
#71918 = CARTESIAN_POINT ( 'NONE',  ( 7.904567251967224095, 9.180748867838630645, 1.199719254218462483 ) ) ;
#71922 = ORIENTED_EDGE ( 'NONE', *, *, #86821, .T. ) ;
#71921 = CARTESIAN_POINT ( 'NONE',  ( 4.828717125059535320, 1.315996081294769304, -1.387672938220223307 ) ) ;
#71923 = CARTESIAN_POINT ( 'NONE',  ( 0.8157880970438775581, -0.3219574891645953785, 2.183050487710703536 ) ) ;
#71924 = CARTESIAN_POINT ( 'NONE',  ( -15.75000000000000000, 12.30000000000000071, 0.6999999999999992895 ) ) ;
#71925 = CARTESIAN_POINT ( 'NONE',  ( 0.04731519813723152057, -1.748418646119804576, 0.7749314921376224685 ) ) ;
#71926 = CARTESIAN_POINT ( 'NONE',  ( 0.07661050522433668353, 0.008287133257128471639, -1.710863442170395432 ) ) ;
#71927 = CARTESIAN_POINT ( 'NONE',  ( -5.688757509019083614, 5.629766575900002401, -2.420000000000000373 ) ) ;
#71928 = CARTESIAN_POINT ( 'NONE',  ( 2.734898984476673789, -1.980466496001157317, -0.6033880717724802167 ) ) ;
#71929 = CARTESIAN_POINT ( 'NONE',  ( -5.052384799386910430, 9.046199365926717917, 1.214306433183764966E-14 ) ) ;
#71930 = CIRCLE ( 'NONE', #161809, 11.00000000000000000 ) ;
#71931 = CARTESIAN_POINT ( 'NONE',  ( -4.616709804987970678, 8.367809121204862421, 0.2297300046584915267 ) ) ;
#71933 = CARTESIAN_POINT ( 'NONE',  ( 0.3917762336288696523, 1.602822130585265015, 1.450656209987542855 ) ) ;
#71932 = CARTESIAN_POINT ( 'NONE',  ( -3.567766978690493307, 7.314145241780881435, 1.040834085586084257E-14 ) ) ;
#71934 = DIRECTION ( 'NONE',  ( -1.000000000000000000, 0.000000000000000000, 0.000000000000000000 ) ) ;
#71935 = CARTESIAN_POINT ( 'NONE',  ( 6.048345925472191631, 6.229027465905275562, 0.7216878364870328300 ) ) ;
#71936 = CARTESIAN_POINT ( 'NONE',  ( 1.926047848139553986, 3.520667328614982328, -0.3999999999999993006 ) ) ;
#71937 = CARTESIAN_POINT ( 'NONE',  ( -1.364683531250000748, 12.92187500034139980, 0.000000000000000000 ) ) ;
#71939 = CARTESIAN_POINT ( 'NONE',  ( -6.317173229324657413, 6.334733287159020954, 0.000000000000000000 ) ) ;
#71938 = CARTESIAN_POINT ( 'NONE',  ( 6.925078400183553029, 7.052683076116534444, 2.553806833665558162 ) ) ;
#71940 = CARTESIAN_POINT ( 'NONE',  ( 4.729033670188855787, 1.730023327335796113, 0.1204123811070593880 ) ) ;
#71941 = CARTESIAN_POINT ( 'NONE',  ( -3.079673448598517549, 6.744702790006905424, 1.040834085586084257E-14 ) ) ;
#71942 = AXIS2_PLACEMENT_3D ( 'NONE', #18437, #179897, #64008 ) ;
#71943 = CARTESIAN_POINT ( 'NONE',  ( 2.870052101067874339, -2.048368873657464118, 0.2992715783270774588 ) ) ;
#71944 = CARTESIAN_POINT ( 'NONE',  ( 4.042653799040228257, -1.567611697763098055, 1.423267961261857950 ) ) ;
#71945 = CARTESIAN_POINT ( 'NONE',  ( 7.450369105909416589, 8.650851030771185890, -1.199719254218441611 ) ) ;
#71946 = CARTESIAN_POINT ( 'NONE',  ( -1.364683531249997417, 3.509375000341423245, 1.214306433183764966E-14 ) ) ;
#71947 = CARTESIAN_POINT ( 'NONE',  ( 2.043745906638486431, 1.354474275242853798, 1.429983431767953617 ) ) ;
#71948 = CARTESIAN_POINT ( 'NONE',  ( 6.113440106766272031, 6.016660024919275429, -0.07562458862005703997 ) ) ;
#71949 = CARTESIAN_POINT ( 'NONE',  ( 0.9668906521006037647, -1.505869814250645478, 1.178657042999963878 ) ) ;
#71950 = CARTESIAN_POINT ( 'NONE',  ( 4.892671604017262865, 1.907728271999886704, -1.270570218630202808 ) ) ;
#71951 = CARTESIAN_POINT ( 'NONE',  ( 1.928079105319381314, 1.052063804484974385, -1.491885150056403653 ) ) ;
#71952 = CARTESIAN_POINT ( 'NONE',  ( 4.716257332707354699, 6.595662536282280719, -1.599625672291269396 ) ) ;
#71953 = CARTESIAN_POINT ( 'NONE',  ( 4.975479186090847605, 7.788180902872553268, 1.082531754730558626 ) ) ;
#71954 = CARTESIAN_POINT ( 'NONE',  ( -8.505042434474312074, 8.816971016508505343, -0.7998128361456291469 ) ) ;
#71955 = CARTESIAN_POINT ( 'NONE',  ( 2.935794159824364868, -1.939102465223912830, 0.5408614042671439082 ) ) ;
#71956 = CARTESIAN_POINT ( 'NONE',  ( 3.133595828963112950, 1.864314371477162169, -0.6108997337519045390 ) ) ;
#71957 = CARTESIAN_POINT ( 'NONE',  ( -7.323375529675950624, 11.69568855126397011, -0.7998128361456291469 ) ) ;
#71958 = CARTESIAN_POINT ( 'NONE',  ( -5.708146366553361162, 6.618257834855742594, -1.199719254218446718 ) ) ;
#71959 = CARTESIAN_POINT ( 'NONE',  ( -1.499999999999997780, 5.681250000682820378, 1.214306433183764966E-14 ) ) ;
#71961 = CARTESIAN_POINT ( 'NONE',  ( 5.119873625132255412, -0.9486883152997215296, -1.493885749217472636 ) ) ;
#71960 = CARTESIAN_POINT ( 'NONE',  ( 5.718719656712253574, -0.05221879637645754357, 2.090152071033167136 ) ) ;
#71962 = DIRECTION ( 'NONE',  ( -8.881784197001252323E-16, 0.000000000000000000, 1.000000000000000000 ) ) ;
#71963 = CARTESIAN_POINT ( 'NONE',  ( 0.9729166594223404019, -0.05710519180573449260, -2.190871861337650994 ) ) ;
#71964 = CARTESIAN_POINT ( 'NONE',  ( 0.09860955243249854008, -0.4675299588126168859, 1.676413046982327515 ) ) ;
#71965 = CARTESIAN_POINT ( 'NONE',  ( 7.786460292950004636, 7.978625184730144149, 1.040834085586084257E-14 ) ) ;
#71966 = CARTESIAN_POINT ( 'NONE',  ( -4.787437654953776267, 6.678706214094487947, -1.250000000000001110 ) ) ;
#71967 = CARTESIAN_POINT ( 'NONE',  ( 5.695955869756449630, 2.025510559372576402, 1.086827626776807554 ) ) ;
#71968 = CARTESIAN_POINT ( 'NONE',  ( -0.1290005225502675879, -0.006633637972621592160, -2.173875058097324064 ) ) ;
#71969 = CARTESIAN_POINT ( 'NONE',  ( 5.360564742968721319, -0.6223997329263281086, 1.618453672356393147 ) ) ;
#71970 = CARTESIAN_POINT ( 'NONE',  ( 2.262606014870732096, 0.9450075053254001212, 1.994452002680577429 ) ) ;
#71971 =( BOUNDED_CURVE ( )  B_SPLINE_CURVE ( 3, ( #81428, #28413, #130262, #78224 ),
 .UNSPECIFIED., .F., .T. ) 
 B_SPLINE_CURVE_WITH_KNOTS ( ( 4, 4 ),
 ( 0.4999999999999986677, 1.000000000000000000 ),
 .UNSPECIFIED. ) 
 CURVE ( )  GEOMETRIC_REPRESENTATION_ITEM ( )  RATIONAL_B_SPLINE_CURVE ( ( 1.000000000000001998, 0.3333333333333334259, 0.3333333333333316495, 1.000000000000000222 ) ) 
 REPRESENTATION_ITEM ( '' )  );
#71972 = CARTESIAN_POINT ( 'NONE',  ( 0.6905673677243575614, 1.117554423744430592, -1.861242299804190869 ) ) ;
#71973 = CARTESIAN_POINT ( 'NONE',  ( -0.4800000000000000933, 2.999999999999999112, -2.500000000000000444 ) ) ;
#71974 = CARTESIAN_POINT ( 'NONE',  ( 0.8314520141109645879, -1.673154641659507558, -1.297526329946703472 ) ) ;
#71975 = CARTESIAN_POINT ( 'NONE',  ( 3.468750000000001776, 0.7852924748298147906, -1.895863743164155180 ) ) ;
#71976 = CARTESIAN_POINT ( 'NONE',  ( -0.07278863622987721826, 7.008482404162161394, -2.000259058016610414 ) ) ;
#71977 = CARTESIAN_POINT ( 'NONE',  ( 4.805647293689061961, -0.5139743781695116365, 1.856484447351488765 ) ) ;
#71978 = CARTESIAN_POINT ( 'NONE',  ( 0.8740457437188209333, 0.4279768726487084285, -2.179530559632827824 ) ) ;
#71979 = VERTEX_POINT ( 'NONE', #22525 ) ;
#71981 = CARTESIAN_POINT ( 'NONE',  ( -1.500000000000011324, 4.379166666666688634, -0.8660254037844313801 ) ) ;
#71980 = CARTESIAN_POINT ( 'NONE',  ( 1.330038945030669995, 1.124775647945252643, -1.997386028781794387 ) ) ;
#71982 = CARTESIAN_POINT ( 'NONE',  ( 6.173040012923759257, 6.096301524699504704, -0.7998128361456281477 ) ) ;
#71983 = CARTESIAN_POINT ( 'NONE',  ( 6.505214776458575265, 6.483838748823460563, 1.040834085586084257E-14 ) ) ;
#71984 = AXIS2_PLACEMENT_3D ( 'NONE', #15427, #80451, #115147 ) ;
#71985 = CARTESIAN_POINT ( 'NONE',  ( 3.739129200393681796, 2.109584919444119855, 0.6958237802787976545 ) ) ;
#71986 = CARTESIAN_POINT ( 'NONE',  ( -7.036318535812428721, 11.15286269184909784, 0.000000000000000000 ) ) ;
#71987 =( LENGTH_UNIT ( ) NAMED_UNIT ( * ) SI_UNIT ( .MILLI., .METRE. ) );
#71988 = CARTESIAN_POINT ( 'NONE',  ( 5.490689023854504747, 9.349628261231513804, 1.040834085586084257E-14 ) ) ;
#71989 = CARTESIAN_POINT ( 'NONE',  ( -8.717529583462656717, 11.19353715217169309, 1.443375672974064550 ) ) ;
#71990 = CARTESIAN_POINT ( 'NONE',  ( 5.858531774880875176, 9.849054480754103835, -0.7216878364870458196 ) ) ;
#71991 = CARTESIAN_POINT ( 'NONE',  ( 1.477185633673218534, -2.006960102380969779, -0.1948397147320118372 ) ) ;
#71993 = CARTESIAN_POINT ( 'NONE',  ( 0.4442778734073973279, -0.9756673871180139290, 1.817250197203540640 ) ) ;
#71992 = CARTESIAN_POINT ( 'NONE',  ( 7.456094412511537151, 10.78619501698377370, 1.199719254218460707 ) ) ;
#71994 = FACE_OUTER_BOUND ( 'NONE', #140926, .T. ) ;
#71995 = CARTESIAN_POINT ( 'NONE',  ( 6.333067150914805765, 9.442309871825708356, 1.082531754730549967 ) ) ;
#71996 = CARTESIAN_POINT ( 'NONE',  ( 0.2922019606856861018, 1.531309713818730822, -1.022077305420886040 ) ) ;
#71997 = CARTESIAN_POINT ( 'NONE',  ( -3.009396220815599321, 6.452359640394901952, 0.6004564335717228474 ) ) ;
#71998 = CARTESIAN_POINT ( 'NONE',  ( -1.364683531250012516, 2.530208333674753174, 0.7879004041258379498 ) ) ;
#71999 = CARTESIAN_POINT ( 'NONE',  ( 1.176598488244801954, -0.03600270464337343435, -1.769546047349578100 ) ) ;
#72000 = CARTESIAN_POINT ( 'NONE',  ( 6.522076087392383315, -1.544353836717025308, 0.7889432867928622972 ) ) ;
#72001 = CARTESIAN_POINT ( 'NONE',  ( 0.3449248370967008537, 0.5783895242766275979, -1.748133987124582012 ) ) ;
#72002 = CARTESIAN_POINT ( 'NONE',  ( 3.773197156129989516, 2.158245952819247471, -0.7729258541082913991 ) ) ;
#72003 = CARTESIAN_POINT ( 'NONE',  ( 3.275182144284936925, 1.168729223632531733, 1.422615900182722992 ) ) ;
#72004 = CARTESIAN_POINT ( 'NONE',  ( 7.099665995050449041, 11.43469409420089455, 0.7998128361456462443 ) ) ;
#72005 = CARTESIAN_POINT ( 'NONE',  ( 4.682524874021861017, -1.770931954651306262, -0.4427778663074270482 ) ) ;
#72006 = CARTESIAN_POINT ( 'NONE',  ( 4.746720300533005421, 1.994071680685698400, -0.2986252114312442640 ) ) ;
#72007 = CARTESIAN_POINT ( 'NONE',  ( -9.504429378379839477, 11.04725468198666150, 1.199719254218462483 ) ) ;
#72009 = CARTESIAN_POINT ( 'NONE',  ( -5.759181390754928742, 9.941071732514568993, 0.000000000000000000 ) ) ;
#72008 = CARTESIAN_POINT ( 'NONE',  ( 3.995213114784367026, 1.913063998889670714, -1.207689374757703771 ) ) ;
#72010 = CARTESIAN_POINT ( 'NONE',  ( 5.842829903504588529, 0.4074447676574670107, 2.065989314711280667 ) ) ;
#72011 = CARTESIAN_POINT ( 'NONE',  ( 8.961696533999443659, 14.59015583931033611, 8.974872064516899783 ) ) ;
#72012 = CARTESIAN_POINT ( 'NONE',  ( 3.754400092289136737, -2.067862582909282487, -0.1045053291982081939 ) ) ;
#72013 = CARTESIAN_POINT ( 'NONE',  ( 2.920892028740289081, 5.495125569250587816, 1.199719254218452047 ) ) ;
#72014 = CARTESIAN_POINT ( 'NONE',  ( 1.360316468749941610, 2.276041667008116942, 0.7853790794158921340 ) ) ;
#72015 = CARTESIAN_POINT ( 'NONE',  ( 5.356147330077114077, 0.8591290142025624910, -1.938821108677920346 ) ) ;
#72017 = CARTESIAN_POINT ( 'NONE',  ( 0.9789820196765993687, -0.04640813864221354085, -1.926104504880983725 ) ) ;
#72016 = CARTESIAN_POINT ( 'NONE',  ( -9.840520565420403543, 10.37502883594562597, 1.040834085586084257E-14 ) ) ;
#72018 = PLANE ( 'NONE',  #175401 ) ;
#72019 = CARTESIAN_POINT ( 'NONE',  ( 0.3616804892651844239, -0.5289564462071428830, 1.897103703902315530 ) ) ;
#72020 = CARTESIAN_POINT ( 'NONE',  ( 3.702785349863636277, 7.334016984900627811, -0.7216878364870338292 ) ) ;
#72021 = CARTESIAN_POINT ( 'NONE',  ( 5.364345920411571100, 6.316227854031381206, 1.080878399565273540 ) ) ;
#72022 = CARTESIAN_POINT ( 'NONE',  ( -3.469446951953614189E-15, 3.500000000000003109, 2.602085213965210642E-15 ) ) ;
#72023 = AXIS2_PLACEMENT_3D ( 'NONE', #77722, #158982, #110299 ) ;
#72024 = CARTESIAN_POINT ( 'NONE',  ( -4.874319919312905647, 5.645460313075203018, -1.199719254218446718 ) ) ;
#72025 = CARTESIAN_POINT ( 'NONE',  ( 1.108037262132562262, 1.686735864949813202, 1.445688421275423075 ) ) ;
#72026 = CARTESIAN_POINT ( 'NONE',  ( 2.573382939595921570, 0.1044104795966259297, -2.103504788083962573 ) ) ;
#72027 = CARTESIAN_POINT ( 'NONE',  ( -2.844178363816758814, 6.540234867753325076, -0.7998128361456481317 ) ) ;
#72028 = CARTESIAN_POINT ( 'NONE',  ( 7.832860060393120882, 10.16142270859057462, 1.599625672291281386 ) ) ;
#72029 = CARTESIAN_POINT ( 'NONE',  ( 0.9415990247386073486, 1.246032235168346380, 1.382555731526733611 ) ) ;
#72030 = CARTESIAN_POINT ( 'NONE',  ( 6.531277313481192337, 8.642909503859968368, 1.599625672291281386 ) ) ;
#72031 = CARTESIAN_POINT ( 'NONE',  ( -2.609770642201835855, 0.3830433331901555993, -0.1872689674646474400 ) ) ;
#72032 = CARTESIAN_POINT ( 'NONE',  ( -6.943184063974178422, 8.233374508458908281, -1.082531754730549967 ) ) ;
#72033 = CARTESIAN_POINT ( 'NONE',  ( -9.178506806771670412, 9.810605484096178941, 1.040834085586084257E-14 ) ) ;
#72034 = CARTESIAN_POINT ( 'NONE',  ( 0.6859744409541921328, 2.042103856186634925, -0.5713114342573709648 ) ) ;
#72035 = CARTESIAN_POINT ( 'NONE',  ( -5.901542003698421190, 10.10715911428198055, 0.000000000000000000 ) ) ;
#72037 = CARTESIAN_POINT ( 'NONE',  ( 3.402741375674179114, 0.4741672551989496998, 1.903589013717405853 ) ) ;
#72036 = CARTESIAN_POINT ( 'NONE',  ( 1.224999999999995204, 0.1249999999999862332, -6.938893903907228378E-15 ) ) ;
#72038 = CARTESIAN_POINT ( 'NONE',  ( 2.659225025413253007, -1.880336703546074073, -1.066323988048665017 ) ) ;
#72039 = CARTESIAN_POINT ( 'NONE',  ( 1.891909123491273492, -0.4922293657834125313, -1.774144672653771293 ) ) ;
#72041 = CARTESIAN_POINT ( 'NONE',  ( -6.007394967034264788, 6.077829431587280062, -0.6506939886842719734 ) ) ;
#72040 = CARTESIAN_POINT ( 'NONE',  ( -5.971440312176176768, 5.931378217152456500, 0.000000000000000000 ) ) ;
#72042 = EDGE_CURVE ( 'NONE', #204338, #48843, #42029, .T. ) ;
#72043 = CARTESIAN_POINT ( 'NONE',  ( 3.468456934111513235, 0.04105959252117792613, -1.740014521098575351 ) ) ;
#72044 = AXIS2_PLACEMENT_3D ( 'NONE', #172312, #57491, #59615 ) ;
#72045 = CARTESIAN_POINT ( 'NONE',  ( 4.473827502829567315, 7.202920605734387749, -1.082531754730548412 ) ) ;
#72046 = CARTESIAN_POINT ( 'NONE',  ( -11.31903982423144051, 5.215113036472975416, 5.710294617915439019 ) ) ;
#72047 = CARTESIAN_POINT ( 'NONE',  ( 0.6554165194554737450, -1.826866057147133349, -1.155366728873077342 ) ) ;
#72048 = EDGE_CURVE ( 'NONE', #120109, #211752, #3545, .T. ) ;
#72049 = CARTESIAN_POINT ( 'NONE',  ( 2.829453700430568652, -1.392333688140505510, 1.458332250898628057 ) ) ;
#72050 = CARTESIAN_POINT ( 'NONE',  ( 6.825078400183551608, 0.5660753733540256905, 2.196387875007102419 ) ) ;
#72051 = CARTESIAN_POINT ( 'NONE',  ( 0.6026772488060898603, -0.7295331166810551382, -2.035022307366324945 ) ) ;
#72052 = CARTESIAN_POINT ( 'NONE',  ( 2.676590784821473168, -1.886132711224804748, -0.5737105244360584111 ) ) ;
#72053 = CARTESIAN_POINT ( 'NONE',  ( 6.609000000000012420, 2.456927087449762404, 2.283703893460458989 ) ) ;
#72054 = CARTESIAN_POINT ( 'NONE',  ( 2.700647863620793121, 1.641916212795376806, 1.036879047414513755 ) ) ;
#72057 = ORIENTED_EDGE ( 'NONE', *, *, #954, .T. ) ;
#72056 = CARTESIAN_POINT ( 'NONE',  ( -4.502716413514310290, 6.346531463890372926, -1.443375672974066548 ) ) ;
#72055 = CARTESIAN_POINT ( 'NONE',  ( 6.504189997394580480, -0.8109953713257547214, 1.730197269205424160 ) ) ;
#72058 = CARTESIAN_POINT ( 'NONE',  ( -5.614485009390564940, 5.722856397143323726, 0.000000000000000000 ) ) ;
#72059 = CARTESIAN_POINT ( 'NONE',  ( 5.896870467300973750, 5.844380064798101237, 0.7998128361456352531 ) ) ;
#72060 = EDGE_CURVE ( 'NONE', #76748, #183021, #130265, .T. ) ;
#72061 = CARTESIAN_POINT ( 'NONE',  ( -4.945692173934974178, 8.992000979557944973, 0.000000000000000000 ) ) ;
#72062 = CARTESIAN_POINT ( 'NONE',  ( -7.442499979258930587, 7.647614495415686164, -0.7998128361456362523 ) ) ;
#72063 = CARTESIAN_POINT ( 'NONE',  ( -1.350829346764931271, 4.253646974019544835, -0.3155766437963781201 ) ) ;
#72064 = CARTESIAN_POINT ( 'NONE',  ( 0.5521677985501523001, 0.6901698128830742185, -2.096122547012829962 ) ) ;
#72065 = DIRECTION ( 'NONE',  ( 0.000000000000000000, 1.000000000000000000, 0.000000000000000000 ) ) ;
#72066 = CARTESIAN_POINT ( 'NONE',  ( 4.030091663008243508, 1.086175826233202857, 1.633415718976807041 ) ) ;
#72067 = CARTESIAN_POINT ( 'NONE',  ( 6.774270308322468459, 11.05506579301824743, 0.7998128361456462443 ) ) ;
#72068 = CARTESIAN_POINT ( 'NONE',  ( 1.442029965644067158, -1.730867108953790590, -1.034163949609874233 ) ) ;
#72069 = VERTEX_POINT ( 'NONE', #79827 ) ;
#72070 = CARTESIAN_POINT ( 'NONE',  ( 1.921263159425983913, -1.888806403119867916, 0.9570566162820994816 ) ) ;
#72071 = CARTESIAN_POINT ( 'NONE',  ( -1.402160292154681736E-14, 1.118750000682820378, -1.732050807568863648 ) ) ;
#72073 = CARTESIAN_POINT ( 'NONE',  ( -6.018930129462987999, 9.109503353427070849, 1.199719254218452047 ) ) ;
#72072 = SURFACE_SIDE_STYLE ('',( #152287 ) ) ;
#72074 = CARTESIAN_POINT ( 'NONE',  ( 3.486116527793288178, -0.3603757036649730683, -1.805346353211812804 ) ) ;
#72075 = ORIENTED_EDGE ( 'NONE', *, *, #73178, .T. ) ;
#72076 = CARTESIAN_POINT ( 'NONE',  ( -10.48453286206953727, 11.12637651536962125, 0.7998128361456462443 ) ) ;
#72077 = CARTESIAN_POINT ( 'NONE',  ( -1.500000000000079936, 7.267697830503743184, 4.207111467970349850 ) ) ;
#72078 = CARTESIAN_POINT ( 'NONE',  ( 4.342108446431157454, -1.306982937058022820, -1.669832246961988176 ) ) ;
#72079 = CARTESIAN_POINT ( 'NONE',  ( -0.02377707250108065939, -0.1326659201078099481, -1.811169398030491928 ) ) ;
#72080 = CARTESIAN_POINT ( 'NONE',  ( -1.500000000000011324, 5.452083334016153415, 0.8660254037844403729 ) ) ;
#72081 = CARTESIAN_POINT ( 'NONE',  ( 7.558834334818744338, 8.777393797832065303, 1.199719254218462483 ) ) ;
#72082 = CARTESIAN_POINT ( 'NONE',  ( 6.737475991348287785, 6.825086509519945999, -0.7998128361456481317 ) ) ;
#72083 = CARTESIAN_POINT ( 'NONE',  ( 4.095036773856917556, 1.742982576809920303, -1.099142878725319239 ) ) ;
#72085 = CARTESIAN_POINT ( 'NONE',  ( 1.680954830071922812, 1.270413995023990106, 1.332975479855981416 ) ) ;
#72084 = CARTESIAN_POINT ( 'NONE',  ( -7.497822643557261024, 8.706213491360317747, -1.199719254218446718 ) ) ;
#72086 = CARTESIAN_POINT ( 'NONE',  ( 1.184414575232636047, -6.859386807788068932E-15, 0.6925866048970821254 ) ) ;
#72087 = FACE_OUTER_BOUND ( 'NONE', #199318, .T. ) ;
#72088 = CARTESIAN_POINT ( 'NONE',  ( -1.492665153618444762, 8.694790292835948620, 2.590406265390401419 ) ) ;
#72089 = DIRECTION ( 'NONE',  ( 1.000000000000000000, 3.451266460341926649E-31, 8.638326563840809144E-31 ) ) ;
#72090 = AXIS2_PLACEMENT_3D ( 'NONE', #188385, #9635, #108286 ) ;
#72091 = CARTESIAN_POINT ( 'NONE',  ( 0.6982365061397632910, -0.7907169553198112322, 2.060542492664858560 ) ) ;
#72092 = CARTESIAN_POINT ( 'NONE',  ( 3.603020308667020277, 1.786206176199186535, -1.388445577547703369 ) ) ;
#72093 = CARTESIAN_POINT ( 'NONE',  ( -8.107412671292051343, 10.48173408797264194, 1.443375672974090751 ) ) ;
#72094 = CARTESIAN_POINT ( 'NONE',  ( 3.867288652163490159, -1.509380944159900428, -1.001465339209107075 ) ) ;
#72095 = CARTESIAN_POINT ( 'NONE',  ( 4.698395719694191897, 1.316562313306284038, -1.391896452211606849 ) ) ;
#72096 = CARTESIAN_POINT ( 'NONE',  ( 5.143061708805018561, -0.2499388813127951525, -2.055141626981969338 ) ) ;
#72097 = CARTESIAN_POINT ( 'NONE',  ( -1.201851678989727383E-14, 3.884375000341423689, 1.575800808251672791 ) ) ;
#72098 = CARTESIAN_POINT ( 'NONE',  ( 3.467610927914951624, 1.923740664667829225, -0.4305075535177785295 ) ) ;
#72099 = CARTESIAN_POINT ( 'NONE',  ( 1.219610691686360049, -1.880083933147856934, 0.4191893400790832613 ) ) ;
#72100 = CARTESIAN_POINT ( 'NONE',  ( 4.205816867194319464, -1.865656749788859647, 0.1373567816406878750 ) ) ;
#72101 = CARTESIAN_POINT ( 'NONE',  ( 3.422812307543467103, 1.464285610008815963, -1.783632237398341536 ) ) ;
#72102 = CARTESIAN_POINT ( 'NONE',  ( 4.263987252221818736, -1.856165113571141445, 0.1354236832897796894 ) ) ;
#72103 = CARTESIAN_POINT ( 'NONE',  ( 0.6823417656249899377, 4.176041667008085767, -1.181850606188754593 ) ) ;
#72104 = CIRCLE ( 'NONE', #30709, 0.07999999999999983513 ) ;
#72105 = CARTESIAN_POINT ( 'NONE',  ( -2.398572866711294438, 5.287202466803544887, -0.8077998227820496480 ) ) ;
#72106 = CARTESIAN_POINT ( 'NONE',  ( 2.227300950330353579, 0.0009978793536376256035, 2.106257355060832115 ) ) ;
#72107 = ADVANCED_FACE ( 'NONE', ( #145937 ), #112541, .T. ) ;
#72108 = CARTESIAN_POINT ( 'NONE',  ( 4.663641652976547647, 4.543262804668490418, 1.214306433183764966E-14 ) ) ;
#72110 = DIRECTION ( 'NONE',  ( 0.000000000000000000, -1.000000000000000000, 0.000000000000000000 ) ) ;
#72109 = CARTESIAN_POINT ( 'NONE',  ( 1.364683531249992088, 5.446875000341417916, 1.214306433183764966E-14 ) ) ;
#72111 = CARTESIAN_POINT ( 'NONE',  ( -1.872340672757990321, 8.979957301293506333, -0.7749999999999996891 ) ) ;
#72112 = CARTESIAN_POINT ( 'NONE',  ( 2.689816194747224110, 2.012238202079220439, -0.6693303307304664385 ) ) ;
#72113 = PLANE ( 'NONE',  #186146 ) ;
#72114 = CARTESIAN_POINT ( 'NONE',  ( 1.160422406460089428, 2.017671146822976880, 0.09473317391113857122 ) ) ;
#72115 = CARTESIAN_POINT ( 'NONE',  ( -0.6823417656250003738, 0.4677083336747517306, -1.181850606188749264 ) ) ;
#72116 = CARTESIAN_POINT ( 'NONE',  ( -3.633221978782304351, 4.301475732409860697, -1.082531754730549967 ) ) ;
#72117 = EDGE_CURVE ( 'NONE', #3320, #141010, #158958, .T. ) ;
#72118 = CARTESIAN_POINT ( 'NONE',  ( 4.904298879841284098, 6.744767997946721216, 1.599625672291267398 ) ) ;
#72119 = ORIENTED_EDGE ( 'NONE', *, *, #175034, .F. ) ;
#72120 = CARTESIAN_POINT ( 'NONE',  ( 1.423353863051743273, -0.05456730952056210171, 2.161080666180377197 ) ) ;
#72121 = CARTESIAN_POINT ( 'NONE',  ( 6.889999999999996128, 2.105039946316529242, 2.031469082812328519 ) ) ;
#72124 = CARTESIAN_POINT ( 'NONE',  ( 4.582292731738905722, 5.408724944192588424, -1.082531754730548412 ) ) ;
#72123 = CARTESIAN_POINT ( 'NONE',  ( 5.526144005543697446, 7.442112546579989996, -1.248357989223557452 ) ) ;
#72122 = CARTESIAN_POINT ( 'NONE',  ( 6.086684617892325733, 6.065829907154645539, -0.7998128361456481317 ) ) ;
#72125 = CARTESIAN_POINT ( 'NONE',  ( 11.97181042169640897, 9.720000000000000639, 0.8318531151397160484 ) ) ;
#72126 = CARTESIAN_POINT ( 'NONE',  ( 5.612517632836664383, 1.944729323200470095, 0.5331731267440716904 ) ) ;
#72127 = CARTESIAN_POINT ( 'NONE',  ( -9.029367117021344313, 9.636609179387466639, 0.7216878364870438212 ) ) ;
#72128 = CARTESIAN_POINT ( 'NONE',  ( 6.286679179808664308, 1.818834136932646839, -1.030939041669608924 ) ) ;
#72129 = LINE ( 'NONE', #138236, #8290 ) ;
#72131 = CARTESIAN_POINT ( 'NONE',  ( 0.6823417656249969321, 11.27604166700806765, -1.181850606188757036 ) ) ;
#72130 = CARTESIAN_POINT ( 'NONE',  ( 0.6204658552826959328, -1.213099742399858627, -1.909634413763374283 ) ) ;
#72132 = CARTESIAN_POINT ( 'NONE',  ( -7.309817376062285099, 11.67987070538135264, 0.000000000000000000 ) ) ;
#72134 = CARTESIAN_POINT ( 'NONE',  ( 1.317839660544089853, 0.9426401379578488449, -1.667518220840451981 ) ) ;
#72133 = CARTESIAN_POINT ( 'NONE',  ( -4.894130264408862452, 7.693273827576896373, -1.082531754730548412 ) ) ;
#72135 = CARTESIAN_POINT ( 'NONE',  ( -1.364683531250000748, 1.571875000341421691, 0.000000000000000000 ) ) ;
#72136 = CARTESIAN_POINT ( 'NONE',  ( 1.500000000000001332, 4.504166666666688634, 0.8660254037844450359 ) ) ;
#72137 = CARTESIAN_POINT ( 'NONE',  ( -0.7500000000000006661, 10.20833333333333393, -1.299038105676657340 ) ) ;
#72138 = CARTESIAN_POINT ( 'NONE',  ( 3.228823373612188519, 0.04322303627742052345, 1.724510841617853840 ) ) ;
#72139 = CARTESIAN_POINT ( 'NONE',  ( 4.366607992053101128, 7.252070536440704096, -1.199719254218448494 ) ) ;
#72140 = VECTOR ( 'NONE', #148252, 1000.000000000000000 ) ;
#72141 = CARTESIAN_POINT ( 'NONE',  ( 1.739140684745379195, -1.277452191371928558, -1.225025713498065549 ) ) ;
#72142 = CARTESIAN_POINT ( 'NONE',  ( 5.526482418920476647, 1.318621124876094397, -1.769340128416618363 ) ) ;
#72143 = VERTEX_POINT ( 'NONE', #91850 ) ;
#72144 = CARTESIAN_POINT ( 'NONE',  ( -5.752402313948099533, 9.933162809573264695, -0.7998128361456362523 ) ) ;
#72146 = CARTESIAN_POINT ( 'NONE',  ( 3.901970389206737444, -1.039011544341267745, -1.727992587138134306 ) ) ;
#72145 = CARTESIAN_POINT ( 'NONE',  ( 4.653055333535057514, 0.3633016933833124185, 2.088981207656291250 ) ) ;
#72148 = EDGE_LOOP ( 'NONE', ( #122525, #117156, #43600, #44159 ) ) ;
#72147 = CARTESIAN_POINT ( 'NONE',  ( 4.605596613081209156, 1.347055988495224232, 1.211539923951672648 ) ) ;
#72149 = CARTESIAN_POINT ( 'NONE',  ( 5.682802662783380754, 6.658966523782627434, 1.199719254218452935 ) ) ;
#72150 = ORIENTED_EDGE ( 'NONE', *, *, #180401, .T. ) ;
#72151 = CARTESIAN_POINT ( 'NONE',  ( 1.516246529245099284, 1.258767711876613848, -1.383943980506313398 ) ) ;
#72152 = CARTESIAN_POINT ( 'NONE',  ( 6.656878040733529289, -1.407521694628325770, 1.162499734694094844 ) ) ;
#72153 = CARTESIAN_POINT ( 'NONE',  ( 6.481129863841750272, -1.659422710288318115, -0.7269172754736009656 ) ) ;
#72154 = CARTESIAN_POINT ( 'NONE',  ( -4.762992037102518950, 4.451245552908022596, -0.7998128361456221525 ) ) ;
#72155 = CARTESIAN_POINT ( 'NONE',  ( -11.73097396203126763, 4.534521666694462105, -5.066462175338618756 ) ) ;
#72156 = CARTESIAN_POINT ( 'NONE',  ( -0.7500000000000006661, 8.739583334016129967, -1.299038105676657340 ) ) ;
#72157 = CARTESIAN_POINT ( 'NONE',  ( -1.364683531250012516, 3.051041667008083547, -0.7879004041258289570 ) ) ;
#72158 = CYLINDRICAL_SURFACE ( 'NONE', #153857, 2.250000000000000444 ) ;
#72159 = CARTESIAN_POINT ( 'NONE',  ( 7.377044979611483200, 7.779176362401098999, -0.7216878364870317197 ) ) ;
#72160 = CARTESIAN_POINT ( 'NONE',  ( -4.421367491832313590, 6.251624388594711590, 1.443375672974065660 ) ) ;
#72161 = CARTESIAN_POINT ( 'NONE',  ( -4.423703259808839938, 8.383013913077441259, 0.7998128361456352531 ) ) ;
#72162 = CARTESIAN_POINT ( 'NONE',  ( 4.412424163657523657, -2.120181911468725033, -0.04909571644767100895 ) ) ;
#72164 = CARTESIAN_POINT ( 'NONE',  ( -10.99931038725301846, 6.873658557531565627, -3.960823121322395224 ) ) ;
#72163 = CARTESIAN_POINT ( 'NONE',  ( -0.1294898018152357000, -0.0008549345193622873455, -1.926395771554180625 ) ) ;
#72165 =( BOUNDED_SURFACE ( )  B_SPLINE_SURFACE ( 1, 2, ( 
 ( #7264, #206545, #73341, #41950, #110195, #26732, #14736, #31024, #109133, #63510, #143741, #79748, #46211, #210811, #127536, #113396, #175146, #129662, #128599, #193508, #176205, #195649, #47284, #59230, #78678, #28880, #191354, #92834, #179404, #97100, #10474, #112327, #207612, #158878, #163152, #145864, #141604, #125388, #43019, #94963, #76549, #178341, #159944, #211870, #11548, #142659, #194565, #208669, #12606, #126458, #161011, #144805, #77618, #62436, #27806, #60300, #192422, #45149, #29950, #44076, #93904, #209735, #96035, #61379, #111261, #177264, #162087, #13677, #196705, #99212, #36310, #80828, #49391, #117644, #184690, #165261, #115510, #180456, #168457, #102389, #48345, #2726, #82937, #18990, #199876, #150091, #66652, #52573, #114456, #68799, #67718, #132798, #181503, #134918, #200925, #212935, #17915, #182561, #130714, #32073, #118702, #146917, #164208, #51519, #64572, #98161, #15795, #85072, #81881, #50449, #84001, #1662, #147966, #213978, #167400, #65598, #131747, #33132, #116567, #197752, #16856, #133869, #586, #166325, #198801, #34184, #100258, #149010, #151157, #183637, #35243, #101318, #107800, #135968, #22169, #55772, #69859, #206284, #56846, #3784, #188969, #86144, #201984, #152215, #185754, #154348, #40613, #90425, #119774, #39526, #24319, #156494, #121929, #155411, #57908, #71998, #53641, #37387, #88284, #103462, #70928, #169524, #204120, #8083, #105624, #203064, #170584, #38462, #187896, #123018, #171653, #21104, #87208, #153272, #4849, #137037, #120858, #54707, #186831, #104539, #5926, #138109, #23250, #20055, #89363, #6994, #73072, #139173, #205204, #106717, #74172, #172743, #140264, #124073, #190037, #41689, #78425, #28620, #178076, #127273, #47020, #27543, #93638, #43821, #112075, #173825, #159681, #109938, #174891, #42761, #45954, #211610, #126199, #76294, #11282, #194313, #128346, #60044, #79495, #175947, #108867, #62190, #25402, #92581, #29694, #91504, #125135, #191092, #207359, #63246, #94708, #145614, #157565, #160750, #208410, #144547, #77361, #9158, #129407, #141344, #177003, #75234, #26471, #12345, #95775, #143475, #193245, #209471, #61113, #195390, #58979, #210554, #158623, #10220, #44892, #142402, #192161, #110998, #161832, #13420, #82684, #148766, #66408, #132553, #146663, #68552, #133621, #163963, #100014, #162892, #67475, #32880, #198552, #179142, #131497, #17666, #101067, #199623, #16603, #97902, #166078, #15539, #196452, #212677, #49144, #51269, #1413, #65350, #14475, #130462, #2475, #117393, #167154, #183390, #200682, #64318, #48095, #114207, #150914, #33939, #18741, #30765, #83752, #147709, #149843, #115260, #96845, #84826, #80564, #116319, #113135, #180205, #34995, #134679, #181253, #50201, #98957, #335, #31827, #81624, #213727, #197501, #165008, #182310, #19812, #169278, #168213, #135727, #171412, #21922, #88031, #5672, #71750, #85899, #7826, #72831, #103218 ),
 ( #20864, #151973, #140011, #156248, #3547, #188727, #54467, #204955, #23000, #121685, #38216, #24080, #69617, #40365, #39278, #104289, #86963, #106467, #172494, #184447, #203886, #154103, #102147, #201749, #90185, #73918, #53390, #89118, #118461, #119527, #52333, #56603, #36065, #137866, #55530, #187652, #185513, #37137, #138934, #153032, #4606, #70680, #105373, #136792, #202818, #155172, #186588, #6756, #170337, #122767, #120611, #42509, #64847, #174642, #29160, #195930, #82160, #107549, #211087, #30230, #41441, #180735, #31303, #189790, #163435, #57670, #173583, #123828, #157314, #128871, #15015, #130993, #91254, #13950, #213217, #196983, #62710, #147192, #113679, #63785, #194854, #32362, #25153, #48622, #47568, #46486, #95251, #114737, #98426, #8905, #146136, #96315, #74985, #141093, #164491, #16077, #207105, #179683, #58732, #124884, #206036, #190848, #108615, #178620, #212149, #129943, #161300, #12885, #81104, #78962, #145084, #112609, #162370, #80033, #97378, #85374, #68021, #19292, #134160, #51823, #183934, #199091, #4094, #116863, #182865, #135220, #21411, #49672, #150389, #35546, #198043, #120086, #184987, #132033, #102700, #214254, #115797, #65885, #99497, #200169, #168757, #70165, #33419, #167691, #152510, #136276, #101624, #69096, #186061, #117941, #181785, #165554, #1958, #17147, #50737, #83223, #151456, #202296, #3028, #53947, #103773, #201232, #37697, #52873, #166626, #86445, #18218, #169825, #119009, #148253, #36613, #133093, #20361, #149306, #84304, #887, #34481, #66954, #100555, #73379, #189275, #153586, #157866, #89667, #190329, #204431, #23559, #5156, #122242, #108098, #203365, #105944, #43058, #87521, #56084, #124371, #191393, #171968, #188200, #187135, #175184, #109171, #55017, #155718, #206584, #156797, #91808, #40914, #71232, #7303, #139485, #205513, #25700, #137347, #57145, #123311, #88594, #170891, #174127, #125427, #39837, #107020, #173044, #9459, #41990, #24627, #207651, #90734, #22483, #75531, #121166, #6233, #141642, #38764, #104845, #154651, #72305, #138410, #8384, #59272, #74466, #140571, #58212, #145901, #28919, #92872, #146956, #208709, #29987, #26771, #27845, #13714, #195685, #95004, #46248, #177305, #144844, #212971, #60336, #211910, #126497, #64612, #112365, #192460, #143779, #142700, #110235, #63547, #210850, #62476, #194604, #178378, #44114, #196745, #47322, #77657, #79787, #76589, #113435, #161050, #96072, #158918, #45187, #129703, #14775, #179442, #128639, #11585, #31063, #209774, #176243, #93943, #12646, #97138, #163192, #193545, #159983, #61414, #130751, #80866, #48385, #127577, #78718, #111302, #162126, #114499, #10514, #197794, #98198, #148007, #180496, #214018, #82978, #33173, #149051, #165302, #81920, #115549, #132841, #32113, #16897, #50492, #84047, #116613, #182607, #19035, #68842, #15834, #17961, #199919, #65640, #131788, #49429, #34230, #150136, #181545, #2771 ) ),
 .UNSPECIFIED., .F., .F., .F. ) 
 B_SPLINE_SURFACE_WITH_KNOTS ( ( 2, 2 ),
 ( 3, 2, 2, 2, 2, 2, 2, 2, 2, 2, 2, 2, 2, 2, 2, 2, 2, 2, 2, 2, 2, 2, 2, 2, 2, 2, 2, 2, 2, 2, 2, 2, 2, 2, 2, 2, 2, 2, 2, 2, 2, 2, 2, 2, 2, 2, 2, 2, 2, 2, 2, 2, 2, 2, 2, 2, 2, 2, 2, 2, 2, 2, 2, 2, 2, 2, 2, 2, 2, 2, 2, 2, 2, 2, 2, 2, 2, 2, 2, 2, 2, 2, 2, 2, 2, 2, 2, 2, 2, 2, 2, 2, 2, 2, 2, 2, 2, 2, 2, 2, 2, 2, 2, 2, 2, 2, 2, 2, 2, 2, 2, 2, 2, 2, 2, 2, 2, 2, 2, 2, 2, 2, 2, 2, 2, 2, 2, 2, 2, 2, 2, 2, 2, 2, 2, 2, 2, 2, 2, 2, 2, 2, 2, 2, 2, 2, 2, 2, 2, 2, 2, 2, 2, 2, 2, 2, 2, 2, 2, 2, 2, 2, 2, 2, 2, 2, 2, 2, 3 ),
 ( 0.000000000000000000, 1.000000000000000000 ),
 ( 0.000000000000000000, 0.005952380952380952051, 0.01190476190476190410, 0.01785714285714285615, 0.02380952380952380820, 0.02976190476190476025, 0.03571428571428571230, 0.04166666666666666435, 0.04761904761904761640, 0.05357142857142856845, 0.05952380952380952051, 0.06547619047619047949, 0.07142857142857142461, 0.07738095238095238360, 0.08333333333333332871, 0.08928571428571428770, 0.09523809523809523281, 0.1011904761904761918, 0.1071428571428571369, 0.1130952380952380959, 0.1190476190476190410, 0.1250000000000000000, 0.1309523809523809590, 0.1369047619047619180, 0.1428571428571428492, 0.1488095238095238082, 0.1547619047619047672, 0.1607142857142857262, 0.1666666666666666574, 0.1726190476190476164, 0.1785714285714285754, 0.1845238095238095344, 0.1904761904761904656, 0.1964285714285714246, 0.2023809523809523836, 0.2083333333333333426, 0.2142857142857142738, 0.2202380952380952328, 0.2261904761904761918, 0.2321428571428571508, 0.2380952380952380820, 0.2440476190476190410, 0.2500000000000000000, 0.2559523809523809312, 0.2619047619047619180, 0.2678571428571428492, 0.2738095238095238360, 0.2797619047619047672, 0.2857142857142856984, 0.2916666666666666852, 0.2976190476190476164, 0.3035714285714285476, 0.3095238095238095344, 0.3154761904761904656, 0.3214285714285714524, 0.3273809523809523836, 0.3333333333333333148, 0.3392857142857143016, 0.3452380952380952328, 0.3511904761904761640, 0.3571428571428571508, 0.3630952380952380820, 0.3690476190476190688, 0.3750000000000000000, 0.3809523809523809312, 0.3869047619047619180, 0.3928571428571428492, 0.3988095238095238360, 0.4047619047619047672, 0.4107142857142856984, 0.4166666666666666852, 0.4226190476190476164, 0.4285714285714285476, 0.4345238095238095344, 0.4404761904761904656, 0.4464285714285714524, 0.4523809523809523836, 0.4583333333333333148, 0.4642857142857143016, 0.4702380952380952328, 0.4761904761904761640, 0.4821428571428571508, 0.4880952380952380820, 0.4940476190476190688, 0.5000000000000000000, 0.5059523809523809312, 0.5119047619047618625, 0.5178571428571429047, 0.5238095238095238360, 0.5297619047619047672, 0.5357142857142856984, 0.5416666666666666297, 0.5476190476190476719, 0.5535714285714286031, 0.5595238095238095344, 0.5654761904761904656, 0.5714285714285713969, 0.5773809523809523281, 0.5833333333333333703, 0.5892857142857143016, 0.5952380952380952328, 0.6011904761904761640, 0.6071428571428570953, 0.6130952380952381375, 0.6190476190476190688, 0.6250000000000000000, 0.6309523809523809312, 0.6369047619047618625, 0.6428571428571429047, 0.6488095238095238360, 0.6547619047619047672, 0.6607142857142856984, 0.6666666666666666297, 0.6726190476190476719, 0.6785714285714286031, 0.6845238095238095344, 0.6904761904761904656, 0.6964285714285713969, 0.7023809523809523281, 0.7083333333333333703, 0.7142857142857143016, 0.7202380952380952328, 0.7261904761904761640, 0.7321428571428570953, 0.7380952380952381375, 0.7440476190476190688, 0.7500000000000000000, 0.7559523809523809312, 0.7619047619047618625, 0.7678571428571429047, 0.7738095238095238360, 0.7797619047619047672, 0.7857142857142856984, 0.7916666666666666297, 0.7976190476190476719, 0.8035714285714286031, 0.8095238095238095344, 0.8154761904761904656, 0.8214285714285713969, 0.8273809523809523281, 0.8333333333333333703, 0.8392857142857143016, 0.8452380952380952328, 0.8511904761904761640, 0.8571428571428570953, 0.8630952380952381375, 0.8690476190476190688, 0.8750000000000000000, 0.8809523809523809312, 0.8869047619047618625, 0.8928571428571429047, 0.8988095238095238360, 0.9047619047619047672, 0.9107142857142856984, 0.9166666666666666297, 0.9226190476190476719, 0.9285714285714286031, 0.9345238095238095344, 0.9404761904761904656, 0.9464285714285713969, 0.9523809523809523281, 0.9583333333333333703, 0.9642857142857143016, 0.9702380952380952328, 0.9761904761904761640, 0.9821428571428570953, 0.9880952380952381375, 0.9940476190476190688, 1.000000000000000000 ),
 .UNSPECIFIED. ) 
 GEOMETRIC_REPRESENTATION_ITEM ( )  RATIONAL_B_SPLINE_SURFACE ( (
 ( 1.000000000000000000, 0.8660254037844387076, 1.000000000000000000, 0.8660254037844387076, 1.000000000000000000, 0.8660254037844387076, 1.000000000000000000, 0.8660254037844387076, 1.000000000000000000, 0.8660254037844387076, 1.000000000000000000, 0.8660254037844387076, 1.000000000000000000, 0.8660254037844387076, 1.000000000000000000, 0.8660254037844387076, 1.000000000000000000, 0.8660254037844387076, 1.000000000000000000, 0.8660254037844387076, 1.000000000000000000, 0.8660254037844387076, 1.000000000000000000, 0.8660254037844387076, 1.000000000000000000, 0.8660254037844387076, 1.000000000000000000, 0.8660254037844387076, 1.000000000000000000, 0.8660254037844387076, 1.000000000000000000, 0.8660254037844387076, 1.000000000000000000, 0.8660254037844387076, 1.000000000000000000, 0.8660254037844387076, 1.000000000000000000, 0.8660254037844387076, 1.000000000000000000, 0.8660254037844387076, 1.000000000000000000, 0.8660254037844387076, 1.000000000000000000, 0.8660254037844387076, 1.000000000000000000, 0.8660254037844387076, 1.000000000000000000, 0.8660254037844387076, 1.000000000000000000, 0.8660254037844387076, 1.000000000000000000, 0.8660254037844387076, 1.000000000000000000, 0.8660254037844387076, 1.000000000000000000, 0.8660254037844387076, 1.000000000000000000, 0.8660254037844387076, 1.000000000000000000, 0.8660254037844387076, 1.000000000000000000, 0.8660254037844387076, 1.000000000000000000, 0.8660254037844387076, 1.000000000000000000, 0.8660254037844387076, 1.000000000000000000, 0.8660254037844387076, 1.000000000000000000, 0.8660254037844387076, 1.000000000000000000, 0.8660254037844387076, 1.000000000000000000, 0.8660254037844387076, 1.000000000000000000, 0.8660254037844387076, 1.000000000000000000, 0.8660254037844387076, 1.000000000000000000, 0.8660254037844387076, 1.000000000000000000, 0.8660254037844387076, 1.000000000000000000, 0.8660254037844387076, 1.000000000000000000, 0.8660254037844387076, 1.000000000000000000, 0.8660254037844387076, 1.000000000000000000, 0.8660254037844387076, 1.000000000000000000, 0.8660254037844387076, 1.000000000000000000, 0.8660254037844387076, 1.000000000000000000, 0.8660254037844387076, 1.000000000000000000, 0.8660254037844387076, 1.000000000000000000, 0.8660254037844387076, 1.000000000000000000, 0.8660254037844387076, 1.000000000000000000, 0.8660254037844387076, 1.000000000000000000, 0.8660254037844387076, 1.000000000000000000, 0.8660254037844387076, 1.000000000000000000, 0.8660254037844387076, 1.000000000000000000, 0.8660254037844387076, 1.000000000000000000, 0.8660254037844387076, 1.000000000000000000, 0.8660254037844387076, 1.000000000000000000, 0.8660254037844387076, 1.000000000000000000, 0.8660254037844387076, 1.000000000000000000, 0.8660254037844387076, 1.000000000000000000, 0.8660254037844387076, 1.000000000000000000, 0.8660254037844387076, 1.000000000000000000, 0.8660254037844387076, 1.000000000000000000, 0.8660254037844387076, 1.000000000000000000, 0.8660254037844387076, 1.000000000000000000, 0.8660254037844387076, 1.000000000000000000, 0.8660254037844387076, 1.000000000000000000, 0.8660254037844387076, 1.000000000000000000, 0.8660254037844387076, 1.000000000000000000, 0.8660254037844387076, 1.000000000000000000, 0.8660254037844387076, 1.000000000000000000, 0.8660254037844387076, 1.000000000000000000, 0.8660254037844387076, 1.000000000000000000, 0.8660254037844387076, 1.000000000000000000, 0.8660254037844387076, 1.000000000000000000, 0.8660254037844387076, 1.000000000000000000, 0.8660254037844387076, 1.000000000000000000, 0.8660254037844387076, 1.000000000000000000, 0.8660254037844387076, 1.000000000000000000, 0.8660254037844387076, 1.000000000000000000, 0.8660254037844387076, 1.000000000000000000, 0.8660254037844387076, 1.000000000000000000, 0.8660254037844387076, 1.000000000000000000, 0.8660254037844387076, 1.000000000000000000, 0.8660254037844387076, 1.000000000000000000, 0.8660254037844387076, 1.000000000000000000, 0.8660254037844387076, 1.000000000000000000, 0.8660254037844387076, 1.000000000000000000, 0.8660254037844387076, 1.000000000000000000, 0.8660254037844387076, 1.000000000000000000, 0.8660254037844387076, 1.000000000000000000, 0.8660254037844387076, 1.000000000000000000, 0.8660254037844387076, 1.000000000000000000, 0.8660254037844387076, 1.000000000000000000, 0.8660254037844387076, 1.000000000000000000, 0.8660254037844387076, 1.000000000000000000, 0.8660254037844387076, 1.000000000000000000, 0.8660254037844387076, 1.000000000000000000, 0.8660254037844387076, 1.000000000000000000, 0.8660254037844387076, 1.000000000000000000, 0.8660254037844387076, 1.000000000000000000, 0.8660254037844387076, 1.000000000000000000, 0.8660254037844387076, 1.000000000000000000, 0.8660254037844387076, 1.000000000000000000, 0.8660254037844387076, 1.000000000000000000, 0.8660254037844387076, 1.000000000000000000, 0.8660254037844387076, 1.000000000000000000, 0.8660254037844387076, 1.000000000000000000, 0.8660254037844387076, 1.000000000000000000, 0.8660254037844387076, 1.000000000000000000, 0.8660254037844387076, 1.000000000000000000, 0.8660254037844387076, 1.000000000000000000, 0.8660254037844387076, 1.000000000000000000, 0.8660254037844387076, 1.000000000000000000, 0.8660254037844387076, 1.000000000000000000, 0.8660254037844387076, 1.000000000000000000, 0.8660254037844387076, 1.000000000000000000, 0.8660254037844387076, 1.000000000000000000, 0.8660254037844387076, 1.000000000000000000, 0.8660254037844387076, 1.000000000000000000, 0.8660254037844387076, 1.000000000000000000, 0.8660254037844387076, 1.000000000000000000, 0.8660254037844387076, 1.000000000000000000, 0.8660254037844387076, 1.000000000000000000, 0.8660254037844387076, 1.000000000000000000, 0.8660254037844387076, 1.000000000000000000, 0.8660254037844387076, 1.000000000000000000, 0.8660254037844387076, 1.000000000000000000, 0.8660254037844387076, 1.000000000000000000, 0.8660254037844387076, 1.000000000000000000, 0.8660254037844387076, 1.000000000000000000, 0.8660254037844387076, 1.000000000000000000, 0.8660254037844387076, 1.000000000000000000, 0.8660254037844387076, 1.000000000000000000, 0.8660254037844387076, 1.000000000000000000, 0.8660254037844387076, 1.000000000000000000, 0.8660254037844387076, 1.000000000000000000, 0.8660254037844387076, 1.000000000000000000, 0.8660254037844387076, 1.000000000000000000, 0.8660254037844387076, 1.000000000000000000, 0.8660254037844387076, 1.000000000000000000, 0.8660254037844387076, 1.000000000000000000, 0.8660254037844387076, 1.000000000000000000, 0.8660254037844387076, 1.000000000000000000, 0.8660254037844387076, 1.000000000000000000, 0.8660254037844387076, 1.000000000000000000, 0.8660254037844387076, 1.000000000000000000, 0.8660254037844387076, 1.000000000000000000, 0.8660254037844387076, 1.000000000000000000, 0.8660254037844387076, 1.000000000000000000, 0.8660254037844387076, 1.000000000000000000, 0.8660254037844387076, 1.000000000000000000, 0.8660254037844387076, 1.000000000000000000, 0.8660254037844387076, 1.000000000000000000, 0.8660254037844387076, 1.000000000000000000, 0.8660254037844387076, 1.000000000000000000, 0.8660254037844387076, 1.000000000000000000, 0.8660254037844387076, 1.000000000000000000, 0.8660254037844387076, 1.000000000000000000, 0.8660254037844387076, 1.000000000000000000, 0.8660254037844387076, 1.000000000000000000, 0.8660254037844387076, 1.000000000000000000, 0.8660254037844387076, 1.000000000000000000, 0.8660254037844387076, 1.000000000000000000, 0.8660254037844387076, 1.000000000000000000, 0.8660254037844387076, 1.000000000000000000, 0.8660254037844387076, 1.000000000000000000),
 ( 1.000000000000000000, 0.8660254037844387076, 1.000000000000000000, 0.8660254037844387076, 1.000000000000000000, 0.8660254037844387076, 1.000000000000000000, 0.8660254037844387076, 1.000000000000000000, 0.8660254037844387076, 1.000000000000000000, 0.8660254037844387076, 1.000000000000000000, 0.8660254037844387076, 1.000000000000000000, 0.8660254037844387076, 1.000000000000000000, 0.8660254037844387076, 1.000000000000000000, 0.8660254037844387076, 1.000000000000000000, 0.8660254037844387076, 1.000000000000000000, 0.8660254037844387076, 1.000000000000000000, 0.8660254037844387076, 1.000000000000000000, 0.8660254037844387076, 1.000000000000000000, 0.8660254037844387076, 1.000000000000000000, 0.8660254037844387076, 1.000000000000000000, 0.8660254037844387076, 1.000000000000000000, 0.8660254037844387076, 1.000000000000000000, 0.8660254037844387076, 1.000000000000000000, 0.8660254037844387076, 1.000000000000000000, 0.8660254037844387076, 1.000000000000000000, 0.8660254037844387076, 1.000000000000000000, 0.8660254037844387076, 1.000000000000000000, 0.8660254037844387076, 1.000000000000000000, 0.8660254037844387076, 1.000000000000000000, 0.8660254037844387076, 1.000000000000000000, 0.8660254037844387076, 1.000000000000000000, 0.8660254037844387076, 1.000000000000000000, 0.8660254037844387076, 1.000000000000000000, 0.8660254037844387076, 1.000000000000000000, 0.8660254037844387076, 1.000000000000000000, 0.8660254037844387076, 1.000000000000000000, 0.8660254037844387076, 1.000000000000000000, 0.8660254037844387076, 1.000000000000000000, 0.8660254037844387076, 1.000000000000000000, 0.8660254037844387076, 1.000000000000000000, 0.8660254037844387076, 1.000000000000000000, 0.8660254037844387076, 1.000000000000000000, 0.8660254037844387076, 1.000000000000000000, 0.8660254037844387076, 1.000000000000000000, 0.8660254037844387076, 1.000000000000000000, 0.8660254037844387076, 1.000000000000000000, 0.8660254037844387076, 1.000000000000000000, 0.8660254037844387076, 1.000000000000000000, 0.8660254037844387076, 1.000000000000000000, 0.8660254037844387076, 1.000000000000000000, 0.8660254037844387076, 1.000000000000000000, 0.8660254037844387076, 1.000000000000000000, 0.8660254037844387076, 1.000000000000000000, 0.8660254037844387076, 1.000000000000000000, 0.8660254037844387076, 1.000000000000000000, 0.8660254037844387076, 1.000000000000000000, 0.8660254037844387076, 1.000000000000000000, 0.8660254037844387076, 1.000000000000000000, 0.8660254037844387076, 1.000000000000000000, 0.8660254037844387076, 1.000000000000000000, 0.8660254037844387076, 1.000000000000000000, 0.8660254037844387076, 1.000000000000000000, 0.8660254037844387076, 1.000000000000000000, 0.8660254037844387076, 1.000000000000000000, 0.8660254037844387076, 1.000000000000000000, 0.8660254037844387076, 1.000000000000000000, 0.8660254037844387076, 1.000000000000000000, 0.8660254037844387076, 1.000000000000000000, 0.8660254037844387076, 1.000000000000000000, 0.8660254037844387076, 1.000000000000000000, 0.8660254037844387076, 1.000000000000000000, 0.8660254037844387076, 1.000000000000000000, 0.8660254037844387076, 1.000000000000000000, 0.8660254037844387076, 1.000000000000000000, 0.8660254037844387076, 1.000000000000000000, 0.8660254037844387076, 1.000000000000000000, 0.8660254037844387076, 1.000000000000000000, 0.8660254037844387076, 1.000000000000000000, 0.8660254037844387076, 1.000000000000000000, 0.8660254037844387076, 1.000000000000000000, 0.8660254037844387076, 1.000000000000000000, 0.8660254037844387076, 1.000000000000000000, 0.8660254037844387076, 1.000000000000000000, 0.8660254037844387076, 1.000000000000000000, 0.8660254037844387076, 1.000000000000000000, 0.8660254037844387076, 1.000000000000000000, 0.8660254037844387076, 1.000000000000000000, 0.8660254037844387076, 1.000000000000000000, 0.8660254037844387076, 1.000000000000000000, 0.8660254037844387076, 1.000000000000000000, 0.8660254037844387076, 1.000000000000000000, 0.8660254037844387076, 1.000000000000000000, 0.8660254037844387076, 1.000000000000000000, 0.8660254037844387076, 1.000000000000000000, 0.8660254037844387076, 1.000000000000000000, 0.8660254037844387076, 1.000000000000000000, 0.8660254037844387076, 1.000000000000000000, 0.8660254037844387076, 1.000000000000000000, 0.8660254037844387076, 1.000000000000000000, 0.8660254037844387076, 1.000000000000000000, 0.8660254037844387076, 1.000000000000000000, 0.8660254037844387076, 1.000000000000000000, 0.8660254037844387076, 1.000000000000000000, 0.8660254037844387076, 1.000000000000000000, 0.8660254037844387076, 1.000000000000000000, 0.8660254037844387076, 1.000000000000000000, 0.8660254037844387076, 1.000000000000000000, 0.8660254037844387076, 1.000000000000000000, 0.8660254037844387076, 1.000000000000000000, 0.8660254037844387076, 1.000000000000000000, 0.8660254037844387076, 1.000000000000000000, 0.8660254037844387076, 1.000000000000000000, 0.8660254037844387076, 1.000000000000000000, 0.8660254037844387076, 1.000000000000000000, 0.8660254037844387076, 1.000000000000000000, 0.8660254037844387076, 1.000000000000000000, 0.8660254037844387076, 1.000000000000000000, 0.8660254037844387076, 1.000000000000000000, 0.8660254037844387076, 1.000000000000000000, 0.8660254037844387076, 1.000000000000000000, 0.8660254037844387076, 1.000000000000000000, 0.8660254037844387076, 1.000000000000000000, 0.8660254037844387076, 1.000000000000000000, 0.8660254037844387076, 1.000000000000000000, 0.8660254037844387076, 1.000000000000000000, 0.8660254037844387076, 1.000000000000000000, 0.8660254037844387076, 1.000000000000000000, 0.8660254037844387076, 1.000000000000000000, 0.8660254037844387076, 1.000000000000000000, 0.8660254037844387076, 1.000000000000000000, 0.8660254037844387076, 1.000000000000000000, 0.8660254037844387076, 1.000000000000000000, 0.8660254037844387076, 1.000000000000000000, 0.8660254037844387076, 1.000000000000000000, 0.8660254037844387076, 1.000000000000000000, 0.8660254037844387076, 1.000000000000000000, 0.8660254037844387076, 1.000000000000000000, 0.8660254037844387076, 1.000000000000000000, 0.8660254037844387076, 1.000000000000000000, 0.8660254037844387076, 1.000000000000000000, 0.8660254037844387076, 1.000000000000000000, 0.8660254037844387076, 1.000000000000000000, 0.8660254037844387076, 1.000000000000000000, 0.8660254037844387076, 1.000000000000000000, 0.8660254037844387076, 1.000000000000000000, 0.8660254037844387076, 1.000000000000000000, 0.8660254037844387076, 1.000000000000000000, 0.8660254037844387076, 1.000000000000000000, 0.8660254037844387076, 1.000000000000000000, 0.8660254037844387076, 1.000000000000000000, 0.8660254037844387076, 1.000000000000000000, 0.8660254037844387076, 1.000000000000000000, 0.8660254037844387076, 1.000000000000000000, 0.8660254037844387076, 1.000000000000000000, 0.8660254037844387076, 1.000000000000000000, 0.8660254037844387076, 1.000000000000000000, 0.8660254037844387076, 1.000000000000000000, 0.8660254037844387076, 1.000000000000000000, 0.8660254037844387076, 1.000000000000000000, 0.8660254037844387076, 1.000000000000000000, 0.8660254037844387076, 1.000000000000000000, 0.8660254037844387076, 1.000000000000000000, 0.8660254037844387076, 1.000000000000000000, 0.8660254037844387076, 1.000000000000000000, 0.8660254037844387076, 1.000000000000000000, 0.8660254037844387076, 1.000000000000000000, 0.8660254037844387076, 1.000000000000000000, 0.8660254037844387076, 1.000000000000000000, 0.8660254037844387076, 1.000000000000000000, 0.8660254037844387076, 1.000000000000000000, 0.8660254037844387076, 1.000000000000000000, 0.8660254037844387076, 1.000000000000000000) ) ) 
 REPRESENTATION_ITEM ( '' )  SURFACE ( )  );
#72166 = CARTESIAN_POINT ( 'NONE',  ( 5.114510421747438862, 1.361449769532377729, -1.425934698893965402 ) ) ;
#72167 = CARTESIAN_POINT ( 'NONE',  ( 1.364683531249986537, 0.6135416670080880985, 0.7879004041258500513 ) ) ;
#72168 = CARTESIAN_POINT ( 'NONE',  ( 0.5100215303667603450, -0.7206480643048470691, 1.879988510241884292 ) ) ;
#72169 = ORIENTED_EDGE ( 'NONE', *, *, #165318, .F. ) ;
#72170 = CARTESIAN_POINT ( 'NONE',  ( 6.473823543489908516, -0.9023987703748233002, 1.913193491996653783 ) ) ;
#72171 = CARTESIAN_POINT ( 'NONE',  ( -0.2103062557254962439, 6.366301347167508951, -3.121735129556555854 ) ) ;
#72172 = CARTESIAN_POINT ( 'NONE',  ( 1.680221237283368696, -1.148429780529091948, -1.722445320287042447 ) ) ;
#72173 = ORIENTED_EDGE ( 'NONE', *, *, #81808, .T. ) ;
#72174 = CARTESIAN_POINT ( 'NONE',  ( 6.201928923608456046, 6.200281597156833691, 0.7998128361456352531 ) ) ;
#72175 = CARTESIAN_POINT ( 'NONE',  ( 5.550083779947807550, 7.568460058062819407, -1.599625672291283607 ) ) ;
#72177 = CARTESIAN_POINT ( 'NONE',  ( 4.168242161197552420, 6.950367390450747251, -1.199719254218452047 ) ) ;
#72176 = CARTESIAN_POINT ( 'NONE',  ( 4.857415893618338032, 2.067970888898474247, -0.3061586078061846461 ) ) ;
#72180 = ORIENTED_EDGE ( 'NONE', *, *, #121971, .T. ) ;
#72179 = CARTESIAN_POINT ( 'NONE',  ( 1.383166562764587271, 0.1333312229490003775, -1.806600723499194538 ) ) ;
#72178 = CARTESIAN_POINT ( 'NONE',  ( 2.889462524698828361, 1.289687736819044472, 1.292329967842877014 ) ) ;
#72181 = CARTESIAN_POINT ( 'NONE',  ( 9.496912337248827995, -9.201070920843591239, -0.2456386449429273644 ) ) ;
#72182 = CIRCLE ( 'NONE', #179526, 0.08000000000000020983 ) ;
#72183 = DIRECTION ( 'NONE',  ( 0.000000000000000000, 1.000000000000000000, 0.000000000000000000 ) ) ;
#72184 = CARTESIAN_POINT ( 'NONE',  ( 4.612475435721691497, -0.9401552641563456492, -1.996616816212187340 ) ) ;
#72185 = CARTESIAN_POINT ( 'NONE',  ( 0.6823417656249934904, 9.755208333674728394, 1.181850606188764807 ) ) ;
#72186 = CARTESIAN_POINT ( 'NONE',  ( 2.367698891403247519, 0.5082884949165042965, -1.843433491391050838 ) ) ;
#72187 = CARTESIAN_POINT ( 'NONE',  ( 8.718056468787178659, 10.12981962079525289, 1.199719254218462483 ) ) ;
#72188 = CARTESIAN_POINT ( 'NONE',  ( 6.443811375169310907, 1.424792453395683500, 1.502365266013883538 ) ) ;
#72189 = CARTESIAN_POINT ( 'NONE',  ( -9.361942704757863609, 15.42902520494341445, 7.422992708136421314 ) ) ;
#72190 = CARTESIAN_POINT ( 'NONE',  ( 6.005464345382193869, -2.175231771021503668, 0.2666438670960933344 ) ) ;
#72191 = CARTESIAN_POINT ( 'NONE',  ( 4.627371609795831357E-16, 2.099999999999997868, -2.600000000000008082 ) ) ;
#72192 = CARTESIAN_POINT ( 'NONE',  ( -0.9005501737259363759, 15.44694762897113627, -11.95586207050005889 ) ) ;
#72193 = ORIENTED_EDGE ( 'NONE', *, *, #168967, .F. ) ;
#72194 = ORIENTED_EDGE ( 'NONE', *, *, #29854, .T. ) ;
#72195 = CARTESIAN_POINT ( 'NONE',  ( 6.938893903907228378E-15, 10.64264068711930733, 1.214306433183764966E-14 ) ) ;
#72196 = CARTESIAN_POINT ( 'NONE',  ( 4.042156614576187579, 1.861303109871172312, 0.1859210194900539626 ) ) ;
#72197 = CARTESIAN_POINT ( 'NONE',  ( 1.001543065824772753E-15, -1.509374999522042016, 3.793834371823810780 ) ) ;
#72198 = EDGE_CURVE ( 'NONE', #45106, #96541, #208750, .T. ) ;
#72199 = CARTESIAN_POINT ( 'NONE',  ( -1.500000000000001110, 12.55208333401612819, 0.8660254037844418162 ) ) ;
#72200 = CARTESIAN_POINT ( 'NONE',  ( -7.375272376154093479, 9.627570410311676596, -1.443375672974059665 ) ) ;
#72201 = CARTESIAN_POINT ( 'NONE',  ( 5.248941747146098180, 6.152795455539095570, -1.199719254218452047 ) ) ;
#72202 = CARTESIAN_POINT ( 'NONE',  ( 6.948098034395241207, -0.8905871627266357393, 1.867117781285509537 ) ) ;
#72203 = CARTESIAN_POINT ( 'NONE',  ( 1.564077599769473803, -1.076297475396456704, 1.704952281334138675 ) ) ;
#72204 = CARTESIAN_POINT ( 'NONE',  ( -8.947491310014823895, 12.52615806407091803, 1.199719254218462483 ) ) ;
#72205 = CARTESIAN_POINT ( 'NONE',  ( 7.614839552730775729, 8.913009562054615031, 1.199719254218452047 ) ) ;
#72206 =( NAMED_UNIT ( * ) PLANE_ANGLE_UNIT ( ) SI_UNIT ( $, .RADIAN. ) );
#72207 = CARTESIAN_POINT ( 'NONE',  ( 1.113517231965298837, -2.137359700923711081, 0.4831916906855234228 ) ) ;
#72208 = CARTESIAN_POINT ( 'NONE',  ( 5.637271085457097541, -1.648663388651723460, 0.7845467231081537651 ) ) ;
#72209 = CARTESIAN_POINT ( 'NONE',  ( -4.623494077460110319, 5.352830164246910272, 1.199719254218462483 ) ) ;
#72210 = CARTESIAN_POINT ( 'NONE',  ( 6.224601922449876312, 6.434659462379210382, 0.000000000000000000 ) ) ;
#72211 = CARTESIAN_POINT ( 'NONE',  ( 9.531545685607134999, 11.07889037375188401, 1.199719254218450271 ) ) ;
#72212 = CARTESIAN_POINT ( 'NONE',  ( -5.764151584465413869, 6.753873599078290546, -1.199719254218453823 ) ) ;
#72213 = CARTESIAN_POINT ( 'NONE',  ( 5.355634372598031767, 6.206993841907870291, -1.199719254218445830 ) ) ;
#72214 = CARTESIAN_POINT ( 'NONE',  ( 5.872089928494542477, 9.864872326636710653, 0.000000000000000000 ) ) ;
#72215 = ORIENTED_EDGE ( 'NONE', *, *, #88807, .F. ) ;
#72217 = CARTESIAN_POINT ( 'NONE',  ( 6.205343618373656334, 1.749435416034326618, -0.9961562333783975376 ) ) ;
#72216 = CARTESIAN_POINT ( 'NONE',  ( 3.140019216317342376, 0.4501627324021878485, 1.785233193441162491 ) ) ;
#72218 = CARTESIAN_POINT ( 'NONE',  ( 2.372814144171823791, -0.5044604469449982531, 2.242205522996820743 ) ) ;
#72220 = CARTESIAN_POINT ( 'NONE',  ( 6.983263157960366563, -0.003091553303710344557, 1.945923119799706669 ) ) ;
#72219 = CARTESIAN_POINT ( 'NONE',  ( 3.497640442645619796, 6.064035702186436616, -1.082531754730543083 ) ) ;
#72221 = CARTESIAN_POINT ( 'NONE',  ( -6.078132937628113908, 5.985576603521232109, 1.040834085586084257E-14 ) ) ;
#72222 = CARTESIAN_POINT ( 'NONE',  ( 0.3423093779009924731, 3.000000000000002665, -0.3423093779010306092 ) ) ;
#72223 = CARTESIAN_POINT ( 'NONE',  ( 2.970861089138316036, -1.445268511421276214, 1.252435071843561731 ) ) ;
#72224 = CARTESIAN_POINT ( 'NONE',  ( -10.64723070543352712, 11.31619066596094392, 0.7998128361456462443 ) ) ;
#72225 = CARTESIAN_POINT ( 'NONE',  ( 6.080034374691865473, 7.023743017405461586, -0.9950221519831742301 ) ) ;
#72226 = CARTESIAN_POINT ( 'NONE',  ( -6.102578539926875933, 10.13377570664109051, 0.7216878364870267237 ) ) ;
#72228 = CARTESIAN_POINT ( 'NONE',  ( 0.8306673739700667358, 0.1335802410974036292, 1.865940672528036304 ) ) ;
#72227 = CARTESIAN_POINT ( 'NONE',  ( 2.314113491060950434, 1.363558105167931966, -1.585015408884550503 ) ) ;
#72229 = CARTESIAN_POINT ( 'NONE',  ( 2.302111043707856020, -1.802142186715177674, 0.9039695891032775155 ) ) ;
#72230 = CARTESIAN_POINT ( 'NONE',  ( 7.239690840017413365, 10.42976116578691403, -1.082531754730537976 ) ) ;
#72231 = CARTESIAN_POINT ( 'NONE',  ( -0.6823417656249969321, 3.530208333674754506, -1.181850606188749264 ) ) ;
#72232 = CARTESIAN_POINT ( 'NONE',  ( 3.315673178333057969, 1.101538733106369072, -1.347505558334564535 ) ) ;
#72233 = CARTESIAN_POINT ( 'NONE',  ( 4.630273154266905777, 5.360739087188218122, 1.199719254218464037 ) ) ;
#72235 = CARTESIAN_POINT ( 'NONE',  ( 0.2875577598566471660, 2.700852594506745863, -1.980716517367338891 ) ) ;
#72234 = CARTESIAN_POINT ( 'NONE',  ( -6.661184041420952440, -7.473374494058216300, 6.773376349083140013 ) ) ;
#72236 = CARTESIAN_POINT ( 'NONE',  ( 2.929983995618768322, 0.9579465210916816575, -1.434183166407378307 ) ) ;
#72237 = CARTESIAN_POINT ( 'NONE',  ( 3.298540952264991777, 1.726358142885858316, -1.349911518210664241 ) ) ;
#72238 = CARTESIAN_POINT ( 'NONE',  ( 5.514374426699260923, -0.9893691592960799364, -1.972764877262770833 ) ) ;
#72239 = CARTESIAN_POINT ( 'NONE',  ( -9.857748099689047194, 5.276144085703439401, -6.217795349555793827 ) ) ;
#72240 = CIRCLE ( 'NONE', #27263, 0.08000000000000041800 ) ;
#72241 = CARTESIAN_POINT ( 'NONE',  ( 3.432658224824499893, -1.297079494776206543, 1.740850151316934991 ) ) ;
#72242 = CARTESIAN_POINT ( 'NONE',  ( 2.578497204056416692, -1.747032809129964503, -0.5301130021647950663 ) ) ;
#72243 = CARTESIAN_POINT ( 'NONE',  ( -0.7500000000000179856, 9.322916667349467446, 1.299038105676658228 ) ) ;
#72244 = CARTESIAN_POINT ( 'NONE',  ( 4.382099326012149909, -2.116931447088743923, -0.04843129487230694169 ) ) ;
#72245 = DIRECTION ( 'NONE',  ( -0.5038915848355121074, -0.5182601445832860643, -0.6910135261110795790 ) ) ;
#72246 = EDGE_LOOP ( 'NONE', ( #61535, #94561, #109755, #50406 ) ) ;
#72248 = CARTESIAN_POINT ( 'NONE',  ( -0.6823417656250212460, 2.113541667008083991, 1.181850606188767472 ) ) ;
#72247 = CARTESIAN_POINT ( 'NONE',  ( 4.581715332782612116, -1.081557967857611935, 2.021163373060499424 ) ) ;
#72249 = CARTESIAN_POINT ( 'NONE',  ( 0.3282377607281096732, 2.573664549684620884, 1.224999999999963674 ) ) ;
#72250 = CARTESIAN_POINT ( 'NONE',  ( 4.227444969362701421, 3.826440640544909400, 1.214306433183764966E-14 ) ) ;
#72251 = CARTESIAN_POINT ( 'NONE',  ( 0.1883438084668061507, 1.224518555304452416, 1.730999496979759300 ) ) ;
#72252 = CARTESIAN_POINT ( 'NONE',  ( -6.887178846062128379, 7.137389529935019183, -0.7216878364870278340 ) ) ;
#72253 = EDGE_CURVE ( 'NONE', #65494, #24495, #149096, .T. ) ;
#72254 = CARTESIAN_POINT ( 'NONE',  ( 2.873965376416980355, 6.296784005887697155, -0.7216878364870267237 ) ) ;
#72255 = CARTESIAN_POINT ( 'NONE',  ( -6.046573321570485327, 6.156683084694754449, 0.000000000000000000 ) ) ;
#72256 = CARTESIAN_POINT ( 'NONE',  ( -9.305047017915315521, 14.48154074413197989, -7.449999999623174496 ) ) ;
#72257 = ORIENTED_EDGE ( 'NONE', *, *, #16992, .F. ) ;
#72258 = CARTESIAN_POINT ( 'NONE',  ( 5.010388774477189777, -1.913804350592800629, 0.6351971752796632398 ) ) ;
#72260 = CARTESIAN_POINT ( 'NONE',  ( 3.221586243988622034, 0.3073416805365276061, -2.039453084318449072 ) ) ;
#72259 = CARTESIAN_POINT ( 'NONE',  ( 4.310602774141044868, 7.116454772218158809, -1.199719254218452047 ) ) ;
#72262 = CARTESIAN_POINT ( 'NONE',  ( -0.1408020194050354501, 2.869306972054268989, -2.588546047063750688 ) ) ;
#72261 = CARTESIAN_POINT ( 'NONE',  ( 7.856023664475727308, 8.130058794835305136, -0.7998128361456341429 ) ) ;
#72263 = CARTESIAN_POINT ( 'NONE',  ( 7.062871678076271920, 7.204714810702593120, -0.7998128361456341429 ) ) ;
#72264 = CARTESIAN_POINT ( 'NONE',  ( 1.642778471875000035, -1.276041666188710400, -2.845375778867859751 ) ) ;
#72265 = CARTESIAN_POINT ( 'NONE',  ( 0.006800380015298257419, 7.009756401597622144, -1.999988438674496383 ) ) ;
#72266 = CARTESIAN_POINT ( 'NONE',  ( -0.02919842301645457147, -0.002306431287177941429, -2.073770398395402115 ) ) ;
#72267 = CARTESIAN_POINT ( 'NONE',  ( 3.744767666119628746, 2.000857235306313875, -0.2496062519145719194 ) ) ;
#72268 = CARTESIAN_POINT ( 'NONE',  ( 3.526749072549471453, -1.699942963128863838, 0.7078653300200200560 ) ) ;
#72269 = CARTESIAN_POINT ( 'NONE',  ( 6.979750152936881058, 7.037463354714830643, 0.7998128361456341429 ) ) ;
#72270 =( NAMED_UNIT ( * ) PLANE_ANGLE_UNIT ( ) SI_UNIT ( $, .RADIAN. ) );
#72271 = CARTESIAN_POINT ( 'NONE',  ( 0.9907087679515521605, 1.524132375323374200, -0.8073730212512005844 ) ) ;
#72272 = CARTESIAN_POINT ( 'NONE',  ( -4.437596350374534815, 4.071617251725375475, -0.7998128361456221525 ) ) ;
#72273 = CARTESIAN_POINT ( 'NONE',  ( 0.4933721672778153544, -2.286813510910344682, 0.2336738355162761571 ) ) ;
#72274 = CARTESIAN_POINT ( 'NONE',  ( -6.632963465583701534, 8.761543347979550589, -1.599625672291263179 ) ) ;
#72275 = CARTESIAN_POINT ( 'NONE',  ( 0.6150082408139592172, 1.559066714514239393, -1.639647465354547196 ) ) ;
#72276 = CARTESIAN_POINT ( 'NONE',  ( 2.561271001754578780, -1.832848164261296597, -1.037248627104673249 ) ) ;
#72277 = CARTESIAN_POINT ( 'NONE',  ( -5.088052786878465739, 9.158088361325352977, 0.000000000000000000 ) ) ;
#72278 = CARTESIAN_POINT ( 'NONE',  ( 6.425674737872927089, 9.584038729905381970, -1.199719254218440723 ) ) ;
#72279 = CARTESIAN_POINT ( 'NONE',  ( 6.495764994278809823, 7.711385593814346073, 1.082531754730549967 ) ) ;
#72280 = PRESENTATION_STYLE_ASSIGNMENT (( #157839 ) ) ;
#72281 = CARTESIAN_POINT ( 'NONE',  ( -7.576308911938196999, 7.733448573549685179, 0.7998128361456462443 ) ) ;
#72282 = EDGE_CURVE ( 'NONE', #18470, #102205, #166414, .T. ) ;
#72283 = CARTESIAN_POINT ( 'NONE',  ( 7.280365300414074703, 7.596107060012304402, -0.7216878364870257245 ) ) ;
#72284 = CARTESIAN_POINT ( 'NONE',  ( 4.161918892217930654, 7.618187422415517496, 0.8381857273355892701 ) ) ;
#72285 = CARTESIAN_POINT ( 'NONE',  ( -5.057354993097396445, 5.859001232490445688, -1.199719254218446718 ) ) ;
#72286 = CARTESIAN_POINT ( 'NONE',  ( 3.902737194376978636, -2.197594379623767580, -0.3235144178719475128 ) ) ;
#72287 = CARTESIAN_POINT ( 'NONE',  ( 2.414256260463796711, 1.430409426244143134, -1.660321623440104810 ) ) ;
#72288 = CARTESIAN_POINT ( 'NONE',  ( -6.521635583373313061, 7.567328587812373719, -1.199719254218446718 ) ) ;
#72290 = VECTOR ( 'NONE', #77691, 1000.000000000000000 ) ;
#72289 = CARTESIAN_POINT ( 'NONE',  ( -4.610654757099099221, 7.536791762327691657, 1.199719254218452935 ) ) ;
#72291 = CARTESIAN_POINT ( 'NONE',  ( 5.301206097546149465, -1.683542251207278628, 1.007010407901312465 ) ) ;
#72292 = CARTESIAN_POINT ( 'NONE',  ( -1.201851678989727383E-14, 1.321875000341419248, 1.575800808251672791 ) ) ;
#72293 = CARTESIAN_POINT ( 'NONE',  ( -3.851925040058337579, 6.547644075826416277, -1.082531754730546636 ) ) ;
#72295 = ORIENTED_EDGE ( 'NONE', *, *, #83213, .T. ) ;
#72294 = CARTESIAN_POINT ( 'NONE',  ( -5.233084105194862445, 9.049089189461916760, 0.7216878364870458196 ) ) ;
#72296 = CARTESIAN_POINT ( 'NONE',  ( 4.166350089634453191, 2.120059694336435374, -0.05518752902338577848 ) ) ;
#72297 = CARTESIAN_POINT ( 'NONE',  ( -7.024532985656169792, 9.288650798055913427, 1.443375672974064550 ) ) ;
#72298 = VERTEX_POINT ( 'NONE', #129741 ) ;
#72300 = CARTESIAN_POINT ( 'NONE',  ( 5.366167234668930419, 1.061923416652654550, 1.882811416686725359 ) ) ;
#72299 = B_SPLINE_CURVE_WITH_KNOTS ( 'NONE', 3,
 ( #145019, #87456, #19230, #182799 ),
 .UNSPECIFIED., .F., .F.,
 ( 4, 4 ),
 ( 1.127778740529212779E-17, 0.0001292189244442736897 ),
 .UNSPECIFIED. ) ;
#72301 = CARTESIAN_POINT ( 'NONE',  ( 4.645640190976921602, 8.571663989448405019, 1.040834085586084257E-14 ) ) ;
#72302 = CARTESIAN_POINT ( 'NONE',  ( 5.548353751603532835, -1.447698842669535413, 1.137588655622793876 ) ) ;
#72303 = UNCERTAINTY_MEASURE_WITH_UNIT (LENGTH_MEASURE( 1.000000000000000082E-05 ), #139680, 'distance_accuracy_value', 'NONE');
#72304 = CARTESIAN_POINT ( 'NONE',  ( -5.882246656098474524, 6.017915526194586917, -0.2943127404537674296 ) ) ;
#72305 = CARTESIAN_POINT ( 'NONE',  ( 0.6823417656249899377, 0.9052083336747520637, 1.181850606188755259 ) ) ;
#72306 = CARTESIAN_POINT ( 'NONE',  ( 0.4326491639514402077, -1.228936893156933330, -1.232681022120321934 ) ) ;
#72307 = CARTESIAN_POINT ( 'NONE',  ( 6.827182134110200806, 4.698030009824885056, 2.473619993765368008 ) ) ;
#72308 = CARTESIAN_POINT ( 'NONE',  ( 1.364683531249986537, -0.7822916663252464931, -0.7879004041258309554 ) ) ;
#72309 = FACE_OUTER_BOUND ( 'NONE', #150622, .T. ) ;
#72310 = CARTESIAN_POINT ( 'NONE',  ( 4.381803836707322652, 1.409801062080328959, 1.638821348427916602 ) ) ;
#72311 = AXIS2_PLACEMENT_3D ( 'NONE', #92176, #44479, #27131 ) ;
#72312 = CARTESIAN_POINT ( 'NONE',  ( -3.815730167242251003, 6.539103397502874948, -1.199719254218452047 ) ) ;
#72313 = CARTESIAN_POINT ( 'NONE',  ( -8.473482818416682605, 8.988077497682020578, -0.7216878364870267237 ) ) ;
#72314 = CARTESIAN_POINT ( 'NONE',  ( 3.872077330825273389, 1.198917189070296541, 1.798566189592496034 ) ) ;
#72315 = CARTESIAN_POINT ( 'NONE',  ( 4.499269426148129192, 1.581550893178500727, 1.176622024725955784 ) ) ;
#72316 = CARTESIAN_POINT ( 'NONE',  ( 3.461945267817592597, 1.365228559796902719, 1.068630620724864588 ) ) ;
#72317 = CARTESIAN_POINT ( 'NONE',  ( 0.3807642395799659130, -0.2741851280289032688, -2.174293136291181483 ) ) ;
#72318 = CARTESIAN_POINT ( 'NONE',  ( 0.8862589459083686227, 1.552251447166236975, 1.707653507296547968 ) ) ;
#72319 = CARTESIAN_POINT ( 'NONE',  ( 3.462233735546389468, 0.9232262379769129446, 1.842458217425169131 ) ) ;
#72320 = CARTESIAN_POINT ( 'NONE',  ( 6.128462272945822242, 0.1949450651400796986, 1.932269955005933904 ) ) ;
#72321 = CARTESIAN_POINT ( 'NONE',  ( -6.846504384776755714, 9.971043634672792422, -1.082531754730537088 ) ) ;
#72322 = CARTESIAN_POINT ( 'NONE',  ( -5.978219388983010418, 5.939287140093762574, -0.7998128361456362523 ) ) ;
#72323 = CARTESIAN_POINT ( 'NONE',  ( -0.7500000000000215383, 2.972916667349487341, 1.299038105676671107 ) ) ;
#72324 = ADVANCED_FACE ( 'NONE', ( #30025 ), #125473, .F. ) ;
#72326 = ORIENTED_EDGE ( 'NONE', *, *, #58887, .T. ) ;
#72325 = CARTESIAN_POINT ( 'NONE',  ( -7.147998200182420999E-13, 2.974000657017301652, -11.66643802584687251 ) ) ;
#72327 = CARTESIAN_POINT ( 'NONE',  ( -8.663296969008007054, 9.209527340038563992, 0.7216878364870438212 ) ) ;
#72328 = CARTESIAN_POINT ( 'NONE',  ( 3.540233119088306513, 0.9941544567689840628, -1.970234943098593039 ) ) ;
#72329 = CARTESIAN_POINT ( 'NONE',  ( 1.642778471875000035, -3.113541666188709200, -2.845375778867859751 ) ) ;
#72330 = VERTEX_POINT ( 'NONE', #43100 ) ;
#72331 = CARTESIAN_POINT ( 'NONE',  ( 0.4263013476871494456, -1.221759592413705908, 1.403788950402263369 ) ) ;
#72332 = CARTESIAN_POINT ( 'NONE',  ( -0.02900071798685524560, -0.004641455105012376459, -2.173770343569726649 ) ) ;
#72333 = SURFACE_STYLE_FILL_AREA ( #88622 ) ;
#72334 = LINE ( 'NONE', #74497, #30442 ) ;
#72336 = DIRECTION ( 'NONE',  ( 2.949029909160572061E-17, 1.000000000000000000, -8.673600428462353400E-15 ) ) ;
#72335 = CARTESIAN_POINT ( 'NONE',  ( -5.929989559956849732, 7.234276776666978215, -1.248630897662094563 ) ) ;
#72337 = CARTESIAN_POINT ( 'NONE',  ( 6.281194495005370193, 1.273289214079580622, 1.330099835651930684 ) ) ;
#72338 = ORIENTED_EDGE ( 'NONE', *, *, #7876, .T. ) ;
#72339 = CARTESIAN_POINT ( 'NONE',  ( 2.360294219997323140, 0.8799647281299802781, 1.863710983410723943 ) ) ;
#72340 = CARTESIAN_POINT ( 'NONE',  ( -1.360316468750009555, -0.1093749996585596795, -2.081668171172168513E-14 ) ) ;
#72341 = CARTESIAN_POINT ( 'NONE',  ( -5.343885102080728977, 9.386283052402845328, 0.7998128361456481317 ) ) ;
#72342 = CARTESIAN_POINT ( 'NONE',  ( 0.000000000000000000, 4.000000000000003553, 0.000000000000000000 ) ) ;
#72343 = COLOUR_RGB ( '', 0.40784314, 0.44705882, 0.49803922) ;
#72344 = CARTESIAN_POINT ( 'NONE',  ( 4.416205349749311004, 6.175325546172740765, 1.599625672291267398 ) ) ;
#72345 = CARTESIAN_POINT ( 'NONE',  ( 1.305620473665240366, -0.5016907458927004626, 1.998752541464960952 ) ) ;
#72346 = EDGE_CURVE ( 'NONE', #179068, #17744, #140583, .T. ) ;
#72348 = CARTESIAN_POINT ( 'NONE',  ( 4.933073973922719624, -1.305863698873997780, -1.298312775753200699 ) ) ;
#72347 = DIRECTION ( 'NONE',  ( -1.000000000000000000, 0.000000000000000000, 0.000000000000000000 ) ) ;
#72349 = CARTESIAN_POINT ( 'NONE',  ( 6.979750152936881058, 7.037463354714830643, 0.7998128361456341429 ) ) ;
#72350 = CARTESIAN_POINT ( 'NONE',  ( -5.926849427829407269, 6.943687749669614995, -1.199719254218453823 ) ) ;
#72351 = FACE_OUTER_BOUND ( 'NONE', #125636, .T. ) ;
#72352 = CARTESIAN_POINT ( 'NONE',  ( 5.004599478379411437, -0.7411955310945415043, -2.078817424605138964 ) ) ;
#72353 = CARTESIAN_POINT ( 'NONE',  ( 0.3335754702045168330, -1.976410766185803691, 0.8757516042032786885 ) ) ;
#72354 = PRESENTATION_LAYER_ASSIGNMENT (  '', '', ( #120838 ) ) ;
#72355 = CARTESIAN_POINT ( 'NONE',  ( -3.795919822146283540, 6.412028311603867436, -1.082531754730549967 ) ) ;
#72356 = CARTESIAN_POINT ( 'NONE',  ( 0.2813230411330031044, 0.1852680230450229892, -1.903361379684164412 ) ) ;
#72357 = CARTESIAN_POINT ( 'NONE',  ( 1.341030165941111241, -1.731997234073547220, -1.032477317303444053 ) ) ;
#72358 = CARTESIAN_POINT ( 'NONE',  ( -6.663994888585885512, -7.154544010627095219, 6.770610912236877610 ) ) ;
#72359 = CARTESIAN_POINT ( 'NONE',  ( 1.423680875022467873, 0.9325134783980688624, 2.100857314651356500 ) ) ;
#72360 = VECTOR ( 'NONE', #114328, 1000.000000000000227 ) ;
#72361 = FACE_OUTER_BOUND ( 'NONE', #168962, .T. ) ;
#72362 = CARTESIAN_POINT ( 'NONE',  ( 6.445967652843097362, -1.252902786447611883, -1.444740716957277904 ) ) ;
#72363 = VERTEX_POINT ( 'NONE', #44152 ) ;
#72364 = CARTESIAN_POINT ( 'NONE',  ( 1.604156678829884886, -0.6703249191640224813, -1.746612230856612769 ) ) ;
#72365 = CARTESIAN_POINT ( 'NONE',  ( 2.606657977298726614, 1.900416011228076130, 0.6748465934659984011 ) ) ;
#72367 = CARTESIAN_POINT ( 'NONE',  ( 1.337314304668908615E-15, -0.9200000000000041478, 10.91999999999999105 ) ) ;
#72366 = CARTESIAN_POINT ( 'NONE',  ( -0.6823417656250003738, 0.4677083336747517306, -1.181850606188749264 ) ) ;
#72369 = CARTESIAN_POINT ( 'NONE',  ( 5.180345272937711520, -1.170841012621581134, 1.750402278287941149 ) ) ;
#72368 = CARTESIAN_POINT ( 'NONE',  ( -9.338868881714763148, 9.789768538289042255, -0.7998128361456291469 ) ) ;
#72370 = ADVANCED_FACE ( 'NONE', ( #93981 ), #95041, .F. ) ;
#72371 = CARTESIAN_POINT ( 'NONE',  ( 6.435316467980822353, 10.65961964595298817, 1.040834085586084257E-14 ) ) ;
#72373 = CARTESIAN_POINT ( 'NONE',  ( -7.330154606482786050, 11.70359747420527619, 0.000000000000000000 ) ) ;
#72372 = CARTESIAN_POINT ( 'NONE',  ( 5.411639590510088027, 6.342609606130419131, -1.199719254218452047 ) ) ;
#72374 = FACE_OUTER_BOUND ( 'NONE', #209383, .T. ) ;
#72375 = CARTESIAN_POINT ( 'NONE',  ( 4.552993113364055766, 0.3493383367317858257, 1.989188622967730025 ) ) ;
#72376 = CARTESIAN_POINT ( 'NONE',  ( 0.6823417656249917140, 5.342708333674749177, 1.181850606188765695 ) ) ;
#72377 = EDGE_CURVE ( 'NONE', #106774, #72069, #88102, .T. ) ;
#72378 = CARTESIAN_POINT ( 'NONE',  ( 6.268047042621852860, -2.047536660891946525, 0.2488583125946699504 ) ) ;
#72379 = CARTESIAN_POINT ( 'NONE',  ( 9.734391104931955141, 10.45913716528321125, 0.7216878364870438212 ) ) ;
#72380 = CARTESIAN_POINT ( 'NONE',  ( 3.849029623751087481, -1.769594347601778361, 1.241129261558816754 ) ) ;
#72381 = CARTESIAN_POINT ( 'NONE',  ( 7.062871678076271920, 7.204714810702593120, -0.7998128361456341429 ) ) ;
#72382 = CARTESIAN_POINT ( 'NONE',  ( -1.500000000000011324, 5.879166666666686858, -0.8660254037844313801 ) ) ;
#72384 = CARTESIAN_POINT ( 'NONE',  ( 1.734723475976807094E-15, 2.499999999999998668, 0.000000000000000000 ) ) ;
#72383 = CARTESIAN_POINT ( 'NONE',  ( 4.518610335104485287, 8.493738834255713854, 0.000000000000000000 ) ) ;
#72385 = CARTESIAN_POINT ( 'NONE',  ( 6.765155463094746580, 9.876136559377135526, 1.082531754730558626 ) ) ;
#72387 = CARTESIAN_POINT ( 'NONE',  ( -0.008694310353118022902, -8.101927612791783417, 11.00038155431018261 ) ) ;
#72386 = CARTESIAN_POINT ( 'NONE',  ( 2.277988012537075502, -2.106425727361205702, 0.5258826003073436839 ) ) ;
#72389 = CARTESIAN_POINT ( 'NONE',  ( 1.469984750362408388, -1.748608032326857353, -0.5769476384821782267 ) ) ;
#72388 = CARTESIAN_POINT ( 'NONE',  ( -4.934804725694212912, 8.701096580044490381, -0.7216878364870207285 ) ) ;
#72390 = CARTESIAN_POINT ( 'NONE',  ( -1.364683531250012516, 3.280208333674756727, 0.7879004041258379498 ) ) ;
#72391 = CARTESIAN_POINT ( 'NONE',  ( 2.753686713869853531, 2.180749500395392282, -0.2175628297749406803 ) ) ;
#72392 = CARTESIAN_POINT ( 'NONE',  ( 6.983263157960365675, 2.037486384657179350, 2.358487060789053569 ) ) ;
#72393 = CARTESIAN_POINT ( 'NONE',  ( 3.960077240414155764, 2.245805352194740756, -0.2739276486512822184 ) ) ;
#72394 = CARTESIAN_POINT ( 'NONE',  ( -5.205440912643032547, 8.160432600470439723, 1.199719254218452047 ) ) ;
#72395 = DIRECTION ( 'NONE',  ( 1.000000000000000000, 0.000000000000000000, 0.000000000000000000 ) ) ;
#72396 = CARTESIAN_POINT ( 'NONE',  ( 6.483128551184942800, 6.753495492978965231, -0.1682882784904728146 ) ) ;
#72397 = CARTESIAN_POINT ( 'NONE',  ( -0.7500000000000006661, 13.45833333333333570, -1.299038105676657340 ) ) ;
#72398 = CARTESIAN_POINT ( 'NONE',  ( 6.211043768836185031, 6.418841616496599123, 0.7216878364870328300 ) ) ;
#72399 = CARTESIAN_POINT ( 'NONE',  ( 5.272599804957129876, -1.666481374185318609, -0.5959551625853221068 ) ) ;
#72400 = CARTESIAN_POINT ( 'NONE',  ( 8.229962938695207342, 9.560377169021284871, 1.199719254218462483 ) ) ;
#72401 = CARTESIAN_POINT ( 'NONE',  ( 2.063634109657853433, 0.3607628843028657939, -2.074664996798830874 ) ) ;
#72403 = CARTESIAN_POINT ( 'NONE',  ( -1.201851678989727383E-14, 0.7125000000000225597, 1.732050807568877637 ) ) ;
#72402 = CARTESIAN_POINT ( 'NONE',  ( -1.402160292154681736E-14, 10.42187500034139447, 1.575800808251682339 ) ) ;
#72404 = CARTESIAN_POINT ( 'NONE',  ( 1.187880472884972560, -1.246972491003460748, -1.524547227783664249 ) ) ;
#72405 = CARTESIAN_POINT ( 'NONE',  ( -3.688700311369816909, 6.461178242310183784, -1.199719254218450271 ) ) ;
#72406 = CARTESIAN_POINT ( 'NONE',  ( 0.3440982351944205653, -0.9282241650855774795, 1.728402704573737125 ) ) ;
#72408 = ORIENTED_EDGE ( 'NONE', *, *, #50440, .T. ) ;
#72407 = CARTESIAN_POINT ( 'NONE',  ( 6.328355405667826616, -0.8624701743435190249, -1.593140579868371987 ) ) ;
#72409 = CARTESIAN_POINT ( 'NONE',  ( 5.910991785878156435, 7.919243054989755670, -1.443375672974057666 ) ) ;
#72410 = CARTESIAN_POINT ( 'NONE',  ( 0.6823417656249882723, -0.5947916663252492686, 1.181850606188755259 ) ) ;
#72411 = CARTESIAN_POINT ( 'NONE',  ( 4.276139911362797363, -1.077190196239918851, 1.529178877381555335 ) ) ;
#72412 = ORIENTED_EDGE ( 'NONE', *, *, #211218, .T. ) ;
#72413 = CARTESIAN_POINT ( 'NONE',  ( 5.998901810315325989, 0.3981486965325408134, 2.031442706791640074 ) ) ;
#72414 = CARTESIAN_POINT ( 'NONE',  ( -3.555477883677943599E-14, 2.312499999999986677, 1.414508159514561436 ) ) ;
#72415 = CARTESIAN_POINT ( 'NONE',  ( -3.811250578772977349, 7.460559751961507224, -0.7216878364870458196 ) ) ;
#72416 = CARTESIAN_POINT ( 'NONE',  ( 3.361659061299089313, -0.9420306218829536116, 0.2814501367822265787 ) ) ;
#72417 = CARTESIAN_POINT ( 'NONE',  ( 6.089583550832340819, 10.25626457594641749, 1.040834085586084257E-14 ) ) ;
#72418 = CARTESIAN_POINT ( 'NONE',  ( -7.641992139597101108, 12.06740792950531649, 0.7998128361456481317 ) ) ;
#72419 = CARTESIAN_POINT ( 'NONE',  ( 4.518610335104485287, 8.493738834255713854, 0.000000000000000000 ) ) ;
#72420 = CARTESIAN_POINT ( 'NONE',  ( -1.364683531250014514, -0.01145833299191483488, -0.7879004041258359514 ) ) ;
#72421 = CARTESIAN_POINT ( 'NONE',  ( 0.7499999999999885647, 1.566666666666688412, -1.299038105676652899 ) ) ;
#72423 = CARTESIAN_POINT ( 'NONE',  ( 5.066996723205273057, 6.934582148538044777, 1.599625672291267398 ) ) ;
#72422 = CARTESIAN_POINT ( 'NONE',  ( 4.545333077707183200, 1.753367681936630840, -0.8802267832125689750 ) ) ;
#72424 = CARTESIAN_POINT ( 'NONE',  ( 2.354842093047845530, -0.8645933883619570937, 1.821462535208747457 ) ) ;
#72425 = CARTESIAN_POINT ( 'NONE',  ( 11.48806469435255551, 13.83089772872449075, -3.468902948106704631 ) ) ;
#72426 = CARTESIAN_POINT ( 'NONE',  ( 0.6092356648998223934, -0.3158941238240610128, 2.168550393043596536 ) ) ;
#72427 = CARTESIAN_POINT ( 'NONE',  ( -11.91826849282518630, 10.19999999999998153, 1.399999999999996581 ) ) ;
#72428 = CARTESIAN_POINT ( 'NONE',  ( 1.897508810457830153, -0.6348907881138059484, 1.759622905829677508 ) ) ;
#72429 = CARTESIAN_POINT ( 'NONE',  ( -0.6823417656249969321, 4.717708333674755394, -1.181850606188749264 ) ) ;
#72430 = CARTESIAN_POINT ( 'NONE',  ( 3.761980314931902214, 0.6741652524458006113, -1.897120442666611506 ) ) ;
#72431 = CARTESIAN_POINT ( 'NONE',  ( -8.993135964566285168, 9.386413468282476913, -0.7998128361456291469 ) ) ;
#72433 = CARTESIAN_POINT ( 'NONE',  ( 3.304427501237202414, 1.341129661294770958, -1.638326698864990716 ) ) ;
#72432 = CARTESIAN_POINT ( 'NONE',  ( -4.107757355260591936, 7.736207981205250661, 1.040834085586084257E-14 ) ) ;
#72434 = CARTESIAN_POINT ( 'NONE',  ( 0.000000000000000000, -3.600000000000005862, 6.200000000000000178 ) ) ;
#72435 = CARTESIAN_POINT ( 'NONE',  ( 4.580570967453869713, 1.276285970795057345, -1.630082184409971324 ) ) ;
#72436 = CARTESIAN_POINT ( 'NONE',  ( 4.993145711582793744, 9.047363440147082159, -0.7998128361456481317 ) ) ;
#72438 = CARTESIAN_POINT ( 'NONE',  ( 6.620655732516679493, 3.689697857139722981, 2.587825964709880910 ) ) ;
#72437 = CARTESIAN_POINT ( 'NONE',  ( 1.470382607095675143, -1.986325758040393685, -0.6527442681472686026 ) ) ;
#72440 = ORIENTED_EDGE ( 'NONE', *, *, #146351, .F. ) ;
#72439 = CARTESIAN_POINT ( 'NONE',  ( 0.1117072452763347851, -0.7311285168369995313, -1.561089762993218999 ) ) ;
#72441 = CARTESIAN_POINT ( 'NONE',  ( 6.089583550832340819, 10.25626457594641749, 1.040834085586084257E-14 ) ) ;
#72442 = CARTESIAN_POINT ( 'NONE',  ( -5.436456409399874623, 5.444880020495701523, 0.000000000000000000 ) ) ;
#72443 = CARTESIAN_POINT ( 'NONE',  ( -11.86687215968023601, 13.60942212305781851, 1.056395335932115209 ) ) ;
#72444 = TOROIDAL_SURFACE ( 'NONE', #82819, 10.92000000000000171, 0.08000000000000000167 ) ;
#72445 = CARTESIAN_POINT ( 'NONE',  ( -9.410012541129075814, 4.000000000000001776, 6.919867902370715917 ) ) ;
#72446 = CARTESIAN_POINT ( 'NONE',  ( 6.100805936025112786, 10.06143132543056673, 1.040834085586084257E-14 ) ) ;
#72447 = CARTESIAN_POINT ( 'NONE',  ( -8.012344526598182026E-15, 13.10937500034139980, -1.575800808251669460 ) ) ;
#72448 = EDGE_CURVE ( 'NONE', #95548, #81487, #176853, .T. ) ;
#72449 = CARTESIAN_POINT ( 'NONE',  ( -0.1110810684432986112, 0.002541288824218449188, -1.796853612742685513 ) ) ;
#72450 = CARTESIAN_POINT ( 'NONE',  ( -8.532158741701643123, 8.848606708273724308, 0.7998128361456462443 ) ) ;
#72451 = CARTESIAN_POINT ( 'NONE',  ( 6.491656622844908853, 6.468020902940851968, 0.7998128361456341429 ) ) ;
#72452 = CARTESIAN_POINT ( 'NONE',  ( 0.3183146091066056949, -6.808378554901781676, 10.86152993230179931 ) ) ;
#72453 = CARTESIAN_POINT ( 'NONE',  ( 2.968872451268290913, 5.447139712246216625, -1.082531754730543971 ) ) ;
#72454 = DIRECTION ( 'NONE',  ( -1.276756478318932585E-15, 1.000000000000000000, -1.665334536937738262E-16 ) ) ;
#72455 = CARTESIAN_POINT ( 'NONE',  ( 2.686486993802192913, 6.285985259411197568, 0.7998128361456362523 ) ) ;
#72456 = ORIENTED_EDGE ( 'NONE', *, *, #63234, .T. ) ;
#72457 = AXIS2_PLACEMENT_3D ( 'NONE', #70058, #6129, #203265 ) ;
#72458 = CARTESIAN_POINT ( 'NONE',  ( 6.362907676916636390, -0.1017654035869921675, -2.013986322929907757 ) ) ;
#72459 = CARTESIAN_POINT ( 'NONE',  ( -1.500000000000022204, 6.280000000000042881, 2.873333333333347728 ) ) ;
#72460 = CARTESIAN_POINT ( 'NONE',  ( 2.325000000000005063, -1.380506584136773856E-31, -3.455330625536332679E-31 ) ) ;
#72461 = PRODUCT_DEFINITION_CONTEXT ( 'detailed design', #132313, 'design' ) ;
#72462 = CARTESIAN_POINT ( 'NONE',  ( -6.501436840734760914, 6.757938919538193367, -0.04654198066046839888 ) ) ;
#72463 = CARTESIAN_POINT ( 'NONE',  ( -6.236387472606166327, 6.378132927569716060, -0.7216878364870278340 ) ) ;
#72464 = CARTESIAN_POINT ( 'NONE',  ( 8.920901888111986366, 12.39117405523060889, 1.082531754730546636 ) ) ;
#72465 = CARTESIAN_POINT ( 'NONE',  ( 3.256658344530354299, -0.5673638227334516504, -1.885978461452636479 ) ) ;
#72466 = CARTESIAN_POINT ( 'NONE',  ( 4.042592340535226647, -1.492244431823461115, 1.356313616978216618 ) ) ;
#72467 = CARTESIAN_POINT ( 'NONE',  ( -6.826694039680798021, 7.923230120171105284, -1.199719254218446718 ) ) ;
#72468 = DIRECTION ( 'NONE',  ( 0.7592566023652995710, 0.6507913734559650498, 0.000000000000000000 ) ) ;
#72469 = CARTESIAN_POINT ( 'NONE',  ( 4.488337453930180132, -0.4787454259813396229, -2.138356021698713416 ) ) ;
#72470 = DIRECTION ( 'NONE',  ( 1.000000000000000000, 0.000000000000000000, 0.000000000000000000 ) ) ;
#72471 = CARTESIAN_POINT ( 'NONE',  ( 3.346621647027960833, 0.4665833272349695360, 1.868923817322089453 ) ) ;
#72472 = CARTESIAN_POINT ( 'NONE',  ( -8.993135964566285168, 9.386413468282476913, -0.7998128361456291469 ) ) ;
#72473 = DIRECTION ( 'NONE',  ( 0.7592566023653005702, -0.6507913734559639396, 0.000000000000000000 ) ) ;
#72474 =( NAMED_UNIT ( * ) SI_UNIT ( $, .STERADIAN. ) SOLID_ANGLE_UNIT ( ) );
#72475 = CARTESIAN_POINT ( 'NONE',  ( -5.995010725448016053, 14.48115586884916439, 10.40486773299997658 ) ) ;
#72476 = CARTESIAN_POINT ( 'NONE',  ( 6.498435699651741615, 6.475929825882159818, -0.7998128361456281477 ) ) ;
#72477 = ORIENTED_EDGE ( 'NONE', *, *, #186745, .T. ) ;
#72478 = CARTESIAN_POINT ( 'NONE',  ( 4.638297949650961982, 5.544340708415133712, -1.082531754730548412 ) ) ;
#72479 = ORIENTED_EDGE ( 'NONE', *, *, #68958, .T. ) ;
#72481 = CARTESIAN_POINT ( 'NONE',  ( 2.613933768341146102, -0.6292564844058865514, 1.912298747220711359 ) ) ;
#72480 = CARTESIAN_POINT ( 'NONE',  ( -0.1294898018152357000, -0.0008549345193622873455, -1.926395771554180625 ) ) ;
#72482 = CARTESIAN_POINT ( 'NONE',  ( 5.149944687579217195, -0.2746161857135383522, -2.281865060072391760 ) ) ;
#72484 = CARTESIAN_POINT ( 'NONE',  ( 3.625696855625531345, 1.816486592755601315, -0.4036080491761192546 ) ) ;
#72483 = CARTESIAN_POINT ( 'NONE',  ( -8.106849506328558164, 8.422688943663599659, 0.000000000000000000 ) ) ;
#72485 = CARTESIAN_POINT ( 'NONE',  ( 6.003228155800906407, 10.22579295840155744, 0.000000000000000000 ) ) ;
#72486 = CARTESIAN_POINT ( 'NONE',  ( -0.4019237886467001974, 11.55133545031536713, 1.500000000000001998 ) ) ;
#72487 = CARTESIAN_POINT ( 'NONE',  ( -6.471393748265538370, 5.229711127717889596, -2.419999999999995044 ) ) ;
#72488 = CARTESIAN_POINT ( 'NONE',  ( -6.073162743917628781, 9.172774736957510555, -1.199719254218440723 ) ) ;
#72489 = CARTESIAN_POINT ( 'NONE',  ( -4.990809943606286048, 5.955604701363006015, -1.082531754730549967 ) ) ;
#72490 = CARTESIAN_POINT ( 'NONE',  ( 5.460518745505165583, -1.890641411385725501, -0.8928391682238371319 ) ) ;
#72491 = CARTESIAN_POINT ( 'NONE',  ( 4.202664430556241726, 7.846932902383524144, 0.7216878364870298324 ) ) ;
#72492 = VERTEX_POINT ( 'NONE', #148043 ) ;
#72493 = B_SPLINE_CURVE_WITH_KNOTS ( 'NONE', 3,
 ( #193593, #142756, #141696, #125486, #160035, #143831, #25751, #112416, #11638, #144892 ),
 .UNSPECIFIED., .F., .F.,
 ( 4, 3, 3, 4 ),
 ( 0.000000000000000000, 6.251591618973408526E-05, 0.0001610295297539614614, 0.0002600460447856825378 ),
 .UNSPECIFIED. ) ;
#72494 = EDGE_CURVE ( 'NONE', #51039, #56474, #65630, .T. ) ;
#72495 = DIRECTION ( 'NONE',  ( 0.8660254037844388186, 0.000000000000000000, -0.4999999999999997780 ) ) ;
#72496 = CARTESIAN_POINT ( 'NONE',  ( 4.000000000000012434, 5.999999999999998224, -1.214306433183764966E-14 ) ) ;
#72497 = CARTESIAN_POINT ( 'NONE',  ( 0.9085097582094739943, 1.384192474337717194, -1.190531929384466281 ) ) ;
#72498 = CARTESIAN_POINT ( 'NONE',  ( -4.761938266897808525, 6.578680616179308771, 1.599625672291267398 ) ) ;
#72499 = CARTESIAN_POINT ( 'NONE',  ( 2.267823513004694647, 1.585025364652093760, -0.7039959249812016706 ) ) ;
#72500 =( LENGTH_UNIT ( ) NAMED_UNIT ( * ) SI_UNIT ( .MILLI., .METRE. ) );
#72501 = DIRECTION ( 'NONE',  ( 0.000000000000000000, 0.000000000000000000, 1.000000000000000000 ) ) ;
#72502 = CARTESIAN_POINT ( 'NONE',  ( -5.018489415352746619, 9.006654751220198207, 0.7998128361456481317 ) ) ;
#72503 = DIRECTION ( 'NONE',  ( 0.7592566023652995710, -0.6507913734559651608, 8.881784197001252323E-16 ) ) ;
#72504 = CARTESIAN_POINT ( 'NONE',  ( 0.3212534483023680165, -1.847719145540312358, -0.9339786784923131968 ) ) ;
#72505 = CARTESIAN_POINT ( 'NONE',  ( 5.900976575431972293, 1.489821718068456979, -1.054992404821846863 ) ) ;
#72506 = CARTESIAN_POINT ( 'NONE',  ( 3.537899350542179189, 1.241011212050652679, 1.519374649786103149 ) ) ;
#72507 = EDGE_CURVE ( 'NONE', #157478, #71404, #76485, .T. ) ;
#72508 = CARTESIAN_POINT ( 'NONE',  ( -0.6125000000000314637, -0.8958333326505307781, 1.060881119635913583 ) ) ;
#72509 = CARTESIAN_POINT ( 'NONE',  ( -9.989660255170729641, 10.54902514065433827, -0.7998128361456291469 ) ) ;
#72510 = CARTESIAN_POINT ( 'NONE',  ( 5.601490020740366838, 9.686822124172440596, 1.040834085586084257E-14 ) ) ;
#72511 = TOROIDAL_SURFACE ( 'NONE', #103778, 0.4800000000000000933, 0.08000000000000000167 ) ;
#72512 = CARTESIAN_POINT ( 'NONE',  ( 3.563236855010095461, -1.732559338849114727, 1.222301536229251306 ) ) ;
#72513 = CARTESIAN_POINT ( 'NONE',  ( -2.982430605326328532, 5.462957558647244305, -1.082531754730543971 ) ) ;
#72514 = EDGE_CURVE ( 'NONE', #83956, #180747, #207662, .T. ) ;
#72515 = CARTESIAN_POINT ( 'NONE',  ( -8.947491310014823895, 12.52615806407091803, 1.199719254218462483 ) ) ;
#72516 = CARTESIAN_POINT ( 'NONE',  ( 1.956005403265232978, -0.7013823251572397499, 1.947930506816720087 ) ) ;
#72518 = CARTESIAN_POINT ( 'NONE',  ( 1.500000000000001332, 15.15625000068279782, 0.000000000000000000 ) ) ;
#72517 = CARTESIAN_POINT ( 'NONE',  ( -11.97302537858628213, 11.29875989808049930, 0.8111997896468087221 ) ) ;
#72520 = ORIENTED_EDGE ( 'NONE', *, *, #190705, .T. ) ;
#72519 = CARTESIAN_POINT ( 'NONE',  ( 4.424628119981884211, -0.9497243516023866627, -2.008178830631357492 ) ) ;
#72521 = CARTESIAN_POINT ( 'NONE',  ( 2.338912275282720277, 0.6088908215152682990, -2.216548965993940801 ) ) ;
#72523 = CARTESIAN_POINT ( 'NONE',  ( 6.772339297775464395, -0.9671665324481359960, -1.821725317472399963 ) ) ;
#72522 = CARTESIAN_POINT ( 'NONE',  ( 9.137832345930652522, 10.72352116074969075, -1.082531754730543083 ) ) ;
#72525 = CARTESIAN_POINT ( 'NONE',  ( -3.475000000000000533, -0.02916666666666653876, -2.006292185433948827 ) ) ;
#72524 = CARTESIAN_POINT ( 'NONE',  ( 4.553559489343365740, 6.405848385690952718, -1.599625672291269396 ) ) ;
#72526 = CYLINDRICAL_SURFACE ( 'NONE', #158181, 1.224999999999996980 ) ;
#72527 = CARTESIAN_POINT ( 'NONE',  ( 6.532758020889952277, -1.641319963461195464, 0.8346263169811756200 ) ) ;
#72528 = DIRECTION ( 'NONE',  ( 0.000000000000000000, 0.000000000000000000, -1.000000000000000000 ) ) ;
#72529 = CARTESIAN_POINT ( 'NONE',  ( 3.093911922779784440, 1.216618333484908998, 1.475457842794763996 ) ) ;
#72530 = CARTESIAN_POINT ( 'NONE',  ( -0.1102773484823937195, 1.312263477441493187, -2.452793124480449283 ) ) ;
#72531 = CARTESIAN_POINT ( 'NONE',  ( 4.594587176762323644, -0.3796550294026636574, -1.682289508650273602 ) ) ;
#72532 = CARTESIAN_POINT ( 'NONE',  ( 2.624232735793774030, 2.001858099149746550, 0.2420302859193757539 ) ) ;
#72533 = CARTESIAN_POINT ( 'NONE',  ( 3.569189921330259807, -1.132127473341357771, 2.000487910885457854 ) ) ;
#72534 = CARTESIAN_POINT ( 'NONE',  ( 3.989755448363790258, 1.635235102580555155, 1.563706588500752837 ) ) ;
#72535 = CARTESIAN_POINT ( 'NONE',  ( 6.410775461673044795, 1.561785836243877235, -1.413106494374539945 ) ) ;
#72536 = CARTESIAN_POINT ( 'NONE',  ( -5.804299160426237059, 7.865044668620976509, -1.443375672974066548 ) ) ;
#72537 = ORIENTED_EDGE ( 'NONE', *, *, #171627, .F. ) ;
#72538 = CARTESIAN_POINT ( 'NONE',  ( 4.780378767880190338, -1.716399873034094803, -0.4305553870933165883 ) ) ;
#72540 = CARTESIAN_POINT ( 'NONE',  ( 1.254322107098894801, 0.9329652568456588968, 2.093986936342966398 ) ) ;
#72539 = CARTESIAN_POINT ( 'NONE',  ( 7.388267364804250725, 7.584343111885245570, -0.7998128361456341429 ) ) ;
#72541 = CARTESIAN_POINT ( 'NONE',  ( 5.472543265827003012, -0.04911201564661467345, -1.840652735559132669 ) ) ;
#72542 = CARTESIAN_POINT ( 'NONE',  ( -4.298098390732130625, 4.973201863064262263, 1.199719254218462483 ) ) ;
#72543 = CARTESIAN_POINT ( 'NONE',  ( 5.999973295341066049, -0.7855225714627244171, -2.046000194487001878 ) ) ;
#72544 = CARTESIAN_POINT ( 'NONE',  ( -5.438755897737433287, 6.374245297895642537, -1.199719254218453823 ) ) ;
#72545 = CARTESIAN_POINT ( 'NONE',  ( -4.135400547368138113, 4.783387712472935149, 1.199719254218462483 ) ) ;
#72546 = CARTESIAN_POINT ( 'NONE',  ( -15.75000000000000000, 12.69999999999998153, 3.599999999999999201 ) ) ;
#72547 = CARTESIAN_POINT ( 'NONE',  ( 6.109843426155951107, 0.6047356833836557977, -1.980059631771100781 ) ) ;
#72548 = CARTESIAN_POINT ( 'NONE',  ( 0.4972802279516430612, -0.2910764605805628014, 1.995268990643041640 ) ) ;
#72549 =( GEOMETRIC_REPRESENTATION_CONTEXT ( 3 ) GLOBAL_UNCERTAINTY_ASSIGNED_CONTEXT ( ( #78715 ) ) GLOBAL_UNIT_ASSIGNED_CONTEXT ( ( #194570, #164213, #208674 ) ) REPRESENTATION_CONTEXT ( 'NONE', 'WORKASPACE' ) );
#72550 = CARTESIAN_POINT ( 'NONE',  ( -0.6823417656250212460, 5.301041667008086655, 1.181850606188767472 ) ) ;
#72551 = CARTESIAN_POINT ( 'NONE',  ( 4.160710321027959679, -1.426769435979913236, 1.294678423299196579 ) ) ;
#72552 = CARTESIAN_POINT ( 'NONE',  ( -8.012344526598182026E-15, 10.79687500034139624, -1.575800808251669460 ) ) ;
#72553 = CARTESIAN_POINT ( 'NONE',  ( -4.175548123328963079, 4.934189567714277302, 1.082531754730560403 ) ) ;
#72554 = CARTESIAN_POINT ( 'NONE',  ( 0.6158632564332514603, 1.820540700843051418, 1.272696253368794439 ) ) ;
#72556 = ORIENTED_EDGE ( 'NONE', *, *, #72719, .T. ) ;
#72555 = FACE_OUTER_BOUND ( 'NONE', #150767, .T. ) ;
#72558 = CARTESIAN_POINT ( 'NONE',  ( -8.002408263930261612, -6.836568542494980250, 7.346809171966449448 ) ) ;
#72557 = DIRECTION ( 'NONE',  ( -0.000000000000000000, -0.000000000000000000, -1.000000000000000000 ) ) ;
#72559 = CARTESIAN_POINT ( 'NONE',  ( 4.054051625686104998, 4.688480637177271149, -1.199719254218446718 ) ) ;
#72560 = CARTESIAN_POINT ( 'NONE',  ( -3.429849674132907200, 6.945315686556337909, -0.7216878364870036311 ) ) ;
#72561 = CARTESIAN_POINT ( 'NONE',  ( 11.89835103415199313, 11.32893085832465729, -1.561208891256347986 ) ) ;
#72562 = CARTESIAN_POINT ( 'NONE',  ( 9.904496571399500127, 11.51333640295184857, 6.696881809148281128 ) ) ;
#72563 = CARTESIAN_POINT ( 'NONE',  ( 8.880227426826630577, 12.34372051706435869, 1.082531754730546636 ) ) ;
#72564 = CARTESIAN_POINT ( 'NONE',  ( 0.9769180011504545735, 1.811320799089161993, 0.7541596914439269161 ) ) ;
#72565 = CARTESIAN_POINT ( 'NONE',  ( 0.6823417656249882723, 2.488541667008084435, -1.181850606188749264 ) ) ;
#72566 = DIRECTION ( 'NONE',  ( -1.000000000000000000, 1.224646799147347537E-16, 0.000000000000000000 ) ) ;
#72567 = CARTESIAN_POINT ( 'NONE',  ( 6.865691018405424728, -0.4312029709039078007, 1.920920986087648163 ) ) ;
#72568 = CARTESIAN_POINT ( 'NONE',  ( -7.458957065812611198, 11.85386701009007204, 0.7998128361456481317 ) ) ;
#72569 = CARTESIAN_POINT ( 'NONE',  ( -4.189106276498259618, 6.870745841681152655, 1.082531754730560403 ) ) ;
#72570 = CARTESIAN_POINT ( 'NONE',  ( 0.1282872750541429741, -1.395696511722638977, -1.781683957999291579 ) ) ;
#72572 = VERTEX_POINT ( 'NONE', #183720 ) ;
#72571 = CARTESIAN_POINT ( 'NONE',  ( -6.552668314106420588, 6.539201209412602189, -0.7998128361456291469 ) ) ;
#72573 = CARTESIAN_POINT ( 'NONE',  ( 1.364683531249990311, 5.134375000341417916, 1.214306433183764966E-14 ) ) ;
#72574 = CARTESIAN_POINT ( 'NONE',  ( 1.756895065592100291, -1.601674646019658255, -0.9660157589584242865 ) ) ;
#72575 = CARTESIAN_POINT ( 'NONE',  ( -0.1229578505166153690, -0.3670672422863025530, -1.699768244568555353 ) ) ;
#72577 = CARTESIAN_POINT ( 'NONE',  ( 4.282901435897610298, 1.957309562236182021, -0.9860176978964061423 ) ) ;
#72576 = CARTESIAN_POINT ( 'NONE',  ( 0.6801582343749952297, 1.807291667008069425, -1.178068619123869398 ) ) ;
#72578 = CARTESIAN_POINT ( 'NONE',  ( 4.876155869083551586, 1.324110019830313734, 1.889726917317616328 ) ) ;
#72579 = CARTESIAN_POINT ( 'NONE',  ( 0.2861016050247901510, -0.9718399577113141508, 1.817365962020002890 ) ) ;
#72580 = CARTESIAN_POINT ( 'NONE',  ( 1.939301023820143577, 0.7432367423349227620, -1.794281902191755540 ) ) ;
#72581 = CARTESIAN_POINT ( 'NONE',  ( -4.541618270453545492, 8.242379048930368768, 0.7216878364870458196 ) ) ;
#72582 = CARTESIAN_POINT ( 'NONE',  ( 7.334597915313080918, 9.580116872663850813, 1.040834085586084257E-14 ) ) ;
#72583 = EDGE_CURVE ( 'NONE', #61877, #76077, #162467, .T. ) ;
#72584 = CARTESIAN_POINT ( 'NONE',  ( 5.072158865288245444, 5.090142562357324429, 0.7216878364870338292 ) ) ;
#72585 = CARTESIAN_POINT ( 'NONE',  ( -10.91944002402979130, -8.407420853759269619, 0.1105873483556677611 ) ) ;
#72586 = CARTESIAN_POINT ( 'NONE',  ( 3.340470361411255418, 0.4872029778183216697, -1.956561305313428978 ) ) ;
#72587 = CARTESIAN_POINT ( 'NONE',  ( -3.592547517496929466, 7.135129837147637488, -0.7216878364870257245 ) ) ;
#72588 = CARTESIAN_POINT ( 'NONE',  ( 11.55950211276791251, 12.22000000000000064, -3.221476510067114329 ) ) ;
#72589 = CARTESIAN_POINT ( 'NONE',  ( 9.748476143425788720, 11.33197590787365172, -1.199719254218440723 ) ) ;
#72590 = CARTESIAN_POINT ( 'NONE',  ( 1.418276456094772708, 1.227529518603141190, -1.351586893430449576 ) ) ;
#72591 = CARTESIAN_POINT ( 'NONE',  ( -6.771371375382467583, 6.864631124226471037, -0.7998128361456362523 ) ) ;
#72592 = CARTESIAN_POINT ( 'NONE',  ( 11.41267819554179042, 3.447199233515649386, -3.708203932499494648 ) ) ;
#72593 = CARTESIAN_POINT ( 'NONE',  ( -10.24086661081948435, 5.004020940043352184, 7.476643068812830251 ) ) ;
#72594 = ORIENTED_EDGE ( 'NONE', *, *, #27793, .F. ) ;
#72595 = CARTESIAN_POINT ( 'NONE',  ( 5.805559403952022635, -0.5031923959765474130, 1.998377753082048347 ) ) ;
#72596 = CARTESIAN_POINT ( 'NONE',  ( -5.587368702163209910, 9.532697562583475559, 0.000000000000000000 ) ) ;
#72597 = UNCERTAINTY_MEASURE_WITH_UNIT (LENGTH_MEASURE( 1.000000000000000082E-05 ), #129868, 'distance_accuracy_value', 'NONE');
#72598 = CARTESIAN_POINT ( 'NONE',  ( 6.170369307550806148, 10.21286493553572328, 0.7216878364870317197 ) ) ;
#72599 = CARTESIAN_POINT ( 'NONE',  ( -5.278201874421821316, 5.052323696447222900, 0.7998128361456341429 ) ) ;
#72600 = CARTESIAN_POINT ( 'NONE',  ( -9.459838494033043332, 12.05956421450382088, 1.599625672291281386 ) ) ;
#72601 = CARTESIAN_POINT ( 'NONE',  ( 5.373696804382912973, 0.3918686645382524203, -1.981109099827490949 ) ) ;
#72603 = ORIENTED_EDGE ( 'NONE', *, *, #206842, .T. ) ;
#72602 = CARTESIAN_POINT ( 'NONE',  ( 5.567086426426935297, -1.752359028239593997, 1.364940763008470226 ) ) ;
#72604 = CARTESIAN_POINT ( 'NONE',  ( -6.237633190739009237, 9.434933268240943249, 1.199719254218452047 ) ) ;
#72605 = CARTESIAN_POINT ( 'NONE',  ( 6.830610463186557624, 6.863467050006115677, 1.040834085586084257E-14 ) ) ;
#72606 = CIRCLE ( 'NONE', #34411, 6.200000000000000178 ) ;
#72607 = CARTESIAN_POINT ( 'NONE',  ( 4.487218586473323612, 1.841840323776536614, -0.9247287835071598128 ) ) ;
#72608 = CARTESIAN_POINT ( 'NONE',  ( 3.744767666119628746, 2.000857235306313875, -0.2496062519145719194 ) ) ;
#72609 = VERTEX_POINT ( 'NONE', #81958 ) ;
#72610 =( BOUNDED_SURFACE ( )  B_SPLINE_SURFACE ( 1, 2, ( 
 ( #208605, #107999, #192356, #74367, #140469, #141542, #91709, #206482, #93839, #42956, #44013, #110133, #176144, #45088, #27744, #159878, #11483, #111197, #80767, #163092, #197692, #198742, #132739, #13617, #144741, #46151, #62374, #146856, #79690, #49337, #64509, #33074, #130653, #28816, #30965, #97040, #99152, #194504, #14673, #78616, #66595, #212876, #196645, #48285, #131689, #114397, #50389, #15736, #179343, #180393, #115455, #32016, #164150, #113336, #98099, #165203, #210751, #81822, #94900, #116510, #160951, #47220, #147904, #213921, #65543, #16795, #181445, #82878, #148956, #12542, #128536, #526, #112264, #178278, #29888, #95973, #162026, #145802, #211808, #63446, #129598, #195585, #3729, #166266, #22110, #19999, #88222, #18928, #4789, #136982, #104481, #200870, #51461, #52514, #36250, #154292, #119717, #183576, #17856, #117583, #83941, #133806, #71939, #35182, #185698, #87147, #2668, #1601, #120798, #70867, #150031, #101259, #153219, #151104, #5867, #34130, #85014, #168403, #184633, #102329, #203009, #170527, #182499, #103404, #138049, #167342, #53583, #68741, #134863, #118648, #86083, #54649, #67661, #152159, #186775, #69802, #135910, #169465, #201928, #204063, #21050, #37330, #38401, #55715, #100200, #199817, #155353, #92524, #174833, #8019, #121868, #39466, #75178, #76237, #41631, #105562, #189979, #90367, #206225, #208354, #26412, #6938, #93583, #175892, #74110, #109880, #27483, #205144, #158563, #25346, #59986, #171595, #156434, #73019, #58921, #107745, #91445, #141288, #106657, #23189, #172684, #139116, #173769, #89304, #124012, #157506, #57851, #207297, #10161, #9102, #56786, #122954, #125080, #191036, #42703, #108810, #188914, #159628, #142346, #11222, #24261, #126139, #192101, #43767, #140203, #40553, #77304, #143416, #209410, #187839, #78367, #193184, #12286, #110939, #94649, #81568, #144487, #30707, #80507, #45895, #176944, #48039, #64263, #28560, #210494, #146604, #112016, #15483, #127216, #128290, #145556, #161772, #13365, #196396, #180146, #61057, #212622, #65294, #178016, #96790, #95720 ),
 ( #62129, #31772, #147654, #160693, #162840, #130408, #213670, #29634, #79439, #44832, #163907, #63188, #194252, #211555, #14418, #114153, #129353, #195332, #46962, #113080, #179085, #97842, #23904, #175520, #43391, #27108, #205861, #93217, #158206, #139833, #106294, #73736, #140913, #44458, #9795, #125774, #59618, #42329, #141977, #10848, #173393, #108444, #127925, #172314, #143048, #61756, #41263, #76922, #109512, #192799, #176577, #160323, #209043, #94283, #77999, #28186, #75870, #191735, #206926, #159248, #57494, #40180, #174464, #60679, #26040, #207989, #126841, #24976, #90009, #91079, #123654, #92153, #11927, #156063, #110575, #7652, #144122, #189616, #58556, #124709, #190668, #210116, #107372, #157139, #8731, #74812, #67046, #95352, #196027, #15112, #130036, #147279, #164582, #47663, #161402, #29260, #64936, #131086, #113774, #81201, #177651, #33511, #31395, #99584, #30331, #16167, #148343, #115890, #212248, #62809, #63882, #179777, #165648, #197076, #194950, #12986, #128971, #79060, #145179, #83312, #46586, #48713, #98520, #14040, #211184, #132122, #82252, #112705, #178715, #214344, #162465, #17237, #45524, #96415, #97469, #163526, #213311, #65974, #181875, #193877, #114826, #149398, #80126, #180825, #146231, #32451, #198133, #49764, #981, #111640, #151047, #15680, #166209, #52464, #102272, #180340, #199762, #101201, #168350, #165148, #99095, #3674, #117526, #115401, #183520, #114343, #65488, #213865, #118590, #84958, #31961, #184578, #116454, #2615, #98044, #35129, #167288, #18875, #131635, #68686, #17799, #197637, #164097, #147847, #474, #36197, #83885, #51407, #133753, #182447, #81767, #49282, #181394, #19943, #134808, #33018, #86029, #34075, #200814, #16739, #152103, #69751, #135856, #82824, #201877, #149976, #148900, #66541, #132682, #198690, #50334, #1546, #100144, #67608, #55659, #155302, #24205, #186719, #121816, #141230, #119660, #156378, #75120, #54597, #90308, #122901, #206168, #189926, #173714, #7961, #107685, #91390, #41571, #23133, #139066, #154237, #205092, #70813, #53526, #187784, #137995 ) ),
 .UNSPECIFIED., .F., .F., .F. ) 
 B_SPLINE_SURFACE_WITH_KNOTS ( ( 2, 2 ),
 ( 3, 2, 2, 2, 2, 2, 2, 2, 2, 2, 2, 2, 2, 2, 2, 2, 2, 2, 2, 2, 2, 2, 2, 2, 2, 2, 2, 2, 2, 2, 2, 2, 2, 2, 2, 2, 2, 2, 2, 2, 2, 2, 2, 2, 2, 2, 2, 2, 2, 2, 2, 2, 2, 2, 2, 2, 2, 2, 2, 2, 2, 2, 2, 2, 2, 2, 2, 2, 2, 2, 2, 2, 2, 2, 2, 2, 2, 2, 2, 2, 2, 2, 2, 2, 2, 2, 2, 2, 2, 2, 2, 2, 2, 2, 2, 2, 2, 2, 2, 2, 2, 2, 2, 2, 2, 2, 2, 2, 2, 2, 2, 2, 2, 2, 2, 2, 2, 2, 2, 2, 3 ),
 ( 0.000000000000000000, 1.000000000000000000 ),
 ( 0.000000000000000000, 0.008333333333333333218, 0.01666666666666666644, 0.02500000000000000139, 0.03333333333333333287, 0.04166666666666666435, 0.05000000000000000278, 0.05833333333333333426, 0.06666666666666666574, 0.07499999999999999722, 0.08333333333333332871, 0.09166666666666666019, 0.1000000000000000056, 0.1083333333333333370, 0.1166666666666666685, 0.1250000000000000000, 0.1333333333333333315, 0.1416666666666666630, 0.1499999999999999944, 0.1583333333333333259, 0.1666666666666666574, 0.1749999999999999889, 0.1833333333333333204, 0.1916666666666666796, 0.2000000000000000111, 0.2083333333333333426, 0.2166666666666666741, 0.2250000000000000056, 0.2333333333333333370, 0.2416666666666666685, 0.2500000000000000000, 0.2583333333333333592, 0.2666666666666666630, 0.2750000000000000222, 0.2833333333333333259, 0.2916666666666666852, 0.2999999999999999889, 0.3083333333333333481, 0.3166666666666666519, 0.3250000000000000111, 0.3333333333333333148, 0.3416666666666666741, 0.3499999999999999778, 0.3583333333333333370, 0.3666666666666666408, 0.3750000000000000000, 0.3833333333333333592, 0.3916666666666666630, 0.4000000000000000222, 0.4083333333333333259, 0.4166666666666666852, 0.4249999999999999889, 0.4333333333333333481, 0.4416666666666666519, 0.4500000000000000111, 0.4583333333333333148, 0.4666666666666666741, 0.4749999999999999778, 0.4833333333333333370, 0.4916666666666666408, 0.5000000000000000000, 0.5083333333333333037, 0.5166666666666667185, 0.5250000000000000222, 0.5333333333333333259, 0.5416666666666666297, 0.5500000000000000444, 0.5583333333333333481, 0.5666666666666666519, 0.5749999999999999556, 0.5833333333333333703, 0.5916666666666666741, 0.5999999999999999778, 0.6083333333333332815, 0.6166666666666666963, 0.6250000000000000000, 0.6333333333333333037, 0.6416666666666667185, 0.6500000000000000222, 0.6583333333333333259, 0.6666666666666666297, 0.6750000000000000444, 0.6833333333333333481, 0.6916666666666666519, 0.6999999999999999556, 0.7083333333333333703, 0.7166666666666666741, 0.7249999999999999778, 0.7333333333333332815, 0.7416666666666666963, 0.7500000000000000000, 0.7583333333333333037, 0.7666666666666667185, 0.7750000000000000222, 0.7833333333333333259, 0.7916666666666666297, 0.8000000000000000444, 0.8083333333333333481, 0.8166666666666666519, 0.8249999999999999556, 0.8333333333333333703, 0.8416666666666666741, 0.8499999999999999778, 0.8583333333333332815, 0.8666666666666666963, 0.8750000000000000000, 0.8833333333333333037, 0.8916666666666667185, 0.9000000000000000222, 0.9083333333333333259, 0.9166666666666666297, 0.9250000000000000444, 0.9333333333333333481, 0.9416666666666666519, 0.9499999999999999556, 0.9583333333333333703, 0.9666666666666666741, 0.9749999999999999778, 0.9833333333333332815, 0.9916666666666666963, 1.000000000000000000 ),
 .UNSPECIFIED. ) 
 GEOMETRIC_REPRESENTATION_ITEM ( )  RATIONAL_B_SPLINE_SURFACE ( (
 ( 1.000000000000000000, 0.8660254037844387076, 1.000000000000000000, 0.8660254037844387076, 1.000000000000000000, 0.8660254037844387076, 1.000000000000000000, 0.8660254037844387076, 1.000000000000000000, 0.8660254037844387076, 1.000000000000000000, 0.8660254037844387076, 1.000000000000000000, 0.8660254037844387076, 1.000000000000000000, 0.8660254037844387076, 1.000000000000000000, 0.8660254037844387076, 1.000000000000000000, 0.8660254037844387076, 1.000000000000000000, 0.8660254037844387076, 1.000000000000000000, 0.8660254037844387076, 1.000000000000000000, 0.8660254037844387076, 1.000000000000000000, 0.8660254037844387076, 1.000000000000000000, 0.8660254037844387076, 1.000000000000000000, 0.8660254037844387076, 1.000000000000000000, 0.8660254037844387076, 1.000000000000000000, 0.8660254037844387076, 1.000000000000000000, 0.8660254037844387076, 1.000000000000000000, 0.8660254037844387076, 1.000000000000000000, 0.8660254037844387076, 1.000000000000000000, 0.8660254037844387076, 1.000000000000000000, 0.8660254037844387076, 1.000000000000000000, 0.8660254037844387076, 1.000000000000000000, 0.8660254037844387076, 1.000000000000000000, 0.8660254037844387076, 1.000000000000000000, 0.8660254037844387076, 1.000000000000000000, 0.8660254037844387076, 1.000000000000000000, 0.8660254037844387076, 1.000000000000000000, 0.8660254037844387076, 1.000000000000000000, 0.8660254037844387076, 1.000000000000000000, 0.8660254037844387076, 1.000000000000000000, 0.8660254037844387076, 1.000000000000000000, 0.8660254037844387076, 1.000000000000000000, 0.8660254037844387076, 1.000000000000000000, 0.8660254037844387076, 1.000000000000000000, 0.8660254037844387076, 1.000000000000000000, 0.8660254037844387076, 1.000000000000000000, 0.8660254037844387076, 1.000000000000000000, 0.8660254037844387076, 1.000000000000000000, 0.8660254037844387076, 1.000000000000000000, 0.8660254037844387076, 1.000000000000000000, 0.8660254037844387076, 1.000000000000000000, 0.8660254037844387076, 1.000000000000000000, 0.8660254037844387076, 1.000000000000000000, 0.8660254037844387076, 1.000000000000000000, 0.8660254037844387076, 1.000000000000000000, 0.8660254037844387076, 1.000000000000000000, 0.8660254037844387076, 1.000000000000000000, 0.8660254037844387076, 1.000000000000000000, 0.8660254037844387076, 1.000000000000000000, 0.8660254037844387076, 1.000000000000000000, 0.8660254037844387076, 1.000000000000000000, 0.8660254037844387076, 1.000000000000000000, 0.8660254037844387076, 1.000000000000000000, 0.8660254037844387076, 1.000000000000000000, 0.8660254037844387076, 1.000000000000000000, 0.8660254037844387076, 1.000000000000000000, 0.8660254037844387076, 1.000000000000000000, 0.8660254037844387076, 1.000000000000000000, 0.8660254037844387076, 1.000000000000000000, 0.8660254037844387076, 1.000000000000000000, 0.8660254037844387076, 1.000000000000000000, 0.8660254037844387076, 1.000000000000000000, 0.8660254037844387076, 1.000000000000000000, 0.8660254037844387076, 1.000000000000000000, 0.8660254037844387076, 1.000000000000000000, 0.8660254037844387076, 1.000000000000000000, 0.8660254037844387076, 1.000000000000000000, 0.8660254037844387076, 1.000000000000000000, 0.8660254037844387076, 1.000000000000000000, 0.8660254037844387076, 1.000000000000000000, 0.8660254037844387076, 1.000000000000000000, 0.8660254037844387076, 1.000000000000000000, 0.8660254037844387076, 1.000000000000000000, 0.8660254037844387076, 1.000000000000000000, 0.8660254037844387076, 1.000000000000000000, 0.8660254037844387076, 1.000000000000000000, 0.8660254037844387076, 1.000000000000000000, 0.8660254037844387076, 1.000000000000000000, 0.8660254037844387076, 1.000000000000000000, 0.8660254037844387076, 1.000000000000000000, 0.8660254037844387076, 1.000000000000000000, 0.8660254037844387076, 1.000000000000000000, 0.8660254037844387076, 1.000000000000000000, 0.8660254037844387076, 1.000000000000000000, 0.8660254037844387076, 1.000000000000000000, 0.8660254037844387076, 1.000000000000000000, 0.8660254037844387076, 1.000000000000000000, 0.8660254037844387076, 1.000000000000000000, 0.8660254037844387076, 1.000000000000000000, 0.8660254037844387076, 1.000000000000000000, 0.8660254037844387076, 1.000000000000000000, 0.8660254037844387076, 1.000000000000000000, 0.8660254037844387076, 1.000000000000000000, 0.8660254037844387076, 1.000000000000000000, 0.8660254037844387076, 1.000000000000000000, 0.8660254037844387076, 1.000000000000000000, 0.8660254037844387076, 1.000000000000000000, 0.8660254037844387076, 1.000000000000000000, 0.8660254037844387076, 1.000000000000000000, 0.8660254037844387076, 1.000000000000000000, 0.8660254037844387076, 1.000000000000000000, 0.8660254037844387076, 1.000000000000000000, 0.8660254037844387076, 1.000000000000000000, 0.8660254037844387076, 1.000000000000000000, 0.8660254037844387076, 1.000000000000000000, 0.8660254037844387076, 1.000000000000000000, 0.8660254037844387076, 1.000000000000000000, 0.8660254037844387076, 1.000000000000000000, 0.8660254037844387076, 1.000000000000000000, 0.8660254037844387076, 1.000000000000000000, 0.8660254037844387076, 1.000000000000000000, 0.8660254037844387076, 1.000000000000000000, 0.8660254037844387076, 1.000000000000000000, 0.8660254037844387076, 1.000000000000000000, 0.8660254037844387076, 1.000000000000000000, 0.8660254037844387076, 1.000000000000000000, 0.8660254037844387076, 1.000000000000000000, 0.8660254037844387076, 1.000000000000000000),
 ( 1.000000000000000000, 0.8660254037844387076, 1.000000000000000000, 0.8660254037844387076, 1.000000000000000000, 0.8660254037844387076, 1.000000000000000000, 0.8660254037844387076, 1.000000000000000000, 0.8660254037844387076, 1.000000000000000000, 0.8660254037844387076, 1.000000000000000000, 0.8660254037844387076, 1.000000000000000000, 0.8660254037844387076, 1.000000000000000000, 0.8660254037844387076, 1.000000000000000000, 0.8660254037844387076, 1.000000000000000000, 0.8660254037844387076, 1.000000000000000000, 0.8660254037844387076, 1.000000000000000000, 0.8660254037844387076, 1.000000000000000000, 0.8660254037844387076, 1.000000000000000000, 0.8660254037844387076, 1.000000000000000000, 0.8660254037844387076, 1.000000000000000000, 0.8660254037844387076, 1.000000000000000000, 0.8660254037844387076, 1.000000000000000000, 0.8660254037844387076, 1.000000000000000000, 0.8660254037844387076, 1.000000000000000000, 0.8660254037844387076, 1.000000000000000000, 0.8660254037844387076, 1.000000000000000000, 0.8660254037844387076, 1.000000000000000000, 0.8660254037844387076, 1.000000000000000000, 0.8660254037844387076, 1.000000000000000000, 0.8660254037844387076, 1.000000000000000000, 0.8660254037844387076, 1.000000000000000000, 0.8660254037844387076, 1.000000000000000000, 0.8660254037844387076, 1.000000000000000000, 0.8660254037844387076, 1.000000000000000000, 0.8660254037844387076, 1.000000000000000000, 0.8660254037844387076, 1.000000000000000000, 0.8660254037844387076, 1.000000000000000000, 0.8660254037844387076, 1.000000000000000000, 0.8660254037844387076, 1.000000000000000000, 0.8660254037844387076, 1.000000000000000000, 0.8660254037844387076, 1.000000000000000000, 0.8660254037844387076, 1.000000000000000000, 0.8660254037844387076, 1.000000000000000000, 0.8660254037844387076, 1.000000000000000000, 0.8660254037844387076, 1.000000000000000000, 0.8660254037844387076, 1.000000000000000000, 0.8660254037844387076, 1.000000000000000000, 0.8660254037844387076, 1.000000000000000000, 0.8660254037844387076, 1.000000000000000000, 0.8660254037844387076, 1.000000000000000000, 0.8660254037844387076, 1.000000000000000000, 0.8660254037844387076, 1.000000000000000000, 0.8660254037844387076, 1.000000000000000000, 0.8660254037844387076, 1.000000000000000000, 0.8660254037844387076, 1.000000000000000000, 0.8660254037844387076, 1.000000000000000000, 0.8660254037844387076, 1.000000000000000000, 0.8660254037844387076, 1.000000000000000000, 0.8660254037844387076, 1.000000000000000000, 0.8660254037844387076, 1.000000000000000000, 0.8660254037844387076, 1.000000000000000000, 0.8660254037844387076, 1.000000000000000000, 0.8660254037844387076, 1.000000000000000000, 0.8660254037844387076, 1.000000000000000000, 0.8660254037844387076, 1.000000000000000000, 0.8660254037844387076, 1.000000000000000000, 0.8660254037844387076, 1.000000000000000000, 0.8660254037844387076, 1.000000000000000000, 0.8660254037844387076, 1.000000000000000000, 0.8660254037844387076, 1.000000000000000000, 0.8660254037844387076, 1.000000000000000000, 0.8660254037844387076, 1.000000000000000000, 0.8660254037844387076, 1.000000000000000000, 0.8660254037844387076, 1.000000000000000000, 0.8660254037844387076, 1.000000000000000000, 0.8660254037844387076, 1.000000000000000000, 0.8660254037844387076, 1.000000000000000000, 0.8660254037844387076, 1.000000000000000000, 0.8660254037844387076, 1.000000000000000000, 0.8660254037844387076, 1.000000000000000000, 0.8660254037844387076, 1.000000000000000000, 0.8660254037844387076, 1.000000000000000000, 0.8660254037844387076, 1.000000000000000000, 0.8660254037844387076, 1.000000000000000000, 0.8660254037844387076, 1.000000000000000000, 0.8660254037844387076, 1.000000000000000000, 0.8660254037844387076, 1.000000000000000000, 0.8660254037844387076, 1.000000000000000000, 0.8660254037844387076, 1.000000000000000000, 0.8660254037844387076, 1.000000000000000000, 0.8660254037844387076, 1.000000000000000000, 0.8660254037844387076, 1.000000000000000000, 0.8660254037844387076, 1.000000000000000000, 0.8660254037844387076, 1.000000000000000000, 0.8660254037844387076, 1.000000000000000000, 0.8660254037844387076, 1.000000000000000000, 0.8660254037844387076, 1.000000000000000000, 0.8660254037844387076, 1.000000000000000000, 0.8660254037844387076, 1.000000000000000000, 0.8660254037844387076, 1.000000000000000000, 0.8660254037844387076, 1.000000000000000000, 0.8660254037844387076, 1.000000000000000000, 0.8660254037844387076, 1.000000000000000000, 0.8660254037844387076, 1.000000000000000000, 0.8660254037844387076, 1.000000000000000000, 0.8660254037844387076, 1.000000000000000000, 0.8660254037844387076, 1.000000000000000000, 0.8660254037844387076, 1.000000000000000000, 0.8660254037844387076, 1.000000000000000000, 0.8660254037844387076, 1.000000000000000000, 0.8660254037844387076, 1.000000000000000000, 0.8660254037844387076, 1.000000000000000000, 0.8660254037844387076, 1.000000000000000000, 0.8660254037844387076, 1.000000000000000000, 0.8660254037844387076, 1.000000000000000000, 0.8660254037844387076, 1.000000000000000000, 0.8660254037844387076, 1.000000000000000000, 0.8660254037844387076, 1.000000000000000000, 0.8660254037844387076, 1.000000000000000000, 0.8660254037844387076, 1.000000000000000000, 0.8660254037844387076, 1.000000000000000000, 0.8660254037844387076, 1.000000000000000000, 0.8660254037844387076, 1.000000000000000000, 0.8660254037844387076, 1.000000000000000000) ) ) 
 REPRESENTATION_ITEM ( '' )  SURFACE ( )  );
#72611 = CARTESIAN_POINT ( 'NONE',  ( 3.469446951953614189E-15, 5.900000000000023448, 1.214306433183764966E-14 ) ) ;
#72612 = CARTESIAN_POINT ( 'NONE',  ( 2.191614386903386613, 5.708633884695917260, -0.7998128361456281477 ) ) ;
#72614 = EDGE_LOOP ( 'NONE', ( #199952, #188334, #70043, #120916 ) ) ;
#72613 = CARTESIAN_POINT ( 'NONE',  ( -6.312203035614172286, 9.521931420595302953, -1.199719254218452047 ) ) ;
#72615 = CARTESIAN_POINT ( 'NONE',  ( 4.827426732796687325, 8.217478009653898852, -0.9130428269800896501 ) ) ;
#72616 = CARTESIAN_POINT ( 'NONE',  ( 4.516953773913958692, 2.015725170860783066, -0.04666989112152990921 ) ) ;
#72617 = CARTESIAN_POINT ( 'NONE',  ( 3.433393508698717511, 0.8267853122289525736, -1.645126075773599039 ) ) ;
#72618 = CARTESIAN_POINT ( 'NONE',  ( 6.966220764712121927, 6.002124920821316323, 2.500000000000000444 ) ) ;
#72619 = CARTESIAN_POINT ( 'NONE',  ( 1.875998176474055423, 2.207483416130914478, -0.6726682516732527262 ) ) ;
#72620 = CARTESIAN_POINT ( 'NONE',  ( 2.911969131885072670, 6.619324097166378706, 0.000000000000000000 ) ) ;
#72621 = CARTESIAN_POINT ( 'NONE',  ( 4.059979352932830743, 2.145800628424157974, -0.2601280725000321148 ) ) ;
#72622 = CARTESIAN_POINT ( 'NONE',  ( 7.072549687823125097, 11.40305840243567381, -0.7998128361456291469 ) ) ;
#72623 = CARTESIAN_POINT ( 'NONE',  ( -5.935772324684618795, 5.819489221753827657, 0.000000000000000000 ) ) ;
#72624 = VECTOR ( 'NONE', #91924, 1000.000000000000114 ) ;
#72625 = CARTESIAN_POINT ( 'NONE',  ( 3.603114471349005754, 1.037088744013005659, -2.051189238963199379 ) ) ;
#72626 = DIRECTION ( 'NONE',  ( 0.7071067811865462405, 0.000000000000000000, -0.7071067811865489050 ) ) ;
#72627 = CARTESIAN_POINT ( 'NONE',  ( 2.096370420935515178, -0.4963513585865795275, -1.803540123670114736 ) ) ;
#72628 = CARTESIAN_POINT ( 'NONE',  ( 0.5089730629182923627, 1.712948150172272976, 0.9756560103859630573 ) ) ;
#72630 = CARTESIAN_POINT ( 'NONE',  ( -6.668631453075260396, 8.873432343378178544, -1.599625672291271394 ) ) ;
#72629 = CARTESIAN_POINT ( 'NONE',  ( -1.364683531250010295, 4.280208333674753618, 0.7879004041258379498 ) ) ;
#72632 = CARTESIAN_POINT ( 'NONE',  ( 1.700138637298425737, -0.7412910010123253679, 2.078789392164873906 ) ) ;
#72631 = CARTESIAN_POINT ( 'NONE',  ( -5.575427483717760424, 7.527751369135936343, 1.599625672291269396 ) ) ;
#72633 = EDGE_CURVE ( 'NONE', #40394, #169854, #164285, .T. ) ;
#72634 = B_SPLINE_CURVE_WITH_KNOTS ( 'NONE', 3,
 ( #59059, #120950, #8174, #171744, #123106, #7086, #23341, #204210, #24403, #75317, #155504, #187987, #205295, #73158, #140352, #141433 ),
 .UNSPECIFIED., .F., .F.,
 ( 4, 3, 3, 3, 3, 4 ),
 ( 0.000000000000000000, 4.416163517948683538E-06, 1.117787330549789718E-05, 1.792356377819956129E-05, 2.465171878521282939E-05, 3.136847552908501679E-05 ),
 .UNSPECIFIED. ) ;
#72635 = DIRECTION ( 'NONE',  ( -1.000000000000000000, 0.000000000000000000, 0.000000000000000000 ) ) ;
#72636 = CARTESIAN_POINT ( 'NONE',  ( 4.008406971134620633, 7.828225232965717595, 0.7998128361456321445 ) ) ;
#72637 = CARTESIAN_POINT ( 'NONE',  ( -4.436542580169821726, 6.199052314996659874, 1.599625672291267398 ) ) ;
#72638 = CARTESIAN_POINT ( 'NONE',  ( 11.94105722165067895, 13.52582762082958823, 1.187919369849770534 ) ) ;
#72639 = CARTESIAN_POINT ( 'NONE',  ( 6.104366069677094053, -0.7090783117675543146, -1.839710284007533225 ) ) ;
#72640 = CARTESIAN_POINT ( 'NONE',  ( 5.233197408665407835, 0.1653354203888204033, 2.301840570688079790 ) ) ;
#72641 = CARTESIAN_POINT ( 'NONE',  ( 0.3440982351944205653, -0.9282241650855774795, 1.728402704573737125 ) ) ;
#72642 = EDGE_CURVE ( 'NONE', #197916, #51499, #35329, .T. ) ;
#72643 = CARTESIAN_POINT ( 'NONE',  ( 3.573143115351416377, 1.862571710426489169, 0.8863520062180642034 ) ) ;
#72644 = CARTESIAN_POINT ( 'NONE',  ( 7.185458225562760148, 8.445751353653788485, -1.082531754730543083 ) ) ;
#72645 = CARTESIAN_POINT ( 'NONE',  ( 3.061108821635398769, 6.793320401875094561, -0.7998128361456362523 ) ) ;
#72646 = CARTESIAN_POINT ( 'NONE',  ( 6.277061933002774374, 9.306694107603160404, 1.082531754730558626 ) ) ;
#72647 = CARTESIAN_POINT ( 'NONE',  ( 1.364683531249990311, 2.946875000341416140, 1.214306433183764966E-14 ) ) ;
#72648 = DIRECTION ( 'NONE',  ( -0.000000000000000000, 1.000000000000000000, 0.000000000000000000 ) ) ;
#72649 = CARTESIAN_POINT ( 'NONE',  ( 6.127922243252466039, 6.251590159990418449, 1.040834085586084257E-14 ) ) ;
#72650 = CARTESIAN_POINT ( 'NONE',  ( 5.758309058547314230, -2.171350062218261989, -0.005773456755737981470 ) ) ;
#72652 = CARTESIAN_POINT ( 'NONE',  ( 4.651808992177354440, 0.7092673950449077669, 1.699362209096597187 ) ) ;
#72651 = CARTESIAN_POINT ( 'NONE',  ( 4.991989969715272757, 4.726297878971393196, 2.500000000000011102 ) ) ;
#72653 = CARTESIAN_POINT ( 'NONE',  ( 11.80251051724250821, 12.29999999999998295, 1.695257889419128361 ) ) ;
#72654 = CARTESIAN_POINT ( 'NONE',  ( 6.550331612656306035, -1.695486744446069727, 1.388264742925699569 ) ) ;
#72655 = CARTESIAN_POINT ( 'NONE',  ( -0.3275200278800330378, 3.116672424413140963, -0.4674645318176217090 ) ) ;
#72656 = CARTESIAN_POINT ( 'NONE',  ( 0.6853298295916141480, -0.2782767918169821164, -2.245138299566074913 ) ) ;
#72657 = CARTESIAN_POINT ( 'NONE',  ( -4.661943307450316709, 7.086702294391122869, 1.392663581761391267 ) ) ;
#72658 = LINE ( 'NONE', #88940, #6332 ) ;
#72659 = CARTESIAN_POINT ( 'NONE',  ( 5.853046489161108035, 7.294594176516559614, 1.271900669079442325 ) ) ;
#72660 = CARTESIAN_POINT ( 'NONE',  ( 0.2758376730330712734, 1.891454726169951250, -0.2806862973558504892 ) ) ;
#72661 = CARTESIAN_POINT ( 'NONE',  ( 1.357869778638900904, 0.7128107867309957379, 1.620144791207811297 ) ) ;
#72662 = CARTESIAN_POINT ( 'NONE',  ( 6.270187311338969671, 2.007533000635489451, -0.1505373637035074819 ) ) ;
#72664 = CARTESIAN_POINT ( 'NONE',  ( 3.093272052591877763, -0.3707496286316728229, 1.879197483129394719 ) ) ;
#72663 = CARTESIAN_POINT ( 'NONE',  ( -8.479735010343349089, 11.98044238112085758, 1.199719254218453823 ) ) ;
#72665 = CARTESIAN_POINT ( 'NONE',  ( -0.1409997244346088141, 2.874455162768466909, -2.488748179275114492 ) ) ;
#72666 = CARTESIAN_POINT ( 'NONE',  ( 4.070725410728625704, 1.394476139410082638, -1.391156265790331581 ) ) ;
#72667 = CARTESIAN_POINT ( 'NONE',  ( -0.1401555495076401980, -1.643345231473653190, -1.339971704266910812 ) ) ;
#72668 = CARTESIAN_POINT ( 'NONE',  ( -3.379006598303881059, 4.965260336153046516, -1.599625672291256295 ) ) ;
#72669 = CARTESIAN_POINT ( 'NONE',  ( 2.658895327995167701, -1.626580691111865207, -0.9237732865615968514 ) ) ;
#72671 = EDGE_LOOP ( 'NONE', ( #138088, #78118, #158228, #130207, #62359, #10360, #156964, #203310, #47790, #206464, #88051, #128091, #74837, #145846, #66295, #190726, #213871, #52687, #76530, #91422, #163727, #77123, #170293, #174810 ) ) ;
#72670 = CARTESIAN_POINT ( 'NONE',  ( 6.551377187490000864, -1.390289022577213984, -1.020726160236499203 ) ) ;
#72672 = EDGE_CURVE ( 'NONE', #98551, #8852, #90416, .T. ) ;
#72674 = CARTESIAN_POINT ( 'NONE',  ( 3.714570900464278846, 5.356752022006865843, 1.443375672974062551 ) ) ;
#72673 = CARTESIAN_POINT ( 'NONE',  ( 2.385638622766753425, 2.017150886971270651, -0.8956362484653990208 ) ) ;
#72675 = AXIS2_PLACEMENT_3D ( 'NONE', #177195, #61306, #158812 ) ;
#72676 = CARTESIAN_POINT ( 'NONE',  ( 1.364683531249988535, 3.967708333674751842, -0.7879004041258239610 ) ) ;
#72677 = CARTESIAN_POINT ( 'NONE',  ( 6.883263157960391787, -0.001104538646235289417, 1.946037152736757925 ) ) ;
#72678 = CARTESIAN_POINT ( 'NONE',  ( 8.776205506747620788, 9.133327934160710981, -0.7998128361456221525 ) ) ;
#72679 = CARTESIAN_POINT ( 'NONE',  ( -8.482597663644387609, 13.04811437422715414, -0.7998128361456281477 ) ) ;
#72680 = CARTESIAN_POINT ( 'NONE',  ( 0.09280742163705514580, -9.178267117872108471, -9.499822780340156925 ) ) ;
#72681 = CARTESIAN_POINT ( 'NONE',  ( 0.1747926744264677312, 1.388892567315727744, -2.112808070315982167 ) ) ;
#72682 = EDGE_CURVE ( 'NONE', #53161, #22926, #26576, .T. ) ;
#72683 = CARTESIAN_POINT ( 'NONE',  ( -7.834948825496938163, -6.134628647623485698, -7.720982897393567690 ) ) ;
#72684 = ORIENTED_EDGE ( 'NONE', *, *, #4041, .T. ) ;
#72685 = CARTESIAN_POINT ( 'NONE',  ( 3.666520218671379450, -0.8364210039109070127, -1.894060025281426807 ) ) ;
#72686 = CARTESIAN_POINT ( 'NONE',  ( 1.499999999999987121, 3.545833333333356041, -0.8660254037844262731 ) ) ;
#72687 = CARTESIAN_POINT ( 'NONE',  ( 4.310602774141044868, 7.116454772218158809, -1.199719254218452047 ) ) ;
#72688 = CARTESIAN_POINT ( 'NONE',  ( -6.382290003970109815, 6.834844811514095397, -0.5765442458998057962 ) ) ;
#72689 = CARTESIAN_POINT ( 'NONE',  ( 0.7154971248738207779, 1.652399868344236245, 1.161036454668294304 ) ) ;
#72690 = CARTESIAN_POINT ( 'NONE',  ( -1.123270288250343141, 2.846052654332832610, 0.7749999999993751887 ) ) ;
#72691 = CARTESIAN_POINT ( 'NONE',  ( -1.364683531249997417, 3.759375000341423689, 1.214306433183764966E-14 ) ) ;
#72693 = CARTESIAN_POINT ( 'NONE',  ( 8.215877900201359552, 11.56864606933486606, -1.082531754730543083 ) ) ;
#72692 = CARTESIAN_POINT ( 'NONE',  ( 0.1745949693968328054, 4.098633874596197657, -2.310325329485760637 ) ) ;
#72694 = CARTESIAN_POINT ( 'NONE',  ( 5.940779784064256219, 1.198679029392090589, 1.620932600025201786 ) ) ;
#72695 = CARTESIAN_POINT ( 'NONE',  ( 5.928903634556547786, -1.614502157299831042, 1.030912532684091110 ) ) ;
#72696 = CARTESIAN_POINT ( 'NONE',  ( 6.539320575229260690, 0.5855366995804256458, 2.057005297509428399 ) ) ;
#72697 = CARTESIAN_POINT ( 'NONE',  ( 3.948915171154475878, -1.822730400009948237, -1.216494452853926322 ) ) ;
#72698 = CARTESIAN_POINT ( 'NONE',  ( -1.500000000000001332, 1.431250000682816825, 0.000000000000000000 ) ) ;
#72699 = CARTESIAN_POINT ( 'NONE',  ( 2.830216799141628492, -0.9462872844297947061, -1.661813493071498726 ) ) ;
#72700 = CARTESIAN_POINT ( 'NONE',  ( -5.473741331615264549, 7.409117525016355010, -1.599625672291256295 ) ) ;
#72701 = CARTESIAN_POINT ( 'NONE',  ( 5.192409643909512873, 6.120528008391641350, -1.082531754730549078 ) ) ;
#72703 = CARTESIAN_POINT ( 'NONE',  ( 1.265250157614560278, 1.862010354082012098, -0.7743342583275418800 ) ) ;
#72702 = CARTESIAN_POINT ( 'NONE',  ( 1.836970198721030181E-16, 5.999999999999998224, 1.500000000000000222 ) ) ;
#72704 = CARTESIAN_POINT ( 'NONE',  ( -0.6823417656250039265, 10.63020833367472839, -1.181850606188755259 ) ) ;
#72706 = CARTESIAN_POINT ( 'NONE',  ( -5.281783360975562225, 8.319775133516907673, 1.199719254218452935 ) ) ;
#72705 = CARTESIAN_POINT ( 'NONE',  ( 5.812113132715003516, 1.472855484078567700, -1.623034594306454137 ) ) ;
#72708 = ORIENTED_EDGE ( 'NONE', *, *, #135923, .T. ) ;
#72707 = CARTESIAN_POINT ( 'NONE',  ( 2.819059531128511598, -0.1711090930666993304, 1.716262065957876004 ) ) ;
#72709 = CARTESIAN_POINT ( 'NONE',  ( 6.029554895997981667, -0.2579198037528374066, 2.104758538420265168 ) ) ;
#72710 = CARTESIAN_POINT ( 'NONE',  ( 8.121497709785879593, 9.433834401960398353, -1.199719254218445830 ) ) ;
#72711 = CARTESIAN_POINT ( 'NONE',  ( 5.066996723205273057, 6.934582148538044777, 1.599625672291267398 ) ) ;
#72712 =( NAMED_UNIT ( * ) PLANE_ANGLE_UNIT ( ) SI_UNIT ( $, .RADIAN. ) );
#72713 = CARTESIAN_POINT ( 'NONE',  ( 0.5198770262540284293, 1.941052373433370448, -0.2841105942011297736 ) ) ;
#72714 = CARTESIAN_POINT ( 'NONE',  ( 7.055228938193936372, -8.176568542494910830, -6.396834479292718534 ) ) ;
#72715 = CARTESIAN_POINT ( 'NONE',  ( 5.307127064745490230, 8.279066444590018392, -1.199719254218452935 ) ) ;
#72716 = DIRECTION ( 'NONE',  ( 0.000000000000000000, 1.000000000000000000, 0.000000000000000000 ) ) ;
#72717 = FACE_OUTER_BOUND ( 'NONE', #189445, .T. ) ;
#72718 =( GEOMETRIC_REPRESENTATION_CONTEXT ( 3 ) GLOBAL_UNCERTAINTY_ASSIGNED_CONTEXT ( ( #102330 ) ) GLOBAL_UNIT_ASSIGNED_CONTEXT ( ( #77369, #160759, #26479 ) ) REPRESENTATION_CONTEXT ( 'NONE', 'WORKASPACE' ) );
#72719 = EDGE_CURVE ( 'NONE', #95923, #210733, #131883, .T. ) ;
#72720 = ORIENTED_EDGE ( 'NONE', *, *, #120570, .T. ) ;
#72721 = CARTESIAN_POINT ( 'NONE',  ( 2.525776224529495906, -1.791516492901791713, 0.2672755921442840354 ) ) ;
#72722 = ORIENTED_EDGE ( 'NONE', *, *, #130589, .F. ) ;
#72723 = CARTESIAN_POINT ( 'NONE',  ( 7.892817981449907982, 12.36003807833360391, 0.7998128361456462443 ) ) ;
#72724 = CARTESIAN_POINT ( 'NONE',  ( 4.655245641445829641, 6.524482229810530498, 1.599625672291269396 ) ) ;
#72725 = CARTESIAN_POINT ( 'NONE',  ( 3.615680081246709143, -0.5227945197113766929, 1.734396599632443525 ) ) ;
#72726 = CARTESIAN_POINT ( 'NONE',  ( 0.4339943706424725378, 3.713305424705313218, 0.4851827343914862922 ) ) ;
#72727 = CARTESIAN_POINT ( 'NONE',  ( 0.1007670162816190901, -8.052608368926284399, 9.499791922504430275 ) ) ;
#72728 = CARTESIAN_POINT ( 'NONE',  ( 5.181774431428755712, 6.445567486282277159, 1.182616053296376979 ) ) ;
#72730 = CARTESIAN_POINT ( 'NONE',  ( -1.364683531250000748, 14.85937500034140157, 0.000000000000000000 ) ) ;
#72729 = CARTESIAN_POINT ( 'NONE',  ( 5.582414374887135544, 1.108435676577405937, -1.494769603722338802 ) ) ;
#72731 = CARTESIAN_POINT ( 'NONE',  ( 2.829585337313187399, 0.6869450147981278620, -1.788391637942953860 ) ) ;
#72732 = DIRECTION ( 'NONE',  ( 0.000000000000000000, 0.000000000000000000, 1.000000000000000000 ) ) ;
#72733 = CARTESIAN_POINT ( 'NONE',  ( -10.99878419127389684, 6.872217442641685103, 3.961452310287494338 ) ) ;
#72734 = CARTESIAN_POINT ( 'NONE',  ( 5.107728353013315292, 7.811434107096660640, 1.148430247377411728 ) ) ;
#72735 = CARTESIAN_POINT ( 'NONE',  ( -1.500000000000008216, 8.500000000000000000, 3.469446951953614189E-15 ) ) ;
#72736 = CARTESIAN_POINT ( 'NONE',  ( -1.445103857048105844, 8.688264192037886247, -2.625611233228243968 ) ) ;
#72737 = CARTESIAN_POINT ( 'NONE',  ( 6.925078400183574345, 7.629137130509068498, 2.744348168701661095 ) ) ;
#72738 = CARTESIAN_POINT ( 'NONE',  ( 7.483737605063422116, 7.833374748769873719, -0.7216878364870257245 ) ) ;
#72739 = CARTESIAN_POINT ( 'NONE',  ( -3.578462479003122976, 6.262291094557191684, 1.199719254218464037 ) ) ;
#72740 = CARTESIAN_POINT ( 'NONE',  ( 1.605537313848971026, -2.074692111233501723, 0.2571424261670462452 ) ) ;
#72741 = CARTESIAN_POINT ( 'NONE',  ( 0.2174332111963481196, -1.791455004416471430, 0.3504355335035569396 ) ) ;
#72742 = CARTESIAN_POINT ( 'NONE',  ( -5.579343907223557331, 6.467988298970945849, 1.199719254218450271 ) ) ;
#72743 = CARTESIAN_POINT ( 'NONE',  ( 2.573050890253928635, 0.09191801231544716178, -1.823395950357763695 ) ) ;
#72744 = CARTESIAN_POINT ( 'NONE',  ( 3.598431038176507002, -2.204323482753521635, -0.1086902067785888437 ) ) ;
#72745 = EDGE_CURVE ( 'NONE', #97721, #140594, #118148, .T. ) ;
#72746 = CARTESIAN_POINT ( 'NONE',  ( 1.387358672525637715, 7.251968950354889643, -4.302625267139783993 ) ) ;
#72747 = CARTESIAN_POINT ( 'NONE',  ( 1.494246876672610025, -1.020364814108923213, 1.617233793950809906 ) ) ;
#72748 = CARTESIAN_POINT ( 'NONE',  ( 1.205442482676940541, -1.550459043822360661, -1.214442484561629509 ) ) ;
#72749 = CARTESIAN_POINT ( 'NONE',  ( 3.245582950214185303, 1.942234966672530261, -0.002794291004394599230 ) ) ;
#72750 = ORIENTED_EDGE ( 'NONE', *, *, #96141, .F. ) ;
#72751 = DIRECTION ( 'NONE',  ( -1.561251128379126077E-17, -1.301042606982605475E-17, -1.000000000000000000 ) ) ;
#72753 = CARTESIAN_POINT ( 'NONE',  ( 0.1680794356360598985, -0.7909032441709142880, -1.683366987590989350 ) ) ;
#72752 = CARTESIAN_POINT ( 'NONE',  ( -5.061990249855848667, 6.999017606288844284, -1.599625672291271394 ) ) ;
#72754 = CARTESIAN_POINT ( 'NONE',  ( 4.386945222473598527, 7.275797305264619652, -1.199719254218452047 ) ) ;
#72755 = CARTESIAN_POINT ( 'NONE',  ( 6.531918710723870092, -6.583723166013912831, 7.057683771862373945 ) ) ;
#72756 = CARTESIAN_POINT ( 'NONE',  ( 7.560643217915098191, 11.97250085420964716, -0.7998128361456291469 ) ) ;
#72757 = CARTESIAN_POINT ( 'NONE',  ( -6.720001414228860881, 7.869031733802326123, -1.199719254218452047 ) ) ;
#72758 = FILL_AREA_STYLE ('',( #121605 ) ) ;
#72759 = ORIENTED_EDGE ( 'NONE', *, *, #147648, .F. ) ;
#72760 = CARTESIAN_POINT ( 'NONE',  ( 6.444921918449731280, 8.612437886315108315, 1.599625672291268286 ) ) ;
#72761 = CARTESIAN_POINT ( 'NONE',  ( -9.367496997601300279, 15.00000000000599343, 7.499999999995378808 ) ) ;
#72762 = CARTESIAN_POINT ( 'NONE',  ( 4.336427269025699971, 1.790907886515300085, 0.3537760332646966432 ) ) ;
#72763 = FILL_AREA_STYLE ('',( #6687 ) ) ;
#72764 = CARTESIAN_POINT ( 'NONE',  ( -8.649738815838677652, 13.03518635187974262, 0.7216878364870357165 ) ) ;
#72765 = CARTESIAN_POINT ( 'NONE',  ( -5.535867093699859964, 7.544539992772745229, 1.349747212490030046 ) ) ;
#72766 = CARTESIAN_POINT ( 'NONE',  ( -11.94105721237523099, 13.40000000000000036, 1.187919463087248273 ) ) ;
#72767 = CARTESIAN_POINT ( 'NONE',  ( 4.469519713540137218, 1.814478506493342191, -0.4545110902946307152 ) ) ;
#72768 = CARTESIAN_POINT ( 'NONE',  ( 7.242026607993941489, 11.60078147596829901, 0.7998128361456462443 ) ) ;
#72769 = CARTESIAN_POINT ( 'NONE',  ( 2.139170349095420143, -1.720849962885454110, 0.8662218532024426043 ) ) ;
#72770 = CARTESIAN_POINT ( 'NONE',  ( 6.385602409055195494, -1.848352663145738095, 0.6577735930803210174 ) ) ;
#72771 = ADVANCED_FACE ( 'NONE', ( #123894 ), #194160, .F. ) ;
#72772 = CARTESIAN_POINT ( 'NONE',  ( -1.364683531250000748, 9.671875000341396245, 0.000000000000000000 ) ) ;
#72773 = CARTESIAN_POINT ( 'NONE',  ( -5.551173829791513192, 8.563787670477010394, 1.199719254218452047 ) ) ;
#72774 = CARTESIAN_POINT ( 'NONE',  ( 4.009460741339333723, 5.700790169694431420, -1.599625672291256295 ) ) ;
#72775 = CARTESIAN_POINT ( 'NONE',  ( -4.950135482320926705, 6.868520377498098739, -1.443375672974066548 ) ) ;
#72776 = CARTESIAN_POINT ( 'NONE',  ( 0.4920138693931704887, -2.106576347024671225, 0.2123275358263312096 ) ) ;
#72777 = CARTESIAN_POINT ( 'NONE',  ( -1.872871967411093186, 3.300000000000011369, -0.3999999999999993006 ) ) ;
#72778 = CARTESIAN_POINT ( 'NONE',  ( 3.475000000000000533, -2.274999999999999467, 0.000000000000000000 ) ) ;
#72779 = CARTESIAN_POINT ( 'NONE',  ( 4.996967907133109676, 0.3485794866864948549, 2.040532872733556768 ) ) ;
#72781 = CARTESIAN_POINT ( 'NONE',  ( -1.201851678989727383E-14, 2.134375000341423689, 1.575800808251672791 ) ) ;
#72780 = CARTESIAN_POINT ( 'NONE',  ( 0.02850758872123548837, -1.683968158181762043, 0.7450552726024004535 ) ) ;
#72782 = CARTESIAN_POINT ( 'NONE',  ( 4.869944851454918400, -0.2802274231045227548, -2.281517807288702127 ) ) ;
#72783 = CARTESIAN_POINT ( 'NONE',  ( 6.317736394288131052, 9.354147645769410602, 1.082531754730558626 ) ) ;
#72784 = CARTESIAN_POINT ( 'NONE',  ( 3.594320121398666856, 7.207474218358159490, -1.734723475976807094E-15 ) ) ;
#72785 = CARTESIAN_POINT ( 'NONE',  ( -0.02301423135257947214, -0.1624751001964518382, -2.256290569412158220 ) ) ;
#72786 = CARTESIAN_POINT ( 'NONE',  ( -0.08522810233021893556, -9.999176686163549377, -9.579508557966956772 ) ) ;
#72787 = CARTESIAN_POINT ( 'NONE',  ( -5.562588163356775972, 9.711712967216715953, 0.7998128361456291469 ) ) ;
#72788 = CARTESIAN_POINT ( 'NONE',  ( 5.138593782488270811, -1.664572445771801634, 0.9999684565626990596 ) ) ;
#72789 = EDGE_LOOP ( 'NONE', ( #53079, #63390, #74983, #11267, #156014, #117231 ) ) ;
#72790 = CARTESIAN_POINT ( 'NONE',  ( 9.368320956918614328, 10.99242454023565507, 1.082531754730549967 ) ) ;
#72791 = EDGE_CURVE ( 'NONE', #106888, #23582, #38451, .T. ) ;
#72793 = ORIENTED_EDGE ( 'NONE', *, *, #98152, .F. ) ;
#72792 =( BOUNDED_CURVE ( )  B_SPLINE_CURVE ( 2, ( #184118, #36801, #106133 ),
 .UNSPECIFIED., .F., .T. ) 
 B_SPLINE_CURVE_WITH_KNOTS ( ( 3, 3 ),
 ( 0.1472187422488249742, 0.1500000000000002165 ),
 .UNSPECIFIED. ) 
 CURVE ( )  GEOMETRIC_REPRESENTATION_ITEM ( )  RATIONAL_B_SPLINE_CURVE ( ( 0.9405305184077480396, 0.9105717077955798322, 1.000000000000007105 ) ) 
 REPRESENTATION_ITEM ( '' )  );
#72794 = CARTESIAN_POINT ( 'NONE',  ( 5.748291730981218706, 0.9368611416523886515, -1.667099895225135686 ) ) ;
#72795 = CARTESIAN_POINT ( 'NONE',  ( 5.753138727196851043, 0.1435251449807967150, -2.011451301405759118 ) ) ;
#72797 = DIRECTION ( 'NONE',  ( 0.000000000000000000, -1.000000000000000000, 0.000000000000000000 ) ) ;
#72796 = CARTESIAN_POINT ( 'NONE',  ( -9.016335848287868160, 10.47781223021269170, 1.199719254218462483 ) ) ;
#72798 = CARTESIAN_POINT ( 'NONE',  ( -3.285556943750000514, -2.326041666188709112, -1.896917185911906500 ) ) ;
#72800 = CARTESIAN_POINT ( 'NONE',  ( 0.7953275966026486232, -0.6425790844533132429, 1.649264876520744272 ) ) ;
#72799 = CARTESIAN_POINT ( 'NONE',  ( 2.730511870197129820, 0.2565026084431647480, 2.074771742164283950 ) ) ;
#72801 = CARTESIAN_POINT ( 'NONE',  ( 10.50000000000000178, 0.000000000000000000, -3.600000000000002309 ) ) ;
#72802 = CARTESIAN_POINT ( 'NONE',  ( 4.382983890270373273, 2.048579214610211530, -1.028644635605566959 ) ) ;
#72803 = CARTESIAN_POINT ( 'NONE',  ( 2.466429552724667129, 0.08583113499382444278, -1.738331801394930043 ) ) ;
#72804 = CARTESIAN_POINT ( 'NONE',  ( 4.891794496432329886, 4.601515088792824670, -0.7998128361456211532 ) ) ;
#72805 = AXIS2_PLACEMENT_3D ( 'NONE', #129594, #30961, #195581 ) ;
#72806 = FACE_OUTER_BOUND ( 'NONE', #10001, .T. ) ;
#72807 = CARTESIAN_POINT ( 'NONE',  ( 1.809482579268039126, -1.467825596939468902, 0.9224971444230285478 ) ) ;
#72808 = CARTESIAN_POINT ( 'NONE',  ( -4.957638175832625493E-14, 2.359375000341373152, -1.570758158831806250 ) ) ;
#72809 = CARTESIAN_POINT ( 'NONE',  ( 1.310759002261387529, -1.470036769156491063, 1.141183394468782364 ) ) ;
#72810 = CARTESIAN_POINT ( 'NONE',  ( 2.295604378506800103, -1.940070289243904567, 0.9748468494522060102 ) ) ;
#72811 = CARTESIAN_POINT ( 'NONE',  ( 4.286349120214771879, 8.152491073559232859, -0.7998128361456221525 ) ) ;
#72812 = CARTESIAN_POINT ( 'NONE',  ( 4.768767694835816862, -0.2516295123269947642, -2.000731945836851544 ) ) ;
#72813 = CARTESIAN_POINT ( 'NONE',  ( 3.375000000000002665, 2.052068128417946724, -1.927395870058053847E-13 ) ) ;
#72814 = CARTESIAN_POINT ( 'NONE',  ( 0.7499999999999885647, 2.847916667349487341, -1.299038105676658228 ) ) ;
#72815 = CARTESIAN_POINT ( 'NONE',  ( 0.8153024884889724655, -0.2858729149923607826, 1.904955193227176879 ) ) ;
#72816 = CARTESIAN_POINT ( 'NONE',  ( -0.6823417656250039265, 14.81770833367473195, -1.181850606188755259 ) ) ;
#72817 = CARTESIAN_POINT ( 'NONE',  ( 4.623389083599304783, 1.933371432498669273, 1.093773624979002879 ) ) ;
#72818 = VERTEX_POINT ( 'NONE', #41504 ) ;
#72819 = CARTESIAN_POINT ( 'NONE',  ( -1.500000000000015099, 0.8791666666666874130, -0.8660254037844313801 ) ) ;
#72820 = CARTESIAN_POINT ( 'NONE',  ( 7.938462636001388795, 9.220293482545153907, -1.199719254218441611 ) ) ;
#72821 = CARTESIAN_POINT ( 'NONE',  ( -0.6823417656250003738, -0.5322916663252491576, -1.181850606188749264 ) ) ;
#72822 = CARTESIAN_POINT ( 'NONE',  ( 0.7158630905677393352, 1.819291361130066287, 1.274270043568943800 ) ) ;
#72824 = CARTESIAN_POINT ( 'NONE',  ( 6.355910407107248083, -0.6622273607519140182, 1.846833223631501264 ) ) ;
#72823 = CIRCLE ( 'NONE', #41786, 12.00000000000000178 ) ;
#72825 = CARTESIAN_POINT ( 'NONE',  ( 9.137832345930652522, 10.72352116074969075, -1.082531754730543083 ) ) ;
#72826 = CARTESIAN_POINT ( 'NONE',  ( 6.257125660641059461, -1.935629482380639033, -1.171090987803388606 ) ) ;
#72827 = CARTESIAN_POINT ( 'NONE',  ( -5.817857314039913241, 5.960124085900898372, 0.000000000000000000 ) ) ;
#72828 = CARTESIAN_POINT ( 'NONE',  ( 2.963389562657412046, 1.741120879107743935, 1.105697716663532892 ) ) ;
#72829 = CARTESIAN_POINT ( 'NONE',  ( -4.869349725602420520, 8.832658446511480577, 1.040834085586084257E-14 ) ) ;
#72830 = CARTESIAN_POINT ( 'NONE',  ( -1.499999999999997780, 3.181250000682818602, 1.214306433183764966E-14 ) ) ;
#72831 = CARTESIAN_POINT ( 'NONE',  ( -1.364683531250014514, -1.219791666325248602, 0.7879004041258379498 ) ) ;
#72832 = CARTESIAN_POINT ( 'NONE',  ( 4.393722961847310593, -0.7179090532695198146, 1.727491627791829742 ) ) ;
#72833 = CARTESIAN_POINT ( 'NONE',  ( 3.762146167370096883, 1.631196324480500115, -0.5889743285819144525 ) ) ;
#72834 = CARTESIAN_POINT ( 'NONE',  ( 3.157457554155696844, 0.7852445609939761040, 1.553317506218002464 ) ) ;
#72835 = CARTESIAN_POINT ( 'NONE',  ( 0.3281778771060560040, 1.171583119817346086, -1.970250653751925762 ) ) ;
#72836 = CARTESIAN_POINT ( 'NONE',  ( -1.001543065824772872E-14, 4.634375000341418804, 1.575800808251672791 ) ) ;
#72837 = CARTESIAN_POINT ( 'NONE',  ( 5.108965175345551835, -0.3053309577524323526, 2.068188354190988676 ) ) ;
#72838 = CARTESIAN_POINT ( 'NONE',  ( 6.140568862321206467, -1.639224632874112020, 1.040935801138809236 ) ) ;
#72839 = CARTESIAN_POINT ( 'NONE',  ( 9.367381717114165340, 13.89470468729395947, 7.500780834020892129 ) ) ;
#72840 = CARTESIAN_POINT ( 'NONE',  ( 0.7037502660087076034, 1.864169469917423161, 0.7691187473759173443 ) ) ;
#72841 = EDGE_CURVE ( 'NONE', #121330, #59550, #207901, .T. ) ;
#72842 = CARTESIAN_POINT ( 'NONE',  ( 0.4574861729177078229, -1.815669959853306370, 1.095388807130371900 ) ) ;
#72843 = CARTESIAN_POINT ( 'NONE',  ( -11.86145016429273191, 12.59412123665269512, -1.100000000000000089 ) ) ;
#72844 = CARTESIAN_POINT ( 'NONE',  ( -9.179033691651859783, 10.66762638080401260, 1.199719254218462483 ) ) ;
#72845 = CARTESIAN_POINT ( 'NONE',  ( 5.445571254183207088, 9.504916896522420444, -0.7998128361456281477 ) ) ;
#72846 = CARTESIAN_POINT ( 'NONE',  ( 3.847109862837356786, 4.045599327266925727, -0.8077998227820462063 ) ) ;
#72847 = CARTESIAN_POINT ( 'NONE',  ( 4.916531288042031989, 1.256637652550334883, -1.324621001416517840 ) ) ;
#72848 = ORIENTED_EDGE ( 'NONE', *, *, #176013, .T. ) ;
#72849 = CARTESIAN_POINT ( 'NONE',  ( -7.553827861469316396, 8.841829255582865699, -1.199719254218452047 ) ) ;
#72850 = CARTESIAN_POINT ( 'NONE',  ( 3.285556943749998737, -0.3427083328553764408, -1.896917185911906500 ) ) ;
#72851 = CARTESIAN_POINT ( 'NONE',  ( -7.314787569772770226, 8.492672571945082183, -1.199719254218452935 ) ) ;
#72852 = CARTESIAN_POINT ( 'NONE',  ( 2.320574876688247024, -0.7769297766534470906, -1.864587897788829718 ) ) ;
#72853 = CARTESIAN_POINT ( 'NONE',  ( 6.071336392737415544, 0.1682094380959769098, -2.200428349287026908 ) ) ;
#72854 = CARTESIAN_POINT ( 'NONE',  ( -5.971440312176176768, 5.931378217152456500, 0.000000000000000000 ) ) ;
#72855 = CARTESIAN_POINT ( 'NONE',  ( 2.869781510094356669, -1.841417136736220650, 0.2678509365347056526 ) ) ;
#72856 = CARTESIAN_POINT ( 'NONE',  ( 2.218730694130720771, 5.740269576461138890, 0.7998128361456462443 ) ) ;
#72857 = DIRECTION ( 'NONE',  ( -1.000000000000000000, 0.000000000000000000, 0.000000000000000000 ) ) ;
#72858 = ORIENTED_EDGE ( 'NONE', *, *, #80683, .T. ) ;
#72859 = VERTEX_POINT ( 'NONE', #106535 ) ;
#72860 = CARTESIAN_POINT ( 'NONE',  ( -5.752737250900127997, 5.605948302338584099, 0.000000000000000000 ) ) ;
#72861 = PRESENTATION_LAYER_ASSIGNMENT (  '', '', ( #145589 ) ) ;
#72862 = CARTESIAN_POINT ( 'NONE',  ( -9.643927338022246332, 10.14567007064778004, -0.7998128361456291469 ) ) ;
#72863 = CARTESIAN_POINT ( 'NONE',  ( 4.723181480036696023, -0.08661695748878039947, 1.823760500460340550 ) ) ;
#72865 = CARTESIAN_POINT ( 'NONE',  ( -4.014602626671047503, 7.795841479962435372, -0.4363419845254731255 ) ) ;
#72864 = CARTESIAN_POINT ( 'NONE',  ( -7.425025402139490360, 8.691559719698066289, 1.199719254218452047 ) ) ;
#72866 = CARTESIAN_POINT ( 'NONE',  ( 6.599791786788117953, 6.770233575417231364, 0.1470628079319712123 ) ) ;
#72867 = CARTESIAN_POINT ( 'NONE',  ( 0.3327679910518215878, -1.139612444193355278, 1.306804640533586026 ) ) ;
#72868 = CARTESIAN_POINT ( 'NONE',  ( 6.667912628260062036, -1.128459271250933149, 1.455361883854713767 ) ) ;
#72869 = CARTESIAN_POINT ( 'NONE',  ( 5.988978958577418688, -0.3324729122747641097, -2.283524998171110543 ) ) ;
#72870 = CARTESIAN_POINT ( 'NONE',  ( 5.065906673361608270, 5.939254536123854677, -1.199719254218450271 ) ) ;
#72871 = CARTESIAN_POINT ( 'NONE',  ( 6.626263010475290649, 1.250585457657760635, -1.762915812992614129 ) ) ;
#72872 = CARTESIAN_POINT ( 'NONE',  ( 6.277588818327314080, 7.282607361925381717, 1.199719254218462483 ) ) ;
#72873 = CARTESIAN_POINT ( 'NONE',  ( 6.257181701683109942, -2.286357481388684221, -0.2351346485395827413 ) ) ;
#72874 = CARTESIAN_POINT ( 'NONE',  ( 6.509799877575638050, 5.178456542363086612, 2.500000000000010214 ) ) ;
#72875 = CARTESIAN_POINT ( 'NONE',  ( -7.611976899429754084, 7.845337568948314022, 0.7998128361456341429 ) ) ;
#72876 = CARTESIAN_POINT ( 'NONE',  ( 6.069203928793593050, 0.1358119448514639727, -1.865795782587629681 ) ) ;
#72878 = CARTESIAN_POINT ( 'NONE',  ( -3.135678666510573365, 6.880318554229450712, 0.000000000000000000 ) ) ;
#72877 = CARTESIAN_POINT ( 'NONE',  ( 3.498220628606643956, -0.9384276995785534314, 1.666209768436441419 ) ) ;
#72879 = CARTESIAN_POINT ( 'NONE',  ( 4.864015066594513215, 2.183220759563545776, -0.3215228633955333759 ) ) ;
#72880 = CARTESIAN_POINT ( 'NONE',  ( 4.434827806327999333, -1.698493238601869182, 1.263996378755541938 ) ) ;
#72881 = CARTESIAN_POINT ( 'NONE',  ( -1.225000000000024736, 1.062500000682836676, -3.122502256758252770E-14 ) ) ;
#72882 = EDGE_CURVE ( 'NONE', #135497, #130628, #36932, .T. ) ;
#72883 = CARTESIAN_POINT ( 'NONE',  ( 6.983263157960378997, 2.960795523694306652, 2.498903865360342369 ) ) ;
#72884 = CARTESIAN_POINT ( 'NONE',  ( -0.1110810684433038154, 7.629137130509058728, -2.396956819904518809 ) ) ;
#72885 = CARTESIAN_POINT ( 'NONE',  ( 4.204437033569277560, 7.919277282557212416, 0.000000000000000000 ) ) ;
#72886 = CARTESIAN_POINT ( 'NONE',  ( -5.628043163004235794, 5.738674243025936761, 0.7216878364870257245 ) ) ;
#72887 = CARTESIAN_POINT ( 'NONE',  ( 5.707716976326653757, 1.605689621071492601, 1.385122894465253607 ) ) ;
#72888 = CARTESIAN_POINT ( 'NONE',  ( 2.890017657663559891, 1.631080081281432559, 1.632583592418336282 ) ) ;
#72889 = CARTESIAN_POINT ( 'NONE',  ( 3.613678190204441254, 0.4790664972640528152, -1.902336835828049244 ) ) ;
#72890 = CARTESIAN_POINT ( 'NONE',  ( -6.147696309153835692, 6.137010213626393096, 0.7998128361456282587 ) ) ;
#72891 = CARTESIAN_POINT ( 'NONE',  ( 6.631690664033638605, 1.975529463507015526, -0.5929735606366983713 ) ) ;
#72892 = CARTESIAN_POINT ( 'NONE',  ( 3.226477370372293763, 6.708047998835573900, 0.7216878364870317197 ) ) ;
#72893 = CARTESIAN_POINT ( 'NONE',  ( 5.740951700743842423, 5.662474837148078421, -0.7998128361456481317 ) ) ;
#72894 = ORIENTED_EDGE ( 'NONE', *, *, #2500, .F. ) ;
#72895 = CARTESIAN_POINT ( 'NONE',  ( 6.104703911763087909, 1.883310800321544409, 0.7212973825745233603 ) ) ;
#72896 = EDGE_CURVE ( 'NONE', #114917, #40498, #122836, .T. ) ;
#72897 = CARTESIAN_POINT ( 'NONE',  ( -8.513630394377489807, 12.01998699582738972, -1.199719254218446718 ) ) ;
#72898 = CARTESIAN_POINT ( 'NONE',  ( -4.492037202130076068, 8.252031063672584210, -0.07255873971346314677 ) ) ;
#72899 = CARTESIAN_POINT ( 'NONE',  ( -0.1409997244346088141, -0.002808977843308038680, -2.000147647483838220 ) ) ;
#72900 = CARTESIAN_POINT ( 'NONE',  ( 2.975608675790370583, -0.2172404834940108442, 2.160205341352925856 ) ) ;
#72901 = CARTESIAN_POINT ( 'NONE',  ( 5.123001941117305336, 7.070197912760590064, 1.599625672291268286 ) ) ;
#72903 = EDGE_CURVE ( 'NONE', #205352, #137219, #82097, .T. ) ;
#72902 = CARTESIAN_POINT ( 'NONE',  ( 0.2816890862925770511, 0.2015970107726860194, -2.110973810222869229 ) ) ;
#72904 = CARTESIAN_POINT ( 'NONE',  ( -1.201851678989727383E-14, 1.993750000682816381, 1.732050807568877637 ) ) ;
#72905 = CARTESIAN_POINT ( 'NONE',  ( -5.995690701609899698, 14.53061816844956411, -10.40446499585326912 ) ) ;
#72906 = CARTESIAN_POINT ( 'NONE',  ( 4.802592184731321545, 8.245026257381830703, 0.8702854636597904259 ) ) ;
#72907 = CARTESIAN_POINT ( 'NONE',  ( 0.5443023342626990280, 2.055102546481206272, 0.1540600304409632249 ) ) ;
#72909 = DIRECTION ( 'NONE',  ( -0.7806247498001041007, 0.000000000000000000, 0.6249999999996198596 ) ) ;
#72908 = CYLINDRICAL_SURFACE ( 'NONE', #49547, 1.224999999999996980 ) ;
#72910 = CARTESIAN_POINT ( 'NONE',  ( 0.6823417656249899377, 0.8427083336747520637, 1.181850606188755259 ) ) ;
#72911 = CARTESIAN_POINT ( 'NONE',  ( 5.962700214836534229, 7.205731455156047183, -1.256203146960620076 ) ) ;
#72912 = VERTEX_POINT ( 'NONE', #108684 ) ;
#72913 = CARTESIAN_POINT ( 'NONE',  ( 3.334525359879161766, 1.211162569113528598, -1.479845612687477274 ) ) ;
#72914 = CARTESIAN_POINT ( 'NONE',  ( 5.242920984569427567, -1.516648554753729616, 0.9119251698698880304 ) ) ;
#72915 = CARTESIAN_POINT ( 'NONE',  ( 5.525830126021535449, 8.604496359403894346, -1.199719254218452047 ) ) ;
#72916 = CARTESIAN_POINT ( 'NONE',  ( -2.903417451620861289, 6.539070793532962611, 0.7998128361456341429 ) ) ;
#72917 = CARTESIAN_POINT ( 'NONE',  ( 0.05258934297286410597, 0.3095000349466696110, 1.784779062553583984 ) ) ;
#72919 = CARTESIAN_POINT ( 'NONE',  ( 6.345329912860430355, 0.3219833572893218698, -1.888178885089139669 ) ) ;
#72918 = CARTESIAN_POINT ( 'NONE',  ( 1.500000000000001332, 7.809254910133564209, -3.635752117228656211 ) ) ;
#72920 = CARTESIAN_POINT ( 'NONE',  ( 0.3618904354094238385, -0.5536326762660361833, 1.994880328902041589 ) ) ;
#72921 = CARTESIAN_POINT ( 'NONE',  ( 1.364683531249986537, -0.2822916663252520997, -0.7879004041258309554 ) ) ;
#72922 = CARTESIAN_POINT ( 'NONE',  ( 5.875831987524620992, 1.115552982110395330, 1.501486808359139946 ) ) ;
#72923 = CARTESIAN_POINT ( 'NONE',  ( 3.264084022359412529, 0.8216391472936382945, 1.630427331384458833 ) ) ;
#72925 = CARTESIAN_POINT ( 'NONE',  ( 5.370783296855561773, 7.572579728427998091, 1.242435897699250891 ) ) ;
#72924 = CARTESIAN_POINT ( 'NONE',  ( 5.180388087185870738, -1.228261608319089149, 1.833297759731546073 ) ) ;
#72926 = CARTESIAN_POINT ( 'NONE',  ( -0.6823417656250212460, 0.8010416670080899859, 1.181850606188755259 ) ) ;
#72927 = CARTESIAN_POINT ( 'NONE',  ( 3.719230382982277927, -1.817711772858042751, -0.9750064267827946995 ) ) ;
#72928 = CARTESIAN_POINT ( 'NONE',  ( -6.367525699912501835, 10.58053041653993098, -0.7998128361456291469 ) ) ;
#72929 = CARTESIAN_POINT ( 'NONE',  ( 8.320953590485093088, 10.73086516036454618, 1.599625672291281386 ) ) ;
#72930 = FACE_OUTER_BOUND ( 'NONE', #65922, .T. ) ;
#72931 = EDGE_CURVE ( 'NONE', #95365, #83422, #5824, .T. ) ;
#72932 = CARTESIAN_POINT ( 'NONE',  ( 0.5972264258897291844, 1.797487153981947916, -1.200333582630601637 ) ) ;
#72933 = CARTESIAN_POINT ( 'NONE',  ( 6.777786256569462431, -2.009253640576996514, 0.4989836931604470505 ) ) ;
#72934 = CARTESIAN_POINT ( 'NONE',  ( 1.364683531249986537, 0.9260416670080896528, 0.7879004041258500513 ) ) ;
#72935 = CARTESIAN_POINT ( 'NONE',  ( 4.306063477043454490, -2.156128079323017754, 0.1542669963271598166 ) ) ;
#72937 = CARTESIAN_POINT ( 'NONE',  ( 1.820681965693775162, -1.389665069980907441, 1.385087887197037571 ) ) ;
#72936 = CARTESIAN_POINT ( 'NONE',  ( 3.897132395768299951, -0.2000006916238558641, -2.009757592718981911 ) ) ;
#72938 = CARTESIAN_POINT ( 'NONE',  ( 6.720655732516649827, 4.686306134629722564, 2.836255308917837947 ) ) ;
#72939 = B_SPLINE_SURFACE_WITH_KNOTS ( 'NONE', 1, 3, ( 
 ( #57144, #140570, #91807, #104844, #55016, #72304, #38763, #170890, #139484, #59271, #138409, #25699, #105943, #56083, #8383, #22482, #21410, #5155, #89666, #88593, #154650, #71231, #43057, #23558, #122241, #40913, #188199, #39836, #155717, #87520, #206583, #58211, #7302, #203364, #205512, #123310, #189274, #124370, #107019, #187134, #174126, #173043, #24626, #137346, #121165, #90733, #141641, #190328, #41989, #108097, #157865, #9458, #75530, #207650, #125426, #191392, #109170, #78716, #196744, #179441, #96071, #194603, #48384, #175183, #144843, #60335, #210849, #193544, #46247, #62475, #142699, #143778, #31061, #26770, #92871, #161049, #145900, #178377, #211909, #195684, #95003, #113434, #45186, #130750, #47321, #126496, #128638, #11584, #27844, #212970, #12645, #77656, #158917, #111301, #192459, #112364, #176242, #93942, #177304, #10513, #162124, #63546, #209773, #208708, #29986, #61413, #28918, #129702, #159982, #44113, #97137, #127576, #13713, #76588, #110234, #79786, #80865, #163191, #14774, #146955, #64611, #198844, #49428, #131787, #214017, #101363, #50491, #17960, #136014, #118745, #35288, #133912, #202027, #114497, #84046, #65639, #150134, #132840, #199918, #1707, #81919, #82977, #184729, #180495, #32112, #66693, #116612, #115548, #102431, #151199, #200969, #98197, #67761, #164245, #181544, #19033, #166368, #152256, #167441, #33172, #86187, #99253, #51565, #68841, #52617, #85113, #15833, #148006, #134961, #197792, #36354, #182606, #165301, #34229, #168500, #100302, #16896, #2770, #117690, #183682, #20099, #149050, #628, #3830, #69904, #89407, #70972, #87255, #56888, #155456, #55818, #7039, #121975, #8129, #189017, #38507, #74215, #73116, #139217, #106760, #124118, #137082, #172789, #187939, #141391, #40659, #186875, #75276, #90472, #91551, #153319, #22216, #204163, #24361, #9204, #54752, #140310, #205247, #23297, #21149, #104585, #120902, #123063, #190081, #156539, #203107, #185798, #170630, #88329, #206328, #154393, #53687, #25444, #39569, #57953, #41733, #107842, #4894, #173870, #157608, #119818, #37431, #103509, #169568, #105671, #5971 ),
 ( #72041, #138154, #171698, #108912, #161876, #174934, #79539, #61156, #208453, #143520, #13463, #11325, #142445, #45998, #209515, #44933, #144587, #207401, #158665, #127318, #29735, #28665, #10263, #26515, #210601, #94750, #193288, #160798, #111041, #145657, #128388, #192204, #211653, #12389, #78468, #112117, #63291, #76338, #92623, #43866, #60085, #126243, #177048, #30807, #109982, #129451, #77403, #27586, #194355, #175992, #59020, #191138, #62230, #96887, #178120, #93684, #80611, #95817, #159726, #195434, #47063, #113180, #179184, #125176, #162936, #14517, #42803, #114247, #198590, #49183, #148803, #35028, #213768, #97947, #84861, #131536, #98995, #81664, #1447, #115302, #181292, #67512, #166115, #102182, #197538, #165050, #50237, #133657, #149882, #17700, #164001, #18775, #147750, #32919, #83787, #16642, #117429, #168249, #150949, #199658, #51304, #183427, #101101, #66446, #167188, #196492, #65389, #48134, #31868, #82726, #372, #132588, #116357, #182347, #2513, #68586, #134711, #200718, #33976, #52369, #100051, #19848, #118498, #15577, #184480, #36097, #146704, #212720, #64359, #130505, #180244, #138971, #41475, #71786, #173618, #122802, #136827, #57704, #73953, #172530, #169314, #23038, #107585, #89154, #137901, #123861, #201785, #189826, #135762, #53425, #202853, #204994, #5709, #85935, #72865, #4644, #152007, #188761, #3579, #185549, #54501, #21960, #56638, #69654, #86994, #24114, #39316, #55568, #119562, #70714, #153067, #121722, #7865, #155207, #20898, #37178, #120645, #186624, #6788, #38251, #103253, #104325, #154141, #40401, #171449, #106503, #170373, #90217, #140045, #156281, #206070, #88068, #203920, #187687, #105411, #193019, #12138, #60898, #59831, #95567, #195174, #91294, #127057, #125983, #109723, #208198, #142183, #160533, #44671, #46808, #76082, #191941, #143264, #78211, #28400, #110783, #42547, #111859, #174679, #43606, #176785, #175730, #210335, #112922, #177864, #144335, #94495, #61973, #128128, #159465, #194091, #75021, #26252, #141132, #124920, #10006, #27324, #11064, #93426, #77143, #45740, #29476, #161617, #13209, #209254, #79283 ) ),
 .UNSPECIFIED., .F., .T., .F.,
 ( 2, 2 ),
 ( 4, 2, 2, 2, 2, 2, 2, 2, 2, 2, 2, 2, 2, 2, 2, 2, 2, 2, 2, 2, 2, 2, 2, 2, 2, 2, 2, 2, 2, 2, 2, 2, 2, 2, 2, 2, 2, 2, 2, 2, 2, 2, 2, 2, 2, 2, 2, 2, 2, 2, 2, 2, 2, 2, 2, 2, 2, 2, 2, 2, 2, 2, 2, 2, 2, 2, 2, 2, 2, 2, 2, 2, 2, 2, 2, 2, 2, 2, 2, 2, 2, 2, 2, 2, 2, 2, 2, 2, 2, 2, 2, 2, 2, 2, 2, 2, 2, 2, 2, 2, 2, 2, 2, 2, 2, 2, 2, 2, 2, 2, 2, 2, 2, 2, 2, 2, 2, 2, 2, 2, 2, 2, 4 ),
 ( 0.000000000000000000, 1.000000000000000000 ),
 ( -6.441036414471523752E-08, 0.0001394059631734492798, 0.0002788763367110432749, 0.0004183467102486372428, 0.0004532143036330357755, 0.0004880818970174342539, 0.0005578170837862312650, 0.0006275522705550282219, 0.0006972874573238252872, 0.0007670226440926222440, 0.0008367578308614192009, 0.0009064930176302162662, 0.0009413606110146147989, 0.0009762282043990132231, 0.001045963391167810180, 0.001115698577936607245, 0.001255168951474201159, 0.001324904138242998224, 0.001394639325011795290, 0.001464374511780592355, 0.001534109698549389203, 0.001603844885318186052, 0.001673580072086983117, 0.001743315258855780182, 0.001813050445624577248, 0.001882785632393374313, 0.001917653225777772846, 0.001952520819162171161, 0.002022256005930968010, 0.002091991192699765075, 0.002231461566237359206, 0.002301196753006155837, 0.002370931939774952903, 0.002405799533159351435, 0.002440667126543749968, 0.002510402313312547033, 0.002649872686850141164, 0.002719607873618938229, 0.002789343060387735294, 0.002859078247156532360, 0.002928813433925329425, 0.002998548620694126490, 0.003068283807462923122, 0.003207754181000516819, 0.003277489367769313884, 0.003312356961153712417, 0.003347224554538110949, 0.003416959741306908015, 0.003486694928075705080, 0.003626165301613299211, 0.003695900488382096276, 0.003765635675150893341, 0.003800503268535291874, 0.003835370861919690406, 0.003905106048688487038, 0.003974841235457283670, 0.004044576422226080735, 0.004114311608994877800, 0.004184046795763674866, 0.004253781982532471931, 0.004323517169301268996, 0.004393252356070066061, 0.004462987542838863127, 0.004532722729607660192, 0.004602457916376456390, 0.004672193103145253455, 0.004741928289914050521, 0.004811663476682847586, 0.004881398663451644651, 0.004951133850220441716, 0.005020869036989238782, 0.005090604223758035847, 0.005125471817142434813, 0.005160339410526832912, 0.005299809784064427043, 0.005439280157602021173, 0.005509015344370818239, 0.005578750531139615304, 0.005613618124524013403, 0.005648485717908412369, 0.005718220904677209435, 0.005857691278214803565, 0.005927426464983600631, 0.005997161651752397696, 0.006066896838521193894, 0.006136632025289990959, 0.006206367212058788024, 0.006276102398827584222, 0.006415572772365178353, 0.006485307959133975418, 0.006520175552518374384, 0.006555043145902772483, 0.006624778332671569549, 0.006694513519440366614, 0.006833983892977960745, 0.006903719079746757810, 0.006973454266515554875, 0.007043189453284351940, 0.007112924640053149006, 0.007182659826821946071, 0.007252395013590743136, 0.007322130200359540202, 0.007391865387128337267, 0.007461600573897134332, 0.007496468167281533299, 0.007531335760665931398, 0.007601070947434728463, 0.007670806134203525528, 0.007810276507741118791, 0.007880011694509915857, 0.007949746881278712055, 0.007984614474663111888, 0.008019482068047509987, 0.008089217254816306185, 0.008228687628353900316, 0.008298422815122698248, 0.008368158001891494446, 0.008437893188660290644, 0.008472760782044688743, 0.008507628375429088577, 0.008647098748966682707, 0.008786569122504276838, 0.008926039496041870969 ),
 .UNSPECIFIED. ) ;
#72942 = CARTESIAN_POINT ( 'NONE',  ( 5.341549334104176872, 9.175631956522799726, 0.7216878364870438212 ) ) ;
#72941 = CARTESIAN_POINT ( 'NONE',  ( -3.285556943750000070, -3.609374999522043659, 0.000000000000000000 ) ) ;
#72940 = CARTESIAN_POINT ( 'NONE',  ( -0.6125000000000019318, 1.458333333333332371, -1.060881119635941339 ) ) ;
#72943 = CARTESIAN_POINT ( 'NONE',  ( -7.469616286486262524, 7.679250187180907794, 0.7998128361456341429 ) ) ;
#72944 = CARTESIAN_POINT ( 'NONE',  ( 2.905482715143858030, -1.942096844255640109, 0.5424705965835219246 ) ) ;
#72946 = CARTESIAN_POINT ( 'NONE',  ( 1.876320386020374986, 0.7120587666045359310, 0.8722162550184342500 ) ) ;
#72945 = CARTESIAN_POINT ( 'NONE',  ( -3.741160322367112379, 6.452105245148518797, 1.199719254218464037 ) ) ;
#72947 = DIRECTION ( 'NONE',  ( -0.6483454320283800199, 0.000000000000000000, 0.7613463080411787542 ) ) ;
#72948 = CARTESIAN_POINT ( 'NONE',  ( 5.238497809344139000, 1.134185964801931679, -1.539638564045167080 ) ) ;
#72949 = CARTESIAN_POINT ( 'NONE',  ( -8.014278199453791274, 8.522615118883788199, 1.530808498934192557E-16 ) ) ;
#72950 = CARTESIAN_POINT ( 'NONE',  ( 4.650083499362856365, 8.368921815991249957, 0.7216878364870438212 ) ) ;
#72952 = CARTESIAN_POINT ( 'NONE',  ( 4.657827466662149973, 1.163286545301238206, 1.646828140416577657 ) ) ;
#72951 = CARTESIAN_POINT ( 'NONE',  ( -9.124274191872645545, 9.747334100047323702, -0.7216878364870267237 ) ) ;
#72953 = CARTESIAN_POINT ( 'NONE',  ( 1.499999999999987121, 4.295833333333352044, -0.8660254037844323793 ) ) ;
#72954 = CARTESIAN_POINT ( 'NONE',  ( 1.364683531249997417, 14.79687500034139447, 2.602085213965210642E-15 ) ) ;
#72955 = CARTESIAN_POINT ( 'NONE',  ( 6.563511714949607168, 0.2886701521849396879, -1.700279369998755508 ) ) ;
#72956 = CARTESIAN_POINT ( 'NONE',  ( 5.794130544993763898, 7.853181283949808744, 1.599625672291269396 ) ) ;
#72957 = CARTESIAN_POINT ( 'NONE',  ( 7.429504990608736037, 11.61158022244479682, -0.7216878364870267237 ) ) ;
#72958 = MECHANICAL_DESIGN_GEOMETRIC_PRESENTATION_REPRESENTATION (  '', ( #156011 ), #149036 ) ;
#72959 = CARTESIAN_POINT ( 'NONE',  ( -11.49966000274973155, 11.24232845564734617, -3.429881629453017222 ) ) ;
#72960 = CARTESIAN_POINT ( 'NONE',  ( 4.604681543780857034, 1.447206075137374759, -1.185162884121161442 ) ) ;
#72961 = DIRECTION ( 'NONE',  ( 0.000000000000000000, -1.000000000000000000, 0.000000000000000000 ) ) ;
#72962 = CARTESIAN_POINT ( 'NONE',  ( 1.797802452481820135, -1.496673605676283492, -1.430578824989765518 ) ) ;
#72963 = ORIENTED_EDGE ( 'NONE', *, *, #8288, .T. ) ;
#72964 = CARTESIAN_POINT ( 'NONE',  ( 4.472210567661338843, 6.310941310395290493, 1.599625672291261402 ) ) ;
#72965 = CARTESIAN_POINT ( 'NONE',  ( 0.2632962822839111650, 1.880428227362867633, -0.7283992291491694360 ) ) ;
#72966 = CARTESIAN_POINT ( 'NONE',  ( 0.5975729546051986585, 1.217269667385068477, 1.341803709015822132 ) ) ;
#72967 = CARTESIAN_POINT ( 'NONE',  ( 5.695833931072550094, 5.817763472438987726, 0.000000000000000000 ) ) ;
#72968 = FACE_OUTER_BOUND ( 'NONE', #41601, .T. ) ;
#72969 = VECTOR ( 'NONE', #141236, 1000.000000000000000 ) ;
#72970 = CARTESIAN_POINT ( 'NONE',  ( 7.659993601596707613, 9.959745173328078849, -1.443375672974058777 ) ) ;
#72971 = CARTESIAN_POINT ( 'NONE',  ( 9.074484886248265880, 9.481320543578137361, 0.7998128361456462443 ) ) ;
#72973 = CARTESIAN_POINT ( 'NONE',  ( 5.905858165902563073, -1.068448527453051966, -1.589740232873719128 ) ) ;
#72972 = CARTESIAN_POINT ( 'NONE',  ( -5.042743069279040036, 7.970618449879118828, 1.199719254218464037 ) ) ;
#72974 = CARTESIAN_POINT ( 'NONE',  ( -11.43190902327453529, 13.65522128257853396, 3.649704988378119186 ) ) ;
#72975 = CARTESIAN_POINT ( 'NONE',  ( -4.066554876651188977, 3.982284276321724992, -0.5266960748315950847 ) ) ;
#72976 = CARTESIAN_POINT ( 'NONE',  ( 5.553597010146855695, 5.912075037831448832, 0.6282849591137803502 ) ) ;
#72978 = ORIENTED_EDGE ( 'NONE', *, *, #99196, .T. ) ;
#72977 = CARTESIAN_POINT ( 'NONE',  ( 5.368665641331531013, 5.365790791082654998, -0.7216878364870207285 ) ) ;
#72979 = CARTESIAN_POINT ( 'NONE',  ( -7.619319141200077361, 9.912291636198670375, 1.443375672974090751 ) ) ;
#72980 = CARTESIAN_POINT ( 'NONE',  ( 3.204151765443470357, -2.159293047372488950, 0.1044485798024074874 ) ) ;
#72981 = CARTESIAN_POINT ( 'NONE',  ( -5.912764389335557702, 8.951956649983198844, 1.082531754730550855 ) ) ;
#72982 = CARTESIAN_POINT ( 'NONE',  ( 6.916067756746836714, 8.201738816693689316, -1.082531754730548412 ) ) ;
#72983 = CARTESIAN_POINT ( 'NONE',  ( 0.9320672075895163333, -2.067649466203642206, 0.4702014512557165515 ) ) ;
#72984 = CARTESIAN_POINT ( 'NONE',  ( 6.088856429251793934, -0.2706771573857471580, -1.805266125362497531 ) ) ;
#72985 = CARTESIAN_POINT ( 'NONE',  ( 2.108605603913331183, 1.463472826393363624, -1.321001006224751917 ) ) ;
#72986 = CARTESIAN_POINT ( 'NONE',  ( 3.920094060441734030, -1.906919942518231936, 0.1457910263855527466 ) ) ;
#72987 = EDGE_LOOP ( 'NONE', ( #54245, #24887, #189145 ) ) ;
#72988 = CARTESIAN_POINT ( 'NONE',  ( -4.386105069058221950, 14.48107186960593573, -11.17860366124935645 ) ) ;
#72989 = CARTESIAN_POINT ( 'NONE',  ( 5.353942763280384654, -0.7107094859252837127, 1.837027094894280399 ) ) ;
#72990 = CARTESIAN_POINT ( 'NONE',  ( 0.7791178172221034925, 1.303614328124411692, 1.439515497156283796 ) ) ;
#72991 = ORIENTED_EDGE ( 'NONE', *, *, #170575, .F. ) ;
#72992 = CARTESIAN_POINT ( 'NONE',  ( -4.936050443827081580, 7.916420063510339666, 1.199719254218452935 ) ) ;
#72994 = FACE_OUTER_BOUND ( 'NONE', #119214, .T. ) ;
#72993 = CARTESIAN_POINT ( 'NONE',  ( -5.320648938720212051, 5.172121614787156929, 0.000000000000000000 ) ) ;
#72995 = CARTESIAN_POINT ( 'NONE',  ( 6.685579144870162693, 6.972466221869550118, -0.7216878364870458196 ) ) ;
#72997 = ORIENTED_EDGE ( 'NONE', *, *, #181457, .F. ) ;
#72996 = CARTESIAN_POINT ( 'NONE',  ( 4.635362334195573197, -0.09024504784891507203, 1.910265517452472084 ) ) ;
#72998 = CARTESIAN_POINT ( 'NONE',  ( 0.5873203293235220723, -0.2722241568871349160, -2.189838084831654541 ) ) ;
#72999 = CARTESIAN_POINT ( 'NONE',  ( 9.681502974757661306, 4.134313097118687885, -7.090028219590201353 ) ) ;
#73000 = CARTESIAN_POINT ( 'NONE',  ( -0.1049974700286886165, -0.1398519552151776535, -1.881156918050665094 ) ) ;
#73001 = CARTESIAN_POINT ( 'NONE',  ( -2.428612866367529932E-14, 2.999999999999999112, 2.500000000000000444 ) ) ;
#73002 = CARTESIAN_POINT ( 'NONE',  ( 1.506653248757179320, -2.110590818861147078, -0.2044851626497797559 ) ) ;
#73004 = CARTESIAN_POINT ( 'NONE',  ( 5.524625123954316486, 0.3981063221985549072, 1.976670730632006601 ) ) ;
#73003 = CARTESIAN_POINT ( 'NONE',  ( -1.420000000000055440, 7.204077025658374822, -4.238769367544433564 ) ) ;
#73005 = CARTESIAN_POINT ( 'NONE',  ( 10.62873463776380056, 11.29999999999998117, 3.199999999999997957 ) ) ;
#73006 = CARTESIAN_POINT ( 'NONE',  ( 2.154816067267216084, -0.5500195584662928017, -1.995915215819036748 ) ) ;
#73007 = CARTESIAN_POINT ( 'NONE',  ( -5.605406444246153974, 8.627059054007450101, -1.199719254218440723 ) ) ;
#73008 = AXIS2_PLACEMENT_3D ( 'NONE', #178415, #45224, #126539 ) ;
#73009 = CARTESIAN_POINT ( 'NONE',  ( -4.981341760169012645, 7.953289812593539843, -1.047584607753747399 ) ) ;
#73010 = CARTESIAN_POINT ( 'NONE',  ( 0.3038912542124502236, -0.5749842496362895794, 2.083749421223294540 ) ) ;
#73011 = COLOUR_RGB ( '', 0.72549020, 0.75294118, 0.79215686) ;
#73012 = DIRECTION ( 'NONE',  ( -0.000000000000000000, -1.000000000000000000, -0.000000000000000000 ) ) ;
#73013 = CARTESIAN_POINT ( 'NONE',  ( 6.075462232699553766, 6.260663157670496304, -0.7216878364870458196 ) ) ;
#73014 = CARTESIAN_POINT ( 'NONE',  ( -4.853001412603734188, 5.021300470422864315, 0.7152689200764159594 ) ) ;
#73015 = ADVANCED_FACE ( 'NONE', ( #42580 ), #26287, .T. ) ;
#73016 = LINE ( 'NONE', #173766, #127427 ) ;
#73017 = CARTESIAN_POINT ( 'NONE',  ( -0.6823417656250003738, 13.46354166700806942, 1.181850606188754593 ) ) ;
#73019 = CARTESIAN_POINT ( 'NONE',  ( -7.279802135894939852, 7.457800344824362604, -0.7998128361456362523 ) ) ;
#73018 = CARTESIAN_POINT ( 'NONE',  ( 6.925078400183575233, 4.701279733332940580, 2.318349140213359583 ) ) ;
#73020 = CARTESIAN_POINT ( 'NONE',  ( 4.922368227709418065, -1.231479607182428104, -1.221251793340462299 ) ) ;
#73021 = CARTESIAN_POINT ( 'NONE',  ( -3.358669367883384105, 4.941533567329135401, -1.599625672291262513 ) ) ;
#73022 = CARTESIAN_POINT ( 'NONE',  ( 2.377862429009020229, -2.009158356589606953, 0.4988364127441884399 ) ) ;
#73023 = CARTESIAN_POINT ( 'NONE',  ( 3.568056664072499995, -1.041641863948725932, 1.843179926220348541 ) ) ;
#73024 = CARTESIAN_POINT ( 'NONE',  ( 6.612626235163189925, 8.737816579155630592, -1.599625672291262513 ) ) ;
#73025 = CARTESIAN_POINT ( 'NONE',  ( -0.6823417656250212460, 3.801041667008085767, 1.181850606188767472 ) ) ;
#73026 = CARTESIAN_POINT ( 'NONE',  ( 1.586696308167453662, 1.896558138806573757, 0.5304675795299080843 ) ) ;
#73027 = CARTESIAN_POINT ( 'NONE',  ( 6.110807642276722795, 6.018297815386236316, -0.1222484578899986352 ) ) ;
#73028 = CARTESIAN_POINT ( 'NONE',  ( 3.152547991667663307, -1.735656589536422212, 1.497406435017712756 ) ) ;
#73029 = CARTESIAN_POINT ( 'NONE',  ( 1.277666653898035021, 1.085793613588705853, 1.467558327050644706 ) ) ;
#73030 = B_SPLINE_CURVE_WITH_KNOTS ( 'NONE', 3,
 ( #39343, #37205, #88095, #38276, #121746, #202879, #153094, #120672, #103279, #135786, #168274, #102209, #187714, #71813, #19875, #201810, #4669, #199686 ),
 .UNSPECIFIED., .F., .F.,
 ( 4, 2, 2, 2, 2, 2, 2, 2, 4 ),
 ( -5.999999996874655676E-08, 0.0005266833517349315576, 0.001053426703469831751, 0.001580170055204731944, 0.002106913406939632354, 0.002633656758674532763, 0.003160400110409432740, 0.003687143462144333150, 0.004213886813879233993 ),
 .UNSPECIFIED. ) ;
#73031 = CARTESIAN_POINT ( 'NONE',  ( 5.367048706163317640, 7.354919138647580290, -1.599625672291281386 ) ) ;
#73032 = CARTESIAN_POINT ( 'NONE',  ( 5.978782553502139940, 6.077593855281705260, -0.7216878364870257245 ) ) ;
#73033 = CARTESIAN_POINT ( 'NONE',  ( -6.672584156219988571, 10.93643194889866521, -0.7998128361456291469 ) ) ;
#73034 = CARTESIAN_POINT ( 'NONE',  ( 3.041273912350466624, 0.05370876457178561797, 2.012661466405294863 ) ) ;
#73035 = CARTESIAN_POINT ( 'NONE',  ( 3.326955106232618586, -1.810811308836293598, -0.7551016064811162387 ) ) ;
#73036 = CARTESIAN_POINT ( 'NONE',  ( -7.537443334193545397, 10.88110209227943770, -1.199719254218446718 ) ) ;
#73037 = CARTESIAN_POINT ( 'NONE',  ( -6.039267359883488950, 9.133230122250985517, 1.199719254218452047 ) ) ;
#73038 = DIRECTION ( 'NONE',  ( 0.000000000000000000, 1.000000000000000000, 0.000000000000000000 ) ) ;
#73040 = CARTESIAN_POINT ( 'NONE',  ( 4.240886712856615226, -1.539575280908970223, 0.8727758839858139606 ) ) ;
#73039 = CARTESIAN_POINT ( 'NONE',  ( 6.175741434174033984, -1.119382356216396479, 1.765513623829425116 ) ) ;
#73041 = CARTESIAN_POINT ( 'NONE',  ( 4.897706171852771462, 4.871974472535213430, 0.6676900015689657408 ) ) ;
#73042 = CARTESIAN_POINT ( 'NONE',  ( 1.008081207548201741, -0.9882381260516819310, -1.956047874660173047 ) ) ;
#73043 = CARTESIAN_POINT ( 'NONE',  ( 5.314300430047540935, 1.610136290765556977, 0.6609758457527656894 ) ) ;
#73044 = CARTESIAN_POINT ( 'NONE',  ( 8.589254009457354400, 9.979550084910457031, -1.199719254218446718 ) ) ;
#73045 = CARTESIAN_POINT ( 'NONE',  ( 0.1333692844072316419, 7.629137130509075604, -2.653547345224521514 ) ) ;
#73046 = CARTESIAN_POINT ( 'NONE',  ( 6.522148393938469901, -2.055459957301557949, 1.029436805849759828 ) ) ;
#73047 = CARTESIAN_POINT ( 'NONE',  ( -3.475000000000000533, -1.385416665710749839, -2.006292185433948827 ) ) ;
#73048 = CARTESIAN_POINT ( 'NONE',  ( 5.448516766998877436, 1.166291874360864345, 1.283151444216067638 ) ) ;
#73049 = CARTESIAN_POINT ( 'NONE',  ( 1.524350002934187653, -1.228176919886795782, -1.833354347511229498 ) ) ;
#73050 = CARTESIAN_POINT ( 'NONE',  ( 5.283699308645180892, -2.063335151747126339, 0.6760268296895615148 ) ) ;
#73051 = CARTESIAN_POINT ( 'NONE',  ( 3.708318708537623021, 4.285125567170706695, -1.199719254218446718 ) ) ;
#73052 = CARTESIAN_POINT ( 'NONE',  ( 1.376322447316252306, -2.107681897322019271, -0.2017570171880012919 ) ) ;
#73053 = CARTESIAN_POINT ( 'NONE',  ( 4.406250000000002665, 1.895863743163984649, -0.7852924748302168023 ) ) ;
#73054 = CARTESIAN_POINT ( 'NONE',  ( 6.827182134110199918, 2.946470958711099541, 2.641117900019366527 ) ) ;
#73055 = CARTESIAN_POINT ( 'NONE',  ( 4.541967935523826938, 0.8243062533531859692, -1.741262965308258970 ) ) ;
#73056 = CARTESIAN_POINT ( 'NONE',  ( 1.524421784905782618, -2.203991335649616357, 0.2763902372489163151 ) ) ;
#73057 = ORIENTED_EDGE ( 'NONE', *, *, #77906, .T. ) ;
#73058 = CARTESIAN_POINT ( 'NONE',  ( 1.499999999999987121, 4.795833333333353821, -0.8660254037844323793 ) ) ;
#73059 = CARTESIAN_POINT ( 'NONE',  ( 3.337278367258157630, 7.045241861776501580, 0.7998128361456341429 ) ) ;
#73060 = CARTESIAN_POINT ( 'NONE',  ( 6.928380191783277908, 8.041863964290678624, 1.199719254218462483 ) ) ;
#73061 = CARTESIAN_POINT ( 'NONE',  ( 4.037882060770150439, -2.125535223720369071, 0.6451317522137323124 ) ) ;
#73062 = CARTESIAN_POINT ( 'NONE',  ( -8.731087737520713432, 10.24898578427137963, 1.082531754730558626 ) ) ;
#73063 = CARTESIAN_POINT ( 'NONE',  ( -0.7662865668244825956, -4.140281660848354583, 0.6727527331025086044 ) ) ;
#73064 = CARTESIAN_POINT ( 'NONE',  ( 5.477130870240836558, 9.333810415348903433, -0.7216878364870267237 ) ) ;
#73065 = CARTESIAN_POINT ( 'NONE',  ( -9.124274191872640216, 10.70770331434866485, -1.082531754730537976 ) ) ;
#73066 = CARTESIAN_POINT ( 'NONE',  ( 5.722950238744198614, 8.730506807626655430, 1.082531754730549967 ) ) ;
#73067 = CARTESIAN_POINT ( 'NONE',  ( 2.373672848961404735, -0.3474683332905931232, -1.986100487175908258 ) ) ;
#73069 = CARTESIAN_POINT ( 'NONE',  ( 6.127400154304522673, 0.1556050751826357770, -2.056880999590751991 ) ) ;
#73068 = CARTESIAN_POINT ( 'NONE',  ( 6.401421083946654100, 10.62007503124645957, -0.7998128361456291469 ) ) ;
#73070 = CARTESIAN_POINT ( 'NONE',  ( 7.146556367734771875, 8.470642196179646533, 1.082531754730549967 ) ) ;
#73071 = CARTESIAN_POINT ( 'NONE',  ( 6.216323138650166058, 1.627425874425829200, 0.6175015193602851893 ) ) ;
#73072 = CARTESIAN_POINT ( 'NONE',  ( 1.364683531249988757, 1.884375000341421913, 0.000000000000000000 ) ) ;
#73073 = CARTESIAN_POINT ( 'NONE',  ( 1.721574597234516890, -0.9778441516922768972, -1.474834890465251291 ) ) ;
#73074 = CARTESIAN_POINT ( 'NONE',  ( 0.6334356698059575574, 0.5880228326464317368, 1.928751028484784413 ) ) ;
#73075 = CARTESIAN_POINT ( 'NONE',  ( -0.006632162239710717895, -1.840811702136424088, -0.04651623371411393176 ) ) ;
#73076 = CARTESIAN_POINT ( 'NONE',  ( 4.282983983471492451, 2.047787327626307441, -1.030491903107624951 ) ) ;
#73077 = CARTESIAN_POINT ( 'NONE',  ( 2.185277780439310202, -0.7877041259056734024, 1.664256631099890971 ) ) ;
#73078 = CARTESIAN_POINT ( 'NONE',  ( 10.09812548408005384, 10.67556790771522124, -0.7998128361456281477 ) ) ;
#73079 = CARTESIAN_POINT ( 'NONE',  ( 11.17802523721653252, 8.279090859639403277, 4.430515473113522340 ) ) ;
#73080 = CARTESIAN_POINT ( 'NONE',  ( 3.469579810302122702, 1.781292651720441711, -0.3989491859636914994 ) ) ;
#73081 = CARTESIAN_POINT ( 'NONE',  ( 3.779922787921150995, 1.701948043757589124, -1.081065327119046016 ) ) ;
#73082 = CARTESIAN_POINT ( 'NONE',  ( -9.989660255170729641, 10.54902514065433827, -0.7998128361456291469 ) ) ;
#73084 = CARTESIAN_POINT ( 'NONE',  ( -9.579665964935227151, -7.246166700194470067, 0.000000000000000000 ) ) ;
#73083 = CARTESIAN_POINT ( 'NONE',  ( 3.256942907105137230, -1.714491093362701335, 1.476422526664717072 ) ) ;
#73085 = CARTESIAN_POINT ( 'NONE',  ( 5.456126526903398499, 2.103703387787753343, -0.1000602029373430374 ) ) ;
#73086 = CARTESIAN_POINT ( 'NONE',  ( 7.430330521100947827, 15.94469773494527765, 9.016016616261696370 ) ) ;
#73087 = CARTESIAN_POINT ( 'NONE',  ( 2.400909748719297188, 0.4512941399696759337, 2.020426262116347349 ) ) ;
#73088 = CARTESIAN_POINT ( 'NONE',  ( 3.460355519985863548, 5.060167411448709629, 1.599625672291267398 ) ) ;
#73089 = CARTESIAN_POINT ( 'NONE',  ( 1.360316468749987573, 0.2760416670081234369, 0.7853790794158701516 ) ) ;
#73090 = CARTESIAN_POINT ( 'NONE',  ( 5.918629486560170960, -0.7630358368452618834, -1.978611909900826582 ) ) ;
#73091 = ITEM_DEFINED_TRANSFORMATION ( 'NONE', 'NONE', #180180,  #200407 ) ;
#73093 = CARTESIAN_POINT ( 'NONE',  ( 1.277817996239123177, 1.146848889641904234, 1.547804080865310850 ) ) ;
#73092 = CARTESIAN_POINT ( 'NONE',  ( -8.696665468161981494, 12.23352791524263239, -1.199719254218446718 ) ) ;
#73094 = CARTESIAN_POINT ( 'NONE',  ( -5.004894982100124068, 5.868074229652107121, 1.199719254218452935 ) ) ;
#73095 = CARTESIAN_POINT ( 'NONE',  ( 8.178592977541601527, 10.56477777859713463, 1.599625672291281386 ) ) ;
#73096 = CARTESIAN_POINT ( 'NONE',  ( 4.353576723319599218, 8.093273587265928271, -0.7216878364870357165 ) ) ;
#73097 = CARTESIAN_POINT ( 'NONE',  ( 4.341180335511626964, 7.176948212357606494, 1.029809165597308063 ) ) ;
#73098 = CARTESIAN_POINT ( 'NONE',  ( -0.4500000000000545231, 4.000000000000003553, -0.8338124244296075682 ) ) ;
#73099 = CARTESIAN_POINT ( 'NONE',  ( -4.578903193113314174, 6.365139696764064325, 1.599625672291267398 ) ) ;
#73100 = CARTESIAN_POINT ( 'NONE',  ( 0.3873739525321840960, -2.094434250752406079, -0.7407286751721677831 ) ) ;
#73101 = CARTESIAN_POINT ( 'NONE',  ( 2.028482804581877019, 1.213238276247522895, -1.721163102310949045 ) ) ;
#73102 = CARTESIAN_POINT ( 'NONE',  ( -3.817502770699643388, 6.611447778194983194, 1.199719254218452935 ) ) ;
#73103 = CARTESIAN_POINT ( 'NONE',  ( 7.914208982075123799, 10.25632978388623684, -1.599625672291262513 ) ) ;
#73104 = CARTESIAN_POINT ( 'NONE',  ( 5.893359673372067675, -1.683065101977880840, 0.7942114673132483205 ) ) ;
#73105 = CARTESIAN_POINT ( 'NONE',  ( 5.913327553854682783, 10.05063257947248800, -0.7998128361456291469 ) ) ;
#73106 = CARTESIAN_POINT ( 'NONE',  ( 11.86145017031048177, 10.09418046486144505, 1.099999999999996980 ) ) ;
#73107 = CARTESIAN_POINT ( 'NONE',  ( -6.292392690518202159, 9.394856334696294553, -1.082531754730549967 ) ) ;
#73108 = CARTESIAN_POINT ( 'NONE',  ( -7.836249599018719536, 12.08611559892311504, 0.7216878364870478180 ) ) ;
#73109 = CARTESIAN_POINT ( 'NONE',  ( 0.4926326669930108371, -1.172979896111199904, 1.766458537607276114 ) ) ;
#73110 = CARTESIAN_POINT ( 'NONE',  ( 11.01135777277262306, 12.69999999999999929, -1.400000000000001910 ) ) ;
#73112 = CARTESIAN_POINT ( 'NONE',  ( 2.980854556682940526, 1.846358069237159949, 0.6635599008937702603 ) ) ;
#73111 = CARTESIAN_POINT ( 'NONE',  ( -4.156403723172807449E-14, -0.06249999999999229089, -1.414508159514581642 ) ) ;
#73113 = CARTESIAN_POINT ( 'NONE',  ( 2.026462046419864826, 1.244889377058140845, -1.767065586814352773 ) ) ;
#73114 = CARTESIAN_POINT ( 'NONE',  ( 1.100829259350871281, -0.4471758257712907247, 1.786007343351428966 ) ) ;
#73116 = CARTESIAN_POINT ( 'NONE',  ( -4.729598638066518035, 6.837371794175130191, -1.235194855336968045 ) ) ;
#73115 = CARTESIAN_POINT ( 'NONE',  ( -5.483346782084204563, 5.361935765378481378, 0.000000000000000000 ) ) ;
#73117 = CARTESIAN_POINT ( 'NONE',  ( 3.310250384734690243, 1.573932026098995518, 0.7429073729697617257 ) ) ;
#73118 = CARTESIAN_POINT ( 'NONE',  ( 5.639828713604826405, 9.523624565940227882, -0.7216878364870267237 ) ) ;
#73119 = CARTESIAN_POINT ( 'NONE',  ( -11.65681998539108655, 6.358950688113277572, -4.978640985104797245 ) ) ;
#73120 = AXIS2_PLACEMENT_3D ( 'NONE', #86589, #55158, #138552 ) ;
#73121 = CARTESIAN_POINT ( 'NONE',  ( 0.6202742476981680797, -1.157488721396517040, -1.825510493854154426 ) ) ;
#73122 = CARTESIAN_POINT ( 'NONE',  ( 2.249374845261054467, -1.976652949091894707, -0.3960421909960794018 ) ) ;
#73123 = DIRECTION ( 'NONE',  ( 1.000000000000000000, 0.000000000000000000, 0.000000000000000000 ) ) ;
#73124 = CARTESIAN_POINT ( 'NONE',  ( -4.442231607132987925, 5.211633625523774960, -1.199719254218453823 ) ) ;
#73125 = CARTESIAN_POINT ( 'NONE',  ( 2.694160965578366262, -1.966063403948969057, -0.1468289651068572232 ) ) ;
#73128 = VERTEX_POINT ( 'NONE', #191977 ) ;
#73127 = CARTESIAN_POINT ( 'NONE',  ( -5.370438244788932280, 6.398504386076097283, 1.082531754730549078 ) ) ;
#73126 = CARTESIAN_POINT ( 'NONE',  ( 10.95308175811721085, 11.29999999999998117, 1.799999999999999600 ) ) ;
#73129 = CARTESIAN_POINT ( 'NONE',  ( -5.438229012412890917, 8.398332043573416783, -1.082531754730549967 ) ) ;
#73130 = CARTESIAN_POINT ( 'NONE',  ( 4.037295881819344956, 7.932205305423046582, -0.7998128361456362523 ) ) ;
#73131 = CARTESIAN_POINT ( 'NONE',  ( -4.796552484184649856, 8.818004674849227342, -0.7998128361456362523 ) ) ;
#73132 = CARTESIAN_POINT ( 'NONE',  ( -7.282664789195997912, 8.525472337930658284, 1.199719254218452047 ) ) ;
#73133 = CARTESIAN_POINT ( 'NONE',  ( -1.406470046317634059, 4.362887876502464124, 0.01120553378793602735 ) ) ;
#73134 = CARTESIAN_POINT ( 'NONE',  ( 6.018676637735699941, 1.555688181992231245, -1.704518584337791021 ) ) ;
#73135 = LINE ( 'NONE', #74236, #66859 ) ;
#73136 = CARTESIAN_POINT ( 'NONE',  ( 3.573055779259231457, 1.771592698278463107, 0.8429337356923997104 ) ) ;
#73137 = CARTESIAN_POINT ( 'NONE',  ( 6.448874621594486989, 10.67543749183559143, 0.7998128361456462443 ) ) ;
#73138 = CARTESIAN_POINT ( 'NONE',  ( 0.1412502902482688505, 0.7743183493036235321, 1.862015731718666078 ) ) ;
#73139 = ORIENTED_EDGE ( 'NONE', *, *, #77470, .F. ) ;
#73140 = CARTESIAN_POINT ( 'NONE',  ( 2.641944905847165792, 2.106676525318150972, -0.2125944600365035908 ) ) ;
#73141 = CARTESIAN_POINT ( 'NONE',  ( -1.201851678989727383E-14, 0.9937500006828198229, 1.732050807568877637 ) ) ;
#73142 = CARTESIAN_POINT ( 'NONE',  ( -5.910464900553636269, 8.982960586366182554, -1.199719254218440723 ) ) ;
#73143 = CARTESIAN_POINT ( 'NONE',  ( 2.308333576337255000, 1.644441489820291924, 0.8281405146027611686 ) ) ;
#73144 = ORIENTED_EDGE ( 'NONE', *, *, #116234, .F. ) ;
#73145 = CARTESIAN_POINT ( 'NONE',  ( -8.947491310014823895, 12.52615806407091803, 1.199719254218462483 ) ) ;
#73146 = FACE_OUTER_BOUND ( 'NONE', #33716, .T. ) ;
#73148 = EDGE_CURVE ( 'NONE', #133229, #16921, #145804, .T. ) ;
#73147 = CARTESIAN_POINT ( 'NONE',  ( 3.586284538990120119, 1.181046903802231984, 1.761068336431830472 ) ) ;
#73149 = CARTESIAN_POINT ( 'NONE',  ( 0.5855841007226803008, -1.826885663252286740, -0.2280376995877145263 ) ) ;
#73150 = CARTESIAN_POINT ( 'NONE',  ( -0.7500000000000215383, 5.472916667349482900, 1.299038105676671107 ) ) ;
#73151 = CARTESIAN_POINT ( 'NONE',  ( 7.938462636001388795, 9.220293482545153907, -1.199719254218441611 ) ) ;
#73152 = CARTESIAN_POINT ( 'NONE',  ( 5.851225812749518695, 8.984124660586543243, -1.199719254218452047 ) ) ;
#73153 = CARTESIAN_POINT ( 'NONE',  ( 4.692684478349196553, -0.4476203070050369104, -2.011419953914685088 ) ) ;
#73155 = CARTESIAN_POINT ( 'NONE',  ( 1.874305484616908934, -0.09156810461483089192, -1.839108553062768214 ) ) ;
#73154 = CARTESIAN_POINT ( 'NONE',  ( -8.213542131780492639, 8.476887330032372603, 1.040834085586084257E-14 ) ) ;
#73156 = CARTESIAN_POINT ( 'NONE',  ( -1.364683531250010295, 5.238541667008086655, -0.7879004041258300672 ) ) ;
#73157 = CARTESIAN_POINT ( 'NONE',  ( -2.679285714285713826, 0.4970443252110372523, -0.5000000000000004441 ) ) ;
#73158 = CARTESIAN_POINT ( 'NONE',  ( -9.499734081922108331, -9.919612995835006330, 0.07111086427374822827 ) ) ;
#73159 = FACE_OUTER_BOUND ( 'NONE', #13632, .T. ) ;
#73160 = AXIS2_PLACEMENT_3D ( 'NONE', #133125, #199123, #50767 ) ;
#73161 = CARTESIAN_POINT ( 'NONE',  ( 0.6455096168876961471, -1.890800792967793686, 1.137844069391671820 ) ) ;
#73162 = CARTESIAN_POINT ( 'NONE',  ( 3.304270634109522486, -2.259957100417890441, 0.1074057698594049759 ) ) ;
#73163 = CARTESIAN_POINT ( 'NONE',  ( -9.002250809794013264, 9.604973487622245898, -0.7216878364870267237 ) ) ;
#73164 = CARTESIAN_POINT ( 'NONE',  ( 3.462975342835975301, -1.477922853017235916, 1.047338699574466014 ) ) ;
#73165 = CARTESIAN_POINT ( 'NONE',  ( 4.276519664212295346, -0.4255873229474533281, -1.867665486979957157 ) ) ;
#73166 = CARTESIAN_POINT ( 'NONE',  ( 5.740704066448026666, -2.019076491677873619, -0.4572469816465085657 ) ) ;
#73167 = CARTESIAN_POINT ( 'NONE',  ( 1.364683531249990311, 3.946875000341417028, 1.214306433183764966E-14 ) ) ;
#73168 = CARTESIAN_POINT ( 'NONE',  ( 2.588696453722662660, -0.3354253448964693574, -1.942569732146891770 ) ) ;
#73169 = CARTESIAN_POINT ( 'NONE',  ( 1.078981819582014445, -0.04439612541052954248, -1.926037623753373618 ) ) ;
#73170 = CARTESIAN_POINT ( 'NONE',  ( 4.328871119428026049, 0.09166491666120352155, 1.868520897946590598 ) ) ;
#73171 = CARTESIAN_POINT ( 'NONE',  ( 2.122082200655984074, -2.237848761721575208, 0.5630162806932179631 ) ) ;
#73172 = CARTESIAN_POINT ( 'NONE',  ( 3.736619961808427259, -1.792986960150410036, -0.4983748678565723678 ) ) ;
#73173 = CARTESIAN_POINT ( 'NONE',  ( 1.364683531249990311, 3.634375000341416584, 1.214306433183764966E-14 ) ) ;
#73174 = CARTESIAN_POINT ( 'NONE',  ( -4.731959306369413198, 5.479372931307791461, -1.199719254218446718 ) ) ;
#73175 = CARTESIAN_POINT ( 'NONE',  ( 5.666418135507635512, 8.698239360479199433, 1.199719254218462483 ) ) ;
#73176 = CARTESIAN_POINT ( 'NONE',  ( -3.147653791585727667, 8.920000000000001705, 2.419999999999999485 ) ) ;
#73178 = EDGE_CURVE ( 'NONE', #9929, #197638, #177897, .T. ) ;
#73177 =( BOUNDED_CURVE ( )  B_SPLINE_CURVE ( 2, ( #132797, #65597, #131746, #179403, #15794, #16854, #115509, #31023, #197751 ),
 .UNSPECIFIED., .F., .T. ) 
 B_SPLINE_CURVE_WITH_KNOTS ( ( 3, 2, 2, 2, 3 ),
 ( 0.9375000000000000000, 0.9404761904761904656, 0.9464285714285713969, 0.9523809523809523281, 0.9553571428571427937 ),
 .UNSPECIFIED. ) 
 CURVE ( )  GEOMETRIC_REPRESENTATION_ITEM ( )  RATIONAL_B_SPLINE_CURVE ( ( 0.9330127018922194093, 0.9330127018922194093, 1.000000000000000000, 0.8660254037844387076, 1.000000000000000000, 0.8660254037844387076, 1.000000000000000000, 0.9330127018922206306, 0.9330127018922194093 ) ) 
 REPRESENTATION_ITEM ( '' )  );
#73179 = CARTESIAN_POINT ( 'NONE',  ( 0.6804681372492230595, -1.168251705716750299, 1.752132397912719242 ) ) ;
#73180 = CARTESIAN_POINT ( 'NONE',  ( 3.348500752450942031, 4.929670182657964084, 1.443375672974066548 ) ) ;
#73182 = DIRECTION ( 'NONE',  ( 0.000000000000000000, -1.000000000000000000, 0.000000000000000000 ) ) ;
#73181 = CARTESIAN_POINT ( 'NONE',  ( -1.364683531249997417, 5.821875000341418804, 1.214306433183764966E-14 ) ) ;
#73183 = CARTESIAN_POINT ( 'NONE',  ( 1.723052270212792836, 1.567896913533245229, -1.427966198690698851 ) ) ;
#73184 = CARTESIAN_POINT ( 'NONE',  ( 0.000000000000000000, -7.246166700194011767, 9.579665964935665912 ) ) ;
#73185 = CARTESIAN_POINT ( 'NONE',  ( 0.4397206748869232351, -1.916487937148562137, 0.6377882026268544280 ) ) ;
#73186 = CARTESIAN_POINT ( 'NONE',  ( -0.6823417656250212460, 1.051041667008083325, 1.181850606188755259 ) ) ;
#73187 = CARTESIAN_POINT ( 'NONE',  ( -3.850152436600983386, 4.554561266531622188, 1.082531754730560403 ) ) ;
#73188 = CARTESIAN_POINT ( 'NONE',  ( 4.137209430464448445, 7.978494768850520558, 1.040834085586084257E-14 ) ) ;
#73189 = ORIENTED_EDGE ( 'NONE', *, *, #166799, .T. ) ;
#73190 = CARTESIAN_POINT ( 'NONE',  ( 1.563986776035675819, 2.129895014553784272, -0.3678597298803277793 ) ) ;
#73191 = CARTESIAN_POINT ( 'NONE',  ( 6.610000000000042952, 4.702635990354799844, 2.282722937023287102 ) ) ;
#73194 = CARTESIAN_POINT ( 'NONE',  ( 2.873965376416980355, 6.296784005887697155, -0.7216878364870267237 ) ) ;
#73193 = CARTESIAN_POINT ( 'NONE',  ( 6.925078400183573457, 0.5887076473912872254, 1.908330883025354030 ) ) ;
#73192 = CARTESIAN_POINT ( 'NONE',  ( 6.398522151006641678, 6.429640362454684954, 0.000000000000000000 ) ) ;
#73195 = CARTESIAN_POINT ( 'NONE',  ( -0.2104748580754409182, 1.337026610731705700, -2.356057411969681326 ) ) ;
#73196 = CARTESIAN_POINT ( 'NONE',  ( 5.928922775424462444, -1.700964743930567513, 1.082835439959836776 ) ) ;
#73197 = CARTESIAN_POINT ( 'NONE',  ( -7.348156068926747331, 11.51667314714914347, 0.7216878364870458196 ) ) ;
#73198 = CARTESIAN_POINT ( 'NONE',  ( 6.614806893291146572, -0.1579704184760947761, 2.055781730312715272 ) ) ;
#73199 = CARTESIAN_POINT ( 'NONE',  ( 0.7499999999999920064, 4.983333333333353821, 1.299038105676669330 ) ) ;
#73201 = CARTESIAN_POINT ( 'NONE',  ( 1.364683531250000748, 10.25520833367473017, -0.7879004041258355073 ) ) ;
#73200 = CARTESIAN_POINT ( 'NONE',  ( 0.3041012005207919255, -0.5996659824250392123, 2.181524510355018265 ) ) ;
#73202 = DIRECTION ( 'NONE',  ( 0.000000000000000000, 0.000000000000000000, -1.000000000000000000 ) ) ;
#73204 = CARTESIAN_POINT ( 'NONE',  ( 1.282674911181800104, 1.565081248417903081, -1.104254300028691071 ) ) ;
#73203 = CARTESIAN_POINT ( 'NONE',  ( -6.683806541412780078, 6.900121841177441873, -0.7216878364870267237 ) ) ;
#73205 = CARTESIAN_POINT ( 'NONE',  ( -0.6823417656250246877, 0.1135416670080893753, 1.181850606188755259 ) ) ;
#73206 = CARTESIAN_POINT ( 'NONE',  ( 1.224999999999995204, 2.666666667349464781, 0.7072540797572858251 ) ) ;
#73207 = CARTESIAN_POINT ( 'NONE',  ( 1.499999999999993117, 9.354166666666667851, 0.8660254037844409281 ) ) ;
#73208 = CARTESIAN_POINT ( 'NONE',  ( 2.437784706471317175, 0.8137022719644730895, -1.520871857739027444 ) ) ;
#73209 = CARTESIAN_POINT ( 'NONE',  ( 4.030516805012513082, 7.924296382481737844, 0.000000000000000000 ) ) ;
#73210 = CARTESIAN_POINT ( 'NONE',  ( 1.827073579719180163, -1.668441312418825095, 0.5905873696427661468 ) ) ;
#73211 = CARTESIAN_POINT ( 'NONE',  ( 1.787745399045566730, 1.925802014453177557, -0.5863169366013292194 ) ) ;
#73212 = CARTESIAN_POINT ( 'NONE',  ( 8.919266336783559623, 2.972657967447078775, 7.510420563956574647 ) ) ;
#73213 = CARTESIAN_POINT ( 'NONE',  ( 8.536830278099042602, 13.11138575775759563, -0.7998128361456352531 ) ) ;
#73214 = CARTESIAN_POINT ( 'NONE',  ( 3.751171811254182753, -1.805526059370649028, 1.268566889074909554 ) ) ;
#73215 = ORIENTED_EDGE ( 'NONE', *, *, #63494, .F. ) ;
#73216 = CARTESIAN_POINT ( 'NONE',  ( 4.658466178349073061, 2.014666459302273616, 0.1442823096002471550 ) ) ;
#73217 = CARTESIAN_POINT ( 'NONE',  ( -7.425025402139490360, 8.691559719698066289, 1.199719254218452047 ) ) ;
#73219 = CARTESIAN_POINT ( 'NONE',  ( 4.464470365011488973, -1.956567236562205325, -0.4871837624095613495 ) ) ;
#73218 = CARTESIAN_POINT ( 'NONE',  ( 3.932379033323248230, -1.091282289853046317, -1.817994770353311473 ) ) ;
#73220 = VERTEX_POINT ( 'NONE', #45776 ) ;
#73221 = CARTESIAN_POINT ( 'NONE',  ( 5.194709132691408549, 6.089524072008651423, 1.199719254218452935 ) ) ;
#73222 = VERTEX_POINT ( 'NONE', #62009 ) ;
#73223 = CARTESIAN_POINT ( 'NONE',  ( 1.410794581852807150, 1.648159533202856686, 0.8848386531258023435 ) ) ;
#73224 = STYLED_ITEM ( 'NONE', ( #174756 ), #74771 ) ;
#73225 = CARTESIAN_POINT ( 'NONE',  ( 4.996790860652426159E-15, 0.6250000006827882704, 1.224999999999976330 ) ) ;
#73226 = CARTESIAN_POINT ( 'NONE',  ( -4.302014814237876017, 3.913438792899272212, 0.7998128361456341429 ) ) ;
#73227 = DIRECTION ( 'NONE',  ( -5.551115123125765446E-17, 0.000000000000000000, 1.000000000000000000 ) ) ;
#73228 = CARTESIAN_POINT ( 'NONE',  ( 0.000000000000000000, 0.000000000000000000, 0.000000000000000000 ) ) ;
#73229 = CARTESIAN_POINT ( 'NONE',  ( -1.201851678989727383E-14, 2.384375000341416584, 1.575800808251672791 ) ) ;
#73230 = CARTESIAN_POINT ( 'NONE',  ( -0.001745240643731549302, -9.900000000000005684, -0.09998476951563611825 ) ) ;
#73231 = CARTESIAN_POINT ( 'NONE',  ( 4.223842396274177347, 0.8578445224393380641, -1.825075645057252505 ) ) ;
#73232 = CARTESIAN_POINT ( 'NONE',  ( 7.363486825997814123, 7.763358516518489516, 0.000000000000000000 ) ) ;
#73233 = CARTESIAN_POINT ( 'NONE',  ( -5.329763783947941036, 5.390681634126922361, 0.000000000000000000 ) ) ;
#73234 = CARTESIAN_POINT ( 'NONE',  ( -6.231907884136888676, 7.299589282028351001, -1.199719254218453823 ) ) ;
#73235 = CARTESIAN_POINT ( 'NONE',  ( 4.430007776716601953, -2.079114408633813582, 0.4165480963118637914 ) ) ;
#73237 = CARTESIAN_POINT ( 'NONE',  ( -11.41048919578708443, 9.369870944694024928, -1.242167297096143264 ) ) ;
#73236 = CARTESIAN_POINT ( 'NONE',  ( -5.546112223000226216, 5.929839062422638918, -0.8878705470019981894 ) ) ;
#73238 = CARTESIAN_POINT ( 'NONE',  ( 5.202397865228217455, -0.6614073030348812665, -1.857238293531390916 ) ) ;
#73239 = CARTESIAN_POINT ( 'NONE',  ( -1.364683531250000748, 0.5093750003414208027, 0.000000000000000000 ) ) ;
#73240 = CARTESIAN_POINT ( 'NONE',  ( 0.4748584900105623507, -1.455329053371579695, 1.391259960792426975 ) ) ;
#73241 = ORIENTED_EDGE ( 'NONE', *, *, #67862, .F. ) ;
#73242 = CARTESIAN_POINT ( 'NONE',  ( 6.227753904044541322, 0.8083430201051154951, -1.957153335705215103 ) ) ;
#73243 = CARTESIAN_POINT ( 'NONE',  ( -0.1021852871783679312, 7.053056311350174745, -4.037408415133499240 ) ) ;
#73244 = CARTESIAN_POINT ( 'NONE',  ( 1.064989848632340363, 1.568927673159369762, -1.351003706900590018 ) ) ;
#73245 = VERTEX_POINT ( 'NONE', #60934 ) ;
#73246 = CARTESIAN_POINT ( 'NONE',  ( 5.662465432362883355, 6.635239754958710989, 1.199719254218451159 ) ) ;
#73247 = CARTESIAN_POINT ( 'NONE',  ( 6.225128807330042591, 7.291680359087043151, -1.199719254218452047 ) ) ;
#73249 = CARTESIAN_POINT ( 'NONE',  ( 6.505214776458575265, 6.483838748823460563, 1.040834085586084257E-14 ) ) ;
#73248 = CARTESIAN_POINT ( 'NONE',  ( 3.574242788201603016, -2.014869992041759872, -0.5574694344734670848 ) ) ;
#73250 = CARTESIAN_POINT ( 'NONE',  ( 5.189738938980948291, 9.276722205444929870, 0.000000000000000000 ) ) ;
#73253 = ORIENTED_EDGE ( 'NONE', *, *, #124080, .F. ) ;
#73252 = CARTESIAN_POINT ( 'NONE',  ( 1.681973674898680216, 0.9313724848135003231, 1.553549296804368707 ) ) ;
#73251 = CARTESIAN_POINT ( 'NONE',  ( 2.274178591966895091, -1.125271047149905890, 1.437439779654096750 ) ) ;
#73254 = CARTESIAN_POINT ( 'NONE',  ( 5.162800556355915838, -1.600310254184673431, 1.519886962452212886 ) ) ;
#73255 = DIRECTION ( 'NONE',  ( 0.000000000000000000, 0.000000000000000000, 1.000000000000000000 ) ) ;
#73256 =( GEOMETRIC_REPRESENTATION_CONTEXT ( 3 ) GLOBAL_UNCERTAINTY_ASSIGNED_CONTEXT ( ( #199953 ) ) GLOBAL_UNIT_ASSIGNED_CONTEXT ( ( #135717, #67466, #82677 ) ) REPRESENTATION_CONTEXT ( 'NONE', 'WORKASPACE' ) );
#73257 = CARTESIAN_POINT ( 'NONE',  ( 4.366400497975233996, 1.037236317483503312, 1.947806255051434343 ) ) ;
#73258 = CARTESIAN_POINT ( 'NONE',  ( 6.608709811657416999, 9.797579649320619311, -1.199719254218440723 ) ) ;
#73259 = CARTESIAN_POINT ( 'NONE',  ( 3.172244755473273781, 6.644776614786712443, 0.000000000000000000 ) ) ;
#73260 = CARTESIAN_POINT ( 'NONE',  ( 2.982959643696237784, -1.767753630637520779, -0.7297678730374329570 ) ) ;
#73261 =( BOUNDED_SURFACE ( )  B_SPLINE_SURFACE ( 1, 2, ( 
 ( #154654, #6237, #117944, #10517, #11588, #8387, #175187, #141645, #90737, #124374, #140574, #24630, #74469, #206587, #58216, #155721, #190332, #123314, #126500, #92875, #60340, #189278, #41994, #107023, #73382, #109174, #207654, #108101, #158921, #173048, #174130, #156800, #40917, #171971, #25703, #208713, #91811, #157869, #76592, #192464, #193548, #9462, #159986, #142703, #44117, #75534, #110238, #59275, #23562, #125432, #191396, #43061, #26773, #176246, #209777, #27848, #143782, #93946, #77661, #61417, #127580, #45190, #89671, #7306, #139488, #205516, #57148, #211913, #32116, #96076, #148010, #162129, #82981, #99257, #197797, #194607, #48389, #132844, #13717, #95007, #178381, #29990, #49432, #198848, #79790, #131792, #112369, #14778, #180499, #98201, #145904, #111305, #214021, #149054, #16900, #63550, #633, #129706, #114502, #177307, #130754, #164249, #195688, #115552, #66697, #47324, #62479, #46251, #113438, #181548, #212974, #163195, #179445, #161054, #15837, #28922, #31066, #196748, #65643, #33176, #97141, #80869, #81923, #146959, #64615, #165306, #12649, #78720, #144847, #210853, #128642, #68845, #17964, #88331, #138157, #5973, #72045, #183686, #104587, #4897, #52621, #153322, #134965, #170632, #21152, #34233, #50495, #101367, #2775, #168503, #84051, #200973, #184732, #152259, #137085, #199923, #151203, #202030, #53690, #35292, #22218, #20103, #103512, #119822, #185802, #37435, #51569, #87258, #166372, #186877, #116616, #117694, #150139, #154395, #36358, #118749, #102435, #70975, #203111, #182611, #100306, #54756, #86190, #3833, #69907, #169571, #120905, #136017, #1711, #167445, #38509, #67765, #133916, #19039, #85117, #159730, #123066, #43870, #158669, #206331, #92626, #74218, #109986, #174937, #187941, #11329, #40662, #156542, #107845, #171700, #8132, #124122, #91554, #76341, #139219, #90476, #141394, #207404, #189020, #175997, #173874, #42807, #59023, #125179, #191141, #205249, #26518, #105673, #126248, #77407, #56891, #23299, #27590, #190084, #140313, #41736, #10266, #142448, #204165, #93688, #106764, #55820, #208456, #121977, #108915, #155459, #157611, #172792, #24364, #39571, #60088, #89410, #57956, #192208, #25447, #7042, #9207, #73118, #75279, #115307, #131541, #15582, #12393, #80616, #165055, #194359, #127322, #210606, #62234, #81669, #16647, #46002, #164006, #144591, #47068, #212725, #130510, #128392, #143524, #180249, #181297, #49188, #112121, #32924, #29739, #146709, #209520, #162941, #196497, #178124, #147755, #99000, #95821, #94754, #78472, #161880, #213773, #30813, #195438, #211657, #193293, #64364, #61160, #13467, #14522, #31873, #65395, #79543, #145661, #63295, #44937, #197543, #111045, #48140, #160802, #96892, #129455, #113185, #177052, #114253, #28669, #179189, #97952, #183432, #3584, #67517, #119567, #133662, #57438, #73681, #169319, #166120, #19853, #107316, #199663, #66451, #149887, #1452, #20903, #173340, #51309, #103258, #83792, #200723, #152013, #69659, #117435, #82732, #185554, #123599, #205807, #35033, #189564, #101107, #85940, #148808, #102187, #135767, #167193, #86999, #41209, #18780, #33981, #17705, #84866, #156009, #184485, #134717, #150954, #132593, #201790, #377, #2518, #168254, #37183, #7597, #68591, #52374, #53430, #118503, #36102, #139780, #198595, #50242, #116362, #182352, #100056, #43341, #206873, #62755, #112655, #194896, #46534, #158151, #79009, #193821, #27054, #127871, #109461, #145125, #210063, #8675, #24920, #75818, #191680, #142993, #58504, #175468, #159198, #126791, #111586, #174412, #125719, #176523, #28134, #9744, #211131, #208992, #77947, #94230, #160268, #11870, #25989, #61703, #140859, #161347, #91024, #92097, #124659, #128915, #10799, #93161, #76873, #45469, #177596, #157086, #74757, #141926, #190616, #60628, #29208, #207938, #59560, #42274, #95298, #144068, #108387, #192746, #12928, #44403, #110523, #131037, #147235, #31348, #15058, #213263, #81150, #162416, #197026, #129990, #133135, #99537, #66997, #195978, #64890, #113725, #80077, #115842, #148297, #48663, #165599, #179729, #114779, #97422, #47611, #178664, #180777, #930, #163476, #32403, #17189 ),
 ( #98469, #164534, #214294, #134198, #30276, #16120, #212194, #96362, #18261, #199134, #181828, #50779, #13993, #82203, #116907, #65928, #132075, #198086, #49713, #33461, #200208, #146179, #83264, #149350, #182907, #34523, #100595, #84344, #51860, #166670, #150432, #1997, #68062, #63832, #3065, #23599, #119044, #5196, #69135, #151496, #204468, #201271, #135257, #168794, #52911, #169859, #172008, #20401, #154689, #105988, #137385, #73421, #203400, #185028, #117982, #101664, #186102, #205549, #89707, #155758, #167732, #19333, #153624, #21447, #7343, #36653, #202334, #183973, #104883, #88632, #87556, #120124, #139523, #35585, #102739, #37734, #6273, #86482, #152547, #85412, #4133, #71270, #103810, #55054, #121205, #70202, #136315, #53985, #187174, #38801, #170926, #22523, #56121, #72344, #138448, #122279, #188237, #39877, #111337, #108137, #93979, #45222, #76625, #12678, #142738, #58253, #57188, #40953, #125469, #144878, #177341, #28954, #107060, #173086, #92910, #109212, #95038, #124409, #141680, #123348, #44150, #27882, #174165, #24666, #175223, #11619, #25738, #190366, #8421, #77694, #110271, #161088, #91848, #60374, #26808, #42027, #9499, #157905, #75571, #207693, #59312, #191431, #90772, #43098, #74506, #143815, #192499, #160020, #140611, #158956, #206623, #156834, #208747, #10551, #126537, #176280, #209812, #61447, #127614, #193579, #189315, #78753, #33207, #13751, #163228, #197832, #99291, #17998, #31100, #198879, #49465, #83012, #211946, #115584, #179477, #62509, #195722, #47357, #64645, #113472, #129739, #97174, #180527, #166405, #128674, #14809, #30022, #194641, #50526, #16932, #214048, #149087, #46285, #146991, #667, #80901, #145935, #213009, #130784, #84088, #210884, #162163, #196778, #165338, #63582, #48421, #116649, #112402, #98228, #114533, #164282, #32149, #178412, #96108, #182646, #15871, #81955, #79824, #148040, #66733, #65676, #131823, #181578, #132878, #34266, #100340, #201010, #186913, #138192, #169607, #105709, #21189, #151239, #150176, #133950, #3869, #23334, #204202, #55856, #199958, #51604, #185837, #202066, #122012, #2808, #20138, #1744, #137120, #120942, #52655, #117729, #53726, #104622, #118784, #68879, #101404, #170670, #203150, #187979, #184770, #153361, #119859, #134999, #102474, #36397, #168541, #86224, #152296, #69942, #183718, #136054, #167479, #22257, #71008, #38545, #19075, #37469, #85156, #35326, #87292, #103546, #4932, #54794, #88367, #154433, #6011, #72081, #67801, #39605, #171737, #106796, #41768, #76369, #126279, #111074, #124153, #77437, #142476, #176026, #90508, #208484, #57990, #155495, #74251, #140345, #157641, #206363, #8167, #190114, #59051, #44966, #7078, #107881, #123099, #73151, #143554, #110013, #92655, #27618, #139257, #25483, #93718, #173907, #24396, #91589, #207432, #9238, #156573, #40693, #89443, #75310, #192237, #172824, #141426, #60120, #43899, #177080, #125209, #209548, #159759, #11356, #191171, #61192, #42838, #205288, #108945, #174965, #26547, #158697, #10295, #127351, #193320, #56926, #189056, #195468, #62260, #160830, #82765, #49221, #31905, #115340, #12422, #179220, #181331, #47099, #178155, #211689, #146741, #30845, #50275, #28696, #194388, #96923, #65426, #95854, #145691, #148838, #116394, #130538, #162973, #196529, #14553, #210634, #128421, #410, #29769, #48172, #46031, #112152, #32959, #161910, #13498, #79572, #63325, #80649, #66482, #129486, #131575, #16680, #114285, #198628, #180282, #113215, #94782, #78502, #212759, #144620, #132622, #64394, #97982, #164041, #15616, #81706, #147787, #213803, #197576, #99034, #165089, #153104, #84898, #149916, #19885, #136865, #150985, #35066, #133693, #202891, #20936, #21997, #18811, #185586, #152044, #101137, #134747, #2549, #167225, #68624, #200756, #52405, #166148, #118532, #199697, #54536, #103289, #70753, #51342, #184515, #117467, #83823, #119602, #3614, #36136, #169351, #183460, #5746, #88107, #102219, #71823, #168288, #37216, #34012, #201820, #87032, #85969, #120683, #154178, #69692, #135796, #53465, #4679, #38286, #186660, #104363, #170408, #17734, #137933, #203955, #55602, #182382, #100087, #1484 ) ),
 .UNSPECIFIED., .F., .F., .F. ) 
 B_SPLINE_SURFACE_WITH_KNOTS ( ( 2, 2 ),
 ( 3, 2, 2, 2, 2, 2, 2, 2, 2, 2, 2, 2, 2, 2, 2, 2, 2, 2, 2, 2, 2, 2, 2, 2, 2, 2, 2, 2, 2, 2, 2, 2, 2, 2, 2, 2, 2, 2, 2, 2, 2, 2, 2, 2, 2, 2, 2, 2, 2, 2, 2, 2, 2, 2, 2, 2, 2, 2, 2, 2, 2, 2, 2, 2, 2, 2, 2, 2, 2, 2, 2, 2, 2, 2, 2, 2, 2, 2, 2, 2, 2, 2, 2, 2, 2, 2, 2, 2, 2, 2, 2, 2, 2, 2, 2, 2, 2, 2, 2, 2, 2, 2, 2, 2, 2, 2, 2, 2, 2, 2, 2, 2, 2, 2, 2, 2, 2, 2, 2, 2, 2, 2, 2, 2, 2, 2, 2, 2, 2, 2, 2, 2, 2, 2, 2, 2, 2, 2, 2, 2, 2, 2, 2, 2, 2, 2, 2, 2, 2, 2, 2, 2, 2, 2, 2, 2, 2, 2, 2, 2, 2, 2, 2, 2, 2, 2, 2, 2, 2, 2, 2, 2, 2, 2, 2, 2, 2, 2, 2, 2, 2, 2, 2, 2, 2, 2, 2, 2, 2, 2, 2, 2, 2, 2, 2, 2, 2, 2, 2, 2, 2, 2, 2, 2, 2, 2, 2, 2, 2, 2, 2, 2, 2, 2, 2, 2, 2, 2, 2, 2, 2, 2, 2, 2, 2, 2, 2, 2, 2, 2, 2, 2, 2, 2, 2, 2, 2, 2, 2, 2, 3 ),
 ( 0.000000000000000000, 1.000000000000000000 ),
 ( 0.000000000000000000, 0.004166666666666666609, 0.008333333333333333218, 0.01250000000000000069, 0.01666666666666666644, 0.02083333333333333218, 0.02500000000000000139, 0.02916666666666666713, 0.03333333333333333287, 0.03749999999999999861, 0.04166666666666666435, 0.04583333333333333010, 0.05000000000000000278, 0.05416666666666666852, 0.05833333333333333426, 0.06250000000000000000, 0.06666666666666666574, 0.07083333333333333148, 0.07499999999999999722, 0.07916666666666666297, 0.08333333333333332871, 0.08749999999999999445, 0.09166666666666666019, 0.09583333333333333981, 0.1000000000000000056, 0.1041666666666666713, 0.1083333333333333370, 0.1125000000000000028, 0.1166666666666666685, 0.1208333333333333343, 0.1250000000000000000, 0.1291666666666666796, 0.1333333333333333315, 0.1375000000000000111, 0.1416666666666666630, 0.1458333333333333426, 0.1499999999999999944, 0.1541666666666666741, 0.1583333333333333259, 0.1625000000000000056, 0.1666666666666666574, 0.1708333333333333370, 0.1749999999999999889, 0.1791666666666666685, 0.1833333333333333204, 0.1875000000000000000, 0.1916666666666666796, 0.1958333333333333315, 0.2000000000000000111, 0.2041666666666666630, 0.2083333333333333426, 0.2124999999999999944, 0.2166666666666666741, 0.2208333333333333259, 0.2250000000000000056, 0.2291666666666666574, 0.2333333333333333370, 0.2374999999999999889, 0.2416666666666666685, 0.2458333333333333204, 0.2500000000000000000, 0.2541666666666666519, 0.2583333333333333592, 0.2625000000000000111, 0.2666666666666666630, 0.2708333333333333148, 0.2750000000000000222, 0.2791666666666666741, 0.2833333333333333259, 0.2874999999999999778, 0.2916666666666666852, 0.2958333333333333370, 0.2999999999999999889, 0.3041666666666666408, 0.3083333333333333481, 0.3125000000000000000, 0.3166666666666666519, 0.3208333333333333592, 0.3250000000000000111, 0.3291666666666666630, 0.3333333333333333148, 0.3375000000000000222, 0.3416666666666666741, 0.3458333333333333259, 0.3499999999999999778, 0.3541666666666666852, 0.3583333333333333370, 0.3624999999999999889, 0.3666666666666666408, 0.3708333333333333481, 0.3750000000000000000, 0.3791666666666666519, 0.3833333333333333592, 0.3875000000000000111, 0.3916666666666666630, 0.3958333333333333148, 0.4000000000000000222, 0.4041666666666666741, 0.4083333333333333259, 0.4124999999999999778, 0.4166666666666666852, 0.4208333333333333370, 0.4249999999999999889, 0.4291666666666666408, 0.4333333333333333481, 0.4375000000000000000, 0.4416666666666666519, 0.4458333333333333592, 0.4500000000000000111, 0.4541666666666666630, 0.4583333333333333148, 0.4625000000000000222, 0.4666666666666666741, 0.4708333333333333259, 0.4749999999999999778, 0.4791666666666666852, 0.4833333333333333370, 0.4874999999999999889, 0.4916666666666666408, 0.4958333333333333481, 0.5000000000000000000, 0.5041666666666666519, 0.5083333333333333037, 0.5124999999999999556, 0.5166666666666667185, 0.5208333333333333703, 0.5250000000000000222, 0.5291666666666666741, 0.5333333333333333259, 0.5374999999999999778, 0.5416666666666666297, 0.5458333333333332815, 0.5500000000000000444, 0.5541666666666666963, 0.5583333333333333481, 0.5625000000000000000, 0.5666666666666666519, 0.5708333333333333037, 0.5749999999999999556, 0.5791666666666667185, 0.5833333333333333703, 0.5875000000000000222, 0.5916666666666666741, 0.5958333333333333259, 0.5999999999999999778, 0.6041666666666666297, 0.6083333333333332815, 0.6125000000000000444, 0.6166666666666666963, 0.6208333333333333481, 0.6250000000000000000, 0.6291666666666666519, 0.6333333333333333037, 0.6374999999999999556, 0.6416666666666667185, 0.6458333333333333703, 0.6500000000000000222, 0.6541666666666666741, 0.6583333333333333259, 0.6624999999999999778, 0.6666666666666666297, 0.6708333333333332815, 0.6750000000000000444, 0.6791666666666666963, 0.6833333333333333481, 0.6875000000000000000, 0.6916666666666666519, 0.6958333333333333037, 0.6999999999999999556, 0.7041666666666667185, 0.7083333333333333703, 0.7125000000000000222, 0.7166666666666666741, 0.7208333333333333259, 0.7249999999999999778, 0.7291666666666666297, 0.7333333333333332815, 0.7375000000000000444, 0.7416666666666666963, 0.7458333333333333481, 0.7500000000000000000, 0.7541666666666666519, 0.7583333333333333037, 0.7624999999999999556, 0.7666666666666667185, 0.7708333333333333703, 0.7750000000000000222, 0.7791666666666666741, 0.7833333333333333259, 0.7874999999999999778, 0.7916666666666666297, 0.7958333333333332815, 0.8000000000000000444, 0.8041666666666666963, 0.8083333333333333481, 0.8125000000000000000, 0.8166666666666666519, 0.8208333333333333037, 0.8249999999999999556, 0.8291666666666667185, 0.8333333333333333703, 0.8375000000000000222, 0.8416666666666666741, 0.8458333333333333259, 0.8499999999999999778, 0.8541666666666666297, 0.8583333333333332815, 0.8625000000000000444, 0.8666666666666666963, 0.8708333333333333481, 0.8750000000000000000, 0.8791666666666666519, 0.8833333333333333037, 0.8874999999999999556, 0.8916666666666667185, 0.8958333333333333703, 0.9000000000000000222, 0.9041666666666666741, 0.9083333333333333259, 0.9124999999999999778, 0.9166666666666666297, 0.9208333333333332815, 0.9250000000000000444, 0.9291666666666666963, 0.9333333333333333481, 0.9375000000000000000, 0.9416666666666666519, 0.9458333333333333037, 0.9499999999999999556, 0.9541666666666667185, 0.9583333333333333703, 0.9625000000000000222, 0.9666666666666666741, 0.9708333333333333259, 0.9749999999999999778, 0.9791666666666666297, 0.9833333333333332815, 0.9875000000000000444, 0.9916666666666666963, 0.9958333333333333481, 1.000000000000000000 ),
 .UNSPECIFIED. ) 
 GEOMETRIC_REPRESENTATION_ITEM ( )  RATIONAL_B_SPLINE_SURFACE ( (
 ( 1.000000000000000000, 0.8660254037844387076, 1.000000000000000000, 0.8660254037844387076, 1.000000000000000000, 0.8660254037844387076, 1.000000000000000000, 0.8660254037844387076, 1.000000000000000000, 0.8660254037844387076, 1.000000000000000000, 0.8660254037844387076, 1.000000000000000000, 0.8660254037844387076, 1.000000000000000000, 0.8660254037844387076, 1.000000000000000000, 0.8660254037844387076, 1.000000000000000000, 0.8660254037844387076, 1.000000000000000000, 0.8660254037844387076, 1.000000000000000000, 0.8660254037844387076, 1.000000000000000000, 0.8660254037844387076, 1.000000000000000000, 0.8660254037844387076, 1.000000000000000000, 0.8660254037844387076, 1.000000000000000000, 0.8660254037844387076, 1.000000000000000000, 0.8660254037844387076, 1.000000000000000000, 0.8660254037844387076, 1.000000000000000000, 0.8660254037844387076, 1.000000000000000000, 0.8660254037844387076, 1.000000000000000000, 0.8660254037844387076, 1.000000000000000000, 0.8660254037844387076, 1.000000000000000000, 0.8660254037844387076, 1.000000000000000000, 0.8660254037844387076, 1.000000000000000000, 0.8660254037844387076, 1.000000000000000000, 0.8660254037844387076, 1.000000000000000000, 0.8660254037844387076, 1.000000000000000000, 0.8660254037844387076, 1.000000000000000000, 0.8660254037844387076, 1.000000000000000000, 0.8660254037844387076, 1.000000000000000000, 0.8660254037844387076, 1.000000000000000000, 0.8660254037844387076, 1.000000000000000000, 0.8660254037844387076, 1.000000000000000000, 0.8660254037844387076, 1.000000000000000000, 0.8660254037844387076, 1.000000000000000000, 0.8660254037844387076, 1.000000000000000000, 0.8660254037844387076, 1.000000000000000000, 0.8660254037844387076, 1.000000000000000000, 0.8660254037844387076, 1.000000000000000000, 0.8660254037844387076, 1.000000000000000000, 0.8660254037844387076, 1.000000000000000000, 0.8660254037844387076, 1.000000000000000000, 0.8660254037844387076, 1.000000000000000000, 0.8660254037844387076, 1.000000000000000000, 0.8660254037844387076, 1.000000000000000000, 0.8660254037844387076, 1.000000000000000000, 0.8660254037844387076, 1.000000000000000000, 0.8660254037844387076, 1.000000000000000000, 0.8660254037844387076, 1.000000000000000000, 0.8660254037844387076, 1.000000000000000000, 0.8660254037844387076, 1.000000000000000000, 0.8660254037844387076, 1.000000000000000000, 0.8660254037844387076, 1.000000000000000000, 0.8660254037844387076, 1.000000000000000000, 0.8660254037844387076, 1.000000000000000000, 0.8660254037844387076, 1.000000000000000000, 0.8660254037844387076, 1.000000000000000000, 0.8660254037844387076, 1.000000000000000000, 0.8660254037844387076, 1.000000000000000000, 0.8660254037844387076, 1.000000000000000000, 0.8660254037844387076, 1.000000000000000000, 0.8660254037844387076, 1.000000000000000000, 0.8660254037844387076, 1.000000000000000000, 0.8660254037844387076, 1.000000000000000000, 0.8660254037844387076, 1.000000000000000000, 0.8660254037844387076, 1.000000000000000000, 0.8660254037844387076, 1.000000000000000000, 0.8660254037844387076, 1.000000000000000000, 0.8660254037844387076, 1.000000000000000000, 0.8660254037844387076, 1.000000000000000000, 0.8660254037844387076, 1.000000000000000000, 0.8660254037844387076, 1.000000000000000000, 0.8660254037844387076, 1.000000000000000000, 0.8660254037844387076, 1.000000000000000000, 0.8660254037844387076, 1.000000000000000000, 0.8660254037844387076, 1.000000000000000000, 0.8660254037844387076, 1.000000000000000000, 0.8660254037844387076, 1.000000000000000000, 0.8660254037844387076, 1.000000000000000000, 0.8660254037844387076, 1.000000000000000000, 0.8660254037844387076, 1.000000000000000000, 0.8660254037844387076, 1.000000000000000000, 0.8660254037844387076, 1.000000000000000000, 0.8660254037844387076, 1.000000000000000000, 0.8660254037844387076, 1.000000000000000000, 0.8660254037844387076, 1.000000000000000000, 0.8660254037844387076, 1.000000000000000000, 0.8660254037844387076, 1.000000000000000000, 0.8660254037844387076, 1.000000000000000000, 0.8660254037844387076, 1.000000000000000000, 0.8660254037844387076, 1.000000000000000000, 0.8660254037844387076, 1.000000000000000000, 0.8660254037844387076, 1.000000000000000000, 0.8660254037844387076, 1.000000000000000000, 0.8660254037844387076, 1.000000000000000000, 0.8660254037844387076, 1.000000000000000000, 0.8660254037844387076, 1.000000000000000000, 0.8660254037844387076, 1.000000000000000000, 0.8660254037844387076, 1.000000000000000000, 0.8660254037844387076, 1.000000000000000000, 0.8660254037844387076, 1.000000000000000000, 0.8660254037844387076, 1.000000000000000000, 0.8660254037844387076, 1.000000000000000000, 0.8660254037844387076, 1.000000000000000000, 0.8660254037844387076, 1.000000000000000000, 0.8660254037844387076, 1.000000000000000000, 0.8660254037844387076, 1.000000000000000000, 0.8660254037844387076, 1.000000000000000000, 0.8660254037844387076, 1.000000000000000000, 0.8660254037844387076, 1.000000000000000000, 0.8660254037844387076, 1.000000000000000000, 0.8660254037844387076, 1.000000000000000000, 0.8660254037844387076, 1.000000000000000000, 0.8660254037844387076, 1.000000000000000000, 0.8660254037844387076, 1.000000000000000000, 0.8660254037844387076, 1.000000000000000000, 0.8660254037844387076, 1.000000000000000000, 0.8660254037844387076, 1.000000000000000000, 0.8660254037844387076, 1.000000000000000000, 0.8660254037844387076, 1.000000000000000000, 0.8660254037844387076, 1.000000000000000000, 0.8660254037844387076, 1.000000000000000000, 0.8660254037844387076, 1.000000000000000000, 0.8660254037844387076, 1.000000000000000000, 0.8660254037844387076, 1.000000000000000000, 0.8660254037844387076, 1.000000000000000000, 0.8660254037844387076, 1.000000000000000000, 0.8660254037844387076, 1.000000000000000000, 0.8660254037844387076, 1.000000000000000000, 0.8660254037844387076, 1.000000000000000000, 0.8660254037844387076, 1.000000000000000000, 0.8660254037844387076, 1.000000000000000000, 0.8660254037844387076, 1.000000000000000000, 0.8660254037844387076, 1.000000000000000000, 0.8660254037844387076, 1.000000000000000000, 0.8660254037844387076, 1.000000000000000000, 0.8660254037844387076, 1.000000000000000000, 0.8660254037844387076, 1.000000000000000000, 0.8660254037844387076, 1.000000000000000000, 0.8660254037844387076, 1.000000000000000000, 0.8660254037844387076, 1.000000000000000000, 0.8660254037844387076, 1.000000000000000000, 0.8660254037844387076, 1.000000000000000000, 0.8660254037844387076, 1.000000000000000000, 0.8660254037844387076, 1.000000000000000000, 0.8660254037844387076, 1.000000000000000000, 0.8660254037844387076, 1.000000000000000000, 0.8660254037844387076, 1.000000000000000000, 0.8660254037844387076, 1.000000000000000000, 0.8660254037844387076, 1.000000000000000000, 0.8660254037844387076, 1.000000000000000000, 0.8660254037844387076, 1.000000000000000000, 0.8660254037844387076, 1.000000000000000000, 0.8660254037844387076, 1.000000000000000000, 0.8660254037844387076, 1.000000000000000000, 0.8660254037844387076, 1.000000000000000000, 0.8660254037844387076, 1.000000000000000000, 0.8660254037844387076, 1.000000000000000000, 0.8660254037844387076, 1.000000000000000000, 0.8660254037844387076, 1.000000000000000000, 0.8660254037844387076, 1.000000000000000000, 0.8660254037844387076, 1.000000000000000000, 0.8660254037844387076, 1.000000000000000000, 0.8660254037844387076, 1.000000000000000000, 0.8660254037844387076, 1.000000000000000000, 0.8660254037844387076, 1.000000000000000000, 0.8660254037844387076, 1.000000000000000000, 0.8660254037844387076, 1.000000000000000000, 0.8660254037844387076, 1.000000000000000000, 0.8660254037844387076, 1.000000000000000000, 0.8660254037844387076, 1.000000000000000000, 0.8660254037844387076, 1.000000000000000000, 0.8660254037844387076, 1.000000000000000000, 0.8660254037844387076, 1.000000000000000000, 0.8660254037844387076, 1.000000000000000000, 0.8660254037844387076, 1.000000000000000000, 0.8660254037844387076, 1.000000000000000000, 0.8660254037844387076, 1.000000000000000000, 0.8660254037844387076, 1.000000000000000000, 0.8660254037844387076, 1.000000000000000000, 0.8660254037844387076, 1.000000000000000000, 0.8660254037844387076, 1.000000000000000000, 0.8660254037844387076, 1.000000000000000000, 0.8660254037844387076, 1.000000000000000000, 0.8660254037844387076, 1.000000000000000000, 0.8660254037844387076, 1.000000000000000000, 0.8660254037844387076, 1.000000000000000000, 0.8660254037844387076, 1.000000000000000000, 0.8660254037844387076, 1.000000000000000000, 0.8660254037844387076, 1.000000000000000000, 0.8660254037844387076, 1.000000000000000000, 0.8660254037844387076, 1.000000000000000000, 0.8660254037844387076, 1.000000000000000000, 0.8660254037844387076, 1.000000000000000000, 0.8660254037844387076, 1.000000000000000000, 0.8660254037844387076, 1.000000000000000000, 0.8660254037844387076, 1.000000000000000000, 0.8660254037844387076, 1.000000000000000000, 0.8660254037844387076, 1.000000000000000000, 0.8660254037844387076, 1.000000000000000000, 0.8660254037844387076, 1.000000000000000000, 0.8660254037844387076, 1.000000000000000000, 0.8660254037844387076, 1.000000000000000000, 0.8660254037844387076, 1.000000000000000000, 0.8660254037844387076, 1.000000000000000000, 0.8660254037844387076, 1.000000000000000000, 0.8660254037844387076, 1.000000000000000000, 0.8660254037844387076, 1.000000000000000000, 0.8660254037844387076, 1.000000000000000000, 0.8660254037844387076, 1.000000000000000000, 0.8660254037844387076, 1.000000000000000000, 0.8660254037844387076, 1.000000000000000000, 0.8660254037844387076, 1.000000000000000000, 0.8660254037844387076, 1.000000000000000000, 0.8660254037844387076, 1.000000000000000000, 0.8660254037844387076, 1.000000000000000000, 0.8660254037844387076, 1.000000000000000000, 0.8660254037844387076, 1.000000000000000000, 0.8660254037844387076, 1.000000000000000000, 0.8660254037844387076, 1.000000000000000000, 0.8660254037844387076, 1.000000000000000000, 0.8660254037844387076, 1.000000000000000000, 0.8660254037844387076, 1.000000000000000000, 0.8660254037844387076, 1.000000000000000000, 0.8660254037844387076, 1.000000000000000000, 0.8660254037844387076, 1.000000000000000000, 0.8660254037844387076, 1.000000000000000000, 0.8660254037844387076, 1.000000000000000000, 0.8660254037844387076, 1.000000000000000000, 0.8660254037844387076, 1.000000000000000000, 0.8660254037844387076, 1.000000000000000000, 0.8660254037844387076, 1.000000000000000000, 0.8660254037844387076, 1.000000000000000000, 0.8660254037844387076, 1.000000000000000000, 0.8660254037844387076, 1.000000000000000000, 0.8660254037844387076, 1.000000000000000000, 0.8660254037844387076, 1.000000000000000000, 0.8660254037844387076, 1.000000000000000000, 0.8660254037844387076, 1.000000000000000000, 0.8660254037844387076, 1.000000000000000000),
 ( 1.000000000000000000, 0.8660254037844387076, 1.000000000000000000, 0.8660254037844387076, 1.000000000000000000, 0.8660254037844387076, 1.000000000000000000, 0.8660254037844387076, 1.000000000000000000, 0.8660254037844387076, 1.000000000000000000, 0.8660254037844387076, 1.000000000000000000, 0.8660254037844387076, 1.000000000000000000, 0.8660254037844387076, 1.000000000000000000, 0.8660254037844387076, 1.000000000000000000, 0.8660254037844387076, 1.000000000000000000, 0.8660254037844387076, 1.000000000000000000, 0.8660254037844387076, 1.000000000000000000, 0.8660254037844387076, 1.000000000000000000, 0.8660254037844387076, 1.000000000000000000, 0.8660254037844387076, 1.000000000000000000, 0.8660254037844387076, 1.000000000000000000, 0.8660254037844387076, 1.000000000000000000, 0.8660254037844387076, 1.000000000000000000, 0.8660254037844387076, 1.000000000000000000, 0.8660254037844387076, 1.000000000000000000, 0.8660254037844387076, 1.000000000000000000, 0.8660254037844387076, 1.000000000000000000, 0.8660254037844387076, 1.000000000000000000, 0.8660254037844387076, 1.000000000000000000, 0.8660254037844387076, 1.000000000000000000, 0.8660254037844387076, 1.000000000000000000, 0.8660254037844387076, 1.000000000000000000, 0.8660254037844387076, 1.000000000000000000, 0.8660254037844387076, 1.000000000000000000, 0.8660254037844387076, 1.000000000000000000, 0.8660254037844387076, 1.000000000000000000, 0.8660254037844387076, 1.000000000000000000, 0.8660254037844387076, 1.000000000000000000, 0.8660254037844387076, 1.000000000000000000, 0.8660254037844387076, 1.000000000000000000, 0.8660254037844387076, 1.000000000000000000, 0.8660254037844387076, 1.000000000000000000, 0.8660254037844387076, 1.000000000000000000, 0.8660254037844387076, 1.000000000000000000, 0.8660254037844387076, 1.000000000000000000, 0.8660254037844387076, 1.000000000000000000, 0.8660254037844387076, 1.000000000000000000, 0.8660254037844387076, 1.000000000000000000, 0.8660254037844387076, 1.000000000000000000, 0.8660254037844387076, 1.000000000000000000, 0.8660254037844387076, 1.000000000000000000, 0.8660254037844387076, 1.000000000000000000, 0.8660254037844387076, 1.000000000000000000, 0.8660254037844387076, 1.000000000000000000, 0.8660254037844387076, 1.000000000000000000, 0.8660254037844387076, 1.000000000000000000, 0.8660254037844387076, 1.000000000000000000, 0.8660254037844387076, 1.000000000000000000, 0.8660254037844387076, 1.000000000000000000, 0.8660254037844387076, 1.000000000000000000, 0.8660254037844387076, 1.000000000000000000, 0.8660254037844387076, 1.000000000000000000, 0.8660254037844387076, 1.000000000000000000, 0.8660254037844387076, 1.000000000000000000, 0.8660254037844387076, 1.000000000000000000, 0.8660254037844387076, 1.000000000000000000, 0.8660254037844387076, 1.000000000000000000, 0.8660254037844387076, 1.000000000000000000, 0.8660254037844387076, 1.000000000000000000, 0.8660254037844387076, 1.000000000000000000, 0.8660254037844387076, 1.000000000000000000, 0.8660254037844387076, 1.000000000000000000, 0.8660254037844387076, 1.000000000000000000, 0.8660254037844387076, 1.000000000000000000, 0.8660254037844387076, 1.000000000000000000, 0.8660254037844387076, 1.000000000000000000, 0.8660254037844387076, 1.000000000000000000, 0.8660254037844387076, 1.000000000000000000, 0.8660254037844387076, 1.000000000000000000, 0.8660254037844387076, 1.000000000000000000, 0.8660254037844387076, 1.000000000000000000, 0.8660254037844387076, 1.000000000000000000, 0.8660254037844387076, 1.000000000000000000, 0.8660254037844387076, 1.000000000000000000, 0.8660254037844387076, 1.000000000000000000, 0.8660254037844387076, 1.000000000000000000, 0.8660254037844387076, 1.000000000000000000, 0.8660254037844387076, 1.000000000000000000, 0.8660254037844387076, 1.000000000000000000, 0.8660254037844387076, 1.000000000000000000, 0.8660254037844387076, 1.000000000000000000, 0.8660254037844387076, 1.000000000000000000, 0.8660254037844387076, 1.000000000000000000, 0.8660254037844387076, 1.000000000000000000, 0.8660254037844387076, 1.000000000000000000, 0.8660254037844387076, 1.000000000000000000, 0.8660254037844387076, 1.000000000000000000, 0.8660254037844387076, 1.000000000000000000, 0.8660254037844387076, 1.000000000000000000, 0.8660254037844387076, 1.000000000000000000, 0.8660254037844387076, 1.000000000000000000, 0.8660254037844387076, 1.000000000000000000, 0.8660254037844387076, 1.000000000000000000, 0.8660254037844387076, 1.000000000000000000, 0.8660254037844387076, 1.000000000000000000, 0.8660254037844387076, 1.000000000000000000, 0.8660254037844387076, 1.000000000000000000, 0.8660254037844387076, 1.000000000000000000, 0.8660254037844387076, 1.000000000000000000, 0.8660254037844387076, 1.000000000000000000, 0.8660254037844387076, 1.000000000000000000, 0.8660254037844387076, 1.000000000000000000, 0.8660254037844387076, 1.000000000000000000, 0.8660254037844387076, 1.000000000000000000, 0.8660254037844387076, 1.000000000000000000, 0.8660254037844387076, 1.000000000000000000, 0.8660254037844387076, 1.000000000000000000, 0.8660254037844387076, 1.000000000000000000, 0.8660254037844387076, 1.000000000000000000, 0.8660254037844387076, 1.000000000000000000, 0.8660254037844387076, 1.000000000000000000, 0.8660254037844387076, 1.000000000000000000, 0.8660254037844387076, 1.000000000000000000, 0.8660254037844387076, 1.000000000000000000, 0.8660254037844387076, 1.000000000000000000, 0.8660254037844387076, 1.000000000000000000, 0.8660254037844387076, 1.000000000000000000, 0.8660254037844387076, 1.000000000000000000, 0.8660254037844387076, 1.000000000000000000, 0.8660254037844387076, 1.000000000000000000, 0.8660254037844387076, 1.000000000000000000, 0.8660254037844387076, 1.000000000000000000, 0.8660254037844387076, 1.000000000000000000, 0.8660254037844387076, 1.000000000000000000, 0.8660254037844387076, 1.000000000000000000, 0.8660254037844387076, 1.000000000000000000, 0.8660254037844387076, 1.000000000000000000, 0.8660254037844387076, 1.000000000000000000, 0.8660254037844387076, 1.000000000000000000, 0.8660254037844387076, 1.000000000000000000, 0.8660254037844387076, 1.000000000000000000, 0.8660254037844387076, 1.000000000000000000, 0.8660254037844387076, 1.000000000000000000, 0.8660254037844387076, 1.000000000000000000, 0.8660254037844387076, 1.000000000000000000, 0.8660254037844387076, 1.000000000000000000, 0.8660254037844387076, 1.000000000000000000, 0.8660254037844387076, 1.000000000000000000, 0.8660254037844387076, 1.000000000000000000, 0.8660254037844387076, 1.000000000000000000, 0.8660254037844387076, 1.000000000000000000, 0.8660254037844387076, 1.000000000000000000, 0.8660254037844387076, 1.000000000000000000, 0.8660254037844387076, 1.000000000000000000, 0.8660254037844387076, 1.000000000000000000, 0.8660254037844387076, 1.000000000000000000, 0.8660254037844387076, 1.000000000000000000, 0.8660254037844387076, 1.000000000000000000, 0.8660254037844387076, 1.000000000000000000, 0.8660254037844387076, 1.000000000000000000, 0.8660254037844387076, 1.000000000000000000, 0.8660254037844387076, 1.000000000000000000, 0.8660254037844387076, 1.000000000000000000, 0.8660254037844387076, 1.000000000000000000, 0.8660254037844387076, 1.000000000000000000, 0.8660254037844387076, 1.000000000000000000, 0.8660254037844387076, 1.000000000000000000, 0.8660254037844387076, 1.000000000000000000, 0.8660254037844387076, 1.000000000000000000, 0.8660254037844387076, 1.000000000000000000, 0.8660254037844387076, 1.000000000000000000, 0.8660254037844387076, 1.000000000000000000, 0.8660254037844387076, 1.000000000000000000, 0.8660254037844387076, 1.000000000000000000, 0.8660254037844387076, 1.000000000000000000, 0.8660254037844387076, 1.000000000000000000, 0.8660254037844387076, 1.000000000000000000, 0.8660254037844387076, 1.000000000000000000, 0.8660254037844387076, 1.000000000000000000, 0.8660254037844387076, 1.000000000000000000, 0.8660254037844387076, 1.000000000000000000, 0.8660254037844387076, 1.000000000000000000, 0.8660254037844387076, 1.000000000000000000, 0.8660254037844387076, 1.000000000000000000, 0.8660254037844387076, 1.000000000000000000, 0.8660254037844387076, 1.000000000000000000, 0.8660254037844387076, 1.000000000000000000, 0.8660254037844387076, 1.000000000000000000, 0.8660254037844387076, 1.000000000000000000, 0.8660254037844387076, 1.000000000000000000, 0.8660254037844387076, 1.000000000000000000, 0.8660254037844387076, 1.000000000000000000, 0.8660254037844387076, 1.000000000000000000, 0.8660254037844387076, 1.000000000000000000, 0.8660254037844387076, 1.000000000000000000, 0.8660254037844387076, 1.000000000000000000, 0.8660254037844387076, 1.000000000000000000, 0.8660254037844387076, 1.000000000000000000, 0.8660254037844387076, 1.000000000000000000, 0.8660254037844387076, 1.000000000000000000, 0.8660254037844387076, 1.000000000000000000, 0.8660254037844387076, 1.000000000000000000, 0.8660254037844387076, 1.000000000000000000, 0.8660254037844387076, 1.000000000000000000, 0.8660254037844387076, 1.000000000000000000, 0.8660254037844387076, 1.000000000000000000, 0.8660254037844387076, 1.000000000000000000, 0.8660254037844387076, 1.000000000000000000, 0.8660254037844387076, 1.000000000000000000, 0.8660254037844387076, 1.000000000000000000, 0.8660254037844387076, 1.000000000000000000, 0.8660254037844387076, 1.000000000000000000, 0.8660254037844387076, 1.000000000000000000, 0.8660254037844387076, 1.000000000000000000, 0.8660254037844387076, 1.000000000000000000, 0.8660254037844387076, 1.000000000000000000, 0.8660254037844387076, 1.000000000000000000, 0.8660254037844387076, 1.000000000000000000, 0.8660254037844387076, 1.000000000000000000, 0.8660254037844387076, 1.000000000000000000, 0.8660254037844387076, 1.000000000000000000, 0.8660254037844387076, 1.000000000000000000, 0.8660254037844387076, 1.000000000000000000, 0.8660254037844387076, 1.000000000000000000, 0.8660254037844387076, 1.000000000000000000, 0.8660254037844387076, 1.000000000000000000, 0.8660254037844387076, 1.000000000000000000, 0.8660254037844387076, 1.000000000000000000, 0.8660254037844387076, 1.000000000000000000, 0.8660254037844387076, 1.000000000000000000, 0.8660254037844387076, 1.000000000000000000, 0.8660254037844387076, 1.000000000000000000, 0.8660254037844387076, 1.000000000000000000, 0.8660254037844387076, 1.000000000000000000, 0.8660254037844387076, 1.000000000000000000, 0.8660254037844387076, 1.000000000000000000, 0.8660254037844387076, 1.000000000000000000, 0.8660254037844387076, 1.000000000000000000, 0.8660254037844387076, 1.000000000000000000, 0.8660254037844387076, 1.000000000000000000, 0.8660254037844387076, 1.000000000000000000, 0.8660254037844387076, 1.000000000000000000, 0.8660254037844387076, 1.000000000000000000, 0.8660254037844387076, 1.000000000000000000, 0.8660254037844387076, 1.000000000000000000) ) ) 
 REPRESENTATION_ITEM ( '' )  SURFACE ( )  );
#73262 = CARTESIAN_POINT ( 'NONE',  ( 9.284636267260101050, 9.726497154758602548, -0.7998128361456281477 ) ) ;
#73263 = CARTESIAN_POINT ( 'NONE',  ( 5.494608840674215955, 2.039112051642687717, 0.3575134270455831986 ) ) ;
#73264 = DIRECTION ( 'NONE',  ( 0.000000000000000000, 0.000000000000000000, -1.000000000000000000 ) ) ;
#73265 = CARTESIAN_POINT ( 'NONE',  ( 6.392125918040960642, -0.5824770489515176397, -2.112646119873210271 ) ) ;
#73266 = CARTESIAN_POINT ( 'NONE',  ( 5.316739912341137853, 7.735632174496787528, -1.307268462668280673 ) ) ;
#73267 = EDGE_LOOP ( 'NONE', ( #201513, #31683, #107170, #137885 ) ) ;
#73268 = AXIS2_PLACEMENT_3D ( 'NONE', #65011, #164665, #83395 ) ;
#73269 = CARTESIAN_POINT ( 'NONE',  ( 3.810548893104170887, 8.469546410357008170, -2.500000000000001776 ) ) ;
#73270 = EDGE_CURVE ( 'NONE', #104869, #104455, #210369, .T. ) ;
#73271 = CARTESIAN_POINT ( 'NONE',  ( 5.598591087800349086, 5.496387455380669529, -0.7998128361456481317 ) ) ;
#73272 = CARTESIAN_POINT ( 'NONE',  ( -3.285556943750000514, -1.976041666188710577, -1.896917185911906722 ) ) ;
#73273 = CARTESIAN_POINT ( 'NONE',  ( -6.966220764712169000, 6.002124920821316323, -2.420000000000000373 ) ) ;
#73274 = CARTESIAN_POINT ( 'NONE',  ( -8.202319746587722449, 8.671720580548228696, 1.040834085586084257E-14 ) ) ;
#73275 = CARTESIAN_POINT ( 'NONE',  ( 3.739016502318667445, 7.584212696005614873, 0.7998128361456271485 ) ) ;
#73276 = CARTESIAN_POINT ( 'NONE',  ( 5.911005882915712384, -1.635593682349820721, 1.269112435710928688 ) ) ;
#73277 = CARTESIAN_POINT ( 'NONE',  ( 4.775960602080351336, 1.110526314841601359, 1.574030653434669746 ) ) ;
#73278 = CARTESIAN_POINT ( 'NONE',  ( 1.370720498019749378, -0.2986500928384462350, -1.994069080148860973 ) ) ;
#73279 = CARTESIAN_POINT ( 'NONE',  ( -9.982881178363895103, 10.54111621771303753, 1.040834085586084257E-14 ) ) ;
#73280 = CARTESIAN_POINT ( 'NONE',  ( 4.947799714344386146, 4.737130853015369958, -0.7998128361456481317 ) ) ;
#73281 = CARTESIAN_POINT ( 'NONE',  ( -0.5445930744354000597, 3.250057683544679943, -0.4000000000000062395 ) ) ;
#73282 = CARTESIAN_POINT ( 'NONE',  ( 1.377182423176852133, 2.023737929115625445, -0.8412682346608522099 ) ) ;
#73283 = CARTESIAN_POINT ( 'NONE',  ( 5.654876981934024549, -1.436564326775534806, 1.126588154728463742 ) ) ;
#73284 = EDGE_CURVE ( 'NONE', #164674, #213687, #127588, .T. ) ;
#73285 = CARTESIAN_POINT ( 'NONE',  ( 4.584065335196252811, 8.362176967788721882, 0.7216878364870328300 ) ) ;
#73286 = CARTESIAN_POINT ( 'NONE',  ( 4.189106276498237413, 3.989638198777126110, -0.7216878364870188411 ) ) ;
#73287 = CARTESIAN_POINT ( 'NONE',  ( -4.633854640820660009, 8.628190524257904670, -0.7998128361456362523 ) ) ;
#73288 = CARTESIAN_POINT ( 'NONE',  ( 4.813308228051395687, 5.574280006603454574, 1.199719254218462483 ) ) ;
#73289 = CARTESIAN_POINT ( 'NONE',  ( 6.034787771858531435, 10.05468647722803865, 0.000000000000000000 ) ) ;
#73290 = VERTEX_POINT ( 'NONE', #181077 ) ;
#73292 = CARTESIAN_POINT ( 'NONE',  ( 6.293232695293600187, -0.1032093112793490142, -2.010699630015537309 ) ) ;
#73291 = CARTESIAN_POINT ( 'NONE',  ( 2.753256032281672372, 1.832158412346639453, -0.1828795585285883096 ) ) ;
#73293 = CARTESIAN_POINT ( 'NONE',  ( 2.443060400399544196, 1.412781429710145975, 1.812861393458516268 ) ) ;
#73294 = CARTESIAN_POINT ( 'NONE',  ( 6.930524233185829885, -1.209519613549964845, 1.545115813350018241 ) ) ;
#73295 = CARTESIAN_POINT ( 'NONE',  ( -6.254388934605767503, 6.191208599995166040, 0.7998128361456341429 ) ) ;
#73296 = CARTESIAN_POINT ( 'NONE',  ( -6.935047222998407257, -6.682123388833687727, 6.658747417465787244 ) ) ;
#73297 = CARTESIAN_POINT ( 'NONE',  ( 2.900541297466651347, -1.884798985816903860, -0.3226963764228693576 ) ) ;
#73298 = B_SPLINE_CURVE_WITH_KNOTS ( 'NONE', 3,
 ( #13574, #64469, #193398, #146813, #180351, #128495, #213878, #99108, #95928, #78575, #210708, #161984, #197649, #14628, #179299, #195540 ),
 .UNSPECIFIED., .F., .F.,
 ( 4, 3, 3, 3, 3, 4 ),
 ( 6.327738642270367575E-19, 5.045320844140702436E-05, 9.514731479413830913E-05, 0.0001285019506255545335, 0.0001554096905450522809, 0.0001555421464865875856 ),
 .UNSPECIFIED. ) ;
#73299 = CARTESIAN_POINT ( 'NONE',  ( -9.969323024750229578, 10.52529837183042716, -0.7998128361456291469 ) ) ;
#73300 = CARTESIAN_POINT ( 'NONE',  ( 0.1392002015415672034, -0.1474423581745692435, -2.037351525059682977 ) ) ;
#73301 = CARTESIAN_POINT ( 'NONE',  ( -3.135678666510573365, 6.880318554229450712, 0.000000000000000000 ) ) ;
#73303 = CARTESIAN_POINT ( 'NONE',  ( 0.7779422811538607707, -1.042605501850740080, 1.552959968518424771 ) ) ;
#73302 = CARTESIAN_POINT ( 'NONE',  ( 3.034800296023100419, -1.842769725714489493, 0.9876625208589999705 ) ) ;
#73304 = CARTESIAN_POINT ( 'NONE',  ( 1.862657450031137474, -0.6818942500997280387, 1.897406292459068222 ) ) ;
#73305 = CARTESIAN_POINT ( 'NONE',  ( 6.778713617152772208, 10.85232362007950258, -0.7216878364870267237 ) ) ;
#73306 = ORIENTED_EDGE ( 'NONE', *, *, #181995, .F. ) ;
#73307 = CARTESIAN_POINT ( 'NONE',  ( -1.364683531250010740, 4.342708333674753618, 0.7879004041258379498 ) ) ;
#73308 = CARTESIAN_POINT ( 'NONE',  ( 2.050002923743666550, -1.344770872215072632, 1.104816081682137963 ) ) ;
#73309 = CARTESIAN_POINT ( 'NONE',  ( 5.497994985541524215, 6.373081223675282736, -1.199719254218445830 ) ) ;
#73311 = CARTESIAN_POINT ( 'NONE',  ( 0.1003079426142767377, 3.401198454231973756, -1.999680697241537741 ) ) ;
#73310 = CYLINDRICAL_SURFACE ( 'NONE', #27112, 0.09999999999999971412 ) ;
#73312 = CARTESIAN_POINT ( 'NONE',  ( 2.455304126353729188, 0.4608866456157869607, -1.662088558372651903 ) ) ;
#73313 = CARTESIAN_POINT ( 'NONE',  ( 2.542740116143254792, -1.820367712357463974, 1.220030464664762393 ) ) ;
#73314 = CARTESIAN_POINT ( 'NONE',  ( 4.811249113497881424, 1.919052844561389692, 1.089612025192594258 ) ) ;
#73315 = CARTESIAN_POINT ( 'NONE',  ( -9.956244568750863166, 5.504298494775027528, -6.025958004757996811 ) ) ;
#73316 = CARTESIAN_POINT ( 'NONE',  ( 2.395604216770229833, -1.940863096919882569, 0.9729980962204368700 ) ) ;
#73317 = CARTESIAN_POINT ( 'NONE',  ( 0.5744775230259161480, -1.718042477583326066, -0.6180270036199516648 ) ) ;
#73318 = CARTESIAN_POINT ( 'NONE',  ( 1.492665153618401241, 8.694790292836037437, -2.590406265390448048 ) ) ;
#73319 = CARTESIAN_POINT ( 'NONE',  ( 4.083301318022297899, 1.702923931485133879, 1.258099284506300153 ) ) ;
#73320 = DIRECTION ( 'NONE',  ( 0.1510067114093955887, 0.000000000000000000, 0.9885327375000383388 ) ) ;
#73321 = ADVANCED_FACE ( 'NONE', ( #14289 ), #161651, .F. ) ;
#73322 = ORIENTED_EDGE ( 'NONE', *, *, #196415, .T. ) ;
#73324 = CARTESIAN_POINT ( 'NONE',  ( 1.364683531249988757, 0.6968750003414209138, 0.000000000000000000 ) ) ;
#73323 = CARTESIAN_POINT ( 'NONE',  ( 5.214511053166543064, 2.117144789807279270, 0.8794703464902029477 ) ) ;
#73325 = LINE ( 'NONE', #189225, #67473 ) ;
#73326 = CARTESIAN_POINT ( 'NONE',  ( 10.71502147350184231, 11.39527989537399755, 0.000000000000000000 ) ) ;
#73327 = CARTESIAN_POINT ( 'NONE',  ( 6.621772978582266767, -0.4938884631311352691, 2.173981893038397839 ) ) ;
#73328 = CARTESIAN_POINT ( 'NONE',  ( -5.585596099150191840, 7.539614753807099667, -1.443375672974052559 ) ) ;
#73329 = CARTESIAN_POINT ( 'NONE',  ( 4.690757960648231695, 5.535267711253469614, 1.082531754730560403 ) ) ;
#73330 = CARTESIAN_POINT ( 'NONE',  ( -7.171900071504754060, 7.469564292951421436, -0.7216878364870267237 ) ) ;
#73331 = CARTESIAN_POINT ( 'NONE',  ( 5.072158865288245444, 5.090142562357324429, 0.7216878364870338292 ) ) ;
#73332 = EDGE_LOOP ( 'NONE', ( #45231, #46646, #185314, #58899 ) ) ;
#73333 = CARTESIAN_POINT ( 'NONE',  ( 4.817029820108094995, 1.034167108704350024, -1.730865207599366240 ) ) ;
#73335 = CARTESIAN_POINT ( 'NONE',  ( 3.256738233524118620, -0.5941274279437200878, -1.975181216424357400 ) ) ;
#73334 = CARTESIAN_POINT ( 'NONE',  ( 4.473300617505036492, 7.306268922809479704, -1.199719254218452047 ) ) ;
#73337 = CARTESIAN_POINT ( 'NONE',  ( -0.2409995289980246258, 1.355929887833319469, -2.254219809973062816 ) ) ;
#73336 = DIRECTION ( 'NONE',  ( -1.000000000000000000, 0.000000000000000000, 0.000000000000000000 ) ) ;
#73338 = EDGE_CURVE ( 'NONE', #26009, #82080, #57668, .T. ) ;
#73339 = CARTESIAN_POINT ( 'NONE',  ( 3.377389663135653031, 6.954388683717978026, -0.7216878364870338292 ) ) ;
#73340 = CARTESIAN_POINT ( 'NONE',  ( 1.642778471875000035, -3.376041666188708046, -2.845375778867859751 ) ) ;
#73341 = CARTESIAN_POINT ( 'NONE',  ( -0.6823417656249969321, 5.717708333674756283, -1.181850606188749264 ) ) ;
#73342 = CARTESIAN_POINT ( 'NONE',  ( 5.894512528888635750, 1.793468170635740710, -1.259063434910556500 ) ) ;
#73343 = CARTESIAN_POINT ( 'NONE',  ( 4.113907844847329187, 0.1017495355152969322, 2.013985960686740295 ) ) ;
#73344 = CARTESIAN_POINT ( 'NONE',  ( 2.806014743833367131, 1.331929863061011465, -1.271513748034671654 ) ) ;
#73345 = EDGE_CURVE ( 'NONE', #213437, #37457, #156787, .T. ) ;
#73346 = CARTESIAN_POINT ( 'NONE',  ( 5.469824908109481854, 8.468880595181346393, -1.199719254218446718 ) ) ;
#73347 = CARTESIAN_POINT ( 'NONE',  ( 6.053692819838605743, 0.5272490726609192491, -1.747765065496959869 ) ) ;
#73348 = CARTESIAN_POINT ( 'NONE',  ( 0.1944798361989338309, 2.004116887782161349, 1.125739740898183294 ) ) ;
#73349 = CARTESIAN_POINT ( 'NONE',  ( -5.377780486114890124, 9.425827667109372143, 0.000000000000000000 ) ) ;
#73350 = CARTESIAN_POINT ( 'NONE',  ( 6.789870067575622947, -0.9739125386618008307, 2.039881742057749303 ) ) ;
#73351 = CARTESIAN_POINT ( 'NONE',  ( 1.910898437428062646, 1.559696066972179107, -1.415416642437119954 ) ) ;
#73352 = CARTESIAN_POINT ( 'NONE',  ( -4.911796789900812144, 8.952456364851418158, 0.7998128361456291469 ) ) ;
#73353 = CARTESIAN_POINT ( 'NONE',  ( 7.775764792637399836, 9.030479331953833011, -1.199719254218441611 ) ) ;
#73354 = CARTESIAN_POINT ( 'NONE',  ( 5.790741006368192778, 8.809596036521288198, -1.082531754730548412 ) ) ;
#73355 =( NAMED_UNIT ( * ) SI_UNIT ( $, .STERADIAN. ) SOLID_ANGLE_UNIT ( ) );
#73356 = CARTESIAN_POINT ( 'NONE',  ( -5.876569516519495551, 8.943415971659659292, 1.199719254218452047 ) ) ;
#73357 = CARTESIAN_POINT ( 'NONE',  ( 5.450014562569148957, 9.302174723065263606, 1.040834085586084257E-14 ) ) ;
#73358 = CARTESIAN_POINT ( 'NONE',  ( 4.919437264989244163, 6.867374270256937585, 1.424029350978267550 ) ) ;
#73359 = CARTESIAN_POINT ( 'NONE',  ( -4.062639585589296942, 7.891496616496157301, 0.7998128361456341429 ) ) ;
#73360 = CARTESIAN_POINT ( 'NONE',  ( 3.726986581234917661, 1.568921747024876634, -1.572872013324580154 ) ) ;
#73361 = CARTESIAN_POINT ( 'NONE',  ( 2.818527994553555516, 2.063739945100159900, 0.7375456357434084786 ) ) ;
#73362 = CARTESIAN_POINT ( 'NONE',  ( -4.740547266272593596, 8.682388910626682943, -0.7998128361456281477 ) ) ;
#73363 = TOROIDAL_SURFACE ( 'NONE', #11054, 2.349999999999999645, 0.1000000000000000056 ) ;
#73364 = CARTESIAN_POINT ( 'NONE',  ( 0.6806489137391663613, -1.222764829241920648, 1.836970590647703627 ) ) ;
#73365 = CARTESIAN_POINT ( 'NONE',  ( -3.786470039966538970, 7.639575156594750283, 0.000000000000000000 ) ) ;
#73366 = CARTESIAN_POINT ( 'NONE',  ( 4.984793487045196869, 1.876812866478014596, 0.5713181500588762063 ) ) ;
#73367 = CARTESIAN_POINT ( 'NONE',  ( 10.07778825365955733, 10.65184113889131012, -0.7998128361456281477 ) ) ;
#73368 = CARTESIAN_POINT ( 'NONE',  ( 6.777182134110200096, 7.629137130509070275, 2.410944104600750038 ) ) ;
#73369 = CARTESIAN_POINT ( 'NONE',  ( -1.201851678989727383E-14, 1.821875000341421691, 1.575800808251672791 ) ) ;
#73370 = CARTESIAN_POINT ( 'NONE',  ( -3.174017359375036929, 6.717120995997236221, 0.7216878364870338292 ) ) ;
#73372 = EDGE_LOOP ( 'NONE', ( #118335, #130533, #77896, #33959 ) ) ;
#73371 = CARTESIAN_POINT ( 'NONE',  ( -6.616015773788831211, 7.781401826584148473, 1.082531754730549967 ) ) ;
#73373 = CARTESIAN_POINT ( 'NONE',  ( 3.726904977748810133, 1.497142547446396410, -1.502090761940577002 ) ) ;
#73374 = CARTESIAN_POINT ( 'NONE',  ( -5.469788628470539926, 5.346117919495872783, -0.7998128361456362523 ) ) ;
#73375 = CARTESIAN_POINT ( 'NONE',  ( 5.436455051933180016, 2.129025116502227810, 0.3735886874452337691 ) ) ;
#73376 = CARTESIAN_POINT ( 'NONE',  ( 4.794779880727245036, 8.745660294157122649, -0.7998128361456281477 ) ) ;
#73377 = CARTESIAN_POINT ( 'NONE',  ( 3.878315922200573862, -0.1843894689829879974, -1.832007427040844183 ) ) ;
#73378 = DIRECTION ( 'NONE',  ( 0.7806247497997951257, 0.000000000000000000, -0.6250000000000058842 ) ) ;
#73379 = CARTESIAN_POINT ( 'NONE',  ( -1.364683531250012516, 2.092708333674750953, 0.7879004041258379498 ) ) ;
#73380 = CARTESIAN_POINT ( 'NONE',  ( 6.562468561866369399, -1.594522334811569131, -0.6977961348336658709 ) ) ;
#73381 = CARTESIAN_POINT ( 'NONE',  ( 11.41381675112459959, 12.69999999999997087, 3.704697986577257129 ) ) ;
#73382 = CARTESIAN_POINT ( 'NONE',  ( 4.378920427533921078, 4.211088041652093494, 1.214306433183764966E-14 ) ) ;
#73383 = CARTESIAN_POINT ( 'NONE',  ( 0.4019237886466816012, 11.92633545031536890, -1.499999999999998668 ) ) ;
#73384 = CARTESIAN_POINT ( 'NONE',  ( 4.469695567000064429, 2.097540297429688838, -0.5223010940857697459 ) ) ;
#73385 = CARTESIAN_POINT ( 'NONE',  ( -5.773074481320628948, 5.629675071162500544, 0.000000000000000000 ) ) ;
#73386 = VECTOR ( 'NONE', #158171, 1000.000000000000114 ) ;
#73387 = CARTESIAN_POINT ( 'NONE',  ( 0.1394461523056798324, 0.009327122704651937685, -1.719853553173174232 ) ) ;
#73388 = CARTESIAN_POINT ( 'NONE',  ( -6.656690234185426824, 10.70996300661758660, 0.7216878364870458196 ) ) ;
#73389 = B_SPLINE_CURVE_WITH_KNOTS ( 'NONE', 3,
 ( #87126, #88199, #38377, #5847, #138027, #153196, #6917 ),
 .UNSPECIFIED., .F., .F.,
 ( 4, 3, 4 ),
 ( 0.000000000000000000, 4.270488675891434798E-05, 4.488495215206818762E-05 ),
 .UNSPECIFIED. ) ;
#73391 = CARTESIAN_POINT ( 'NONE',  ( 3.010779355932476253, 1.566693023359872372, -1.489686202715050145 ) ) ;
#73390 = AXIS2_PLACEMENT_3D ( 'NONE', #189709, #28283, #94378 ) ;
#73392 = CARTESIAN_POINT ( 'NONE',  ( 5.009034487593355678, 1.713717141372484765, 0.9743026824079579207 ) ) ;
#73393 = CARTESIAN_POINT ( 'NONE',  ( 3.901445378353602944, 0.2529189268129055090, 1.715120161964154510 ) ) ;
#73394 = CARTESIAN_POINT ( 'NONE',  ( 0.3456114054924685486, 0.6817542107791437767, -2.082909237240769151 ) ) ;
#73395 = CARTESIAN_POINT ( 'NONE',  ( 0.9038794553481295235, 1.888499008566895787, 1.325839279686758632 ) ) ;
#73396 = CARTESIAN_POINT ( 'NONE',  ( 3.813790581289760784, -2.030913156241159978, 0.3485601269093330234 ) ) ;
#73397 = CARTESIAN_POINT ( 'NONE',  ( 5.688998805639625012, 1.473442329711650345, 1.265259504309938610 ) ) ;
#73398 = CARTESIAN_POINT ( 'NONE',  ( -6.493992390821436977, 10.52014885602626393, 0.7216878364870458196 ) ) ;
#73399 = CARTESIAN_POINT ( 'NONE',  ( -3.969505113751027547, 7.853116076009993840, 1.214306433183764966E-14 ) ) ;
#73400 = CARTESIAN_POINT ( 'NONE',  ( -2.679285714285713826, 0.4970443252110354759, 0.000000000000000000 ) ) ;
#73402 = ORIENTED_EDGE ( 'NONE', *, *, #206408, .T. ) ;
#73401 = CARTESIAN_POINT ( 'NONE',  ( -5.340986169140711226, 5.195848383611072485, 0.000000000000000000 ) ) ;
#73403 = CARTESIAN_POINT ( 'NONE',  ( -7.171900071504745178, 9.390302721554109056, -1.443375672974058777 ) ) ;
#73404 = CARTESIAN_POINT ( 'NONE',  ( 2.714145368365259436, -2.182908968410116834, 0.3227909207665635716 ) ) ;
#73405 = CARTESIAN_POINT ( 'NONE',  ( -3.285556943749998737, -4.017708332855375986, 1.896917185911908499 ) ) ;
#73406 = ORIENTED_EDGE ( 'NONE', *, *, #55165, .T. ) ;
#73407 = CARTESIAN_POINT ( 'NONE',  ( 1.199803204733034923, 0.7606819372595281514, -1.698589668608577963 ) ) ;
#73408 = CARTESIAN_POINT ( 'NONE',  ( -0.02880301295726198432, 1.985184585160368664, -2.687100061827327302 ) ) ;
#73409 = CARTESIAN_POINT ( 'NONE',  ( -1.001543065824772872E-14, 5.493750000682816825, 1.732050807568877637 ) ) ;
#73410 = CARTESIAN_POINT ( 'NONE',  ( 4.757767692435503015, 7.006667324785019524, -1.397933448811568224 ) ) ;
#73412 = DIRECTION ( 'NONE',  ( -0.000000000000000000, -1.000000000000000000, -0.000000000000000000 ) ) ;
#73411 = CARTESIAN_POINT ( 'NONE',  ( -1.201851678989727383E-14, 5.118750000682815937, -1.732050807568863648 ) ) ;
#73413 = CARTESIAN_POINT ( 'NONE',  ( 6.456982894382444549, 0.3095715517048603926, -1.814770079682447967 ) ) ;
#73414 = VERTEX_POINT ( 'NONE', #211435 ) ;
#73415 = CARTESIAN_POINT ( 'NONE',  ( 2.342715047087840397, 0.4503528687099351280, 2.010914609654746332 ) ) ;
#73416 = CARTESIAN_POINT ( 'NONE',  ( -0.6801582343750334214, 0.1822916670080609869, 1.178068619123799898 ) ) ;
#73417 = CARTESIAN_POINT ( 'NONE',  ( -7.718669524881690336, 7.899535955317097624, 0.7998128361456462443 ) ) ;
#73418 = CARTESIAN_POINT ( 'NONE',  ( 0.6311622855796495957, 3.299999999999997158, -0.4000000000000131783 ) ) ;
#73420 = EDGE_CURVE ( 'NONE', #133104, #171149, #44708, .T. ) ;
#73419 = CARTESIAN_POINT ( 'NONE',  ( 11.94105722165067895, 11.02582762082958467, 1.187919369849770534 ) ) ;
#73421 = CARTESIAN_POINT ( 'NONE',  ( 3.846762897975340767, 5.510976019103107859, -1.599625672291256295 ) ) ;
#73422 = CIRCLE ( 'NONE', #156462, 2.000000000000000000 ) ;
#73423 = CARTESIAN_POINT ( 'NONE',  ( 1.006794875882726314, 1.561001636543899673, -1.345678083183374341 ) ) ;
#73425 = CARTESIAN_POINT ( 'NONE',  ( 5.056134578334451568, -1.329838508726857382, 1.273713382018211382 ) ) ;
#73424 = CARTESIAN_POINT ( 'NONE',  ( -3.022498986271247023, 2.800000000000024691, -2.500000000000000444 ) ) ;
#73426 = CARTESIAN_POINT ( 'NONE',  ( 5.608269097547198712, 9.694731047113750222, -0.7998128361456281477 ) ) ;
#73427 = CARTESIAN_POINT ( 'NONE',  ( -4.620296487206990932, 8.612372678375294299, 0.000000000000000000 ) ) ;
#73428 = SURFACE_STYLE_USAGE ( .BOTH. , #56127 ) ;
#73429 = CARTESIAN_POINT ( 'NONE',  ( 4.969440760808212509, 0.2186952961555181096, -2.196011921426939129 ) ) ;
#73430 = CARTESIAN_POINT ( 'NONE',  ( 6.696538538688765918, -0.5935452916538739299, -2.183133895321730744 ) ) ;
#73431 = CARTESIAN_POINT ( 'NONE',  ( -6.412643469583822586, 6.583764924043652655, 1.040834085586084257E-14 ) ) ;
#73432 = CARTESIAN_POINT ( 'NONE',  ( 0.3867804997886997720, -1.801505969789623629, -0.6421655129100201087 ) ) ;
#73433 = CARTESIAN_POINT ( 'NONE',  ( 0.6554828803995507158, 1.942095732595986890, -0.5424746339172461518 ) ) ;
#73434 = DIRECTION ( 'NONE',  ( 0.000000000000000000, 0.000000000000000000, 1.000000000000000000 ) ) ;
#73435 = DIRECTION ( 'NONE',  ( 1.276756478318932585E-15, -1.000000000000000000, 1.665334536937738262E-16 ) ) ;
#73436 = CARTESIAN_POINT ( 'NONE',  ( -0.2753771601587257645, 6.383602266891855059, 3.144803022522423053 ) ) ;
#73437 = CARTESIAN_POINT ( 'NONE',  ( 4.175548122884573665, 3.973820352894515295, 1.214306433183764966E-14 ) ) ;
#73438 = CARTESIAN_POINT ( 'NONE',  ( 1.129532124359374334, -1.183843481993757774, -1.448407549327054955 ) ) ;
#73439 = CARTESIAN_POINT ( 'NONE',  ( 2.237517880698642880, 0.5331670712399002587, -1.944730990508992008 ) ) ;
#73441 = CARTESIAN_POINT ( 'NONE',  ( -5.618858236835076347, 6.511109054719892875, 1.020627645029206443 ) ) ;
#73440 = CARTESIAN_POINT ( 'NONE',  ( 0.6823417656249882723, 0.6760416670080898749, -1.181850606188749264 ) ) ;
#73443 = CARTESIAN_POINT ( 'NONE',  ( 4.248724916491292802, 0.5614479688690295900, 2.029775142636090379 ) ) ;
#73442 = CARTESIAN_POINT ( 'NONE',  ( -7.395082721250053837, 10.71501471051202614, -1.199719254218446718 ) ) ;
#73444 = CARTESIAN_POINT ( 'NONE',  ( 6.584456157731144899, 10.83361595066169514, -0.7998128361456291469 ) ) ;
#73446 = CARTESIAN_POINT ( 'NONE',  ( -7.018317073368468328, 11.33978701890523233, -0.7998128361456291469 ) ) ;
#73445 = CARTESIAN_POINT ( 'NONE',  ( 3.250922972226694352, 7.014770244231638863, 0.7998128361456281477 ) ) ;
#73447 = CARTESIAN_POINT ( 'NONE',  ( 1.396038594575822023, 3.355321791732675418, 0.1345620919992574216 ) ) ;
#73448 = CARTESIAN_POINT ( 'NONE',  ( 3.849871613625083899, -1.395920841890609498, -1.459997210279185831 ) ) ;
#73449 = B_SPLINE_CURVE_WITH_KNOTS ( 'NONE', 3,
 ( #37848, #118102, #4248, #106913, #134321, #151614, #102854, #83389, #199260, #20513 ),
 .UNSPECIFIED., .F., .F.,
 ( 4, 3, 3, 4 ),
 ( -1.883571653736190889E-06, 0.000000000000000000, 1.648379509549351119E-05, 5.799965632663460626E-05 ),
 .UNSPECIFIED. ) ;
#73450 = CARTESIAN_POINT ( 'NONE',  ( 1.364683531249990311, 5.134375000341417916, 1.214306433183764966E-14 ) ) ;
#73451 = EDGE_CURVE ( 'NONE', #172976, #183133, #166224, .T. ) ;
#73452 = CARTESIAN_POINT ( 'NONE',  ( 6.197729521560835231, -1.491448369540880670, -1.425081351520232964 ) ) ;
#73453 = CARTESIAN_POINT ( 'NONE',  ( 7.768458830950378591, 12.00702636951006497, 1.040834085586084257E-14 ) ) ;
#73454 = CARTESIAN_POINT ( 'NONE',  ( 4.218171724704827596, -1.107204882465680607, -1.856345114869990320 ) ) ;
#73455 = CARTESIAN_POINT ( 'NONE',  ( 7.147083253059300922, 8.367293879104554577, 1.199719254218452935 ) ) ;
#73456 = CARTESIAN_POINT ( 'NONE',  ( 0.7499999999999902300, 5.816666666666685082, -1.299038105676658228 ) ) ;
#73458 = CARTESIAN_POINT ( 'NONE',  ( -9.498763045327489607, -9.581505939640113212, 0.1791256580974910639 ) ) ;
#73457 = CARTESIAN_POINT ( 'NONE',  ( 7.191674137406095291, 7.354984346587396082, 0.000000000000000000 ) ) ;
#73459 =( BOUNDED_SURFACE ( )  B_SPLINE_SURFACE ( 1, 2, ( 
 ( #183278, #168108, #186473, #87919, #20760, #150804, #55418, #117280, #2368, #3441, #185405, #169165, #202710, #137755, #86854, #68445, #153993, #200575, #152919, #4498, #118350, #70566, #136685, #38109, #170230, #39174, #21815, #5561, #71642, #203774, #121572, #187543, #105257, #171298, #89005, #175583, #176640, #173460, #91141, #90070, #41326, #188613, #156133, #106356, #124773, #40245, #74873, #110638, #208051, #7715, #107436, #8794, #190732, #138818, #192865, #172379, #75934, #72724, #73799, #59678, #27173, #123714, #158269, #209106, #140979, #189676, #42395, #25040, #9858, #60744, #157197, #108505, #142035, #23968, #139893, #191796, #174528, #26106, #92218, #125838, #205924, #43458, #206988, #58617, #93277, #57557, #109579, #159315, #204839, #56492, #10912, #76988, #126906, #143115, #44521, #28252, #94345, #122650, #160387, #32510, #16230, #11987, #177713, #111704, #82314, #29322, #14102, #80192, #163593, #146297, #211248, #64992, #195017, #48774, #179838, #13048, #144188, #95416, #78063, #45588, #112772, #62873, #178783, #129040, #127987, #79127, #212309, #99643, #46649, #61820, #30397, #147342, #180888, #113842, #161468, #148408, #210180, #193941, #96483, #63944, #130099, #81263, #214407, #31459, #145243, #98585, #162530, #196093, #47726, #97536, #15176, #213370, #131146, #197135, #132185, #114889, #164647, #66038, #198191, #49826, #115951, #181941, #33571, #85517, #133242, #149460, #171839, #105813, #55957, #1043, #199247, #156670, #74346, #34633, #73250, #17299, #50894, #190208, #106898, #41868, #138286, #23432, #89543, #100704, #184077, #118092, #155594, #183016, #35696, #205387, #101772, #19437, #117019, #7179, #139357, #151603, #69242, #204301, #2105, #84453, #122110, #165710, #68179, #83377, #67106, #167840, #188075, #166780, #18376, #57026, #3171, #123193, #189154, #134310, #150541, #40793, #39704, #172924, #24500, #90611, #200317, #51968, #8262, #140450, #206461, #58088, #124250, #208582, #28796, #129579, #107977, #77534, #78599, #43994, #175062, #127452, #29870, #63427, #61291, #145786, #12526 ),
 ( #60215, #193423, #95953, #126376, #11461, #111178, #9338, #191267, #144719, #143655, #209650, #45067, #177180, #141524, #94880, #158794, #142575, #210731, #42933, #75411, #10391, #25577, #174006, #192335, #62357, #162008, #194486, #160932, #92750, #128518, #91688, #27723, #46129, #112246, #157741, #59151, #13597, #109043, #178257, #207532, #125309, #195566, #79671, #26649, #211789, #76466, #110112, #176123, #93817, #159858, #116493, #64492, #131671, #83920, #213903, #115435, #146836, #50370, #182482, #181426, #165183, #82861, #98080, #180375, #16777, #68720, #164135, #134842, #163073, #49318, #148937, #47202, #113317, #34110, #33056, #166247, #67642, #15719, #212855, #150011, #509, #100182, #133789, #99134, #179323, #30944, #17837, #1581, #183556, #65526, #130634, #147887, #199797, #97019, #14654, #66577, #51442, #197674, #114380, #132719, #35163, #2647, #198724, #84992, #117561, #101239, #167321, #18908, #151083, #80748, #196626, #48266, #31999, #81804, #70847, #186756, #122934, #53563, #136962, #19978, #38379, #88201, #52496, #56768, #202989, #89286, #103383, #24240, #153198, #155334, #4769, #3707, #6918, #72995, #169445, #21030, #23171, #90342, #54629, #87128, #86062, #74090, #156411, #7998, #120776, #105540, #36229, #104460, #200845, #118626, #154274, #170507, #5849, #135892, #168382, #22089, #152139, #184612, #204043, #138029, #71919, #102308, #69784, #188891, #171574, #139097, #55693, #201910, #205124, #121848, #187819, #40532, #39446, #119696, #185680, #106636, #172664, #37309, #158541, #9082, #26390, #61035, #161753, #140181, #109858, #110917, #76213, #207274, #159602, #62110, #95698, #93558, #177999, #44813, #10138, #78345, #77281, #176923, #11200, #59964, #209391, #29613, #210472, #142323, #126119, #128269, #58905, #208333, #173748, #192079, #27460, #206203, #194231, #43745, #28538, #42681, #13344, #92502, #94630, #175872, #157487, #160673, #12268, #108788, #174814, #144468, #57831, #143393, #127196, #25325, #123992, #189960, #41610, #193163, #45875, #107721, #111997, #91426, #75156, #141266, #125058 ) ),
 .UNSPECIFIED., .F., .F., .T. ) 
 B_SPLINE_SURFACE_WITH_KNOTS ( ( 2, 2 ),
 ( 3, 2, 2, 2, 2, 2, 2, 2, 2, 2, 2, 2, 2, 2, 2, 2, 2, 2, 2, 2, 2, 2, 2, 2, 2, 2, 2, 2, 2, 2, 2, 2, 2, 2, 2, 2, 2, 2, 2, 2, 2, 2, 2, 2, 2, 2, 2, 2, 2, 2, 2, 2, 2, 2, 2, 2, 2, 2, 2, 2, 2, 2, 2, 2, 2, 2, 2, 2, 2, 2, 2, 2, 2, 2, 2, 2, 2, 2, 2, 2, 2, 2, 2, 2, 2, 2, 2, 2, 2, 2, 2, 2, 2, 2, 2, 2, 2, 2, 2, 2, 2, 2, 2, 2, 2, 2, 2, 2, 2, 2, 2, 2, 2, 2, 2, 2, 2, 2, 2, 2, 3 ),
 ( 0.000000000000000000, 1.000000000000000000 ),
 ( 0.000000000000000000, 0.008333333333333333218, 0.01666666666666666644, 0.02500000000000000139, 0.03333333333333333287, 0.04166666666666666435, 0.05000000000000000278, 0.05833333333333333426, 0.06666666666666666574, 0.07499999999999999722, 0.08333333333333332871, 0.09166666666666666019, 0.1000000000000000056, 0.1083333333333333370, 0.1166666666666666685, 0.1250000000000000000, 0.1333333333333333315, 0.1416666666666666630, 0.1499999999999999944, 0.1583333333333333259, 0.1666666666666666574, 0.1749999999999999889, 0.1833333333333333204, 0.1916666666666666796, 0.2000000000000000111, 0.2083333333333333426, 0.2166666666666666741, 0.2250000000000000056, 0.2333333333333333370, 0.2416666666666666685, 0.2500000000000000000, 0.2583333333333333592, 0.2666666666666666630, 0.2750000000000000222, 0.2833333333333333259, 0.2916666666666666852, 0.2999999999999999889, 0.3083333333333333481, 0.3166666666666666519, 0.3250000000000000111, 0.3333333333333333148, 0.3416666666666666741, 0.3499999999999999778, 0.3583333333333333370, 0.3666666666666666408, 0.3750000000000000000, 0.3833333333333333592, 0.3916666666666666630, 0.4000000000000000222, 0.4083333333333333259, 0.4166666666666666852, 0.4249999999999999889, 0.4333333333333333481, 0.4416666666666666519, 0.4500000000000000111, 0.4583333333333333148, 0.4666666666666666741, 0.4749999999999999778, 0.4833333333333333370, 0.4916666666666666408, 0.5000000000000000000, 0.5083333333333333037, 0.5166666666666667185, 0.5250000000000000222, 0.5333333333333333259, 0.5416666666666666297, 0.5500000000000000444, 0.5583333333333333481, 0.5666666666666666519, 0.5749999999999999556, 0.5833333333333333703, 0.5916666666666666741, 0.5999999999999999778, 0.6083333333333332815, 0.6166666666666666963, 0.6250000000000000000, 0.6333333333333333037, 0.6416666666666667185, 0.6500000000000000222, 0.6583333333333333259, 0.6666666666666666297, 0.6750000000000000444, 0.6833333333333333481, 0.6916666666666666519, 0.6999999999999999556, 0.7083333333333333703, 0.7166666666666666741, 0.7249999999999999778, 0.7333333333333332815, 0.7416666666666666963, 0.7500000000000000000, 0.7583333333333333037, 0.7666666666666667185, 0.7750000000000000222, 0.7833333333333333259, 0.7916666666666666297, 0.8000000000000000444, 0.8083333333333333481, 0.8166666666666666519, 0.8249999999999999556, 0.8333333333333333703, 0.8416666666666666741, 0.8499999999999999778, 0.8583333333333332815, 0.8666666666666666963, 0.8750000000000000000, 0.8833333333333333037, 0.8916666666666667185, 0.9000000000000000222, 0.9083333333333333259, 0.9166666666666666297, 0.9250000000000000444, 0.9333333333333333481, 0.9416666666666666519, 0.9499999999999999556, 0.9583333333333333703, 0.9666666666666666741, 0.9749999999999999778, 0.9833333333333332815, 0.9916666666666666963, 1.000000000000000000 ),
 .UNSPECIFIED. ) 
 GEOMETRIC_REPRESENTATION_ITEM ( )  RATIONAL_B_SPLINE_SURFACE ( (
 ( 1.000000000000000000, 0.8660254037844387076, 1.000000000000000000, 0.8660254037844387076, 1.000000000000000000, 0.8660254037844387076, 1.000000000000000000, 0.8660254037844387076, 1.000000000000000000, 0.8660254037844387076, 1.000000000000000000, 0.8660254037844387076, 1.000000000000000000, 0.8660254037844387076, 1.000000000000000000, 0.8660254037844387076, 1.000000000000000000, 0.8660254037844387076, 1.000000000000000000, 0.8660254037844387076, 1.000000000000000000, 0.8660254037844387076, 1.000000000000000000, 0.8660254037844387076, 1.000000000000000000, 0.8660254037844387076, 1.000000000000000000, 0.8660254037844387076, 1.000000000000000000, 0.8660254037844387076, 1.000000000000000000, 0.8660254037844387076, 1.000000000000000000, 0.8660254037844387076, 1.000000000000000000, 0.8660254037844387076, 1.000000000000000000, 0.8660254037844387076, 1.000000000000000000, 0.8660254037844387076, 1.000000000000000000, 0.8660254037844387076, 1.000000000000000000, 0.8660254037844387076, 1.000000000000000000, 0.8660254037844387076, 1.000000000000000000, 0.8660254037844387076, 1.000000000000000000, 0.8660254037844387076, 1.000000000000000000, 0.8660254037844387076, 1.000000000000000000, 0.8660254037844387076, 1.000000000000000000, 0.8660254037844387076, 1.000000000000000000, 0.8660254037844387076, 1.000000000000000000, 0.8660254037844387076, 1.000000000000000000, 0.8660254037844387076, 1.000000000000000000, 0.8660254037844387076, 1.000000000000000000, 0.8660254037844387076, 1.000000000000000000, 0.8660254037844387076, 1.000000000000000000, 0.8660254037844387076, 1.000000000000000000, 0.8660254037844387076, 1.000000000000000000, 0.8660254037844387076, 1.000000000000000000, 0.8660254037844387076, 1.000000000000000000, 0.8660254037844387076, 1.000000000000000000, 0.8660254037844387076, 1.000000000000000000, 0.8660254037844387076, 1.000000000000000000, 0.8660254037844387076, 1.000000000000000000, 0.8660254037844387076, 1.000000000000000000, 0.8660254037844387076, 1.000000000000000000, 0.8660254037844387076, 1.000000000000000000, 0.8660254037844387076, 1.000000000000000000, 0.8660254037844387076, 1.000000000000000000, 0.8660254037844387076, 1.000000000000000000, 0.8660254037844387076, 1.000000000000000000, 0.8660254037844387076, 1.000000000000000000, 0.8660254037844387076, 1.000000000000000000, 0.8660254037844387076, 1.000000000000000000, 0.8660254037844387076, 1.000000000000000000, 0.8660254037844387076, 1.000000000000000000, 0.8660254037844387076, 1.000000000000000000, 0.8660254037844387076, 1.000000000000000000, 0.8660254037844387076, 1.000000000000000000, 0.8660254037844387076, 1.000000000000000000, 0.8660254037844387076, 1.000000000000000000, 0.8660254037844387076, 1.000000000000000000, 0.8660254037844387076, 1.000000000000000000, 0.8660254037844387076, 1.000000000000000000, 0.8660254037844387076, 1.000000000000000000, 0.8660254037844387076, 1.000000000000000000, 0.8660254037844387076, 1.000000000000000000, 0.8660254037844387076, 1.000000000000000000, 0.8660254037844387076, 1.000000000000000000, 0.8660254037844387076, 1.000000000000000000, 0.8660254037844387076, 1.000000000000000000, 0.8660254037844387076, 1.000000000000000000, 0.8660254037844387076, 1.000000000000000000, 0.8660254037844387076, 1.000000000000000000, 0.8660254037844387076, 1.000000000000000000, 0.8660254037844387076, 1.000000000000000000, 0.8660254037844387076, 1.000000000000000000, 0.8660254037844387076, 1.000000000000000000, 0.8660254037844387076, 1.000000000000000000, 0.8660254037844387076, 1.000000000000000000, 0.8660254037844387076, 1.000000000000000000, 0.8660254037844387076, 1.000000000000000000, 0.8660254037844387076, 1.000000000000000000, 0.8660254037844387076, 1.000000000000000000, 0.8660254037844387076, 1.000000000000000000, 0.8660254037844387076, 1.000000000000000000, 0.8660254037844387076, 1.000000000000000000, 0.8660254037844387076, 1.000000000000000000, 0.8660254037844387076, 1.000000000000000000, 0.8660254037844387076, 1.000000000000000000, 0.8660254037844387076, 1.000000000000000000, 0.8660254037844387076, 1.000000000000000000, 0.8660254037844387076, 1.000000000000000000, 0.8660254037844387076, 1.000000000000000000, 0.8660254037844387076, 1.000000000000000000, 0.8660254037844387076, 1.000000000000000000, 0.8660254037844387076, 1.000000000000000000, 0.8660254037844387076, 1.000000000000000000, 0.8660254037844387076, 1.000000000000000000, 0.8660254037844387076, 1.000000000000000000, 0.8660254037844387076, 1.000000000000000000, 0.8660254037844387076, 1.000000000000000000, 0.8660254037844387076, 1.000000000000000000, 0.8660254037844387076, 1.000000000000000000, 0.8660254037844387076, 1.000000000000000000, 0.8660254037844387076, 1.000000000000000000, 0.8660254037844387076, 1.000000000000000000, 0.8660254037844387076, 1.000000000000000000, 0.8660254037844387076, 1.000000000000000000, 0.8660254037844387076, 1.000000000000000000, 0.8660254037844387076, 1.000000000000000000, 0.8660254037844387076, 1.000000000000000000, 0.8660254037844387076, 1.000000000000000000, 0.8660254037844387076, 1.000000000000000000, 0.8660254037844387076, 1.000000000000000000, 0.8660254037844387076, 1.000000000000000000, 0.8660254037844387076, 1.000000000000000000, 0.8660254037844387076, 1.000000000000000000, 0.8660254037844387076, 1.000000000000000000, 0.8660254037844387076, 1.000000000000000000, 0.8660254037844387076, 1.000000000000000000, 0.8660254037844387076, 1.000000000000000000),
 ( 1.000000000000000000, 0.8660254037844387076, 1.000000000000000000, 0.8660254037844387076, 1.000000000000000000, 0.8660254037844387076, 1.000000000000000000, 0.8660254037844387076, 1.000000000000000000, 0.8660254037844387076, 1.000000000000000000, 0.8660254037844387076, 1.000000000000000000, 0.8660254037844387076, 1.000000000000000000, 0.8660254037844387076, 1.000000000000000000, 0.8660254037844387076, 1.000000000000000000, 0.8660254037844387076, 1.000000000000000000, 0.8660254037844387076, 1.000000000000000000, 0.8660254037844387076, 1.000000000000000000, 0.8660254037844387076, 1.000000000000000000, 0.8660254037844387076, 1.000000000000000000, 0.8660254037844387076, 1.000000000000000000, 0.8660254037844387076, 1.000000000000000000, 0.8660254037844387076, 1.000000000000000000, 0.8660254037844387076, 1.000000000000000000, 0.8660254037844387076, 1.000000000000000000, 0.8660254037844387076, 1.000000000000000000, 0.8660254037844387076, 1.000000000000000000, 0.8660254037844387076, 1.000000000000000000, 0.8660254037844387076, 1.000000000000000000, 0.8660254037844387076, 1.000000000000000000, 0.8660254037844387076, 1.000000000000000000, 0.8660254037844387076, 1.000000000000000000, 0.8660254037844387076, 1.000000000000000000, 0.8660254037844387076, 1.000000000000000000, 0.8660254037844387076, 1.000000000000000000, 0.8660254037844387076, 1.000000000000000000, 0.8660254037844387076, 1.000000000000000000, 0.8660254037844387076, 1.000000000000000000, 0.8660254037844387076, 1.000000000000000000, 0.8660254037844387076, 1.000000000000000000, 0.8660254037844387076, 1.000000000000000000, 0.8660254037844387076, 1.000000000000000000, 0.8660254037844387076, 1.000000000000000000, 0.8660254037844387076, 1.000000000000000000, 0.8660254037844387076, 1.000000000000000000, 0.8660254037844387076, 1.000000000000000000, 0.8660254037844387076, 1.000000000000000000, 0.8660254037844387076, 1.000000000000000000, 0.8660254037844387076, 1.000000000000000000, 0.8660254037844387076, 1.000000000000000000, 0.8660254037844387076, 1.000000000000000000, 0.8660254037844387076, 1.000000000000000000, 0.8660254037844387076, 1.000000000000000000, 0.8660254037844387076, 1.000000000000000000, 0.8660254037844387076, 1.000000000000000000, 0.8660254037844387076, 1.000000000000000000, 0.8660254037844387076, 1.000000000000000000, 0.8660254037844387076, 1.000000000000000000, 0.8660254037844387076, 1.000000000000000000, 0.8660254037844387076, 1.000000000000000000, 0.8660254037844387076, 1.000000000000000000, 0.8660254037844387076, 1.000000000000000000, 0.8660254037844387076, 1.000000000000000000, 0.8660254037844387076, 1.000000000000000000, 0.8660254037844387076, 1.000000000000000000, 0.8660254037844387076, 1.000000000000000000, 0.8660254037844387076, 1.000000000000000000, 0.8660254037844387076, 1.000000000000000000, 0.8660254037844387076, 1.000000000000000000, 0.8660254037844387076, 1.000000000000000000, 0.8660254037844387076, 1.000000000000000000, 0.8660254037844387076, 1.000000000000000000, 0.8660254037844387076, 1.000000000000000000, 0.8660254037844387076, 1.000000000000000000, 0.8660254037844387076, 1.000000000000000000, 0.8660254037844387076, 1.000000000000000000, 0.8660254037844387076, 1.000000000000000000, 0.8660254037844387076, 1.000000000000000000, 0.8660254037844387076, 1.000000000000000000, 0.8660254037844387076, 1.000000000000000000, 0.8660254037844387076, 1.000000000000000000, 0.8660254037844387076, 1.000000000000000000, 0.8660254037844387076, 1.000000000000000000, 0.8660254037844387076, 1.000000000000000000, 0.8660254037844387076, 1.000000000000000000, 0.8660254037844387076, 1.000000000000000000, 0.8660254037844387076, 1.000000000000000000, 0.8660254037844387076, 1.000000000000000000, 0.8660254037844387076, 1.000000000000000000, 0.8660254037844387076, 1.000000000000000000, 0.8660254037844387076, 1.000000000000000000, 0.8660254037844387076, 1.000000000000000000, 0.8660254037844387076, 1.000000000000000000, 0.8660254037844387076, 1.000000000000000000, 0.8660254037844387076, 1.000000000000000000, 0.8660254037844387076, 1.000000000000000000, 0.8660254037844387076, 1.000000000000000000, 0.8660254037844387076, 1.000000000000000000, 0.8660254037844387076, 1.000000000000000000, 0.8660254037844387076, 1.000000000000000000, 0.8660254037844387076, 1.000000000000000000, 0.8660254037844387076, 1.000000000000000000, 0.8660254037844387076, 1.000000000000000000, 0.8660254037844387076, 1.000000000000000000, 0.8660254037844387076, 1.000000000000000000, 0.8660254037844387076, 1.000000000000000000, 0.8660254037844387076, 1.000000000000000000, 0.8660254037844387076, 1.000000000000000000, 0.8660254037844387076, 1.000000000000000000, 0.8660254037844387076, 1.000000000000000000, 0.8660254037844387076, 1.000000000000000000, 0.8660254037844387076, 1.000000000000000000, 0.8660254037844387076, 1.000000000000000000, 0.8660254037844387076, 1.000000000000000000, 0.8660254037844387076, 1.000000000000000000, 0.8660254037844387076, 1.000000000000000000, 0.8660254037844387076, 1.000000000000000000, 0.8660254037844387076, 1.000000000000000000, 0.8660254037844387076, 1.000000000000000000, 0.8660254037844387076, 1.000000000000000000, 0.8660254037844387076, 1.000000000000000000, 0.8660254037844387076, 1.000000000000000000, 0.8660254037844387076, 1.000000000000000000, 0.8660254037844387076, 1.000000000000000000, 0.8660254037844387076, 1.000000000000000000, 0.8660254037844387076, 1.000000000000000000) ) ) 
 REPRESENTATION_ITEM ( '' )  SURFACE ( )  );
#73460 = CARTESIAN_POINT ( 'NONE',  ( 8.242994206984347372, 8.719174117677642499, 1.040834085586084257E-14 ) ) ;
#73462 = CARTESIAN_POINT ( 'NONE',  ( -1.793747577714859487, 2.512287210193241194, -2.500000000000000444 ) ) ;
#73461 = CARTESIAN_POINT ( 'NONE',  ( 2.067058339702015246, 1.609816819982702985, -1.457078277656477905 ) ) ;
#73464 = CARTESIAN_POINT ( 'NONE',  ( 2.296224312773272658, 1.477747569344042278, -1.098160524033331642 ) ) ;
#73463 = CARTESIAN_POINT ( 'NONE',  ( -6.263503779833496488, 6.409768619334935913, 0.7216878364870317197 ) ) ;
#73465 = CARTESIAN_POINT ( 'NONE',  ( 0.6823417656249899377, 2.592708333674753618, 1.181850606188767472 ) ) ;
#73466 = CARTESIAN_POINT ( 'NONE',  ( 3.298540952264991777, 1.726358142885858316, -1.349911518210664241 ) ) ;
#73467 = CARTESIAN_POINT ( 'NONE',  ( 6.983263157960363898, 3.684327263089666182, 2.667753665259400275 ) ) ;
#73468 = CARTESIAN_POINT ( 'NONE',  ( 3.713984175222109663, -2.229511888261398678, 0.3841874803040145059 ) ) ;
#73469 = CARTESIAN_POINT ( 'NONE',  ( -7.393273838153706201, 7.519907654134449615, 0.7998128361456341429 ) ) ;
#73470 = CARTESIAN_POINT ( 'NONE',  ( 1.364683531249990311, 4.696875000341417916, 1.214306433183764966E-14 ) ) ;
#73471 = CARTESIAN_POINT ( 'NONE',  ( 6.361499291607088935, 6.832587723092125032, 0.6030276918116053153 ) ) ;
#73472 = CARTESIAN_POINT ( 'NONE',  ( -0.7500000000000179856, 13.04166666666666607, 1.299038105676658228 ) ) ;
#73473 = CARTESIAN_POINT ( 'NONE',  ( 5.343321937561575474, 8.287607122913563273, -1.082531754730548412 ) ) ;
#73474 = CARTESIAN_POINT ( 'NONE',  ( 5.606658687911298955, 1.339352548545174937, -1.156898068784556255 ) ) ;
#73475 = CARTESIAN_POINT ( 'NONE',  ( 3.545567672969043294, -1.859159518717553139, 0.7725093927312511877 ) ) ;
#73476 = CARTESIAN_POINT ( 'NONE',  ( 8.067265095331215718, 9.370563018429956870, 1.199719254218462483 ) ) ;
#73477 = CARTESIAN_POINT ( 'NONE',  ( 2.186679620839627969, -2.065140684961807249, -0.4117111178513747638 ) ) ;
#73478 = VECTOR ( 'NONE', #37004, 1000.000000000000000 ) ;
#73480 = CARTESIAN_POINT ( 'NONE',  ( -1.499999999999997780, 1.650000000000019451, 0.000000000000000000 ) ) ;
#73479 = CARTESIAN_POINT ( 'NONE',  ( 0.6823417656249969321, 10.77604166700806765, -1.181850606188757036 ) ) ;
#73481 = CARTESIAN_POINT ( 'NONE',  ( 0.6605274321102487800, -0.6603073245880388686, -1.855717402334137622 ) ) ;
#73482 = CARTESIAN_POINT ( 'NONE',  ( -4.442231607132987925, 5.211633625523774960, -1.199719254218453823 ) ) ;
#73483 = CARTESIAN_POINT ( 'NONE',  ( 3.634019179650556097, 7.351260730161411239, -0.2183562399340302218 ) ) ;
#73485 = ORIENTED_EDGE ( 'NONE', *, *, #103038, .F. ) ;
#73484 = CARTESIAN_POINT ( 'NONE',  ( 5.976795019380008789, -1.274598912183276589, 1.287626877918945922 ) ) ;
#73486 = CARTESIAN_POINT ( 'NONE',  ( 8.107412671292047790, 8.560995659369956101, 0.7216878364870458196 ) ) ;
#73487 = EDGE_CURVE ( 'NONE', #197566, #184334, #83438, .T. ) ;
#73488 = CARTESIAN_POINT ( 'NONE',  ( 4.873830839387755631, 1.077430855447782942, 1.529020332772989210 ) ) ;
#73489 = CARTESIAN_POINT ( 'NONE',  ( 4.552840656090682891, 4.206068941727564514, 1.214306433183764966E-14 ) ) ;
#73490 = EDGE_LOOP ( 'NONE', ( #64010, #116015, #160386, #123709 ) ) ;
#73491 = CARTESIAN_POINT ( 'NONE',  ( 4.188381925097388603, 1.111774711627441681, -1.746232563387891457 ) ) ;
#73492 = CARTESIAN_POINT ( 'NONE',  ( -1.225000000000042277, 2.229166666666690499, -0.7072540797573217963 ) ) ;
#73493 = CARTESIAN_POINT ( 'NONE',  ( -5.031484404002922517, 6.963427452793760963, 1.443375672974058777 ) ) ;
#73494 = CARTESIAN_POINT ( 'NONE',  ( 0.000000000000000000, -0.8934598047668927956, -3.291472234583660672 ) ) ;
#73495 = CARTESIAN_POINT ( 'NONE',  ( 8.776205506747620788, 9.133327934160710981, -0.7998128361456221525 ) ) ;
#73496 = CARTESIAN_POINT ( 'NONE',  ( -1.543624195544814226, 8.695410207106890610, 2.508689898543552399 ) ) ;
#73497 = CARTESIAN_POINT ( 'NONE',  ( 7.180978637093494044, 8.406838493811077839, -1.199719254218452047 ) ) ;
#73498 = CARTESIAN_POINT ( 'NONE',  ( -1.556029036868112447, 0.5000000000000007772, 1.827231139298829632 ) ) ;
#73499 = CARTESIAN_POINT ( 'NONE',  ( 0.6823417656249882723, -0.3239583329919110133, -1.181850606188749264 ) ) ;
#73500 = CARTESIAN_POINT ( 'NONE',  ( -0.7500000000000215383, 0.6916666666666876351, 1.299038105676659116 ) ) ;
#73502 = CARTESIAN_POINT ( 'NONE',  ( 5.392392409933256303, 7.314210449720692786, 1.599625672291267398 ) ) ;
#73501 = CARTESIAN_POINT ( 'NONE',  ( 4.299235682465595509, -1.708000122724560477, 0.9650500775852040025 ) ) ;
#73503 = CARTESIAN_POINT ( 'NONE',  ( 2.530624857006387618, 1.977747929495787371, -0.3905373530270899174 ) ) ;
#73504 = DIRECTION ( 'NONE',  ( -1.000000000000000000, 0.000000000000000000, 3.491481338843133355E-15 ) ) ;
#73505 = CARTESIAN_POINT ( 'NONE',  ( 6.639320575229258559, 2.978120323461688645, 2.350396677589302374 ) ) ;
#73506 = DIRECTION ( 'NONE',  ( 0.000000000000000000, -1.000000000000000000, 0.000000000000000000 ) ) ;
#73507 = CARTESIAN_POINT ( 'NONE',  ( 2.442468673064964957, 0.4055347385497136137, 1.825902681341363021 ) ) ;
#73508 = CARTESIAN_POINT ( 'NONE',  ( 1.364683531249988535, 5.655208333674751842, -0.7879004041258300672 ) ) ;
#73509 = CARTESIAN_POINT ( 'NONE',  ( 4.359639327901571271, -1.559048523801108477, -1.273764430229076483 ) ) ;
#73510 = CARTESIAN_POINT ( 'NONE',  ( -9.481229494658258261, 9.955855920056455588, -0.7998128361456291469 ) ) ;
#73512 = CARTESIAN_POINT ( 'NONE',  ( 3.497769638136785986, -2.085511745926827309, 0.3643098080348127765 ) ) ;
#73511 = CARTESIAN_POINT ( 'NONE',  ( -4.582292731738899505, 8.289832587096611860, 0.7216878364870458196 ) ) ;
#73513 = DIRECTION ( 'NONE',  ( -0.6483454320283800199, 0.000000000000000000, 0.7613463080411787542 ) ) ;
#73514 = CARTESIAN_POINT ( 'NONE',  ( 5.037584538744971141, 1.933038169019934527, -0.7419538039311265321 ) ) ;
#73515 = CARTESIAN_POINT ( 'NONE',  ( 4.681308178468477799, 8.683552984847038303, 0.000000000000000000 ) ) ;
#73517 = CARTESIAN_POINT ( 'NONE',  ( 6.620655732516642189, 2.417337544263608251, 2.554705107920357321 ) ) ;
#73516 = CARTESIAN_POINT ( 'NONE',  ( 1.452797965663179314, -1.794991982752047965, -1.071751678227941929 ) ) ;
#73519 = ORIENTED_EDGE ( 'NONE', *, *, #193336, .F. ) ;
#73518 = CARTESIAN_POINT ( 'NONE',  ( 6.124025070245508573, -1.016541136310184390, -1.516163765885633286 ) ) ;
#73520 = CARTESIAN_POINT ( 'NONE',  ( 8.111855979677986994, 8.358253485912799263, 1.040834085586084257E-14 ) ) ;
#73522 = AXIS2_PLACEMENT_3D ( 'NONE', #184094, #72468, #136441 ) ;
#73521 = CARTESIAN_POINT ( 'NONE',  ( -11.96535697748088900, 13.75262667064456856, 0.9148528286453682101 ) ) ;
#73523 = CARTESIAN_POINT ( 'NONE',  ( -10.64985034906098882, 4.117567600086831980, 6.884957259278849051 ) ) ;
#73524 = CARTESIAN_POINT ( 'NONE',  ( 7.741342523278705201, 9.094283034322399928, 1.082531754730558626 ) ) ;
#73525 = CARTESIAN_POINT ( 'NONE',  ( 1.364683531249996529, 11.77604166700806765, 0.7879004041258403923 ) ) ;
#73526 = CARTESIAN_POINT ( 'NONE',  ( 6.340485057729076779, 1.096952271789692901, -1.566184530335120950 ) ) ;
#73527 = CARTESIAN_POINT ( 'NONE',  ( -8.779068160048691283, 10.20099992726700933, -1.199719254218446718 ) ) ;
#73528 = CARTESIAN_POINT ( 'NONE',  ( 6.169123589417988995, 7.156064594864501416, -1.199719254218445830 ) ) ;
#73529 = CARTESIAN_POINT ( 'NONE',  ( -11.81907076198602802, 11.25731224596479052, -1.592066415281275349 ) ) ;
#73530 = FACE_OUTER_BOUND ( 'NONE', #160893, .T. ) ;
#73531 = EDGE_CURVE ( 'NONE', #44, #210733, #62718, .T. ) ;
#73532 = CARTESIAN_POINT ( 'NONE',  ( 4.207107738942202246, 3.802713871720993399, 1.214306433183764966E-14 ) ) ;
#73533 = ORIENTED_EDGE ( 'NONE', *, *, #102642, .T. ) ;
#73534 = CARTESIAN_POINT ( 'NONE',  ( 6.310172759758509109, 1.158674036163497734, -1.650093421473826316 ) ) ;
#73535 = DIRECTION ( 'NONE',  ( 0.000000000000000000, 1.000000000000000000, 0.000000000000000000 ) ) ;
#73536 = CARTESIAN_POINT ( 'NONE',  ( 1.326446625878273444, -2.791019202464277584E-14, 0.3259839236695623588 ) ) ;
#73537 = AXIS2_PLACEMENT_3D ( 'NONE', #190384, #172022, #8434 ) ;
#73538 = VECTOR ( 'NONE', #120425, 1000.000000000000000 ) ;
#73539 = CARTESIAN_POINT ( 'NONE',  ( -0.1399997263889819488, 4.088450529495776919, -2.555104583160577203 ) ) ;
#73540 = CARTESIAN_POINT ( 'NONE',  ( -5.910991785878183080, 5.998504626387068051, -0.7216878364870278340 ) ) ;
#73541 = CARTESIAN_POINT ( 'NONE',  ( 9.083599731475976213, 12.58098820582193689, 1.082531754730546636 ) ) ;
#73542 = CARTESIAN_POINT ( 'NONE',  ( 2.289847402107755947, -1.282740503449712577, -1.494545344566786449 ) ) ;
#73543 = CARTESIAN_POINT ( 'NONE',  ( 4.745720352911135365, 1.994069623535676961, -0.2986464557954356946 ) ) ;
#73544 = CARTESIAN_POINT ( 'NONE',  ( -6.856673000209188906, 9.022537805042615489, 1.599625672291283607 ) ) ;
#73545 = CARTESIAN_POINT ( 'NONE',  ( 6.827182134110199030, 1.254919323356920025, 2.204230526214937758 ) ) ;
#73546 = CARTESIAN_POINT ( 'NONE',  ( 4.892620165872568094, 1.823077252308364482, -1.215776859382920794 ) ) ;
#73547 = DIRECTION ( 'NONE',  ( 0.000000000000000000, 0.000000000000000000, 1.000000000000000000 ) ) ;
#73548 = CARTESIAN_POINT ( 'NONE',  ( 3.205993170255555302, -1.924248618553949353, 0.09317337220685062427 ) ) ;
#73549 = CARTESIAN_POINT ( 'NONE',  ( -8.402302512167102222, 10.82577223566020841, -1.599625672291263179 ) ) ;
#73550 = CARTESIAN_POINT ( 'NONE',  ( -0.1294898018152357000, -0.0008549345193622873455, -1.926395771554180625 ) ) ;
#73551 = CYLINDRICAL_SURFACE ( 'NONE', #115965, 1.250000000000000000 ) ;
#73552 = EDGE_CURVE ( 'NONE', #182199, #45216, #155871, .T. ) ;
#73553 = SURFACE_STYLE_FILL_AREA ( #105012 ) ;
#73554 = CARTESIAN_POINT ( 'NONE',  ( 0.6823417656249969321, 12.77604166700806232, -1.181850606188757036 ) ) ;
#73555 = STYLED_ITEM ( 'NONE', ( #69949 ), #128748 ) ;
#73556 = CARTESIAN_POINT ( 'NONE',  ( 5.443762371086860341, 6.309809840144842141, 1.199719254218462483 ) ) ;
#73557 = CARTESIAN_POINT ( 'NONE',  ( -0.3282377607281442011, 1.301335450315356468, 1.224999999999969003 ) ) ;
#73558 = CARTESIAN_POINT ( 'NONE',  ( 5.885648082108200896, 6.039213315313952002, 0.7216878364870328300 ) ) ;
#73559 = ORIENTED_EDGE ( 'NONE', *, *, #113892, .F. ) ;
#73561 = CARTESIAN_POINT ( 'NONE',  ( 2.877592485514004039, 0.2932790309252801819, -1.991490711024199944 ) ) ;
#73560 = CARTESIAN_POINT ( 'NONE',  ( 6.356982874815331641, 0.3076174260261410054, -1.815216213958574132 ) ) ;
#73562 = CARTESIAN_POINT ( 'NONE',  ( 5.571695488097110349, 1.745893177897942738, -1.494929824115182937 ) ) ;
#73564 = CARTESIAN_POINT ( 'NONE',  ( 3.115880741807099508, 1.852434257297396858, -0.1774315261868253668 ) ) ;
#73563 = FILL_AREA_STYLE_COLOUR ( '', #19457 ) ;
#73565 = CARTESIAN_POINT ( 'NONE',  ( 3.285556943749998737, -0.6052083328553753416, -1.896917185911906500 ) ) ;
#73566 = DIRECTION ( 'NONE',  ( -1.000000000000000000, 0.000000000000000000, 0.000000000000000000 ) ) ;
#73567 = CARTESIAN_POINT ( 'NONE',  ( -7.542413527904030524, 7.693903958843159252, 1.040834085586084257E-14 ) ) ;
#73568 = CARTESIAN_POINT ( 'NONE',  ( -4.882344714696960075, 5.829061934302122161, 1.082531754730549078 ) ) ;
#73569 = CARTESIAN_POINT ( 'NONE',  ( 6.128480205876102538, 0.2055166225264984381, 2.080635545183810553 ) ) ;
#73570 = CARTESIAN_POINT ( 'NONE',  ( 6.209271165378815738, 7.306866450105836464, -1.082531754730543083 ) ) ;
#73571 = AXIS2_PLACEMENT_3D ( 'NONE', #69560, #201694, #53338 ) ;
#73572 = SURFACE_STYLE_FILL_AREA ( #105033 ) ;
#73574 = CARTESIAN_POINT ( 'NONE',  ( 4.379447312414087357, 5.068108938359919158, -1.199719254218452047 ) ) ;
#73573 = DIRECTION ( 'NONE',  ( 0.000000000000000000, 8.546850786086437571E-32, 1.000000000000000000 ) ) ;
#73575 = CARTESIAN_POINT ( 'NONE',  ( 6.024008130617486856, -0.9641997184709062418, -1.430004917837023104 ) ) ;
#73576 = CARTESIAN_POINT ( 'NONE',  ( -5.412729640353771465, 7.337937218544611895, 1.599625672291269396 ) ) ;
#73577 = CARTESIAN_POINT ( 'NONE',  ( 1.617354066682510805, 0.1696363612940926524, 1.725835137016252796 ) ) ;
#73578 = CARTESIAN_POINT ( 'NONE',  ( -11.78331023100045627, 11.29999999999999893, -1.800000000000001155 ) ) ;
#73579 = DIRECTION ( 'NONE',  ( -0.000000000000000000, 1.000000000000000000, 0.000000000000000000 ) ) ;
#73580 = CARTESIAN_POINT ( 'NONE',  ( -5.961834861707238531, 7.978559976790334574, -1.599625672291263179 ) ) ;
#73581 = CARTESIAN_POINT ( 'NONE',  ( -5.807007791129851881, 6.063258055044094874, 0.5391689476613946708 ) ) ;
#73582 = CARTESIAN_POINT ( 'NONE',  ( 6.543812728621629660, 1.490886027097729105, 1.578480410219210928 ) ) ;
#73583 = CARTESIAN_POINT ( 'NONE',  ( 5.514214477338500231, -0.8245889995748825196, -1.628937154514856545 ) ) ;
#73584 = CARTESIAN_POINT ( 'NONE',  ( 2.377722661024490147, -1.904092233959910896, 0.4717398701708991893 ) ) ;
#73585 = CARTESIAN_POINT ( 'NONE',  ( 0.08053691275167890185, 14.48195938056239385, 11.99972973886013961 ) ) ;
#73586 = CARTESIAN_POINT ( 'NONE',  ( 6.520158902582615212, 5.290451655907107309, 2.438235897557464948 ) ) ;
#73587 = CARTESIAN_POINT ( 'NONE',  ( 7.772902139336337335, 7.962807338847539107, 0.7998128361456341429 ) ) ;
#73588 = CARTESIAN_POINT ( 'NONE',  ( 3.440189854244297241, -1.264556376030629981, -1.702001827410426049 ) ) ;
#73589 = CARTESIAN_POINT ( 'NONE',  ( 6.827182134110199918, 0.5620517916639695688, 2.240906645742099190 ) ) ;
#73590 = CARTESIAN_POINT ( 'NONE',  ( -5.603170282960403092, 6.190551086330195574, -0.8764620106105174280 ) ) ;
#73591 = CARTESIAN_POINT ( 'NONE',  ( 1.639598513223254006, 1.914365469054382540, -0.7886191548351070280 ) ) ;
#73593 = CARTESIAN_POINT ( 'NONE',  ( 0.7500000000000006661, 14.94791666734946567, -1.299038105676657340 ) ) ;
#73592 = CARTESIAN_POINT ( 'NONE',  ( -11.19002393767586589, 0.9691415390508402172, 4.042856490848052431 ) ) ;
#73595 = ORIENTED_EDGE ( 'NONE', *, *, #4542, .F. ) ;
#73594 = CARTESIAN_POINT ( 'NONE',  ( 2.930584098205230248, -1.096850167032170420, -1.931549987457868989 ) ) ;
#73596 = CARTESIAN_POINT ( 'NONE',  ( 1.987358909443589283, -2.298030411116751992, 0.06136411900238383788 ) ) ;
#73598 = CARTESIAN_POINT ( 'NONE',  ( 6.965701137139799215, -0.4614044149895025204, 2.017943399502773349 ) ) ;
#73597 = CARTESIAN_POINT ( 'NONE',  ( 8.270110514656016321, 12.59228666716665401, 0.7216878364870438212 ) ) ;
#73600 = CARTESIAN_POINT ( 'NONE',  ( 1.001543065824772753E-15, -0.6125000000000012657, 4.012584370867899430 ) ) ;
#73599 = CARTESIAN_POINT ( 'NONE',  ( 5.876533236880477240, 5.820653295974182129, 0.7998128361456352531 ) ) ;
#73601 = EDGE_CURVE ( 'NONE', #88820, #29350, #197550, .T. ) ;
#73602 = CARTESIAN_POINT ( 'NONE',  ( -9.336326716892651589, 8.920000000000001705, 2.500000000000000444 ) ) ;
#73603 = CARTESIAN_POINT ( 'NONE',  ( -11.07123366811363852, 11.30000000000000071, 0.8055925608785192704 ) ) ;
#73604 = CARTESIAN_POINT ( 'NONE',  ( -10.23394195678222651, -9.091017468561377157, 0.1786341213272082673 ) ) ;
#73605 = EDGE_CURVE ( 'NONE', #182913, #202980, #165900, .T. ) ;
#73606 = CARTESIAN_POINT ( 'NONE',  ( 3.234525475359388391, 1.209690070866603406, -1.481213593849866950 ) ) ;
#73607 = CARTESIAN_POINT ( 'NONE',  ( -0.1104750535120268551, 0.2303756098476944791, -2.137063993957021513 ) ) ;
#73608 = CARTESIAN_POINT ( 'NONE',  ( 4.049579987339441800, 0.5806670320154716514, -1.624208954244592773 ) ) ;
#73609 = CARTESIAN_POINT ( 'NONE',  ( 1.815639016007553730, -1.320828798922760949, -1.523793687088881299 ) ) ;
#73610 = CARTESIAN_POINT ( 'NONE',  ( 2.602471654445730032, -0.2222675636014606049, 2.287907847288372043 ) ) ;
#73611 = CARTESIAN_POINT ( 'NONE',  ( 3.181238891614282416, -0.1630793868099291999, -2.256562113509274159 ) ) ;
#73612 = CARTESIAN_POINT ( 'NONE',  ( 5.110040610736272804, -2.096041292509024156, 0.2052846074404850174 ) ) ;
#73613 = CARTESIAN_POINT ( 'NONE',  ( -6.780486220610186798, 8.043560357867583832, -1.082531754730549967 ) ) ;
#73614 = CARTESIAN_POINT ( 'NONE',  ( 5.079261616685217362, 1.651278277306899911, -0.6370931631965012221 ) ) ;
#73616 = CARTESIAN_POINT ( 'NONE',  ( 0.5512257746139355152, -1.939593085364198721, -1.221404215731338283 ) ) ;
#73615 = CARTESIAN_POINT ( 'NONE',  ( 5.176180785367283654, 9.260904359562321275, -0.7998128361456481317 ) ) ;
#73617 = B_SPLINE_CURVE_WITH_KNOTS ( 'NONE', 3,
 ( #59727, #141028, #125886, #90114, #106399, #191844, #43507, #159361, #60795, #122697 ),
 .UNSPECIFIED., .F., .F.,
 ( 4, 1, 1, 1, 1, 1, 1, 4 ),
 ( 0.000000000000000000, 0.09853459476447307130, 0.1926867929487333375, 0.2613852218134048999, 0.3629775382994345767, 0.5216635214973427415, 0.7338723600040717443, 1.000000000000000000 ),
 .UNSPECIFIED. ) ;
#73618 = CARTESIAN_POINT ( 'NONE',  ( 5.542853976212075651, -1.453887124689148935, -1.129494548679485844 ) ) ;
#73619 = CARTESIAN_POINT ( 'NONE',  ( -4.620631424159025613, 4.285158171140619032, -0.7998128361456221525 ) ) ;
#73620 = UNCERTAINTY_MEASURE_WITH_UNIT (LENGTH_MEASURE( 1.000000000000000082E-05 ), #75431, 'distance_accuracy_value', 'NONE');
#73621 = CARTESIAN_POINT ( 'NONE',  ( 5.771465802492605768, 1.302860414194568550, 1.761948869136241047 ) ) ;
#73622 = CARTESIAN_POINT ( 'NONE',  ( -2.611917148927046295, 6.198987107056845858, 1.040834085586084257E-14 ) ) ;
#73623 = CARTESIAN_POINT ( 'NONE',  ( -10.61081979358358041, -7.079050064870600067, 0.4638907948587486230 ) ) ;
#73624 = CARTESIAN_POINT ( 'NONE',  ( 5.986797818411375260, 1.994257276370488219, 0.5558945855626205024 ) ) ;
#73625 = EDGE_CURVE ( 'NONE', #37843, #34325, #132372, .T. ) ;
#73626 = CARTESIAN_POINT ( 'NONE',  ( -0.01248194115436446205, -0.5331630387654020531, 1.944732228473695868 ) ) ;
#73627 = VECTOR ( 'NONE', #50437, 1000.000000000000000 ) ;
#73628 = CARTESIAN_POINT ( 'NONE',  ( -0.7500000000000249800, -0.5270833326505158789, 1.299038105676659116 ) ) ;
#73629 = CARTESIAN_POINT ( 'NONE',  ( 4.002502541323429419, -0.6052661472178870739, -1.829015351804675005 ) ) ;
#73630 = CARTESIAN_POINT ( 'NONE',  ( 1.364683531249997417, 9.984375000341398021, 2.602085213965210642E-15 ) ) ;
#73631 = CYLINDRICAL_SURFACE ( 'NONE', #126322, 11.10000000000000320 ) ;
#73632 = CARTESIAN_POINT ( 'NONE',  ( 1.002519415922138002, -0.9925456330053865628, 1.987394366727333717 ) ) ;
#73634 = VERTEX_POINT ( 'NONE', #184261 ) ;
#73633 = CARTESIAN_POINT ( 'NONE',  ( 4.927462483923885195, 4.713404084191450849, -0.7998128361456481317 ) ) ;
#73637 = CIRCLE ( 'NONE', #153117, 0.07999999999999933553 ) ;
#73636 = FACE_OUTER_BOUND ( 'NONE', #146579, .T. ) ;
#73635 = CARTESIAN_POINT ( 'NONE',  ( -4.340018570150322219, 5.196348098997705556, -1.082531754730551743 ) ) ;
#73638 = CARTESIAN_POINT ( 'NONE',  ( 2.679707916995359263, 6.278076336469897711, -0.7998128361456291469 ) ) ;
#73639 = CARTESIAN_POINT ( 'NONE',  ( -0.7500000000000179856, 9.072916667349467446, 1.299038105676658228 ) ) ;
#73640 = LINE ( 'NONE', #92053, #90672 ) ;
#73641 = CARTESIAN_POINT ( 'NONE',  ( 10.35124615470471277, 10.47624511309397199, -5.983076183620329225 ) ) ;
#73642 = CARTESIAN_POINT ( 'NONE',  ( 9.449669878600614581, 12.04770082983265844, -1.443375672974058777 ) ) ;
#73643 = CARTESIAN_POINT ( 'NONE',  ( 1.293326634533353170, -1.775083115552608559, 0.8357255594537355003 ) ) ;
#73644 = CARTESIAN_POINT ( 'NONE',  ( 1.364683531249988535, 2.967708333674755394, -0.7879004041258239610 ) ) ;
#73645 = CARTESIAN_POINT ( 'NONE',  ( 0.4169036860910191322, 3.145283463680761393, -0.4342470185719746190 ) ) ;
#73646 = CARTESIAN_POINT ( 'NONE',  ( 6.602011099637477010, 0.7519813002578833450, -1.812223124677159181 ) ) ;
#73647 = CARTESIAN_POINT ( 'NONE',  ( -8.134002093194872884, 11.57708731111429401, 1.199719254218453823 ) ) ;
#73648 = CARTESIAN_POINT ( 'NONE',  ( -4.067082893975237035, 7.688754443039000464, 1.040834085586084257E-14 ) ) ;
#73649 = CARTESIAN_POINT ( 'NONE',  ( 0.07556134207191073093, -0.004209888912004143384, -2.244269416743961187 ) ) ;
#73651 = ORIENTED_EDGE ( 'NONE', *, *, #47472, .T. ) ;
#73650 = CARTESIAN_POINT ( 'NONE',  ( -5.042743069279040036, 7.970618449879118828, 1.199719254218464037 ) ) ;
#73652 = CARTESIAN_POINT ( 'NONE',  ( 0.6823417656249917140, 5.592708333674749177, 1.181850606188765695 ) ) ;
#73653 = CARTESIAN_POINT ( 'NONE',  ( 0.8955150854165813135, -0.6789544621725839280, 1.743152336062703256 ) ) ;
#73654 = CARTESIAN_POINT ( 'NONE',  ( 0.6504783628028444342, 0.8526279987398683868, 1.509985294034902337 ) ) ;
#73656 = CARTESIAN_POINT ( 'NONE',  ( 4.388337494309430653, -0.4807229498768311182, -2.138019847805587403 ) ) ;
#73655 = CARTESIAN_POINT ( 'NONE',  ( 1.360316468749949825, 2.244791667008100511, 0.7853790794158780342 ) ) ;
#73657 = CARTESIAN_POINT ( 'NONE',  ( 4.964078638949532163, 2.283327717301757431, -0.3329734184051634238 ) ) ;
#73658 = CARTESIAN_POINT ( 'NONE',  ( 6.608673410152685612, 1.530114183832030905, -1.380643333410998430 ) ) ;
#73659 = CARTESIAN_POINT ( 'NONE',  ( 2.413922445368326564, 1.268163163618090561, -1.470779158573028322 ) ) ;
#73660 = CARTESIAN_POINT ( 'NONE',  ( -4.568734577680875653, 8.274014740695587733, -0.7216878364870257245 ) ) ;
#73661 = CARTESIAN_POINT ( 'NONE',  ( 1.387358672534392046, 7.251968950353694154, -4.302625267138185272 ) ) ;
#73662 = CARTESIAN_POINT ( 'NONE',  ( 4.887034483293543730, -1.997634423138573867, -0.7120497732875651353 ) ) ;
#73663 = CARTESIAN_POINT ( 'NONE',  ( 0.6801582343750038895, 0.3072916670080680368, -1.178068619123848526 ) ) ;
#73664 = CARTESIAN_POINT ( 'NONE',  ( 3.656875104409584853, 1.122498086849915921, 1.674887873639265390 ) ) ;
#73665 = CARTESIAN_POINT ( 'NONE',  ( -5.056828107772860292, 6.922718763866881453, -1.443375672974051449 ) ) ;
#73666 = CARTESIAN_POINT ( 'NONE',  ( -8.093291352714894415, 8.406871097780989288, -0.7998128361456362523 ) ) ;
#73667 = CARTESIAN_POINT ( 'NONE',  ( 8.075853055234393452, 12.57357899774884658, 0.7998128361456462443 ) ) ;
#73668 = CARTESIAN_POINT ( 'NONE',  ( 0.4690313652776016418, 0.1822212253758948297, -1.816563760317004395 ) ) ;
#73669 = CARTESIAN_POINT ( 'NONE',  ( -5.088052786878465739, 9.158088361325352977, 0.000000000000000000 ) ) ;
#73670 = CARTESIAN_POINT ( 'NONE',  ( -5.608413262169404945, 5.655525674710887962, 0.4595228360113173260 ) ) ;
#73671 = CARTESIAN_POINT ( 'NONE',  ( -10.80846816847880909, 4.295462489797631456, 4.678010962757586100 ) ) ;
#73672 = VERTEX_POINT ( 'NONE', #36953 ) ;
#73673 = CARTESIAN_POINT ( 'NONE',  ( 5.049710947255391602, 0.6486796242286404501, -1.956199288699921768 ) ) ;
#73674 = CARTESIAN_POINT ( 'NONE',  ( -7.092323753280154186, 7.447001598347859463, 0.7216878364870317197 ) ) ;
#73675 = CARTESIAN_POINT ( 'NONE',  ( -3.415764635639130020, 6.072476943965863683, 1.199719254218462483 ) ) ;
#73676 = CARTESIAN_POINT ( 'NONE',  ( -9.755255220232635693, 11.33988483081495957, -1.199719254218441611 ) ) ;
#73677 = CARTESIAN_POINT ( 'NONE',  ( 4.986975786537023225, -1.902434985030461156, -0.6785184294546533490 ) ) ;
#73679 = ORIENTED_EDGE ( 'NONE', *, *, #41144, .T. ) ;
#73678 = CARTESIAN_POINT ( 'NONE',  ( 6.041669411999269990, -2.092492953876758044, 0.7457244993839227121 ) ) ;
#73681 = CARTESIAN_POINT ( 'NONE',  ( 6.616015773788773480, 10.66250946948817813, -0.7216878364870267237 ) ) ;
#73680 = CARTESIAN_POINT ( 'NONE',  ( -3.383641855062333281, 6.105276709951447778, -1.199719254218452047 ) ) ;
#73682 = CIRCLE ( 'NONE', #194731, 10.25000000000000000 ) ;
#73683 = CARTESIAN_POINT ( 'NONE',  ( 6.654354466208897811, 6.657835053532175529, 0.7998128361456341429 ) ) ;
#73684 = CARTESIAN_POINT ( 'NONE',  ( 4.153237585930975584, -1.712380083513395768, -1.146421031332397922 ) ) ;
#73685 = CARTESIAN_POINT ( 'NONE',  ( 4.236954046275762664, 2.015912997090345549, -0.05229627655192746472 ) ) ;
#73686 = VERTEX_POINT ( 'NONE', #51084 ) ;
#73687 = CARTESIAN_POINT ( 'NONE',  ( 0.1753634416057497925, 0.0001173177735149660839, -2.144164757042037017 ) ) ;
#73688 = CARTESIAN_POINT ( 'NONE',  ( -1.880721860161314041, 2.480169305151522341, 2.464325445266503323 ) ) ;
#73690 = ORIENTED_EDGE ( 'NONE', *, *, #21981, .T. ) ;
#73689 = CARTESIAN_POINT ( 'NONE',  ( -7.456058132872594335, 7.663432341298296535, 0.000000000000000000 ) ) ;
#73691 = CARTESIAN_POINT ( 'NONE',  ( 4.807910157829258679, 8.239027388120819140, -0.8806314816870459694 ) ) ;
#73692 = CARTESIAN_POINT ( 'NONE',  ( 3.620470095612156047, 0.4925664443866035191, -1.954873191151075940 ) ) ;
#73693 = CARTESIAN_POINT ( 'NONE',  ( 3.064218985076866630, -1.701416833343888824, -0.7040189834505713451 ) ) ;
#73694 = CARTESIAN_POINT ( 'NONE',  ( 2.679285714285720044, 0.4970443252110459120, -0.09999999999999592548 ) ) ;
#73695 = CARTESIAN_POINT ( 'NONE',  ( 1.506910664365119334, -0.8341063803433286239, -2.151852887045426765 ) ) ;
#73696 = CARTESIAN_POINT ( 'NONE',  ( 5.982890925380405456, 10.20206618957764100, 0.000000000000000000 ) ) ;
#73697 = CARTESIAN_POINT ( 'NONE',  ( 3.708425082824120533, -0.8722964037291662809, -1.977944213000272455 ) ) ;
#73698 = CARTESIAN_POINT ( 'NONE',  ( 9.596473800374404561, 10.09030761005864285, 0.000000000000000000 ) ) ;
#73699 = CARTESIAN_POINT ( 'NONE',  ( -4.903245109636583443, 8.872203061218007392, -0.7998128361456281477 ) ) ;
#73700 = CARTESIAN_POINT ( 'NONE',  ( 3.374663776259867909, -0.4515557078652779333, 2.253457335377069271 ) ) ;
#73701 = CARTESIAN_POINT ( 'NONE',  ( 0.07802162204156329328, -7.185026885903937455, -9.499679971350921903 ) ) ;
#73702 = VECTOR ( 'NONE', #23563, 1000.000000000000000 ) ;
#73703 = CARTESIAN_POINT ( 'NONE',  ( 2.606148294764852213, -0.7140300644919925777, -1.729217693616967644 ) ) ;
#73704 = AXIS2_PLACEMENT_3D ( 'NONE', #78379, #94662, #113090 ) ;
#73705 = CARTESIAN_POINT ( 'NONE',  ( 0.3507686748964663481, -1.586079953665324060, 1.170567870040557290 ) ) ;
#73707 = CARTESIAN_POINT ( 'NONE',  ( 2.501185699981960830, -0.1928336239410358699, 2.007256303757164240 ) ) ;
#73706 = CARTESIAN_POINT ( 'NONE',  ( -1.364683531250010295, 5.238541667008086655, -0.7879004041258300672 ) ) ;
#73709 = CARTESIAN_POINT ( 'NONE',  ( 1.348561525465460820, 2.204488851003219896, 0.1053889787279923829 ) ) ;
#73708 = CARTESIAN_POINT ( 'NONE',  ( -4.713430959045263435, 8.650753218861462202, 0.7998128361456481317 ) ) ;
#73710 = CARTESIAN_POINT ( 'NONE',  ( 4.547870462380197765, 7.393267075163835855, 1.199719254218462483 ) ) ;
#73711 = CARTESIAN_POINT ( 'NONE',  ( -5.250031796989778066, 7.148123067953287446, 1.599625672291267398 ) ) ;
#73712 = CARTESIAN_POINT ( 'NONE',  ( -7.778383330260348671, -5.907420853759295376, 7.778383330260377981 ) ) ;
#73713 = CARTESIAN_POINT ( 'NONE',  ( 5.594591524781380443, -0.4782570758292312707, -1.912467619381743811 ) ) ;
#73714 = CARTESIAN_POINT ( 'NONE',  ( 5.619831112054756161, -2.252673335196005766, 0.5002786026085581650 ) ) ;
#73715 = CARTESIAN_POINT ( 'NONE',  ( 0.1507198084474276056, -0.4258245693303016610, -1.922078969575198526 ) ) ;
#73716 = CARTESIAN_POINT ( 'NONE',  ( 3.432538798476657327, -1.232314722524804562, 1.653799735942045990 ) ) ;
#73717 = CARTESIAN_POINT ( 'NONE',  ( 5.504247177468175600, 8.405076892812779477, 1.082531754730558626 ) ) ;
#73718 = VECTOR ( 'NONE', #12066, 1000.000000000000000 ) ;
#73719 = CARTESIAN_POINT ( 'NONE',  ( 7.452141709366786770, 8.723195411463290583, 1.199719254218452047 ) ) ;
#73720 = CARTESIAN_POINT ( 'NONE',  ( 6.683806541412754321, 8.820860269780128604, -1.443375672974058777 ) ) ;
#73721 = CARTESIAN_POINT ( 'NONE',  ( -1.201851678989727383E-14, 2.884375000341418804, 1.575800808251672791 ) ) ;
#73722 = CARTESIAN_POINT ( 'NONE',  ( -8.117903383641394299, 14.55181945421660927, 8.822823676310077801 ) ) ;
#73723 = CARTESIAN_POINT ( 'NONE',  ( 5.653386866774156694, 5.697965554099049257, -0.7216878364870207285 ) ) ;
#73724 = CARTESIAN_POINT ( 'NONE',  ( 4.791568617006563002, -1.986896891843348723, 0.8757425373496147136 ) ) ;
#73726 = CARTESIAN_POINT ( 'NONE',  ( 5.284640796330934087, 1.621094592300664328, -0.8731043043393662550 ) ) ;
#73725 = CARTESIAN_POINT ( 'NONE',  ( -2.168941388506379742, 5.474256019991960542, -0.7216878364870267237 ) ) ;
#73727 = B_SPLINE_CURVE_WITH_KNOTS ( 'NONE', 3,
 ( #89163, #170381, #39325, #155217 ),
 .UNSPECIFIED., .F., .F.,
 ( 4, 4 ),
 ( 0.000000000000000000, 9.170750103614400562E-05 ),
 .UNSPECIFIED. ) ;
#73729 = CARTESIAN_POINT ( 'NONE',  ( 11.89844258446855285, 12.27147310670036973, 1.560502987793273233 ) ) ;
#73728 = CARTESIAN_POINT ( 'NONE',  ( -11.91294103507080315, 11.11460089956407060, 1.446263142085468134 ) ) ;
#73730 = DIRECTION ( 'NONE',  ( 0.05872483221476459958, 0.000000000000000000, 0.9982742078614211811 ) ) ;
#73731 = CARTESIAN_POINT ( 'NONE',  ( 0.4911964603225346115, 1.381658100223854380, 1.261112594198803061 ) ) ;
#73732 = CARTESIAN_POINT ( 'NONE',  ( 0.2282871097136250915, -1.394050316402313916, -1.782836666206646603 ) ) ;
#73733 = CARTESIAN_POINT ( 'NONE',  ( -4.418103850092305329, 7.323797853316306394, 1.240345400901581296 ) ) ;
#73734 = DIRECTION ( 'NONE',  ( 0.000000000000000000, 0.000000000000000000, -1.000000000000000000 ) ) ;
#73735 = CARTESIAN_POINT ( 'NONE',  ( 5.652821694808577213, 7.451312062667313718, 1.328372732707931103 ) ) ;
#73736 = CARTESIAN_POINT ( 'NONE',  ( -5.302647476276252547, 5.359045941843285199, 0.7216878364870257245 ) ) ;
#73737 = CARTESIAN_POINT ( 'NONE',  ( 11.44789321844504215, 13.79999999999999893, -3.303298730975399167 ) ) ;
#73738 = CARTESIAN_POINT ( 'NONE',  ( 2.342341949348641261, 0.3848992280063111004, 1.727307115810622351 ) ) ;
#73739 = CARTESIAN_POINT ( 'NONE',  ( 6.147140879040452255, 0.1997598139246952731, 2.003170966399501651 ) ) ;
#73741 = CARTESIAN_POINT ( 'NONE',  ( 3.321808155663192874, 0.8583493116562285197, -1.712590381118280991 ) ) ;
#73740 = CARTESIAN_POINT ( 'NONE',  ( -8.967828540435322182, 12.54988483289483980, 1.199719254218462483 ) ) ;
#73742 = CARTESIAN_POINT ( 'NONE',  ( -5.199652918878400189E-15, 3.038454817776198968, -11.99999999999998579 ) ) ;
#73743 = CARTESIAN_POINT ( 'NONE',  ( 4.773860271397749599, -1.931934984910467890, 0.3821518213343431669 ) ) ;
#73745 = EDGE_CURVE ( 'NONE', #53448, #114068, #117209, .T. ) ;
#73744 = CARTESIAN_POINT ( 'NONE',  ( 6.328379800955010737, -0.9556441952764772596, -1.779432800462784847 ) ) ;
#73746 = CARTESIAN_POINT ( 'NONE',  ( -2.788906526875773208E-15, 10.93750000000000178, -1.499999999999998446 ) ) ;
#73747 = CARTESIAN_POINT ( 'NONE',  ( 2.447944060942487621, 1.870205405844455049, 0.04815357881200743595 ) ) ;
#73749 = VERTEX_POINT ( 'NONE', #202635 ) ;
#73748 = CARTESIAN_POINT ( 'NONE',  ( 6.568995754424670430, -1.580519633186812767, -0.6912669513192554183 ) ) ;
#73751 = CARTESIAN_POINT ( 'NONE',  ( 3.633221978782282147, 5.261844946711204507, -1.443375672974057666 ) ) ;
#73750 = CARTESIAN_POINT ( 'NONE',  ( 2.684424123961434816, -1.133677649706768431, 1.893296980138805097 ) ) ;
#73752 = CARTESIAN_POINT ( 'NONE',  ( 1.364683531249988535, 3.467708333674749621, -0.7879004041258239610 ) ) ;
#73753 = CARTESIAN_POINT ( 'NONE',  ( 6.654749070045313353, -0.5220710138904552933, -1.891073168474053823 ) ) ;
#73755 = EDGE_CURVE ( 'NONE', #8935, #208480, #67973, .T. ) ;
#73754 = CARTESIAN_POINT ( 'NONE',  ( 7.564559641420864899, 10.91273778404466199, -1.199719254218446718 ) ) ;
#73756 = CARTESIAN_POINT ( 'NONE',  ( -10.64045162862669081, 11.30828174301964140, -0.7998128361456221525 ) ) ;
#73757 = LINE ( 'NONE', #121531, #33310 ) ;
#73758 = CARTESIAN_POINT ( 'NONE',  ( -3.420146311865638555, -0.02861402253355461306, -0.3000856501258975517 ) ) ;
#73759 = DIRECTION ( 'NONE',  ( 1.000000000000000000, 6.532318089225149424E-16, -4.440892098500620245E-16 ) ) ;
#73760 = CARTESIAN_POINT ( 'NONE',  ( 2.154816067267216084, -0.5500195584662926906, -1.995915215819036748 ) ) ;
#73761 = CARTESIAN_POINT ( 'NONE',  ( -1.499999999999997780, 3.400000000000021227, 1.214306433183764966E-14 ) ) ;
#73762 = CARTESIAN_POINT ( 'NONE',  ( 3.974511587100456822, 7.788680618259193444, 1.040834085586084257E-14 ) ) ;
#73763 = CARTESIAN_POINT ( 'NONE',  ( 4.903208829997618423, 5.749440385532527564, -1.199719254218450271 ) ) ;
#73764 = CARTESIAN_POINT ( 'NONE',  ( 6.024112365460934981, -2.104525519549589330, 0.2592714029671301934 ) ) ;
#73765 = CARTESIAN_POINT ( 'NONE',  ( 1.499999999999993117, 10.38541666734946212, 0.8660254037844408170 ) ) ;
#73766 = CARTESIAN_POINT ( 'NONE',  ( -1.364683531250012516, 3.738541667008087099, -0.7879004041258300672 ) ) ;
#73768 = CARTESIAN_POINT ( 'NONE',  ( 8.270110514656016321, 12.59228666716665401, 0.7216878364870438212 ) ) ;
#73767 = CARTESIAN_POINT ( 'NONE',  ( 0.07479286986305544449, 2.046156589154801253, -2.272744413733415403 ) ) ;
#73769 = CARTESIAN_POINT ( 'NONE',  ( 5.536482449520531368, 1.943773098233076757, -0.5350085594507183462 ) ) ;
#73770 = CARTESIAN_POINT ( 'NONE',  ( 4.733546111355320107, 0.5950593785610300834, -1.821060146467222918 ) ) ;
#73771 = CARTESIAN_POINT ( 'NONE',  ( 6.539320575229251808, 7.629137130509035636, 2.603262396134010892 ) ) ;
#73772 = CARTESIAN_POINT ( 'NONE',  ( 3.614928802375876771, -0.1595779646587774658, 2.185787688459623901 ) ) ;
#73773 = CARTESIAN_POINT ( 'NONE',  ( -0.7500000000000006661, 1.389583334016154748, -1.299038105676652011 ) ) ;
#73774 = CARTESIAN_POINT ( 'NONE',  ( 2.214975196874233720, 1.533708969217022933, -1.142120075431733994 ) ) ;
#73775 = CARTESIAN_POINT ( 'NONE',  ( -6.905180308061733996, 6.950465202360470052, 0.7998128361456341429 ) ) ;
#73777 = CARTESIAN_POINT ( 'NONE',  ( 6.257425474675967436, 2.026018168931587482, -0.6146651352928398371 ) ) ;
#73776 = DIRECTION ( 'NONE',  ( 0.000000000000000000, 0.000000000000000000, 1.000000000000000000 ) ) ;
#73778 = CARTESIAN_POINT ( 'NONE',  ( -1.364683531250010295, 9.692708333674737275, 0.7879004041258445001 ) ) ;
#73780 = CARTESIAN_POINT ( 'NONE',  ( -6.469175572376043348, 7.576401584974034265, 1.199719254218452047 ) ) ;
#73779 = CARTESIAN_POINT ( 'NONE',  ( 5.653911837654605144, 0.8871495062587383407, 2.004161502255866090 ) ) ;
#73782 = VERTEX_POINT ( 'NONE', #85704 ) ;
#73781 = CARTESIAN_POINT ( 'NONE',  ( 3.363966847960923268, 0.7745139696748448710, 1.541148353905038126 ) ) ;
#73783 = CARTESIAN_POINT ( 'NONE',  ( 6.205353461901607304, 1.844339991697005798, -1.046509186232460920 ) ) ;
#73784 = CARTESIAN_POINT ( 'NONE',  ( 9.433775957010412938, 9.900493459467314850, 0.000000000000000000 ) ) ;
#73785 = CARTESIAN_POINT ( 'NONE',  ( 3.985207087413062066, 6.736826471035503694, -1.199719254218452047 ) ) ;
#73786 = CARTESIAN_POINT ( 'NONE',  ( -1.247849810309911600, 13.37576698399836594, 0.5524780460566154350 ) ) ;
#73787 = ADVANCED_FACE ( 'NONE', ( #3366 ), #101963, .T. ) ;
#73788 = CARTESIAN_POINT ( 'NONE',  ( 0.3265133270617843197, -1.284392789319420913, 1.483054880892266114 ) ) ;
#73789 = DIRECTION ( 'NONE',  ( 5.551115123125765446E-17, 0.000000000000000000, -1.000000000000000000 ) ) ;
#73790 = CARTESIAN_POINT ( 'NONE',  ( 6.491656622844908853, 6.468020902940851968, 0.7998128361456341429 ) ) ;
#73791 = DIRECTION ( 'NONE',  ( 0.7927788072564095900, 0.000000000000000000, -0.6095094443608766177 ) ) ;
#73792 = ORIENTED_EDGE ( 'NONE', *, *, #80476, .T. ) ;
#73793 = CARTESIAN_POINT ( 'NONE',  ( -11.86239285000046095, 13.80000000000000249, -1.812080536912752837 ) ) ;
#73794 = EDGE_LOOP ( 'NONE', ( #109038, #53020, #59708, #99794, #43556, #94413, #41231 ) ) ;
#73795 = CARTESIAN_POINT ( 'NONE',  ( 2.754343952779594318, 1.798010375687082218, 0.2196673718751484539 ) ) ;
#73796 = EDGE_LOOP ( 'NONE', ( #41320, #69303, #122411, #125420, #12521, #57092, #126968, #164386, #96016, #155567, #100425, #53208, #63489, #46583, #22850, #14621, #11132, #98845, #24005, #156196, #126971, #36488, #110625, #120485, #109540, #83771, #57021 ) ) ;
#73797 = CARTESIAN_POINT ( 'NONE',  ( 10.70146331988817323, 11.37946204949139251, 0.7998128361456341429 ) ) ;
#73798 = CIRCLE ( 'NONE', #97945, 11.09999999999999964 ) ;
#73799 = CARTESIAN_POINT ( 'NONE',  ( 5.194709132691408549, 6.089524072008651423, 1.199719254218452935 ) ) ;
#73800 = CARTESIAN_POINT ( 'NONE',  ( 4.283730857329768327, 1.755957581118623434, -0.4444456398857503099 ) ) ;
#73801 = CARTESIAN_POINT ( 'NONE',  ( 5.980555156959511898, 9.991415093179179863, -0.7216878364870458196 ) ) ;
#73802 = DIRECTION ( 'NONE',  ( -1.276756478318932585E-15, 1.000000000000000000, -1.665334536937738262E-16 ) ) ;
#73803 = CARTESIAN_POINT ( 'NONE',  ( 5.872608658597049391, 5.988986745869715023, 0.2392922861021197500 ) ) ;
#73805 = CARTESIAN_POINT ( 'NONE',  ( -8.012344526598182026E-15, 14.04687500034139624, -1.575800808251669460 ) ) ;
#73804 = CARTESIAN_POINT ( 'NONE',  ( 5.142936340713559318, -0.2273772366201456396, -1.847015746109672119 ) ) ;
#73806 = CARTESIAN_POINT ( 'NONE',  ( 3.216317514422084578, 1.869562491224942224, 0.4167181705077570575 ) ) ;
#73807 = CARTESIAN_POINT ( 'NONE',  ( 1.412830140145465263, 1.608106816955911178, 0.8641515426408912237 ) ) ;
#73808 = FACE_OUTER_BOUND ( 'NONE', #36198, .T. ) ;
#73809 = CARTESIAN_POINT ( 'NONE',  ( -10.71030397718323890, 6.055815897892919075, -4.668189396100475008 ) ) ;
#73810 = B_SPLINE_CURVE_WITH_KNOTS ( 'NONE', 3,
 ( #45905, #129359, #13371, #32829 ),
 .UNSPECIFIED., .F., .F.,
 ( 4, 4 ),
 ( 0.000000000000000000, 0.0002847049822659113399 ),
 .UNSPECIFIED. ) ;
#73811 = CARTESIAN_POINT ( 'NONE',  ( 5.916355900263067014, 7.140870225795406867, 1.119544393390920600 ) ) ;
#73812 = CARTESIAN_POINT ( 'NONE',  ( -11.41108574530292863, 9.841631446223672697, 3.405883542057530633 ) ) ;
#73813 = B_SPLINE_CURVE_WITH_KNOTS ( 'NONE', 3,
 ( #26337, #5791, #173697, #104407, #208279, #170456, #71868, #142268, #41556, #25273 ),
 .UNSPECIFIED., .F., .F.,
 ( 4, 3, 3, 4 ),
 ( 1.740265443795535820E-15, 3.125156195614331076E-05, 5.753630127952281341E-05, 8.382839040627577314E-05 ),
 .UNSPECIFIED. ) ;
#73814 = CARTESIAN_POINT ( 'NONE',  ( -6.329301559086026430, 6.910747120380293929, 0.8034454130101459368 ) ) ;
#73815 = CARTESIAN_POINT ( 'NONE',  ( -4.217958839219735800, 3.978389137448586244, 0.5316758947214468289 ) ) ;
#73816 = CARTESIAN_POINT ( 'NONE',  ( 5.802526556968819804, 9.713438716531550554, -0.7216878364870267237 ) ) ;
#73817 = CARTESIAN_POINT ( 'NONE',  ( -4.223528545856940042, 4.886203710709899006, -1.199719254218446718 ) ) ;
#73818 = CARTESIAN_POINT ( 'NONE',  ( -9.499679971350920127, -7.185026885903970317, -0.07802162204179896587 ) ) ;
#73819 = CARTESIAN_POINT ( 'NONE',  ( 1.500065138910465334, -0.7538795759346494929, -1.950162888426725250 ) ) ;
#73820 = CARTESIAN_POINT ( 'NONE',  ( 6.106463915388694375, -0.6937866221692154944, -1.797298315204816310 ) ) ;
#73821 = CARTESIAN_POINT ( 'NONE',  ( -6.403528624356093601, 6.365204904703887223, 1.040834085586084257E-14 ) ) ;
#73822 = CARTESIAN_POINT ( 'NONE',  ( 2.045663570152244315, 0.7015605659913305425, -1.685594894050304493 ) ) ;
#73823 = CARTESIAN_POINT ( 'NONE',  ( 3.035963658818414235, -1.482449291622448095, -1.634993338104336891 ) ) ;
#73824 = ADVANCED_FACE ( 'NONE', ( #166974 ), #121582, .T. ) ;
#73825 = CARTESIAN_POINT ( 'NONE',  ( 11.89942855770814312, 12.30000000000000071, 0.6999999999999992895 ) ) ;
#73826 = CARTESIAN_POINT ( 'NONE',  ( 1.300873410958070409, -0.2835801433653042380, -1.891145142470892715 ) ) ;
#73827 = ORIENTED_EDGE ( 'NONE', *, *, #73345, .F. ) ;
#73828 = CARTESIAN_POINT ( 'NONE',  ( 1.416386825446398712, 0.7951318926605431825, 1.802096770617849897 ) ) ;
#73829 = CARTESIAN_POINT ( 'NONE',  ( 3.104954810669264376, -0.3761875069782861236, 1.905116956637223913 ) ) ;
#73830 = VERTEX_POINT ( 'NONE', #120422 ) ;
#73831 = CARTESIAN_POINT ( 'NONE',  ( -1.123270288254055060, 3.033552654332631437, 0.7749999999939940487 ) ) ;
#73833 = CARTESIAN_POINT ( 'NONE',  ( 6.825069993440997074, -1.701324435194497831, -0.7545304760708021474 ) ) ;
#73832 = CARTESIAN_POINT ( 'NONE',  ( -5.330290668828105538, 6.247702530834755130, 1.199719254218452935 ) ) ;
#73834 = CARTESIAN_POINT ( 'NONE',  ( 5.032011289327418702, 5.899709921417326974, 1.199719254218452935 ) ) ;
#73835 = CARTESIAN_POINT ( 'NONE',  ( 0.000000000000000000, 3.956598013261175772, 0.000000000000000000 ) ) ;
#73836 = CARTESIAN_POINT ( 'NONE',  ( 10.39640486358069360, 11.02356051713265650, 0.7998128361456462443 ) ) ;
#73837 = CARTESIAN_POINT ( 'NONE',  ( -5.101610940492132151, 9.173906207207963348, -0.7998128361456362523 ) ) ;
#73838 = CARTESIAN_POINT ( 'NONE',  ( 2.366952063387484095, 0.1042156695447923470, -2.189191704635709890 ) ) ;
#73839 = CARTESIAN_POINT ( 'NONE',  ( -11.01135777277262129, 10.19999999999999929, -1.400000000000001910 ) ) ;
#73840 = VERTEX_POINT ( 'NONE', #38033 ) ;
#73841 = CARTESIAN_POINT ( 'NONE',  ( 7.035755370848908896, 7.173079118937375931, 0.7998128361456352531 ) ) ;
#73842 = CYLINDRICAL_SURFACE ( 'NONE', #186052, 1.250000000000000000 ) ;
#73844 = ADVANCED_FACE ( 'NONE', ( #150732 ), #191527, .T. ) ;
#73843 = CARTESIAN_POINT ( 'NONE',  ( 2.578497204056416692, -1.747032809129964503, -0.5301130021647950663 ) ) ;
#73845 = CARTESIAN_POINT ( 'NONE',  ( -2.788906526875773208E-15, 12.96875000068279782, -1.499999999999998446 ) ) ;
#73846 = CARTESIAN_POINT ( 'NONE',  ( -8.188761592974033832, 12.49737959187099179, -0.7216878364870267237 ) ) ;
#73847 = CARTESIAN_POINT ( 'NONE',  ( -4.588266729941921973, 8.494429388143421633, -0.1275441020149002680 ) ) ;
#73848 = CARTESIAN_POINT ( 'NONE',  ( -3.023105066167347310, 5.702484939155337607, 2.420000000000010587 ) ) ;
#73849 = CARTESIAN_POINT ( 'NONE',  ( 6.916630921265960019, 11.22115317478565188, 0.7998128361456462443 ) ) ;
#73850 = CARTESIAN_POINT ( 'NONE',  ( 2.684106373981818727, -0.9902706917056921521, 1.652370099195903386 ) ) ;
#73851 = CARTESIAN_POINT ( 'NONE',  ( 6.315287901512626867, -1.680818388338392699, -1.011408691396285420 ) ) ;
#73852 = CARTESIAN_POINT ( 'NONE',  ( -1.500000000000008216, 15.25000000000000000, 3.469446951953614189E-15 ) ) ;
#73853 = CARTESIAN_POINT ( 'NONE',  ( -7.172426956829277778, 8.326585190177668849, -1.199719254218452935 ) ) ;
#73854 = CARTESIAN_POINT ( 'NONE',  ( 4.684505768721569652, 5.424010470718658716, -1.199719254218452047 ) ) ;
#73855 = CARTESIAN_POINT ( 'NONE',  ( -4.706088717274938382, 6.583799151611112954, 1.443375672974058777 ) ) ;
#73856 = VECTOR ( 'NONE', #83577, 1000.000000000000000 ) ;
#73857 = AXIS2_PLACEMENT_3D ( 'NONE', #176958, #180157, #195342 ) ;
#73858 = CARTESIAN_POINT ( 'NONE',  ( 9.728138913005292210, 11.30824913904973705, -1.199719254218440723 ) ) ;
#73859 = CARTESIAN_POINT ( 'NONE',  ( 11.92045683181315674, 13.65275927879483042, 1.382340670101856350 ) ) ;
#73860 = CARTESIAN_POINT ( 'NONE',  ( 5.471561611210747245, -0.3092806512635417060, 2.046926588373791933 ) ) ;
#73862 = CARTESIAN_POINT ( 'NONE',  ( 0.6823417656249899377, 3.238541667008085323, -1.181850606188754593 ) ) ;
#73861 = CARTESIAN_POINT ( 'NONE',  ( -0.1121326479804653220, -0.4008509640632436088, -1.803546454093779561 ) ) ;
#73863 = CIRCLE ( 'NONE', #46209, 10.99999999999999112 ) ;
#73864 = CARTESIAN_POINT ( 'NONE',  ( 5.309350125645185159, 1.371050412704700516, -1.844953357796705218 ) ) ;
#73865 = CARTESIAN_POINT ( 'NONE',  ( 5.992340707560147806, 8.974519344586754599, 1.082531754730558626 ) ) ;
#73867 = CARTESIAN_POINT ( 'NONE',  ( -8.914213045750475573, 3.487142912321096855, -8.026393478126237824 ) ) ;
#73866 = CARTESIAN_POINT ( 'NONE',  ( 3.743459811148990291, 7.381470523066878009, -0.7216878364870338292 ) ) ;
#73868 = CARTESIAN_POINT ( 'NONE',  ( 0.006404353242023088852, -0.9848532314915852126, -2.067437341614616120 ) ) ;
#73870 = ADVANCED_FACE ( 'NONE', ( #22815 ), #149150, .T. ) ;
#73869 = CARTESIAN_POINT ( 'NONE',  ( -10.91944002402978775, -9.900000000000005684, 0.1105873483556694958 ) ) ;
#73871 = CARTESIAN_POINT ( 'NONE',  ( -6.720001414228860881, 7.869031733802326123, -1.199719254218452047 ) ) ;
#73872 = CARTESIAN_POINT ( 'NONE',  ( 4.488185891274095063, -0.4267898533511414461, -1.894319381339019559 ) ) ;
#73873 = ORIENTED_EDGE ( 'NONE', *, *, #204859, .T. ) ;
#73874 = CARTESIAN_POINT ( 'NONE',  ( 9.042925270190632858, 10.61279623905300085, 1.082531754730549967 ) ) ;
#73875 = EDGE_CURVE ( 'NONE', #45206, #106547, #106822, .T. ) ;
#73876 = AXIS2_PLACEMENT_3D ( 'NONE', #143360, #10108, #27429 ) ;
#73877 = VERTEX_POINT ( 'NONE', #171220 ) ;
#73878 = CARTESIAN_POINT ( 'NONE',  ( -0.03490996608559569087, -1.614503017106348581, 1.202435150695363664 ) ) ;
#73879 = CARTESIAN_POINT ( 'NONE',  ( 0.6446037793155032780, -1.481899804082789984, 0.8824728545121940382 ) ) ;
#73880 = CARTESIAN_POINT ( 'NONE',  ( 5.471888747823221877, -0.9023485654677811940, 1.803414228490702209 ) ) ;
#73882 = LINE ( 'NONE', #29405, #209411 ) ;
#73881 = CARTESIAN_POINT ( 'NONE',  ( -8.143643823302737061, 12.65266822716189843, 0.000000000000000000 ) ) ;
#73883 = CARTESIAN_POINT ( 'NONE',  ( 1.642778471875001811, -0.7802083328553761632, 2.845375778867859751 ) ) ;
#73885 = CARTESIAN_POINT ( 'NONE',  ( 1.269958040854075154, -1.126728106645444205, 1.364847948389063870 ) ) ;
#73884 = CARTESIAN_POINT ( 'NONE',  ( 2.853556533831374420, 2.080516846217596250, -0.2054353837145187767 ) ) ;
#73886 = CARTESIAN_POINT ( 'NONE',  ( 6.522112240665402183, -1.799906897009293738, 0.9091900463213120620 ) ) ;
#73888 = CARTESIAN_POINT ( 'NONE',  ( 4.488395308864603805, -0.4996631572763092222, -2.236994043316854697 ) ) ;
#73887 = CARTESIAN_POINT ( 'NONE',  ( 4.085803189671889157, 5.860132702740892263, -1.599625672291273171 ) ) ;
#73889 = CARTESIAN_POINT ( 'NONE',  ( 2.624636096055412704, -1.623921194558699765, 0.6262662122848341451 ) ) ;
#73890 = CARTESIAN_POINT ( 'NONE',  ( 5.379888026524302980, 5.170957540566797128, -0.7998128361456211532 ) ) ;
#73891 = CARTESIAN_POINT ( 'NONE',  ( -2.678032581596935024, -0.4534618882029449183, -0.1088563323523765447 ) ) ;
#73892 = CARTESIAN_POINT ( 'NONE',  ( 2.178627760304178818, -0.8125915806111455586, -1.531602080710131153 ) ) ;
#73893 = CARTESIAN_POINT ( 'NONE',  ( -0.6801582343750386395, 2.380208333674735499, -1.178068619123869398 ) ) ;
#73894 = CARTESIAN_POINT ( 'NONE',  ( 1.592022279046673816, 0.9211323807055901147, -1.617040898905151458 ) ) ;
#73895 =( BOUNDED_CURVE ( )  B_SPLINE_CURVE ( 2, ( #65340, #31817, #163953, #16592, #212666, #48085, #47009 ),
 .UNSPECIFIED., .F., .T. ) 
 B_SPLINE_CURVE_WITH_KNOTS ( ( 3, 2, 2, 3 ),
 ( 0.1612917726641805993, 0.1666666666666666574, 0.1805555555555555525, 0.1875000000000000000 ),
 .UNSPECIFIED. ) 
 CURVE ( )  GEOMETRIC_REPRESENTATION_ITEM ( )  RATIONAL_B_SPLINE_CURVE ( ( 0.9364346073024809591, 0.9481528537347150287, 1.000000000000000000, 0.8660254037844387076, 1.000000000000000000, 0.9330127018922194093, 0.9330127018922194093 ) ) 
 REPRESENTATION_ITEM ( '' )  );
#73896 = CARTESIAN_POINT ( 'NONE',  ( 2.717415358725610908, -1.887964963866497259, -1.072103292869843960 ) ) ;
#73897 = CARTESIAN_POINT ( 'NONE',  ( 4.462605117192430804, 8.358123070033169455, 1.040834085586084257E-14 ) ) ;
#73898 = CARTESIAN_POINT ( 'NONE',  ( 3.555875268649951959, 1.124244472066991518, 1.673854899288424347 ) ) ;
#73899 = CARTESIAN_POINT ( 'NONE',  ( 2.093750000000001332, -1.895863743164132531, -0.7852924748298759638 ) ) ;
#73900 = CARTESIAN_POINT ( 'NONE',  ( -1.500000000000013101, 2.910416667349485120, -0.8660254037844313801 ) ) ;
#73901 = CARTESIAN_POINT ( 'NONE',  ( 1.377817859240665577, 1.145177193861897758, 1.548917676831958801 ) ) ;
#73902 = CARTESIAN_POINT ( 'NONE',  ( -0.6823417656250039265, 14.31770833367473195, -1.181850606188755259 ) ) ;
#73903 = CARTESIAN_POINT ( 'NONE',  ( 4.904621534589208132, -2.204716393758818782, -0.2710871420372409912 ) ) ;
#73904 = VERTEX_POINT ( 'NONE', #75855 ) ;
#73905 =( LENGTH_UNIT ( ) NAMED_UNIT ( * ) SI_UNIT ( .MILLI., .METRE. ) );
#73906 = CARTESIAN_POINT ( 'NONE',  ( -1.500000000000001332, 0.4000000000000253353, 0.000000000000000000 ) ) ;
#73907 = CARTESIAN_POINT ( 'NONE',  ( 8.599949509769960088, 8.927695937686774386, 1.040834085586084257E-14 ) ) ;
#73908 = CARTESIAN_POINT ( 'NONE',  ( -0.6823417656250003738, -0.2822916663252489355, -1.181850606188749264 ) ) ;
#73909 = CARTESIAN_POINT ( 'NONE',  ( 6.205373625529961856, 1.933303589146176948, -1.094015395867214080 ) ) ;
#73910 = CARTESIAN_POINT ( 'NONE',  ( 5.142999638377217408, -0.2383176028181442918, -1.947251298587366231 ) ) ;
#73911 = CARTESIAN_POINT ( 'NONE',  ( 8.920901888111989919, 11.43080484092926241, 1.443375672974076540 ) ) ;
#73912 = SURFACE_SIDE_STYLE ('',( #157307 ) ) ;
#73913 = CARTESIAN_POINT ( 'NONE',  ( 5.202513629402051976, -0.7552652112401860851, -2.132769717564055867 ) ) ;
#73914 = CARTESIAN_POINT ( 'NONE',  ( -6.617788377246204945, 6.893376992974917350, -0.7216878364870338292 ) ) ;
#73915 = CARTESIAN_POINT ( 'NONE',  ( 2.840340301219072217, -1.062657783794159538, 1.767763702702547679 ) ) ;
#73916 = CARTESIAN_POINT ( 'NONE',  ( -4.530395885260773525, 8.437212299446219532, 0.7998128361456481317 ) ) ;
#73917 = CARTESIAN_POINT ( 'NONE',  ( 0.7499999999999885647, 3.097916667349487341, -1.299038105676658228 ) ) ;
#73918 = CARTESIAN_POINT ( 'NONE',  ( -1.364683531250010295, 5.301041667008085767, -0.7879004041258300672 ) ) ;
#73919 = CARTESIAN_POINT ( 'NONE',  ( 5.219927230130699591, -0.9996001844756461363, -1.580852690948472361 ) ) ;
#73920 = CARTESIAN_POINT ( 'NONE',  ( 3.797271647414564910, 1.222981480435406443, -1.229749918556479304 ) ) ;
#73921 = CARTESIAN_POINT ( 'NONE',  ( 1.768729326414076430, 1.665373798791164317, -0.5055230280728554293 ) ) ;
#73922 = CARTESIAN_POINT ( 'NONE',  ( 0.2579210422260198587, 2.266244506498811706, -0.3445303224042794432 ) ) ;
#73923 = CARTESIAN_POINT ( 'NONE',  ( 0.7103623821160671703, -2.195938746145317477, 0.2182302698266261887 ) ) ;
#73924 = CARTESIAN_POINT ( 'NONE',  ( 4.335544241866786663, 0.8922555979511301860, -1.890918108395107211 ) ) ;
#73925 = CARTESIAN_POINT ( 'NONE',  ( 5.367111071781861753, 1.871067490511884479, -0.5196462679451731015 ) ) ;
#73926 = CARTESIAN_POINT ( 'NONE',  ( 8.032759536594785033, 15.33864185422659787, 8.916444764510272236 ) ) ;
#73927 =( NAMED_UNIT ( * ) PLANE_ANGLE_UNIT ( ) SI_UNIT ( $, .RADIAN. ) );
#73928 = CARTESIAN_POINT ( 'NONE',  ( 1.020157974382044364, -1.821741137083273010, 0.8647263380179845971 ) ) ;
#73929 = CARTESIAN_POINT ( 'NONE',  ( 0.05319811239242258627, 0.3688592364489845510, 2.088132107045739705 ) ) ;
#73930 = CARTESIAN_POINT ( 'NONE',  ( 6.486953984781112403, -2.015912550161761629, 0.05229459904129707404 ) ) ;
#73931 = CARTESIAN_POINT ( 'NONE',  ( -7.883176251342026042, 11.28445716228600126, -1.199719254218446718 ) ) ;
#73932 = CARTESIAN_POINT ( 'NONE',  ( 7.416473721875251890, 8.611306416064660851, 1.199719254218462483 ) ) ;
#73933 = CARTESIAN_POINT ( 'NONE',  ( 4.670415550810885996, -1.190324863180821646, 1.384379922071424351 ) ) ;
#73934 = CARTESIAN_POINT ( 'NONE',  ( 2.415298318263587873, 1.970979330149217335, 0.9926799514654092160 ) ) ;
#73935 = ORIENTED_EDGE ( 'NONE', *, *, #55279, .T. ) ;
#73936 = CARTESIAN_POINT ( 'NONE',  ( -4.841670253411603397, 5.781608396135871075, 1.082531754730549078 ) ) ;
#73937 = CARTESIAN_POINT ( 'NONE',  ( -4.462568837553487100, 5.235360394347691404, -1.199719254218453823 ) ) ;
#73938 = CARTESIAN_POINT ( 'NONE',  ( 1.001543065824772753E-15, -2.209374999522042859, 3.793834371823811669 ) ) ;
#73939 = CARTESIAN_POINT ( 'NONE',  ( -7.182068686937172153, 9.402166106225269715, 1.599625672291283607 ) ) ;
#73940 = CARTESIAN_POINT ( 'NONE',  ( 1.705338084499245843, 1.755316507598453368, -0.9991084507309263563 ) ) ;
#73941 = CARTESIAN_POINT ( 'NONE',  ( -3.447516199624892419, 7.244129009529488350, 0.7998128361456352531 ) ) ;
#73942 = CARTESIAN_POINT ( 'NONE',  ( 2.922522432510234136, -1.287038294151692241, 1.344341647096161996 ) ) ;
#73943 = CARTESIAN_POINT ( 'NONE',  ( 10.70146331988817323, 11.37946204949139251, 0.7998128361456341429 ) ) ;
#73944 = FACE_BOUND ( 'NONE', #143904, .T. ) ;
#73945 = ORIENTED_EDGE ( 'NONE', *, *, #21894, .T. ) ;
#73946 = EDGE_LOOP ( 'NONE', ( #171368, #35429, #74598, #68183, #190428, #28532, #8683, #167358, #47043, #155252, #201633, #45304, #33828, #161536, #114412, #77248, #183812, #123965, #46124, #165994, #8825, #112796, #31900, #35490, #193661, #25614, #53473, #204837 ) ) ;
#73947 = CARTESIAN_POINT ( 'NONE',  ( -5.037017762676898158, 5.835274463666530131, -1.199719254218446718 ) ) ;
#73948 = AXIS2_PLACEMENT_3D ( 'NONE', #88151, #158490, #156362 ) ;
#73949 = CARTESIAN_POINT ( 'NONE',  ( -9.481229494658258261, 9.955855920056455588, -0.7998128361456291469 ) ) ;
#73951 = EDGE_CURVE ( 'NONE', #30509, #143616, #66096, .T. ) ;
#73950 = CARTESIAN_POINT ( 'NONE',  ( 5.127504350819418910, -1.732488751877172772, 0.5760870007271366999 ) ) ;
#73953 = CARTESIAN_POINT ( 'NONE',  ( -3.983506901647102083, 7.838413813543339437, 0.2012387096505599549 ) ) ;
#73952 = CARTESIAN_POINT ( 'NONE',  ( -5.915100157312088491, 10.12297696016459092, -0.7998128361456362523 ) ) ;
#73954 = CARTESIAN_POINT ( 'NONE',  ( 6.454497976780569246, 6.866128686250288382, -0.6735470152485992790 ) ) ;
#73955 = CARTESIAN_POINT ( 'NONE',  ( 0.6492036743409674848, -0.2036512653956819019, -1.721755200737408842 ) ) ;
#73956 = CARTESIAN_POINT ( 'NONE',  ( 0.4623611518889169103, 0.1752324854824957590, -1.731468860160074952 ) ) ;
#73957 = CARTESIAN_POINT ( 'NONE',  ( 4.758593218111947465, 0.8799714688421821362, 2.133523255312119726 ) ) ;
#73958 = CARTESIAN_POINT ( 'NONE',  ( 5.204350862799327793, 7.165104988056252289, -1.599625672291281386 ) ) ;
#73959 = CARTESIAN_POINT ( 'NONE',  ( 6.907524304660562109, -0.4813806915026208055, 2.115094849305596103 ) ) ;
#73960 = CARTESIAN_POINT ( 'NONE',  ( 6.144869935491714230, 8.192100896205568361, -1.599625672291262513 ) ) ;
#73961 = CARTESIAN_POINT ( 'NONE',  ( 5.659591354751080772, -0.5502123075824224552, -2.231479479524396403 ) ) ;
#73962 = CARTESIAN_POINT ( 'NONE',  ( 3.001048869802148023, 2.786623193720112024, 2.499999999999998668 ) ) ;
#73963 = CARTESIAN_POINT ( 'NONE',  ( -6.129167961829681488, 9.308390501180058507, -1.199719254218452047 ) ) ;
#73964 = CIRCLE ( 'NONE', #153593, 0.5000000000000006661 ) ;
#73965 = CARTESIAN_POINT ( 'NONE',  ( 5.453920962983416665, 1.868457504587007545, -0.09292587778651077712 ) ) ;
#73967 = CARTESIAN_POINT ( 'NONE',  ( -4.604929450496978660, 5.401447776115099408, -1.199719254218453823 ) ) ;
#73966 = CARTESIAN_POINT ( 'NONE',  ( 3.058751851047710080, 0.4689117840017149041, 1.853869267190631831 ) ) ;
#73968 = CARTESIAN_POINT ( 'NONE',  ( 4.793709216081707858, 1.633822259641436903, 1.483752339651790653 ) ) ;
#73969 = CARTESIAN_POINT ( 'NONE',  ( 4.276635374070654194, -0.4674139498860945263, -2.064944810692950217 ) ) ;
#73970 = CARTESIAN_POINT ( 'NONE',  ( -0.6125000000000296874, 0.3541666673494772710, 1.060881119635899816 ) ) ;
#73971 = CARTESIAN_POINT ( 'NONE',  ( 6.983263157960365675, 7.629137130509070275, 2.446189081643288521 ) ) ;
#73972 = CARTESIAN_POINT ( 'NONE',  ( 6.658462837642799670, 6.940830530104329377, 0.7216878364870328300 ) ) ;
#73973 = CARTESIAN_POINT ( 'NONE',  ( -5.112833325684916552, 7.058334528089422300, -1.443375672974066548 ) ) ;
#73974 = CARTESIAN_POINT ( 'NONE',  ( 2.274872074667996458, -1.419342104801555982, 1.819364073307845997 ) ) ;
#73975 = CARTESIAN_POINT ( 'NONE',  ( 3.297265573180406584, -1.731424309613574852, 0.9225008839797432802 ) ) ;
#73976 = CARTESIAN_POINT ( 'NONE',  ( -3.772911886352873445, 7.623757310712139912, 0.7998128361456350310 ) ) ;
#73977 = EDGE_CURVE ( 'NONE', #69312, #37010, #202251, .T. ) ;
#73978 = CARTESIAN_POINT ( 'NONE',  ( 6.825054090417398633, -1.883341039872712397, -0.8414091007707087400 ) ) ;
#73979 = CARTESIAN_POINT ( 'NONE',  ( 2.548569689688999329, 5.917155704705049146, -0.7216878364870267237 ) ) ;
#73980 = CARTESIAN_POINT ( 'NONE',  ( 5.252858170651868441, 5.093032385374103299, -0.7998128361456481317 ) ) ;
#73981 = EDGE_LOOP ( 'NONE', ( #78916, #171636, #187609, #203768 ) ) ;
#73982 = CARTESIAN_POINT ( 'NONE',  ( 5.313685493615880162, -1.282986534165726944, -1.555701818360885280 ) ) ;
#73983 = CARTESIAN_POINT ( 'NONE',  ( -7.621654909176601045, 12.04368116068139472, 0.7998128361456481317 ) ) ;
#73984 = DIRECTION ( 'NONE',  ( 2.949029909160572061E-17, 1.000000000000000000, -8.673600428462353400E-15 ) ) ;
#73985 = CARTESIAN_POINT ( 'NONE',  ( -10.47476631618627252, 5.237304525980054137, 5.169966676860812349 ) ) ;
#73986 = CARTESIAN_POINT ( 'NONE',  ( 1.762787986429158016, -0.7786651900678620564, -2.026813006651595028 ) ) ;
#73987 = DIRECTION ( 'NONE',  ( 0.6507913734559641616, 0.7592566023653004592, 0.000000000000000000 ) ) ;
#73988 = CARTESIAN_POINT ( 'NONE',  ( -1.500000000000013101, 0.2020833340161521663, 0.8660254037844403729 ) ) ;
#73989 = VECTOR ( 'NONE', #78006, 1000.000000000000114 ) ;
#73990 = CARTESIAN_POINT ( 'NONE',  ( -1.790679264613934007, 14.55177512361720460, -11.85442263018568099 ) ) ;
#73991 = PRESENTATION_STYLE_ASSIGNMENT (( #106541 ) ) ;
#73992 = CARTESIAN_POINT ( 'NONE',  ( 5.371503168974233411, 7.687194297833679357, 1.321221623412481394 ) ) ;
#73993 = CARTESIAN_POINT ( 'NONE',  ( 1.036483977676525114, 2.029821650745375905, 0.3549538351500410305 ) ) ;
#73995 = CARTESIAN_POINT ( 'NONE',  ( 6.727182134110203826, 2.985950691969770254, 2.264927069331075238 ) ) ;
#73994 = CARTESIAN_POINT ( 'NONE',  ( 0.07775346131143417994, 7.629137130509094256, -2.888902737517151209 ) ) ;
#73996 = CARTESIAN_POINT ( 'NONE',  ( -1.402160292154681736E-14, 0.3218750003414227456, 1.575800808251672791 ) ) ;
#73997 = DIRECTION ( 'NONE',  ( 1.224646799147353207E-16, 1.000000000000000000, -0.000000000000000000 ) ) ;
#73998 = ORIENTED_EDGE ( 'NONE', *, *, #137674, .F. ) ;
#73999 = CARTESIAN_POINT ( 'NONE',  ( 3.510326737904199135, -1.910220267131033323, -0.09114558060911714943 ) ) ;
#74000 = CARTESIAN_POINT ( 'NONE',  ( 5.453870971094811004, 1.767685242813926250, -0.08968725887432274502 ) ) ;
#74001 = CARTESIAN_POINT ( 'NONE',  ( 5.417364897112183719, 8.477953592343014932, 1.199719254218451159 ) ) ;
#74002 = CARTESIAN_POINT ( 'NONE',  ( -3.928111819657352566, 5.605883094398769195, 1.599625672291267398 ) ) ;
#74004 = CARTESIAN_POINT ( 'NONE',  ( 0.2334084307264666924, 0.5983727300521198833, -1.819970363327483076 ) ) ;
#74003 = CARTESIAN_POINT ( 'NONE',  ( -6.775479680898221169, -7.217880409000307473, 6.775479680898245149 ) ) ;
#74005 = CARTESIAN_POINT ( 'NONE',  ( -1.500000000000015099, 0.3791666666666850261, -0.8660254037844383745 ) ) ;
#74006 = CARTESIAN_POINT ( 'NONE',  ( 1.205626512970816355, -1.630946839658468983, -1.275175305487465049 ) ) ;
#74007 = CARTESIAN_POINT ( 'NONE',  ( -1.364683531250000748, -0.6781249996585803075, 0.000000000000000000 ) ) ;
#74008 = ADVANCED_FACE ( 'NONE', ( #58541 ), #213657, .T. ) ;
#74009 = CARTESIAN_POINT ( 'NONE',  ( 5.682452175617663137, -1.825344843996518529, -0.4084625512627630406 ) ) ;
#74010 = CARTESIAN_POINT ( 'NONE',  ( 2.771877994228102882, 0.9767612972278701955, 1.542236413651025151 ) ) ;
#74012 = CARTESIAN_POINT ( 'NONE',  ( 6.476386945563378461, 6.757828299745357370, 0.2189195654383000456 ) ) ;
#74011 = CARTESIAN_POINT ( 'NONE',  ( 6.076841795016812320, -2.094286673724785164, -0.6961510500591641115 ) ) ;
#74013 = CARTESIAN_POINT ( 'NONE',  ( -1.402160292154681736E-14, -0.05312499965857903073, -1.575800808251665908 ) ) ;
#74014 = CARTESIAN_POINT ( 'NONE',  ( 3.033693852995589246, 1.959511903404848043, -0.6444255830786119743 ) ) ;
#74015 = ADVANCED_FACE ( 'NONE', ( #178702 ), #207991, .T. ) ;
#74017 = CARTESIAN_POINT ( 'NONE',  ( -7.527801604085656351, 9.805521176231838609, 1.599625672291295375 ) ) ;
#74016 = VECTOR ( 'NONE', #124866, 1000.000000000000000 ) ;
#74018 = CARTESIAN_POINT ( 'NONE',  ( 9.264299036839600987, 9.702770385934682551, -0.7998128361456281477 ) ) ;
#74019 = CARTESIAN_POINT ( 'NONE',  ( 3.520313441042647984, 7.258782781191745137, 0.7998128361456321445 ) ) ;
#74020 = CARTESIAN_POINT ( 'NONE',  ( 0.2456851981432126020, -1.670693100197045977, -1.371219901248825535 ) ) ;
#74021 = CARTESIAN_POINT ( 'NONE',  ( 5.617656447048144486, 0.4075009240860455462, -2.029694874052537568 ) ) ;
#74023 = CARTESIAN_POINT ( 'NONE',  ( 1.364683531249986537, 0.4677083336747514530, -0.7879004041258309554 ) ) ;
#74022 = CIRCLE ( 'NONE', #157213, 0.04999999999999969746 ) ;
#74024 = CARTESIAN_POINT ( 'NONE',  ( 3.849029623751087481, -1.769594347601778361, 1.241129261558816754 ) ) ;
#74025 = CARTESIAN_POINT ( 'NONE',  ( -4.620365152176808543, 8.363145938788004941, -0.2588828456067792660 ) ) ;
#74027 = CARTESIAN_POINT ( 'NONE',  ( 1.873419974815058842, -0.2433403713097622156, 1.946663811685337420 ) ) ;
#74026 = CARTESIAN_POINT ( 'NONE',  ( 4.652993067401423488, 0.3473450764862345830, 1.989417523455960568 ) ) ;
#74028 = CARTESIAN_POINT ( 'NONE',  ( 3.929058411375439874, 4.999999999999997335, 0.7500000000000006661 ) ) ;
#74029 = EDGE_CURVE ( 'NONE', #19630, #97098, #44632, .T. ) ;
#74032 = CARTESIAN_POINT ( 'NONE',  ( 6.480434237652132445, 7.623223367758051872, 1.082531754730558626 ) ) ;
#74031 = CARTESIAN_POINT ( 'NONE',  ( -3.474999999999998312, -0.3208333333333319715, 2.006292185433951047 ) ) ;
#74030 = CARTESIAN_POINT ( 'NONE',  ( -1.225000000000058265, 1.520833333333367232, 0.7072540797572596238 ) ) ;
#74033 = CARTESIAN_POINT ( 'NONE',  ( -7.605197822622922210, 7.837428646007010613, -0.7998128361456362523 ) ) ;
#74034 = CARTESIAN_POINT ( 'NONE',  ( 1.973842561262352469, -0.8578407463649927456, 1.825077436249371354 ) ) ;
#74036 = CARTESIAN_POINT ( 'NONE',  ( 1.992392395334954491, 0.1979219324388767909, 0.6149939648490070354 ) ) ;
#74035 = CARTESIAN_POINT ( 'NONE',  ( -3.730464822054482710, 7.503959392372201442, 1.040834085586084257E-14 ) ) ;
#74037 = CARTESIAN_POINT ( 'NONE',  ( 1.499999999999999778, 7.809273069926267574, 3.635729725621137387 ) ) ;
#74038 = CARTESIAN_POINT ( 'NONE',  ( 5.853752780977106163, -1.389761788226477002, -1.313969904969368496 ) ) ;
#74039 = B_SPLINE_CURVE_WITH_KNOTS ( 'NONE', 3,
 ( #141272, #91432, #110925, #205131, #42688, #90348, #209397, #172670, #139104, #40539, #26397, #27468 ),
 .UNSPECIFIED., .F., .F.,
 ( 4, 2, 2, 2, 2, 4 ),
 ( 0.003750395023273722043, 0.003985267534258110644, 0.004220140045242499680, 0.004689885067211279485, 0.005159630089180061892, 0.005629375111148844299 ),
 .UNSPECIFIED. ) ;
#74040 = CARTESIAN_POINT ( 'NONE',  ( -3.195971524519394702, 4.751719416737803847, -1.599625672291262513 ) ) ;
#74041 = CARTESIAN_POINT ( 'NONE',  ( 3.999292125906894313, 7.609665213625947722, 0.7216878364870317197 ) ) ;
#74043 = CARTESIAN_POINT ( 'NONE',  ( 3.163685574146878565, 1.281377625384312324, 1.556896677758594416 ) ) ;
#74042 = CARTESIAN_POINT ( 'NONE',  ( -8.798878505144658746, 10.32807501316600884, -1.082531754730543083 ) ) ;
#74044 = CARTESIAN_POINT ( 'NONE',  ( -1.500000000000011324, 3.670833333333356485, 0.8660254037844403729 ) ) ;
#74045 = CARTESIAN_POINT ( 'NONE',  ( 1.364683531249997417, 14.54687500034139447, 2.602085213965210642E-15 ) ) ;
#74046 = CARTESIAN_POINT ( 'NONE',  ( 5.930603204692192598, 1.663448300781378508, 0.4554771339976750322 ) ) ;
#74047 = CARTESIAN_POINT ( 'NONE',  ( 7.713663051532233972, 7.963971413067895355, -0.7998128361456341429 ) ) ;
#74048 = CARTESIAN_POINT ( 'NONE',  ( 9.137832345930652522, 10.72352116074969075, -1.082531754730543083 ) ) ;
#74049 = DIRECTION ( 'NONE',  ( 0.000000000000000000, 1.561251128379122346E-12, 1.000000000000000000 ) ) ;
#74050 = CARTESIAN_POINT ( 'NONE',  ( 3.971829172498120286, 1.036919360001643531, 1.556626693588740062 ) ) ;
#74051 = FACE_OUTER_BOUND ( 'NONE', #90140, .T. ) ;
#74052 = CARTESIAN_POINT ( 'NONE',  ( 2.729418486472269922, 0.1060373921930452268, -2.067687848736274869 ) ) ;
#74053 = VERTEX_POINT ( 'NONE', #135833 ) ;
#74054 = CARTESIAN_POINT ( 'NONE',  ( 3.366167277942881064, 7.149221934233827014, -0.7998128361456362523 ) ) ;
#74055 = CARTESIAN_POINT ( 'NONE',  ( -0.0003749349099593791675, -1.976945657698804704, 0.3961262320883383592 ) ) ;
#74056 = CARTESIAN_POINT ( 'NONE',  ( 0.5799530485631685384, 0.8934014309100688500, 1.575905833579164694 ) ) ;
#74057 = CARTESIAN_POINT ( 'NONE',  ( 3.553645660113312399, 7.160020680191912845, -1.734723475976807094E-15 ) ) ;
#74058 = DIRECTION ( 'NONE',  ( 0.000000000000000000, 1.000000000000000000, 0.000000000000000000 ) ) ;
#74059 = ORIENTED_EDGE ( 'NONE', *, *, #164392, .T. ) ;
#74060 = CARTESIAN_POINT ( 'NONE',  ( 7.090551149822728938, 10.25576486055978442, 1.082531754730558626 ) ) ;
#74061 = CARTESIAN_POINT ( 'NONE',  ( 7.344766530301147789, 9.591980256816594164, 1.599625672291281386 ) ) ;
#74062 = CARTESIAN_POINT ( 'NONE',  ( 6.169544653506280341, 1.324940883694783578, 1.383738526680919012 ) ) ;
#74063 = CARTESIAN_POINT ( 'NONE',  ( 5.192409644353875642, 5.160158794608717514, 1.040834085586084257E-14 ) ) ;
#74064 = DIRECTION ( 'NONE',  ( 0.000000000000000000, 1.000000000000000000, 0.000000000000000000 ) ) ;
#74065 = COLOUR_RGB ( '', 0.40784314, 0.44705882, 0.49803922) ;
#74066 = DIRECTION ( 'NONE',  ( 0.000000000000000000, 1.000000000000000000, -8.546850786086437571E-32 ) ) ;
#74068 = ORIENTED_EDGE ( 'NONE', *, *, #145048, .F. ) ;
#74067 = CARTESIAN_POINT ( 'NONE',  ( 5.192409644353875642, 5.160158794608717514, 1.040834085586084257E-14 ) ) ;
#74069 = CARTESIAN_POINT ( 'NONE',  ( -9.015808963407680565, 9.620791333504852716, 1.040834085586084257E-14 ) ) ;
#74070 = CARTESIAN_POINT ( 'NONE',  ( 3.467792127863758456, 2.109446376165153847, -0.4717452660116944196 ) ) ;
#74071 = CARTESIAN_POINT ( 'NONE',  ( -6.102578539926875933, 10.13377570664109051, 0.7216878364870267237 ) ) ;
#74072 = CARTESIAN_POINT ( 'NONE',  ( 4.415115299905642665, 5.179997933758551554, -1.199719254218450271 ) ) ;
#74073 = DIRECTION ( 'NONE',  ( -0.04520447523801534445, 0.000000000000000000, 0.9989777552170296948 ) ) ;
#74074 = CARTESIAN_POINT ( 'NONE',  ( 5.368107995252269227, 0.9013511576922846880, 1.587453057759043551 ) ) ;
#74075 = ADVANCED_FACE ( 'NONE', ( #40474 ), #4715, .F. ) ;
#74077 = CARTESIAN_POINT ( 'NONE',  ( 8.729527388974888780, 11.83892083880631851, -8.258113299037200150 ) ) ;
#74076 =( BOUNDED_CURVE ( )  B_SPLINE_CURVE ( 2, ( #120333, #154900, #73639, #169003, #137592, #172220, #70406, #136525, #88843 ),
 .UNSPECIFIED., .F., .T. ) 
 B_SPLINE_CURVE_WITH_KNOTS ( ( 3, 2, 2, 2, 3 ),
 ( 0.8839285714285713969, 0.8869047619047618625, 0.8928571428571429047, 0.8988095238095238360, 0.9017857142857143016 ),
 .UNSPECIFIED. ) 
 CURVE ( )  GEOMETRIC_REPRESENTATION_ITEM ( )  RATIONAL_B_SPLINE_CURVE ( ( 0.9330127018922194093, 0.9330127018922194093, 1.000000000000000000, 0.8660254037844387076, 1.000000000000000000, 0.8660254037844387076, 1.000000000000000000, 0.9330127018922194093, 0.9330127018922194093 ) ) 
 REPRESENTATION_ITEM ( '' )  );
#74078 = CARTESIAN_POINT ( 'NONE',  ( 1.528526583484477230, 1.898816187374774200, 0.5295601200957336108 ) ) ;
#74079 = CARTESIAN_POINT ( 'NONE',  ( 3.832203377193269755, -0.9874410831685247469, -1.637625244210038300 ) ) ;
#74080 = EDGE_LOOP ( 'NONE', ( #157055, #146646, #99860, #143259, #118202 ) ) ;
#74081 =( REPRESENTATION_RELATIONSHIP ('NONE','NONE', #84563, #121983 ) REPRESENTATION_RELATIONSHIP_WITH_TRANSFORMATION ( #89381 )SHAPE_REPRESENTATION_RELATIONSHIP( ) );
#74082 = CARTESIAN_POINT ( 'NONE',  ( -11.41381676900480713, 10.06958039977600627, -3.704697931490059215 ) ) ;
#74083 = CARTESIAN_POINT ( 'NONE',  ( 5.107841235723004303, 0.6198312778436664283, -1.869525964861347589 ) ) ;
#74084 = ORIENTED_EDGE ( 'NONE', *, *, #139225, .T. ) ;
#74085 = CARTESIAN_POINT ( 'NONE',  ( 0.3044966626061855752, 1.689057509992748729, 0.9581197715371556622 ) ) ;
#74086 = ORIENTED_EDGE ( 'NONE', *, *, #27372, .T. ) ;
#74087 = CARTESIAN_POINT ( 'NONE',  ( -5.798046968499580345, 6.793418213784815585, 1.199719254218452935 ) ) ;
#74089 = CARTESIAN_POINT ( 'NONE',  ( 6.011998765391792787, -0.7129019540204998284, 1.997330473063135381 ) ) ;
#74088 = CARTESIAN_POINT ( 'NONE',  ( -5.367048706163331850, 7.354919138647580290, -1.599625672291271394 ) ) ;
#74090 = CARTESIAN_POINT ( 'NONE',  ( 5.844973620822835336, 7.912498205750389424, 1.443375672974064550 ) ) ;
#74092 = ORIENTED_EDGE ( 'NONE', *, *, #204228, .T. ) ;
#74091 = CARTESIAN_POINT ( 'NONE',  ( 3.703681524037071071, 1.387051605615218008, 1.316649548728260344 ) ) ;
#74093 = CARTESIAN_POINT ( 'NONE',  ( 1.395868886378356821, 1.671639904693554168, 1.440724375100350008 ) ) ;
#74094 = CARTESIAN_POINT ( 'NONE',  ( 9.681420877353952292, 3.865149423709351328, -7.090140323037471326 ) ) ;
#74095 = CARTESIAN_POINT ( 'NONE',  ( 6.199863759850236633, 1.389832719217662049, 1.456544111691231658 ) ) ;
#74096 = DIRECTION ( 'NONE',  ( 0.000000000000000000, 0.7999999999999973799, -0.6000000000000034195 ) ) ;
#74097 = CARTESIAN_POINT ( 'NONE',  ( -1.408750476333751944, 7.229967155397921452, -4.273289540530492481 ) ) ;
#74098 = CARTESIAN_POINT ( 'NONE',  ( -0.05958166578300463923, 7.052156984183643118, -3.952571211854608801 ) ) ;
#74099 = CARTESIAN_POINT ( 'NONE',  ( 1.785682506433339478, -1.950172559450613852, 0.6955597780969878796 ) ) ;
#74100 = CARTESIAN_POINT ( 'NONE',  ( -4.713430959045263435, 8.650753218861462202, 0.7998128361456481317 ) ) ;
#74101 = CARTESIAN_POINT ( 'NONE',  ( -4.929275754869433257, 8.007250896656138650, 0.9949873637682864480 ) ) ;
#74102 = CARTESIAN_POINT ( 'NONE',  ( -4.495112795249930571, 8.049017979306610115, -2.444655174081867166 ) ) ;
#74103 = CARTESIAN_POINT ( 'NONE',  ( 4.476163270806094552, 8.373940915915776273, 0.7998128361456462443 ) ) ;
#74104 = FILL_AREA_STYLE_COLOUR ( '', #121171 ) ;
#74105 = CARTESIAN_POINT ( 'NONE',  ( 4.502716413514295191, 6.346531463890372926, -1.443375672974068769 ) ) ;
#74106 = CARTESIAN_POINT ( 'NONE',  ( 0.1588444833727359340, -6.630981389236866086, 9.484513307599966581 ) ) ;
#74107 = CARTESIAN_POINT ( 'NONE',  ( 0.000000000000000000, 0.5000000000000004441, 0.000000000000000000 ) ) ;
#74108 = CARTESIAN_POINT ( 'NONE',  ( -1.364683531250014514, 11.90104166700806587, -0.7879004041258335089 ) ) ;
#74110 = CARTESIAN_POINT ( 'NONE',  ( -6.631873415740034083, 7.766215735565355160, 1.199719254218452047 ) ) ;
#74109 = CARTESIAN_POINT ( 'NONE',  ( 6.925078400183545035, 0.003529629153843985134, 1.755452343125718073 ) ) ;
#74111 = CARTESIAN_POINT ( 'NONE',  ( 4.746542152430166972, 1.714266118827989516, -0.2609391866443058206 ) ) ;
#74112 = CARTESIAN_POINT ( 'NONE',  ( -4.277761160311629673, 4.949475094240346706, 1.199719254218462483 ) ) ;
#74113 = CARTESIAN_POINT ( 'NONE',  ( 2.536061329345109971, 1.270221119870031057, 1.634730569901183150 ) ) ;
#74114 = CARTESIAN_POINT ( 'NONE',  ( 3.866910228754817158, -0.2097145705111657654, -2.106837283413672601 ) ) ;
#74115 = CARTESIAN_POINT ( 'NONE',  ( 7.623762449586013901, 7.788811034138823253, 1.040834085586084257E-14 ) ) ;
#74116 = CARTESIAN_POINT ( 'NONE',  ( 1.364683531249988535, 3.363541667008085323, 0.7879004041258499402 ) ) ;
#74117 = CARTESIAN_POINT ( 'NONE',  ( 1.287880319801449902, -1.245359047439015932, -1.525745898539744516 ) ) ;
#74118 = CARTESIAN_POINT ( 'NONE',  ( 5.931217288863120274, 6.131947776268360961, 0.7575795127007216578 ) ) ;
#74120 = CARTESIAN_POINT ( 'NONE',  ( 0.07037084582631887575, 0.7337836260858082715, 1.766209603411242668 ) ) ;
#74119 = CARTESIAN_POINT ( 'NONE',  ( 1.001543065824772753E-15, -1.312499999999998224, 4.012584370867899430 ) ) ;
#74121 = CARTESIAN_POINT ( 'NONE',  ( 3.416269409239420352, 1.454353297360365449, -1.771818544839237175 ) ) ;
#74123 = EDGE_CURVE ( 'NONE', #170783, #153954, #8733, .T. ) ;
#74122 = CARTESIAN_POINT ( 'NONE',  ( 1.435882461153328515, 0.9014729512111450127, -1.587519582607027635 ) ) ;
#74124 = CARTESIAN_POINT ( 'NONE',  ( 4.746236293235721604, 7.694970221153795364, 1.199719254218451159 ) ) ;
#74125 = CARTESIAN_POINT ( 'NONE',  ( 6.033015167956792268, 8.061603667414825480, -1.443375672974057666 ) ) ;
#74126 = CARTESIAN_POINT ( 'NONE',  ( -8.681298431451969222, 9.022603012982438386, 1.040834085586084257E-14 ) ) ;
#74127 = CARTESIAN_POINT ( 'NONE',  ( 2.443610342004947533, -1.876944004186463566, 0.7284700530331960078 ) ) ;
#74128 = CARTESIAN_POINT ( 'NONE',  ( 2.834756127989654484, -1.875839772035441388, -0.5741054328185363209 ) ) ;
#74129 = CARTESIAN_POINT ( 'NONE',  ( -6.984421689334302741, 11.30024240419870374, 0.000000000000000000 ) ) ;
#74130 = CARTESIAN_POINT ( 'NONE',  ( -6.388916700537716764, 8.476822122092563916, 1.599625672291283607 ) ) ;
#74132 = EDGE_CURVE ( 'NONE', #163067, #73414, #184575, .T. ) ;
#74131 = CARTESIAN_POINT ( 'NONE',  ( 7.777967379493318845, -9.999999999999994671, 7.664830294503448549 ) ) ;
#74135 = B_SPLINE_CURVE_WITH_KNOTS ( 'NONE', 3,
 ( #22284, #89476, #117757, #101432, #135025, #155531, #55887, #23367, #186943, #2837 ),
 .UNSPECIFIED., .F., .F.,
 ( 4, 3, 3, 4 ),
 ( 9.585285410731671485E-17, 4.411882185274044424E-05, 8.611515704366408169E-05, 0.0001647628875604093836 ),
 .UNSPECIFIED. ) ;
#74134 = CARTESIAN_POINT ( 'NONE',  ( 4.047515533282939337, 0.5961193180711570339, -1.666553171763493602 ) ) ;
#74133 = CARTESIAN_POINT ( 'NONE',  ( 6.667919252303131650, -1.287369299672879830, 1.647753151290908047 ) ) ;
#74136 = CARTESIAN_POINT ( 'NONE',  ( -4.864214080903581205, 4.879786425613829692, -0.6392378712632117432 ) ) ;
#74137 = CARTESIAN_POINT ( 'NONE',  ( 0.9201892814816803323, 1.302667801055312990, -1.762099327409505811 ) ) ;
#74138 = CARTESIAN_POINT ( 'NONE',  ( 5.841712918432809154, 1.738692355929325029, 0.07866246996769517275 ) ) ;
#74139 = CARTESIAN_POINT ( 'NONE',  ( 9.074484886248265880, 9.481320543578137361, 0.7998128361456462443 ) ) ;
#74140 = CARTESIAN_POINT ( 'NONE',  ( 0.2331713839410394229, 1.378908429916062994, -2.211717543205340863 ) ) ;
#74141 = CARTESIAN_POINT ( 'NONE',  ( 0.2108991129620274019, -1.778944881630979413, -1.454728436597878316 ) ) ;
#74142 = DIRECTION ( 'NONE',  ( -0.000000000000000000, 1.000000000000000000, 9.023263958591317418E-17 ) ) ;
#74143 = CARTESIAN_POINT ( 'NONE',  ( 5.782511917101329502, -1.690859530023439250, 0.3827970650602616765 ) ) ;
#74144 = CARTESIAN_POINT ( 'NONE',  ( 5.828641854062238892, -1.381805371539744698, 1.674691576451936781 ) ) ;
#74145 = DIRECTION ( 'NONE',  ( 0.000000000000000000, -1.000000000000000000, 0.000000000000000000 ) ) ;
#74146 = CARTESIAN_POINT ( 'NONE',  ( 0.4095560439901060334, -2.008447366592306604, 0.6704124886842844910 ) ) ;
#74147 = CARTESIAN_POINT ( 'NONE',  ( 2.531250000000001332, -0.7852924748301189917, -1.895863743164030613 ) ) ;
#74148 = CARTESIAN_POINT ( 'NONE',  ( 6.827182134110199030, 6.034458849223407029, 2.683941674059683979 ) ) ;
#74149 = CARTESIAN_POINT ( 'NONE',  ( 4.506809989931632288, 1.489605450875215453, -1.221516061710873347 ) ) ;
#74150 = CARTESIAN_POINT ( 'NONE',  ( -1.500000000000015099, 11.26041666734946567, -0.8660254037844309360 ) ) ;
#74151 = CARTESIAN_POINT ( 'NONE',  ( 1.682608811002960447, 1.145563986048125704, 1.903002289297763605 ) ) ;
#74152 = ORIENTED_EDGE ( 'NONE', *, *, #62840, .F. ) ;
#74153 = CARTESIAN_POINT ( 'NONE',  ( -0.7500000000000215383, 4.441666666666691299, 1.299038105676671107 ) ) ;
#74154 = CARTESIAN_POINT ( 'NONE',  ( 4.497554271431305040, 6.270232621468402989, -1.599625672291256295 ) ) ;
#74155 = CARTESIAN_POINT ( 'NONE',  ( 7.142447996300871793, 7.227277505306155092, 0.7998128361456341429 ) ) ;
#74156 = CARTESIAN_POINT ( 'NONE',  ( 3.914843843660667400, -0.6973054565188941956, -2.109062029434173535 ) ) ;
#74157 = CARTESIAN_POINT ( 'NONE',  ( -7.971831135155409420, 11.28392484344787405, 1.082531754730549967 ) ) ;
#74158 = DIRECTION ( 'NONE',  ( -1.000000000000000000, -3.451266460341926649E-31, -8.638326563840809144E-31 ) ) ;
#74159 = CARTESIAN_POINT ( 'NONE',  ( 5.816084710582486217, 9.729256562414162701, 1.040834085586084257E-14 ) ) ;
#74160 = CARTESIAN_POINT ( 'NONE',  ( -9.476786185827959841, 10.15859809299519334, 0.7216878364870438212 ) ) ;
#74161 = CIRCLE ( 'NONE', #56836, 0.07999999999999994615 ) ;
#74162 = ADVANCED_FACE ( 'NONE', ( #39390 ), #166470, .T. ) ;
#74163 = CARTESIAN_POINT ( 'NONE',  ( 7.187230829020130329, 7.557726520044554697, 0.7216878364870267237 ) ) ;
#74164 = CARTESIAN_POINT ( 'NONE',  ( 0.9146856577476671912, -1.281363086869342194, -1.556907195799726917 ) ) ;
#74166 = CARTESIAN_POINT ( 'NONE',  ( 6.654736832427365911, -0.5462217193984253427, -1.988994552010774797 ) ) ;
#74165 = CARTESIAN_POINT ( 'NONE',  ( 7.889955328148847258, 11.29236608522730911, -1.199719254218446718 ) ) ;
#74167 = DIRECTION ( 'NONE',  ( 1.000000000000000000, 0.000000000000000000, 0.000000000000000000 ) ) ;
#74168 = CARTESIAN_POINT ( 'NONE',  ( 7.038091138825468107, 8.344099429118761790, -1.082531754730548412 ) ) ;
#74169 = AXIS2_PLACEMENT_3D ( 'NONE', #48513, #15968, #65773 ) ;
#74170 = CARTESIAN_POINT ( 'NONE',  ( 6.163578228761874556, 0.9028020746227163329, 1.487850569839582970 ) ) ;
#74171 = FACE_OUTER_BOUND ( 'NONE', #206682, .T. ) ;
#74172 = CARTESIAN_POINT ( 'NONE',  ( -0.6823417656250212460, 1.801041667008083991, 1.181850606188755259 ) ) ;
#74173 = CARTESIAN_POINT ( 'NONE',  ( 1.704008468626088790, -0.6311095051503686770, -1.653581786927365904 ) ) ;
#74174 = CARTESIAN_POINT ( 'NONE',  ( 6.557244222609861062, -1.057944526735156821, 1.374202748628235327 ) ) ;
#74175 = CARTESIAN_POINT ( 'NONE',  ( 6.339394973347380002, 0.6569538336487945607, -1.611921592020611582 ) ) ;
#74176 = CARTESIAN_POINT ( 'NONE',  ( 4.406014021519581547, -0.9797006336973247409, -2.072624738501188446 ) ) ;
#74177 = CARTESIAN_POINT ( 'NONE',  ( 1.364683531249988757, -0.1156249996585798079, 0.000000000000000000 ) ) ;
#74178 = CARTESIAN_POINT ( 'NONE',  ( 2.536835285771392279, -1.364265644482412609, -1.236541980112846550 ) ) ;
#74179 = CARTESIAN_POINT ( 'NONE',  ( 7.886038904643079661, 12.35212915539230139, -0.7998128361456352531 ) ) ;
#74180 = CARTESIAN_POINT ( 'NONE',  ( 8.983524160790528512, 13.98338966858836940, -7.957451094343901410 ) ) ;
#74181 = CARTESIAN_POINT ( 'NONE',  ( 3.153144192703428939, -1.491587519860730238, -1.052284964708279258 ) ) ;
#74182 = CARTESIAN_POINT ( 'NONE',  ( 4.008435526009396455, -1.928752077057366732, 0.5880193435906443389 ) ) ;
#74183 = CARTESIAN_POINT ( 'NONE',  ( -9.992522908471816123, 11.61669713376064372, 1.199719254218462483 ) ) ;
#74185 = CARTESIAN_POINT ( 'NONE',  ( 0.000000000000000000, 7.849261790823902629, 0.000000000000000000 ) ) ;
#74184 = CARTESIAN_POINT ( 'NONE',  ( 3.169090989670137581, -2.089828869452925009, -0.8673982956902188679 ) ) ;
#74186 = CARTESIAN_POINT ( 'NONE',  ( 5.280345248378272238, -1.172444710293341963, 1.749198092158671614 ) ) ;
#74187 = CARTESIAN_POINT ( 'NONE',  ( 9.060091309786827196, 14.48005966906119646, 7.135690472246977833 ) ) ;
#74188 = AXIS2_PLACEMENT_3D ( 'NONE', #109704, #196219, #63006 ) ;
#74189 = CARTESIAN_POINT ( 'NONE',  ( 2.787621587699981696, -1.932700977737045633, 0.7428295258242522126 ) ) ;
#74190 = CARTESIAN_POINT ( 'NONE',  ( 4.436542580169809291, 6.199052314996659874, 1.599625672291267398 ) ) ;
#74191 = CARTESIAN_POINT ( 'NONE',  ( -1.360316468750016439, -0.07812499965861169349, -3.469446951953614189E-14 ) ) ;
#74192 = CARTESIAN_POINT ( 'NONE',  ( 5.549516566986255839, -1.916978305411633166, 0.9067721062034905799 ) ) ;
#74194 = CARTESIAN_POINT ( 'NONE',  ( 1.436025505276457226, 0.9502256629446425018, -1.675776081635256043 ) ) ;
#74193 = CARTESIAN_POINT ( 'NONE',  ( -7.831806290188425557, 12.28885777186185990, -0.7998128361456281477 ) ) ;
#74195 = CARTESIAN_POINT ( 'NONE',  ( -4.842197138736131556, 5.678260079060780008, 1.199719254218452935 ) ) ;
#74196 = CARTESIAN_POINT ( 'NONE',  ( 8.748035429315576650, 11.22912730566677553, -1.599625672291255185 ) ) ;
#74197 = CARTESIAN_POINT ( 'NONE',  ( 4.543390873910894356, 8.314723429622471684, 0.7216878364870317197 ) ) ;
#74198 = CARTESIAN_POINT ( 'NONE',  ( 4.113906668039927439, 7.442175195026684342, 0.6721147198667943856 ) ) ;
#74199 = CARTESIAN_POINT ( 'NONE',  ( -3.475000000000000533, -1.385416665710749617, -2.006292185433948827 ) ) ;
#74200 = CARTESIAN_POINT ( 'NONE',  ( -4.928552533767591726, 5.708731696605642725, 1.199719254218462483 ) ) ;
#74201 = CARTESIAN_POINT ( 'NONE',  ( 0.2115809916233695465, 1.842269378952247738, -1.241004044093022340 ) ) ;
#74202 = CARTESIAN_POINT ( 'NONE',  ( 2.643703295229280936, -1.559600718570711031, -1.415347570850413739 ) ) ;
#74203 = CARTESIAN_POINT ( 'NONE',  ( -3.923105346307911745, 5.670318552149568703, -1.599625672291283607 ) ) ;
#74204 = CARTESIAN_POINT ( 'NONE',  ( 6.753933077901968396, 11.03133902419432566, 0.7998128361456462443 ) ) ;
#74205 = CARTESIAN_POINT ( 'NONE',  ( 6.403157621081472683, -1.572583794901558862, 0.9946829920960180704 ) ) ;
#74206 = CARTESIAN_POINT ( 'NONE',  ( 7.450369105909416589, 8.650851030771185890, -1.199719254218441611 ) ) ;
#74207 = CARTESIAN_POINT ( 'NONE',  ( -6.699137298928187434, 8.909022496873262753, 1.443375672974064550 ) ) ;
#74208 = CARTESIAN_POINT ( 'NONE',  ( -7.863365906246054138, 11.15738207638699464, -1.082531754730543971 ) ) ;
#74209 = CARTESIAN_POINT ( 'NONE',  ( -0.1753031400193918732, -0.9122597987226389593, -1.912455998546586544 ) ) ;
#74210 = CARTESIAN_POINT ( 'NONE',  ( -6.050681693448748177, 10.28115541899069463, 0.7998128361456291469 ) ) ;
#74212 = CARTESIAN_POINT ( 'NONE',  ( 2.787496613063783713, -1.831585881375777713, 0.7034878451678548972 ) ) ;
#74211 = CARTESIAN_POINT ( 'NONE',  ( -1.552391752028397856E-14, -0.5624999999999785727, -1.414508159514605401 ) ) ;
#74213 = CARTESIAN_POINT ( 'NONE',  ( 1.903414394802248166, 1.797162532295241366, 1.201017911493490020 ) ) ;
#74215 = CARTESIAN_POINT ( 'NONE',  ( -4.699291399009611681, 6.864061528938182555, -1.228208583504811990 ) ) ;
#74214 = CARTESIAN_POINT ( 'NONE',  ( -4.339491684825780737, 7.220434844675483355, -1.199719254218455378 ) ) ;
#74216 = CARTESIAN_POINT ( 'NONE',  ( -1.402160292154681736E-14, 1.946875000341422579, -1.575800808251660134 ) ) ;
#74217 = CARTESIAN_POINT ( 'NONE',  ( 3.872797606970843631, 1.637851192275063816, -0.5887498661538635991 ) ) ;
#74218 = CARTESIAN_POINT ( 'NONE',  ( 5.829642864196162400, 7.824335979694092558, 1.443375672974062551 ) ) ;
#74219 = CARTESIAN_POINT ( 'NONE',  ( -11.38508626655161216, 5.468933214068770532, 5.576081633246319669 ) ) ;
#74220 = CARTESIAN_POINT ( 'NONE',  ( 1.985703663612121472, 1.880146017696176619, 0.7282698753105636413 ) ) ;
#74221 = CARTESIAN_POINT ( 'NONE',  ( -3.070819976954469066, 2.800000000000024691, 2.497101503361902619 ) ) ;
#74222 = DIRECTION ( 'NONE',  ( 1.000000000000000000, 0.000000000000000000, -4.336808689942015369E-15 ) ) ;
#74223 = CARTESIAN_POINT ( 'NONE',  ( 2.061341786089391004, 0.3389245507335619245, -1.941969530725436766 ) ) ;
#74224 = AXIS2_PLACEMENT_3D ( 'NONE', #95277, #128895, #94208 ) ;
#74225 = B_SPLINE_CURVE_WITH_KNOTS ( 'NONE', 1,
 ( #32060, #34174 ),
 .UNSPECIFIED., .F., .F.,
 ( 2, 2 ),
 ( 0.000000000000000000, 0.5613011892072224951 ),
 .UNSPECIFIED. ) ;
#74228 = EDGE_LOOP ( 'NONE', ( #60932, #29354, #12640, #171493, #192050 ) ) ;
#74227 = CARTESIAN_POINT ( 'NONE',  ( -5.695833931516914639, 6.778132687258748845, 1.082531754730549078 ) ) ;
#74226 = SURFACE_STYLE_FILL_AREA ( #170643 ) ;
#74229 = CARTESIAN_POINT ( 'NONE',  ( -4.285785955251283141, 8.014184357852876417, 0.000000000000000000 ) ) ;
#74230 = CARTESIAN_POINT ( 'NONE',  ( 6.170896192875352959, 7.228408975556602556, 1.199719254218453823 ) ) ;
#74231 = CIRCLE ( 'NONE', #87988, 0.07999999999999998779 ) ;
#74232 = CARTESIAN_POINT ( 'NONE',  ( -6.577640801285370209, 7.702944352034914566, -1.199719254218452047 ) ) ;
#74233 = CARTESIAN_POINT ( 'NONE',  ( 2.104171369714701534, -0.8614446868937111201, 1.826873676003283320 ) ) ;
#74234 = CARTESIAN_POINT ( 'NONE',  ( -8.785320351530977234, 13.19336481018743079, 1.040834085586084257E-14 ) ) ;
#74235 = CARTESIAN_POINT ( 'NONE',  ( 5.579250153011313884, -0.04958841179729735205, -2.307219497322360535 ) ) ;
#74236 = CARTESIAN_POINT ( 'NONE',  ( 2.550000000000000266, -7.105553651663779391, 1.849324200890695824 ) ) ;
#74237 = CARTESIAN_POINT ( 'NONE',  ( 2.553501467334079678, 1.513274546892771966, 1.248348448719404757 ) ) ;
#74238 = CARTESIAN_POINT ( 'NONE',  ( 8.259941899223605333, 10.65968485389279508, -1.599625672291268286 ) ) ;
#74239 = CARTESIAN_POINT ( 'NONE',  ( 0.6510177983308338412, 0.9963039324867200008, 1.753029211773032392 ) ) ;
#74240 = ORIENTED_EDGE ( 'NONE', *, *, #186277, .F. ) ;
#74241 = CARTESIAN_POINT ( 'NONE',  ( 2.149754410345839251, 2.075462379332591478, -0.4182697058867020923 ) ) ;
#74243 = CARTESIAN_POINT ( 'NONE',  ( -5.669280788808708671, 9.765911353585494226, 0.7998128361456481317 ) ) ;
#74242 = FACE_BOUND ( 'NONE', #97818, .T. ) ;
#74244 = CARTESIAN_POINT ( 'NONE',  ( 1.728195974063054141, 0.1793598003074353686, 1.832383557197496460 ) ) ;
#74245 = ORIENTED_EDGE ( 'NONE', *, *, #199925, .T. ) ;
#74246 = CARTESIAN_POINT ( 'NONE',  ( -7.784352752540590004, 12.23349531127272094, 0.7998128361456481317 ) ) ;
#74247 = DIRECTION ( 'NONE',  ( 0.000000000000000000, 0.000000000000000000, 1.000000000000000000 ) ) ;
#74248 = CARTESIAN_POINT ( 'NONE',  ( 3.814780496183818315, -0.6684712460508880350, -2.012520831323429515 ) ) ;
#74249 = CARTESIAN_POINT ( 'NONE',  ( 6.667919370488161412, -1.192936252400189190, 1.533121312111614065 ) ) ;
#74250 = CARTESIAN_POINT ( 'NONE',  ( -0.7499999999999972244, 5.139583334016151639, -1.299038105676652899 ) ) ;
#74251 = CARTESIAN_POINT ( 'NONE',  ( 7.263417608619159083, 9.497073181520933716, -1.599625672291262513 ) ) ;
#74252 = CARTESIAN_POINT ( 'NONE',  ( 7.038618024149998043, 8.240751112043669835, -1.199719254218452047 ) ) ;
#74253 = CARTESIAN_POINT ( 'NONE',  ( 4.112614458092584968, 1.460029904434188008, -1.454618372460781295 ) ) ;
#74255 = CARTESIAN_POINT ( 'NONE',  ( 1.663359199420410883, 0.9473472845980964729, 1.578708189602283873 ) ) ;
#74254 = CARTESIAN_POINT ( 'NONE',  ( -7.874588291438845644, 8.081441182967111558, -0.7998128361456291469 ) ) ;
#74256 = CARTESIAN_POINT ( 'NONE',  ( -1.364683531249997417, 5.259375000341425022, 1.214306433183764966E-14 ) ) ;
#74257 = FACE_BOUND ( 'NONE', #9375, .T. ) ;
#74258 = CARTESIAN_POINT ( 'NONE',  ( -2.972099262745669712, 6.689475916503727859, 0.05200437644970179463 ) ) ;
#74259 = FACE_OUTER_BOUND ( 'NONE', #56252, .T. ) ;
#74260 = CARTESIAN_POINT ( 'NONE',  ( 1.102499568101540817, -2.207063161980229005, 0.003256074490760872773 ) ) ;
#74261 = CARTESIAN_POINT ( 'NONE',  ( 4.253392140805613231, -1.877938019876054243, -1.261413133637336204 ) ) ;
#74262 = CARTESIAN_POINT ( 'NONE',  ( -8.026063749610056419, 10.38682701267698150, -1.443375672974059665 ) ) ;
#74263 = CARTESIAN_POINT ( 'NONE',  ( 3.480526544955347301, -1.212856340575025005, 1.345865543471187253 ) ) ;
#74264 = CARTESIAN_POINT ( 'NONE',  ( 2.606530347446478046, 1.805417332896454230, 0.6411187296449465389 ) ) ;
#74265 = CARTESIAN_POINT ( 'NONE',  ( 3.877443546529443452, -0.1552652338182025915, 2.064615508632794860 ) ) ;
#74266 = CARTESIAN_POINT ( 'NONE',  ( 1.364683531249990311, 3.196875000341416140, 1.214306433183764966E-14 ) ) ;
#74267 = CARTESIAN_POINT ( 'NONE',  ( 3.063307058708428787, 0.2908816738307045680, -1.949781715572605600 ) ) ;
#74268 = PRODUCT_RELATED_PRODUCT_CATEGORY ( 'part', '', ( #192368 ) ) ;
#74269 = CARTESIAN_POINT ( 'NONE',  ( 0.6746739519505640104, -1.812841073067989361, -0.6519485973254712796 ) ) ;
#74270 = CARTESIAN_POINT ( 'NONE',  ( 3.555401268124198655, 0.4554524271490404952, -1.814226883376020671 ) ) ;
#74271 = CARTESIAN_POINT ( 'NONE',  ( 2.034188542434863578, -1.509292173632442280, -1.745791301847523513 ) ) ;
#74272 = CARTESIAN_POINT ( 'NONE',  ( 4.017883236588020601, 1.847182159994051442, -0.2260418734564421939 ) ) ;
#74273 = CARTESIAN_POINT ( 'NONE',  ( 1.364683531249990311, 4.613541667008083103, 0.7879004041258500513 ) ) ;
#74274 = CARTESIAN_POINT ( 'NONE',  ( -3.276266675996675204, 6.974061555304760240, -0.7998128361456281477 ) ) ;
#74275 = CARTESIAN_POINT ( 'NONE',  ( 5.612185521052973414, 8.634967976948757951, -1.199719254218440723 ) ) ;
#74276 = CARTESIAN_POINT ( 'NONE',  ( 0.000000000000000000, 13.79999999999999893, 0.000000000000000000 ) ) ;
#74277 = CARTESIAN_POINT ( 'NONE',  ( 0.2410290108679030985, 0.3623031737408002884, 2.074505700167991407 ) ) ;
#74278 = CARTESIAN_POINT ( 'NONE',  ( 3.836594282542920009, 4.538743420130594508, 1.082531754730560403 ) ) ;
#74280 = DIRECTION ( 'NONE',  ( 0.000000000000000000, 0.000000000000000000, -1.000000000000000000 ) ) ;
#74279 = CARTESIAN_POINT ( 'NONE',  ( -1.364683531250010295, 4.342708333674753618, 0.7879004041258379498 ) ) ;
#74281 = CARTESIAN_POINT ( 'NONE',  ( 1.810938747355747447, -0.5704394276861005642, -2.042344090522000055 ) ) ;
#74282 = CARTESIAN_POINT ( 'NONE',  ( 1.125267019654611733, 1.783345095244772249, 0.9482059100444378830 ) ) ;
#74283 = CARTESIAN_POINT ( 'NONE',  ( -1.364683531250014514, 0.9885416670080898749, -0.7879004041258289570 ) ) ;
#74284 = CARTESIAN_POINT ( 'NONE',  ( -4.284013352238255301, 6.981470763377843447, -1.082531754730549967 ) ) ;
#74285 = CARTESIAN_POINT ( 'NONE',  ( 4.852928918687680948, 7.749168607522574526, 1.199719254218462483 ) ) ;
#74286 = CARTESIAN_POINT ( 'NONE',  ( 1.071799524545346216, 2.083542002058445863, -0.5754571431841256635 ) ) ;
#74289 = CARTESIAN_POINT ( 'NONE',  ( 4.202664430556254160, 5.926194473780837413, 1.443375672974062551 ) ) ;
#74288 = CARTESIAN_POINT ( 'NONE',  ( 6.825078400183572036, 4.699117039843025090, 2.418333817060664526 ) ) ;
#74287 = CARTESIAN_POINT ( 'NONE',  ( 4.376249722160992839, 8.327651452488305850, 0.000000000000000000 ) ) ;
#74290 = CARTESIAN_POINT ( 'NONE',  ( -0.2104748580754391973, 0.7011259924453935310, -2.185273273056092869 ) ) ;
#74291 = CARTESIAN_POINT ( 'NONE',  ( 5.454314652423888354, -1.275559214091715354, 1.561879324423600668 ) ) ;
#74293 = CARTESIAN_POINT ( 'NONE',  ( -5.112833325684904118, 8.979072956692109031, -0.7216878364870338292 ) ) ;
#74292 = CARTESIAN_POINT ( 'NONE',  ( -8.893785580884703279, 10.43879993486270585, 1.082531754730558626 ) ) ;
#74294 = CARTESIAN_POINT ( 'NONE',  ( -9.340724465469246951, 14.55305236562982962, -7.462818192253934946 ) ) ;
#74296 = CARTESIAN_POINT ( 'NONE',  ( -1.364683531250014514, 11.08854166700806054, -0.7879004041258335089 ) ) ;
#74295 = CARTESIAN_POINT ( 'NONE',  ( 0.4271420986578051138, 2.166143833277152542, 0.6532491227348672380 ) ) ;
#74297 = CARTESIAN_POINT ( 'NONE',  ( -9.459838494033043332, 12.05956421450382088, 1.599625672291281386 ) ) ;
#74299 = CARTESIAN_POINT ( 'NONE',  ( 0.7728743906838764222, 1.688931763573727540, -0.9039392725495792869 ) ) ;
#74298 = CARTESIAN_POINT ( 'NONE',  ( -6.046573321570485327, 6.156683084694754449, 0.000000000000000000 ) ) ;
#74300 = CARTESIAN_POINT ( 'NONE',  ( -0.6823417656250212460, 1.363541667008083547, 1.181850606188755259 ) ) ;
#74301 = CARTESIAN_POINT ( 'NONE',  ( -1.499999999999997780, 4.400000000000021672, 1.214306433183764966E-14 ) ) ;
#74302 = CARTESIAN_POINT ( 'NONE',  ( 1.499999999999993117, 8.604166666666664298, 0.8660254037844409281 ) ) ;
#74303 = CARTESIAN_POINT ( 'NONE',  ( 2.367434161175852925, 1.691737554211050210, -0.3355112704105273624 ) ) ;
#74304 = CARTESIAN_POINT ( 'NONE',  ( 5.643937085038755797, 9.806620042512378177, -0.7998128361456481317 ) ) ;
#74305 = CARTESIAN_POINT ( 'NONE',  ( 6.215487077222150880, 6.216099443039444949, 0.000000000000000000 ) ) ;
#74306 = CARTESIAN_POINT ( 'NONE',  ( 0.3855647087021807362, -0.8419519913594010196, 1.556653678627561543 ) ) ;
#74307 = CARTESIAN_POINT ( 'NONE',  ( 2.297522961200649139, 1.839619113207457524, -0.8179307585152847393 ) ) ;
#74308 =( LENGTH_UNIT ( ) NAMED_UNIT ( * ) SI_UNIT ( .MILLI., .METRE. ) );
#74309 = CARTESIAN_POINT ( 'NONE',  ( 10.18233705906309972, 11.83814697611718714, 1.199719254218450271 ) ) ;
#74310 = CARTESIAN_POINT ( 'NONE',  ( 3.680891063843365174, -2.126115503207156809, -0.5908918699835326027 ) ) ;
#74311 = ORIENTED_EDGE ( 'NONE', *, *, #120127, .T. ) ;
#74312 = CARTESIAN_POINT ( 'NONE',  ( 7.388830529323379359, 11.56412668427855195, -0.7216878364870267237 ) ) ;
#74314 = CARTESIAN_POINT ( 'NONE',  ( 3.234000073275579812, 2.016598147164900823, -0.002828922958116042007 ) ) ;
#74313 = CARTESIAN_POINT ( 'NONE',  ( 4.582752651445391123, -1.384437811569695587, 1.606279107262520434 ) ) ;
#74316 = ORIENTED_EDGE ( 'NONE', *, *, #132981, .F. ) ;
#74315 = CARTESIAN_POINT ( 'NONE',  ( 3.498146571883210321, -0.8881612436112231723, 1.578813691393302410 ) ) ;
#74317 = CARTESIAN_POINT ( 'NONE',  ( 5.224688093219824303, 7.188831756880171397, -1.599625672291283607 ) ) ;
#74318 = ORIENTED_EDGE ( 'NONE', *, *, #19773, .T. ) ;
#74319 = CARTESIAN_POINT ( 'NONE',  ( 1.744777856283234785, -1.581906188472384400, 0.9981555316627908070 ) ) ;
#74320 = AXIS2_PLACEMENT_3D ( 'NONE', #8575, #73579, #107218 ) ;
#74321 = CARTESIAN_POINT ( 'NONE',  ( 5.707590141996651489, -0.4392596013848491521, 1.771934311310577659 ) ) ;
#74322 = CARTESIAN_POINT ( 'NONE',  ( -2.252626078164912560, 5.779814191167667481, 0.7998128361456341429 ) ) ;
#74323 = DIRECTION ( 'NONE',  ( -0.000000000000000000, -8.546850786086437571E-32, -1.000000000000000000 ) ) ;
#74324 = CARTESIAN_POINT ( 'NONE',  ( -1.451998047845039830, 7.315968950354585942, -4.301760722576429607 ) ) ;
#74325 = AXIS2_PLACEMENT_3D ( 'NONE', #98338, #182770, #13864 ) ;
#74326 = CARTESIAN_POINT ( 'NONE',  ( -1.364683531250014514, 1.301041667008083325, -0.7879004041258289570 ) ) ;
#74327 = DIRECTION ( 'NONE',  ( -0.9998476951563912696, 0.000000000000000000, 0.01745240643728004568 ) ) ;
#74328 = CARTESIAN_POINT ( 'NONE',  ( 7.526184669361807522, 7.953172667109813077, 0.000000000000000000 ) ) ;
#74329 = CARTESIAN_POINT ( 'NONE',  ( -5.478903473698268023, 5.564677938835638216, -0.7216878364870338292 ) ) ;
#74330 = CARTESIAN_POINT ( 'NONE',  ( -7.422162748838431412, 7.623887726591770608, -0.7998128361456362523 ) ) ;
#74331 = CARTESIAN_POINT ( 'NONE',  ( 4.570628194609677841, 0.8141925398062774821, 1.958264201954627026 ) ) ;
#74333 = CARTESIAN_POINT ( 'NONE',  ( -11.40891844150367618, 9.366729182080655747, 1.257950088934312705 ) ) ;
#74332 = CARTESIAN_POINT ( 'NONE',  ( -0.02968770228137588424, 5.725071598255107475, -2.420367217772397606 ) ) ;
#74334 = CARTESIAN_POINT ( 'NONE',  ( 4.376219360443936779, -1.137518282590570751, 1.609873005976544924 ) ) ;
#74336 = CARTESIAN_POINT ( 'NONE',  ( 6.381121926128928479, -1.751337275642101510, -0.7685668267764720341 ) ) ;
#74335 = VECTOR ( 'NONE', #159243, 1000.000000000000000 ) ;
#74337 = ORIENTED_EDGE ( 'NONE', *, *, #65502, .T. ) ;
#74338 = CARTESIAN_POINT ( 'NONE',  ( -0.1232448511370512201, -0.4725888426768353190, -2.071762565325820038 ) ) ;
#74339 = CARTESIAN_POINT ( 'NONE',  ( 0.9771079587245214970, 1.912259438035465386, 0.7939916666956441382 ) ) ;
#74340 = CARTESIAN_POINT ( 'NONE',  ( 5.345657705538078730, 9.458627433094950021, 0.7998128361456331437 ) ) ;
#74341 = ORIENTED_EDGE ( 'NONE', *, *, #193470, .F. ) ;
#74342 = CARTESIAN_POINT ( 'NONE',  ( 6.717138760927786834, 6.801359740696030443, -0.7998128361456481317 ) ) ;
#74343 = CARTESIAN_POINT ( 'NONE',  ( 6.688968683495743583, 8.897159112202094988, -1.599625672291283607 ) ) ;
#74345 = CARTESIAN_POINT ( 'NONE',  ( 4.981731378017507872, 7.899438143407371271, -1.199719254218452047 ) ) ;
#74344 = CARTESIAN_POINT ( 'NONE',  ( 3.908215892115148637, 1.478387765550030153, -1.478483494758761951 ) ) ;
#74346 = CARTESIAN_POINT ( 'NONE',  ( 5.688527969385528849, 8.794310509995222347, -1.199719254218452047 ) ) ;
#74349 = VERTEX_POINT ( 'NONE', #36176 ) ;
#74348 = CARTESIAN_POINT ( 'NONE',  ( 0.7854713186128524649, 1.746033005210102962, -0.4821264535347525859 ) ) ;
#74347 = CARTESIAN_POINT ( 'NONE',  ( 1.746812667857342349, -1.544096848276183209, 0.9736100143667850704 ) ) ;
#74350 = CARTESIAN_POINT ( 'NONE',  ( 6.024089167411393220, -1.222679950896175205, -1.837027303407394507 ) ) ;
#74351 = CARTESIAN_POINT ( 'NONE',  ( -0.2680151545362914889, -6.654245765634851040, -10.99740610014212550 ) ) ;
#74352 = CARTESIAN_POINT ( 'NONE',  ( 4.120313900606538127, -1.131812998600056241, -1.894281110011143632 ) ) ;
#74353 = CARTESIAN_POINT ( 'NONE',  ( 0.6823417656249969321, 8.588541667008065872, -1.181850606188757036 ) ) ;
#74354 = CARTESIAN_POINT ( 'NONE',  ( 2.350135150926917493, 0.8998847150011926033, -1.687291145760522859 ) ) ;
#74355 = CARTESIAN_POINT ( 'NONE',  ( 8.934986926605834157, 10.38290515491702770, -1.199719254218446718 ) ) ;
#74356 = CARTESIAN_POINT ( 'NONE',  ( 5.582505937350194181, 1.236201877336528421, -1.660625051266072960 ) ) ;
#74357 = VECTOR ( 'NONE', #165403, 1000.000000000000000 ) ;
#74359 = CARTESIAN_POINT ( 'NONE',  ( -1.567404983201070801, 8.684828555514158666, -2.500997594616635844 ) ) ;
#74358 = CARTESIAN_POINT ( 'NONE',  ( 1.513761821635687177, 8.683429030108589686, -2.534756493980068637 ) ) ;
#74360 = CARTESIAN_POINT ( 'NONE',  ( 5.724229345562060089, 2.111793275502030554, 0.5857118945327836057 ) ) ;
#74361 = ORIENTED_EDGE ( 'NONE', *, *, #134113, .T. ) ;
#74362 = EDGE_LOOP ( 'NONE', ( #3214, #2889, #35224, #47842 ) ) ;
#74363 = CARTESIAN_POINT ( 'NONE',  ( 3.475000000000000533, -2.231249999044084831, 0.000000000000000000 ) ) ;
#74364 = CARTESIAN_POINT ( 'NONE',  ( 4.008199524592567897, 7.584238231759597326, 0.2402771892247856922 ) ) ;
#74365 = CARTESIAN_POINT ( 'NONE',  ( 5.923986774528332333, 5.876015756563318426, -0.7998128361456481317 ) ) ;
#74366 = CARTESIAN_POINT ( 'NONE',  ( -0.02319159430949970652, 4.096340798889516854, -2.366022381217198767 ) ) ;
#74367 = CARTESIAN_POINT ( 'NONE',  ( -3.923105346307911745, 5.670318552149568703, -1.599625672291283607 ) ) ;
#74369 = CARTESIAN_POINT ( 'NONE',  ( -8.514157279702033065, 9.995900250149611921, -1.082531754730543971 ) ) ;
#74368 = CIRCLE ( 'NONE', #32933, 0.5000000000000008882 ) ;
#74370 = CARTESIAN_POINT ( 'NONE',  ( 3.736153849017632922, 6.516540702899320081, -1.199719254218453823 ) ) ;
#74371 = CARTESIAN_POINT ( 'NONE',  ( 5.664915734613279241, 1.571387620024040421, -1.347999112033698266 ) ) ;
#74372 = CARTESIAN_POINT ( 'NONE',  ( 4.477124871421138685, -0.001476069148669684195, -1.926676517386548992 ) ) ;
#74373 = CARTESIAN_POINT ( 'NONE',  ( 6.415624682135008250, -1.382911306069923407, -1.603242893440869343 ) ) ;
#74374 = FILL_AREA_STYLE_COLOUR ( '', #146188 ) ;
#74375 = CARTESIAN_POINT ( 'NONE',  ( 8.018721507839716267, 8.319872945426633137, -0.7998128361456341429 ) ) ;
#74376 = CARTESIAN_POINT ( 'NONE',  ( -5.608757509019071108, 5.629766575900002401, 7.500000000000000000 ) ) ;
#74377 = CARTESIAN_POINT ( 'NONE',  ( 0.5686479265839607944, -2.064760635122906418, -0.7346842419702694915 ) ) ;
#74378 = CARTESIAN_POINT ( 'NONE',  ( 5.338443970399977978, 1.799313579390570128, 0.3082849261525285600 ) ) ;
#74379 = CARTESIAN_POINT ( 'NONE',  ( 6.699137298928158124, 6.988284068270579574, 0.7216878364870328300 ) ) ;
#74380 = EDGE_CURVE ( 'NONE', #55552, #37994, #128538, .T. ) ;
#74381 = CARTESIAN_POINT ( 'NONE',  ( 3.511198595814926993, 6.079853547550633230, 1.082531754730558626 ) ) ;
#74382 = CARTESIAN_POINT ( 'NONE',  ( -4.444040490229335560, 8.406740681901359480, 0.7998128361456352531 ) ) ;
#74383 = CARTESIAN_POINT ( 'NONE',  ( 5.705283713252285338, 5.550585841749444249, -0.7998128361456211532 ) ) ;
#74384 = CARTESIAN_POINT ( 'NONE',  ( 3.528865121306874464, 7.339036084825155015, -0.7998128361456362523 ) ) ;
#74385 = VERTEX_POINT ( 'NONE', #170448 ) ;
#74387 = CARTESIAN_POINT ( 'NONE',  ( 6.433844876963536130, -1.951739824409718160, 0.4931976252120565118 ) ) ;
#74386 = CARTESIAN_POINT ( 'NONE',  ( 2.225889136967126536, 1.786374552192676823, 0.4457033907802817052 ) ) ;
#74388 = CARTESIAN_POINT ( 'NONE',  ( 0.9315567102232256147, 1.134920720140248251, 1.998545780126102844 ) ) ;
#74389 = CARTESIAN_POINT ( 'NONE',  ( 6.350445966956749899, -1.952004966925089624, -0.1956573963535559180 ) ) ;
#74390 = CARTESIAN_POINT ( 'NONE',  ( -5.473741331615264549, 7.409117525016355010, -1.599625672291256295 ) ) ;
#74391 = CARTESIAN_POINT ( 'NONE',  ( -4.911143975938936812, 6.978132228647320190, -1.257868731225549208 ) ) ;
#74392 = CARTESIAN_POINT ( 'NONE',  ( -3.110706179331648169, 5.716575411607132118, 1.199719254218462483 ) ) ;
#74394 = EDGE_CURVE ( 'NONE', #149864, #97098, #183783, .T. ) ;
#74393 = CARTESIAN_POINT ( 'NONE',  ( 0.9419464005683108043, 1.389173191389100337, 1.535309223701806447 ) ) ;
#74395 = CARTESIAN_POINT ( 'NONE',  ( -4.228163802615396705, 6.026220084508304708, -1.599625672291271394 ) ) ;
#74397 = CARTESIAN_POINT ( 'NONE',  ( 1.586564105604048480, -0.2713065988851799393, -1.850747533123621391 ) ) ;
#74396 = CARTESIAN_POINT ( 'NONE',  ( 2.700817844316987237, 1.767710524334182853, 1.116111477495850934 ) ) ;
#74398 = CARTESIAN_POINT ( 'NONE',  ( 2.284529629648517801, -1.956262009633228605, 0.4871271731112236658 ) ) ;
#74399 = CARTESIAN_POINT ( 'NONE',  ( 9.598809568795314107, 10.30095870645710754, -0.7216878364870257245 ) ) ;
#74400 = ORIENTED_EDGE ( 'NONE', *, *, #81569, .T. ) ;
#74401 = CARTESIAN_POINT ( 'NONE',  ( -1.201851678989727383E-14, 4.009375000341416140, -1.575800808251660134 ) ) ;
#74402 = CARTESIAN_POINT ( 'NONE',  ( 1.786251233324965826, 1.514223802825481302, -0.8579289008448316434 ) ) ;
#74403 = CARTESIAN_POINT ( 'NONE',  ( 4.798696304233017074, 7.685897223992134819, -1.199719254218452047 ) ) ;
#74405 = CARTESIAN_POINT ( 'NONE',  ( 0.3402877347799608265, 2.652045119545964891, -1.971798190796337336 ) ) ;
#74404 = CARTESIAN_POINT ( 'NONE',  ( 1.416786528094139630, 7.999640415717689912, 11.00953083556808387 ) ) ;
#74406 = CARTESIAN_POINT ( 'NONE',  ( 3.334305206967770552, 1.683047542859770429, 0.3767605245002195180 ) ) ;
#74407 = CARTESIAN_POINT ( 'NONE',  ( 2.999763140970078901, -2.188934734890151113, 0.1099877568606702771 ) ) ;
#74408 = CARTESIAN_POINT ( 'NONE',  ( 5.602238545945851023, -2.207063162045197924, -0.003355105161521875021 ) ) ;
#74409 = CARTESIAN_POINT ( 'NONE',  ( -11.19531657929523583, 4.806608400964729633, -5.951317567608690240 ) ) ;
#74410 = CARTESIAN_POINT ( 'NONE',  ( 1.991327249661909882, 0.2097703728867078010, 2.160876515670279385 ) ) ;
#74411 = CARTESIAN_POINT ( 'NONE',  ( 1.295219883412350503, 1.381147610352757127, 1.194082977437810333 ) ) ;
#74412 = CARTESIAN_POINT ( 'NONE',  ( 1.499999999998099076, 8.654187183607731981, -2.562246142702386376 ) ) ;
#74413 = CARTESIAN_POINT ( 'NONE',  ( 3.608711286396129481, 2.011918449240827744, 0.6600949426460513969 ) ) ;
#74414 = CARTESIAN_POINT ( 'NONE',  ( -1.387358672536882054, 7.315968950353378020, 4.254625267137783773 ) ) ;
#74415 = EDGE_LOOP ( 'NONE', ( #191386, #131176, #176473, #202133 ) ) ;
#74417 = CARTESIAN_POINT ( 'NONE',  ( -0.6823417656250212460, 1.613541667008083769, 1.181850606188755259 ) ) ;
#74416 = CARTESIAN_POINT ( 'NONE',  ( 3.368946006165595364, 0.05471657373835739357, -2.291868861755571363 ) ) ;
#74418 = CARTESIAN_POINT ( 'NONE',  ( 11.41157692552970460, 11.25910337086998148, 3.404533818002359880 ) ) ;
#74419 = CARTESIAN_POINT ( 'NONE',  ( 2.679707916995359263, 6.278076336469897711, -0.7998128361456291469 ) ) ;
#74420 = CARTESIAN_POINT ( 'NONE',  ( 0.5047332052380922862, -2.104974169346077506, -0.2554120829242333968 ) ) ;
#74421 = CARTESIAN_POINT ( 'NONE',  ( -4.446711195602239819, 8.131654128270509929, -0.7216878364870267237 ) ) ;
#74422 = CARTESIAN_POINT ( 'NONE',  ( 2.562127843302666186, 5.932973550587659517, 0.000000000000000000 ) ) ;
#74423 = CARTESIAN_POINT ( 'NONE',  ( -6.575341312503472757, 7.733948288417905381, 1.082531754730549967 ) ) ;
#74424 = ADVANCED_FACE ( 'NONE', ( #6861 ), #89228, .F. ) ;
#74425 = CARTESIAN_POINT ( 'NONE',  ( 6.825078400183573812, 0.002648415797040087893, 1.855566311045192540 ) ) ;
#74426 = ORIENTED_EDGE ( 'NONE', *, *, #159272, .F. ) ;
#74427 = CARTESIAN_POINT ( 'NONE',  ( 4.711564657724523819, 1.930417226389494090, 0.5826574956761670920 ) ) ;
#74429 = CARTESIAN_POINT ( 'NONE',  ( 3.362228078103552953, -2.060403055893737623, 0.09660672959950138139 ) ) ;
#74428 = CARTESIAN_POINT ( 'NONE',  ( 4.635998460869027227, 7.496083073400806818, -1.199719254218452047 ) ) ;
#74430 = CARTESIAN_POINT ( 'NONE',  ( 7.289443866002793371, 8.533381260871966134, 1.199719254218452047 ) ) ;
#74431 = CARTESIAN_POINT ( 'NONE',  ( 5.207740400980577888, 5.248321020665011716, 0.000000000000000000 ) ) ;
#74432 = CARTESIAN_POINT ( 'NONE',  ( -1.642778471874998480, -3.901041666188709289, 2.845375778867863303 ) ) ;
#74433 = CARTESIAN_POINT ( 'NONE',  ( 1.734723475976807094E-15, -3.469446951953614189E-15, -0.2879360613984097150 ) ) ;
#74434 = CARTESIAN_POINT ( 'NONE',  ( 6.456982561897790518, 0.3786298020890948024, -2.158335565738931816 ) ) ;
#74435 = CARTESIAN_POINT ( 'NONE',  ( 3.990861413484114273, -2.010826503599131065, 0.1511389102963680842 ) ) ;
#74436 = CARTESIAN_POINT ( 'NONE',  ( 3.860763913883006992, 0.2215400755124704024, -1.827792592973469743 ) ) ;
#74437 = CARTESIAN_POINT ( 'NONE',  ( 6.012151052656117933, 9.101594430485762999, 1.199719254218460707 ) ) ;
#74438 = CARTESIAN_POINT ( 'NONE',  ( 6.721730220878607831, -1.769880579078547012, 0.4471725050417332814 ) ) ;
#74439 = CARTESIAN_POINT ( 'NONE',  ( -7.063961727919978451, 8.200042423116789436, 1.199719254218450271 ) ) ;
#74440 = CARTESIAN_POINT ( 'NONE',  ( 0.5446534387809185418, 2.256470935699141034, 0.1650129453365980214 ) ) ;
#74441 = CARTESIAN_POINT ( 'NONE',  ( 2.385502688336095911, 1.925211662925530254, -0.8542917040773172488 ) ) ;
#74442 = CARTESIAN_POINT ( 'NONE',  ( -4.586401103172829785, 8.572828063668767484, 0.7998128361456281477 ) ) ;
#74443 = CARTESIAN_POINT ( 'NONE',  ( 6.889514614038635187, 11.18951748302043114, -0.7998128361456291469 ) ) ;
#74444 = CARTESIAN_POINT ( 'NONE',  ( 7.797347741190739256, 8.269529584243604958, 0.7216878364870267237 ) ) ;
#74446 = VECTOR ( 'NONE', #166992, 1000.000000000000000 ) ;
#74445 = CARTESIAN_POINT ( 'NONE',  ( -7.063961727919978451, 8.200042423116789436, 1.199719254218450271 ) ) ;
#74447 = CARTESIAN_POINT ( 'NONE',  ( 7.009202228140744673, 9.200488570962775725, -1.443375672974058777 ) ) ;
#74448 = CARTESIAN_POINT ( 'NONE',  ( 4.176068722599148408, 7.364853391560295393, -0.8050483301465498620 ) ) ;
#74449 = CARTESIAN_POINT ( 'NONE',  ( -4.924636110261798372, 6.768494766770632332, 1.599625672291267398 ) ) ;
#74450 = CARTESIAN_POINT ( 'NONE',  ( 3.867602925442710671, -1.848332671738551980, -1.231929692598219050 ) ) ;
#74451 = CARTESIAN_POINT ( 'NONE',  ( 1.271705539736139423, 1.307743536042236920, 1.758333696453084016 ) ) ;
#74452 = CARTESIAN_POINT ( 'NONE',  ( 0.3818278861203865393, 2.057605126571937060, -0.7983354260262252033 ) ) ;
#74453 = CARTESIAN_POINT ( 'NONE',  ( -3.610214042988883598, 7.433943160120816351, 0.7998128361456352531 ) ) ;
#74454 = CARTESIAN_POINT ( 'NONE',  ( 4.299235682465595509, -1.708000122724560477, 0.9650500775852040025 ) ) ;
#74455 = CARTESIAN_POINT ( 'NONE',  ( 9.728138913005292210, 11.30824913904973705, -1.199719254218440723 ) ) ;
#74456 = CARTESIAN_POINT ( 'NONE',  ( 3.708318708537623021, 4.285125567170706695, -1.199719254218446718 ) ) ;
#74457 = CARTESIAN_POINT ( 'NONE',  ( -1.364683531250014514, -0.01145833299191483488, -0.7879004041258359514 ) ) ;
#74458 = CARTESIAN_POINT ( 'NONE',  ( 6.610000000000026077, 2.442988107647511509, 2.382821027452782570 ) ) ;
#74460 = ORIENTED_EDGE ( 'NONE', *, *, #50859, .T. ) ;
#74459 = CARTESIAN_POINT ( 'NONE',  ( -5.748293942514180799, 7.729428904398431222, -1.443375672974052559 ) ) ;
#74461 = CARTESIAN_POINT ( 'NONE',  ( 2.971057270251746818, -1.603071526910588629, 1.388259434452358665 ) ) ;
#74462 = CARTESIAN_POINT ( 'NONE',  ( -4.659162064951642535, 5.464719159645540003, 1.199719254218452935 ) ) ;
#74463 = CARTESIAN_POINT ( 'NONE',  ( 5.594645800149128156, -0.5210773734287167391, -2.097845705497362712 ) ) ;
#74464 = CARTESIAN_POINT ( 'NONE',  ( 4.142028884782995135, 0.4951553702221401232, 1.773339192993342639 ) ) ;
#74465 = CARTESIAN_POINT ( 'NONE',  ( 9.305047017613611970, 4.518467169708414666, -7.450000000000005507 ) ) ;
#74466 = CARTESIAN_POINT ( 'NONE',  ( -1.364683531250000748, 0.8218750003414210248, 0.000000000000000000 ) ) ;
#74467 = CARTESIAN_POINT ( 'NONE',  ( 0.1337851541256071808, 0.2942392587969425155, 1.715217768732644643 ) ) ;
#74468 = CARTESIAN_POINT ( 'NONE',  ( 6.727182134110170075, 7.629137130509032971, 2.510944104600740356 ) ) ;
#74469 = CARTESIAN_POINT ( 'NONE',  ( 4.216222584169931231, 4.021273891060765493, 1.214306433183764966E-14 ) ) ;
#74470 = CARTESIAN_POINT ( 'NONE',  ( -2.788906526875773208E-15, 11.93750000000000000, -1.499999999999998446 ) ) ;
#74471 = CARTESIAN_POINT ( 'NONE',  ( 3.819328725847204620, -0.1613130240520690706, 2.155748724213396361 ) ) ;
#74472 = CARTESIAN_POINT ( 'NONE',  ( -3.425406365747000859, 7.148057860013469877, 1.040834085586084257E-14 ) ) ;
#74473 = CARTESIAN_POINT ( 'NONE',  ( 5.079453798366286854, 1.392331892589277142, -1.458333960840517696 ) ) ;
#74474 = CARTESIAN_POINT ( 'NONE',  ( -7.985389288324697965, 10.33937347451072775, -1.443375672974058777 ) ) ;
#74475 = CARTESIAN_POINT ( 'NONE',  ( 3.415052781332720055, 1.953485055394106107, 0.9259690932504063277 ) ) ;
#74476 =( BOUNDED_CURVE ( )  B_SPLINE_CURVE ( 2, ( #48990, #47944, #146509, #133462, #46870, #115108, #32721 ),
 .UNSPECIFIED., .F., .T. ) 
 B_SPLINE_CURVE_WITH_KNOTS ( ( 3, 2, 2, 3 ),
 ( 0.2142857142857144681, 0.2202380952380953438, 0.2261904761904762196, 0.2321428571428570953 ),
 .UNSPECIFIED. ) 
 CURVE ( )  GEOMETRIC_REPRESENTATION_ITEM ( )  RATIONAL_B_SPLINE_CURVE ( ( 0.9999999999999956701, 0.8660254037844430375, 1.000000000000000000, 0.8660254037844387076, 1.000000000000000000, 0.8660254037844399289, 0.9999999999999987788 ) ) 
 REPRESENTATION_ITEM ( '' )  );
#74477 = CARTESIAN_POINT ( 'NONE',  ( 3.989495051124877456, 1.425666444934305499, 1.361731899605103768 ) ) ;
#74478 = CIRCLE ( 'NONE', #122960, 0.08000000000000014044 ) ;
#74479 = CARTESIAN_POINT ( 'NONE',  ( -0.1290005225502675879, -0.006633637972621592160, -2.173875058097324064 ) ) ;
#74480 = CARTESIAN_POINT ( 'NONE',  ( 0.5347316126107805045, 1.182704979252725108, -1.981343935211031138 ) ) ;
#74481 = CARTESIAN_POINT ( 'NONE',  ( 3.110674321496671446, 1.495003355660160516, -1.418639704521322153 ) ) ;
#74482 = CARTESIAN_POINT ( 'NONE',  ( 5.231954969198427285, 1.913977456902911767, 0.3281912247276967398 ) ) ;
#74483 = B_SPLINE_CURVE_WITH_KNOTS ( 'NONE', 3,
 ( #29255, #110569, #174459, #12981, #140908, #211178 ),
 .UNSPECIFIED., .F., .F.,
 ( 4, 2, 4 ),
 ( 0.000000000000000000, 0.0003141553954499744054, 0.0006283107908999488109 ),
 .UNSPECIFIED. ) ;
#74484 = CARTESIAN_POINT ( 'NONE',  ( -8.527715432871366019, 10.01171809551380143, 1.082531754730558626 ) ) ;
#74485 = CARTESIAN_POINT ( 'NONE',  ( -5.281783360975562225, 8.319775133516907673, 1.199719254218452935 ) ) ;
#74486 = CARTESIAN_POINT ( 'NONE',  ( 11.84668730067608244, 10.19999999999998153, 1.399999999999998357 ) ) ;
#74488 = EDGE_LOOP ( 'NONE', ( #127888, #46263 ) ) ;
#74487 = CARTESIAN_POINT ( 'NONE',  ( -2.993318053567081360, 6.714231172462041819, 0.000000000000000000 ) ) ;
#74489 = CARTESIAN_POINT ( 'NONE',  ( -7.822691444960713447, 9.189190109618056823, -1.082531754730543083 ) ) ;
#74490 = CARTESIAN_POINT ( 'NONE',  ( 2.169229845753062325, -2.017539712319418310, -0.8944986170207609444 ) ) ;
#74491 = CARTESIAN_POINT ( 'NONE',  ( 1.642778471875001811, -0.3427083328553758301, 2.845375778867859751 ) ) ;
#74492 = ORIENTED_EDGE ( 'NONE', *, *, #68305, .F. ) ;
#74493 = CARTESIAN_POINT ( 'NONE',  ( 6.086763564210844635, 1.889667650816441391, 0.5265613530214608984 ) ) ;
#74494 =( BOUNDED_CURVE ( )  B_SPLINE_CURVE ( 3, ( #163373, #164428, #179620, #211024 ),
 .UNSPECIFIED., .F., .T. ) 
 B_SPLINE_CURVE_WITH_KNOTS ( ( 4, 4 ),
 ( 4.712388980384530690, 6.283185307179586232 ),
 .UNSPECIFIED. ) 
 CURVE ( )  GEOMETRIC_REPRESENTATION_ITEM ( )  RATIONAL_B_SPLINE_CURVE ( ( 1.000000000000000000, 0.8047378541243275230, 0.8047378541243275230, 1.000000000000000000 ) ) 
 REPRESENTATION_ITEM ( '' )  );
#74495 = CARTESIAN_POINT ( 'NONE',  ( -0.02919842301646497981, 7.629137130509056952, -2.673797582091000269 ) ) ;
#74496 = FILL_AREA_STYLE_COLOUR ( '', #128632 ) ;
#74497 = CARTESIAN_POINT ( 'NONE',  ( 9.578206935422253210, -9.825744180092243596, -0.1671882239536598425 ) ) ;
#74499 = DIRECTION ( 'NONE',  ( -1.561251128379126077E-17, -1.301042606982605475E-17, -1.000000000000000000 ) ) ;
#74498 = CARTESIAN_POINT ( 'NONE',  ( -4.650083499807267984, 5.295740330745369207, 1.164732466530402855 ) ) ;
#74500 = CARTESIAN_POINT ( 'NONE',  ( 5.542853976212075651, -1.453887124689148935, -1.129494548679485622 ) ) ;
#74501 = ORIENTED_EDGE ( 'NONE', *, *, #31532, .T. ) ;
#74502 = CARTESIAN_POINT ( 'NONE',  ( 1.885689728351304995, 1.420446345011391553, 1.493427266136108322 ) ) ;
#74503 = CARTESIAN_POINT ( 'NONE',  ( -1.360316468750013108, 1.140625000341413564, -2.081668171172168513E-14 ) ) ;
#74504 = CARTESIAN_POINT ( 'NONE',  ( -5.859094939400033120, 9.987361195942037639, -0.7998128361456231517 ) ) ;
#74505 = PLANE ( 'NONE',  #117220 ) ;
#74506 = CARTESIAN_POINT ( 'NONE',  ( 6.159481859310094620, 6.080483678816896109, 1.040834085586084257E-14 ) ) ;
#74507 = CARTESIAN_POINT ( 'NONE',  ( 0.5146158036630330557, 1.421672375139692246, -1.492246178604545115 ) ) ;
#74508 =( BOUNDED_CURVE ( )  B_SPLINE_CURVE ( 2, ( #23710, #57292, #88739, #123456, #189418, #5298, #54096, #188345, #39984 ),
 .UNSPECIFIED., .F., .T. ) 
 B_SPLINE_CURVE_WITH_KNOTS ( ( 3, 2, 2, 2, 3 ),
 ( 0.4196428571428570953, 0.4226190476190476164, 0.4285714285714285476, 0.4345238095238095344, 0.4375000000000000000 ),
 .UNSPECIFIED. ) 
 CURVE ( )  GEOMETRIC_REPRESENTATION_ITEM ( )  RATIONAL_B_SPLINE_CURVE ( ( 0.9330127018922194093, 0.9330127018922180770, 1.000000000000000000, 0.8660254037844387076, 1.000000000000000000, 0.8660254037844387076, 1.000000000000000000, 0.9330127018922194093, 0.9330127018922194093 ) ) 
 REPRESENTATION_ITEM ( '' )  );
#74510 = CARTESIAN_POINT ( 'NONE',  ( 4.563899478665734755, -1.199029595066217313, 1.397436126395680267 ) ) ;
#74509 = CARTESIAN_POINT ( 'NONE',  ( -10.91033749632886973, 4.885617943545219610, -4.996452313011736202 ) ) ;
#74511 = CARTESIAN_POINT ( 'NONE',  ( 6.608709811657416999, 9.797579649320619311, -1.199719254218440723 ) ) ;
#74512 = CARTESIAN_POINT ( 'NONE',  ( -6.089547271193396227, 7.133501900260939443, -1.199719254218453823 ) ) ;
#74514 = ORIENTED_EDGE ( 'NONE', *, *, #27400, .T. ) ;
#74513 = CARTESIAN_POINT ( 'NONE',  ( -0.7500000000000006661, 10.45833333333333393, -1.299038105676657340 ) ) ;
#74515 = TOROIDAL_SURFACE ( 'NONE', #195576, 10.89999999999920988, 0.2000000000000000111 ) ;
#74516 = CARTESIAN_POINT ( 'NONE',  ( 4.916741810085082598, 1.523553907054091328, -1.596827639139485777 ) ) ;
#74517 = CARTESIAN_POINT ( 'NONE',  ( 0.1929406647830470833, -0.4748886411078504510, -2.116594070111991410 ) ) ;
#74518 = CARTESIAN_POINT ( 'NONE',  ( -5.639828713604883248, 6.642516923036197340, 1.082531754730548412 ) ) ;
#74519 = CARTESIAN_POINT ( 'NONE',  ( -0.2049973002360427898, -0.1418364932926942379, -1.881151990943498387 ) ) ;
#74520 = CARTESIAN_POINT ( 'NONE',  ( 6.385945889491149607, -1.915137183225220197, 0.05458341080493907954 ) ) ;
#74521 = CARTESIAN_POINT ( 'NONE',  ( 7.146556367734764770, 9.431011410480991231, 1.443375672974063439 ) ) ;
#74522 = ADVANCED_FACE ( 'NONE', ( #102252 ), #190743, .T. ) ;
#74523 = CARTESIAN_POINT ( 'NONE',  ( 9.428250952287722697, 13.54490846161957585, -7.423481931054030092 ) ) ;
#74524 = CARTESIAN_POINT ( 'NONE',  ( 6.164708882046985750, 0.6044385376218417427, 1.814302210532907411 ) ) ;
#74525 = LINE ( 'NONE', #40971, #88585 ) ;
#74526 = CARTESIAN_POINT ( 'NONE',  ( 0.9185735243398345240, 1.726912363944958617, 0.7195956246372691156 ) ) ;
#74527 = CARTESIAN_POINT ( 'NONE',  ( 1.938685741270998797, -1.555697844595272716, 1.282991390469834458 ) ) ;
#74529 = CARTESIAN_POINT ( 'NONE',  ( -5.293380042321269130, 6.810232436340249329, 1.224475135354096800 ) ) ;
#74528 = CARTESIAN_POINT ( 'NONE',  ( 0.6823417656249899377, 0.5927083336747518416, 1.181850606188755259 ) ) ;
#74531 = CARTESIAN_POINT ( 'NONE',  ( 4.090527498900095260, -2.083119126933795418, -0.3091809127075405006 ) ) ;
#74530 = CARTESIAN_POINT ( 'NONE',  ( -8.015895134177625891, 10.37496362800581018, 1.599625672291295375 ) ) ;
#74532 = CARTESIAN_POINT ( 'NONE',  ( 6.286176778230493589, 10.48562334124426698, 0.7998128361456462443 ) ) ;
#74534 = CARTESIAN_POINT ( 'NONE',  ( -9.203287345578106127, 9.631590079462940324, 0.7998128361456462443 ) ) ;
#74533 = CARTESIAN_POINT ( 'NONE',  ( 5.747730777550676073, 5.670383760089384495, 0.000000000000000000 ) ) ;
#74535 = LINE ( 'NONE', #9525, #54734 ) ;
#74536 = CARTESIAN_POINT ( 'NONE',  ( 3.674085990935217261, 2.004049791156937044, -0.2512726544132165563 ) ) ;
#74537 = CARTESIAN_POINT ( 'NONE',  ( 1.364683531249992088, 5.384375000341417916, 1.214306433183764966E-14 ) ) ;
#74538 = AXIS2_PLACEMENT_3D ( 'NONE', #16819, #183600, #35207 ) ;
#74539 = CARTESIAN_POINT ( 'NONE',  ( 8.270110514656016321, 12.59228666716665401, 0.7216878364870438212 ) ) ;
#74540 = CARTESIAN_POINT ( 'NONE',  ( 4.938837616837212785, 0.3641351946921667082, 2.130543054529559832 ) ) ;
#74541 = CARTESIAN_POINT ( 'NONE',  ( 5.040599249230596435, 9.102725900736217568, 0.7998128361456341429 ) ) ;
#74542 = CARTESIAN_POINT ( 'NONE',  ( -1.364683531250014514, -0.6572916663252459379, 0.7879004041258379498 ) ) ;
#74544 = CARTESIAN_POINT ( 'NONE',  ( -9.495512617570035729, -9.134774474195801020, 0.2994571439533236235 ) ) ;
#74543 = CARTESIAN_POINT ( 'NONE',  ( 5.855142236255289845, 7.924361590421551860, -1.599625672291281386 ) ) ;
#74545 = CARTESIAN_POINT ( 'NONE',  ( 7.388830529323379359, 11.56412668427855195, -0.7216878364870267237 ) ) ;
#74547 = CARTESIAN_POINT ( 'NONE',  ( -0.2863826248021646981, -7.730039540835470291, 10.99644352130520097 ) ) ;
#74546 = CARTESIAN_POINT ( 'NONE',  ( 1.469425047783163407, 1.914459939344328010, 1.024175319008380658 ) ) ;
#74549 = CARTESIAN_POINT ( 'NONE',  ( 0.7140992756325339474, 1.701125707204936166, 0.7050099338341904165 ) ) ;
#74548 = CARTESIAN_POINT ( 'NONE',  ( -6.249945626219832739, 6.393950773452325542, 1.040834085586084257E-14 ) ) ;
#74550 = CARTESIAN_POINT ( 'NONE',  ( 1.364683531249988757, 1.384375000341421469, 0.000000000000000000 ) ) ;
#74551 = CARTESIAN_POINT ( 'NONE',  ( 2.929422067023911502, -1.473737196803912797, -1.622193633833472814 ) ) ;
#74552 = CARTESIAN_POINT ( 'NONE',  ( 3.450319916561462197, 2.262689076145682598, 0.002162386163321801912 ) ) ;
#74553 = CARTESIAN_POINT ( 'NONE',  ( -7.528855374290365887, 7.678086112960552434, -0.7998128361456291469 ) ) ;
#74554 = CARTESIAN_POINT ( 'NONE',  ( -1.364683531249997417, 4.571875000341417028, 1.214306433183764966E-14 ) ) ;
#74555 = CARTESIAN_POINT ( 'NONE',  ( 6.479309170914094196, 6.755949689298615723, 0.1985876171829506487 ) ) ;
#74556 = CARTESIAN_POINT ( 'NONE',  ( 1.499999999999997113, 12.89583333333333215, -0.8660254037844378194 ) ) ;
#74557 = CARTESIAN_POINT ( 'NONE',  ( 5.777182853198898904, 6.873039762554409293, -1.082531754730548412 ) ) ;
#74558 = CARTESIAN_POINT ( 'NONE',  ( 3.760817854529928894, -1.559684770762577388, -0.8363013385033011282 ) ) ;
#74559 =( BOUNDED_CURVE ( )  B_SPLINE_CURVE ( 2, ( #211560, #178024, #63195, #196401, #14423, #48046, #31778 ),
 .UNSPECIFIED., .F., .T. ) 
 B_SPLINE_CURVE_WITH_KNOTS ( ( 3, 2, 2, 3 ),
 ( 0.3035714285714285476, 0.3095238095238095899, 0.3154761904761906322, 0.3214285714285716744 ),
 .UNSPECIFIED. ) 
 CURVE ( )  GEOMETRIC_REPRESENTATION_ITEM ( )  RATIONAL_B_SPLINE_CURVE ( ( 1.000000000000000000, 0.8660254037844387076, 1.000000000000000000, 0.8660254037844387076, 1.000000000000000000, 0.8660254037844337116, 1.000000000000005107 ) ) 
 REPRESENTATION_ITEM ( '' )  );
#74560 = CARTESIAN_POINT ( 'NONE',  ( 7.527801604085637699, 9.805521176231838609, 1.599625672291281386 ) ) ;
#74561 = CARTESIAN_POINT ( 'NONE',  ( 1.255059265495124476, -1.660252808076821296, 1.295518548220045529 ) ) ;
#74564 = EDGE_CURVE ( 'NONE', #209385, #1117, #38323, .T. ) ;
#74563 = CARTESIAN_POINT ( 'NONE',  ( 0.7499999999999885647, 1.316666666666688190, -1.299038105676652899 ) ) ;
#74562 = CARTESIAN_POINT ( 'NONE',  ( 0.6823417656249969321, 11.27604166700806765, -1.181850606188757036 ) ) ;
#74565 = CARTESIAN_POINT ( 'NONE',  ( 1.416386825446398712, 0.7951318926605431825, 1.802096770617849897 ) ) ;
#74566 = CARTESIAN_POINT ( 'NONE',  ( -5.334207092333882017, 5.187939460669764635, 0.7998128361456281477 ) ) ;
#74567 = CARTESIAN_POINT ( 'NONE',  ( -0.4571195463272921256, 7.927888240403309084, -1.992899296338165982 ) ) ;
#74569 = VERTEX_POINT ( 'NONE', #202930 ) ;
#74568 = CARTESIAN_POINT ( 'NONE',  ( 5.150580392983738598, 1.786086171955153068, 0.3018458199737662495 ) ) ;
#74570 = CARTESIAN_POINT ( 'NONE',  ( 6.561783159334121152, 8.678499657355050800, -1.443375672974057666 ) ) ;
#74571 = CARTESIAN_POINT ( 'NONE',  ( 4.662891624058607576, -1.671085903211678270, -0.8408918736509605196 ) ) ;
#74572 = CARTESIAN_POINT ( 'NONE',  ( 4.452052287080165982, -0.7971045336818067817, 1.910850710330507907 ) ) ;
#74573 = CARTESIAN_POINT ( 'NONE',  ( 0.6124999999999914957, 1.416666666666690944, -1.060881119635986414 ) ) ;
#74574 = CARTESIAN_POINT ( 'NONE',  ( -5.600926855776888758, 7.627776979863398310, -1.443375672974066548 ) ) ;
#74575 = CARTESIAN_POINT ( 'NONE',  ( 7.781490099239519509, 11.16582331816642260, 1.199719254218460707 ) ) ;
#74576 = CARTESIAN_POINT ( 'NONE',  ( -8.319899820280397762, 12.85830022363583147, -0.7998128361456281477 ) ) ;
#74577 = CARTESIAN_POINT ( 'NONE',  ( 5.820193082016415609, 10.01225203898631655, 0.000000000000000000 ) ) ;
#74578 = EDGE_CURVE ( 'NONE', #199345, #7836, #31978, .T. ) ;
#74579 = DIRECTION ( 'NONE',  ( 0.000000000000000000, -1.000000000000000000, 0.000000000000000000 ) ) ;
#74580 = CARTESIAN_POINT ( 'NONE',  ( 1.364683531249988535, 5.217708333674750065, -0.7879004041258300672 ) ) ;
#74581 = CARTESIAN_POINT ( 'NONE',  ( -0.7500000000000215383, 0.4416666666666874130, 1.299038105676659116 ) ) ;
#74582 = CARTESIAN_POINT ( 'NONE',  ( 4.334394203492665909, -1.131343785558375226, 1.602600411086833931 ) ) ;
#74583 = CARTESIAN_POINT ( 'NONE',  ( 1.897814322125553010, 0.1948091626960517242, 2.006652841580962132 ) ) ;
#74584 = FACE_OUTER_BOUND ( 'NONE', #110491, .T. ) ;
#74585 = SURFACE_STYLE_USAGE ( .BOTH. , #159031 ) ;
#74586 = DIRECTION ( 'NONE',  ( 0.000000000000000000, 1.000000000000000000, 0.000000000000000000 ) ) ;
#74587 = CARTESIAN_POINT ( 'NONE',  ( 2.143623209005097507, 0.7202431893391960660, -1.726524797105493336 ) ) ;
#74588 = CARTESIAN_POINT ( 'NONE',  ( -1.001543065824772872E-14, 5.321875000341422357, 1.575800808251672791 ) ) ;
#74589 = CARTESIAN_POINT ( 'NONE',  ( 2.584242159373177028, 1.080601423880021894, 1.698455611904861495 ) ) ;
#74591 = CARTESIAN_POINT ( 'NONE',  ( 3.708711176059620751, 2.011172256762243649, 0.6619615953592747903 ) ) ;
#74590 = CARTESIAN_POINT ( 'NONE',  ( -5.829642864196175722, 7.824335979694092558, 1.443375672974064550 ) ) ;
#74592 = DIRECTION ( 'NONE',  ( -0.000000000000000000, -1.000000000000000000, -0.000000000000000000 ) ) ;
#74593 = CARTESIAN_POINT ( 'NONE',  ( 4.422371208857902580, 0.9731212702417373350, 1.827393648576709717 ) ) ;
#74594 = CARTESIAN_POINT ( 'NONE',  ( 5.936491157937257235, 8.019268665717216749, 1.599625672291268286 ) ) ;
#74596 = CARTESIAN_POINT ( 'NONE',  ( 6.720655732516649827, 0.5547967289194677409, 2.325046546815363602 ) ) ;
#74595 = CARTESIAN_POINT ( 'NONE',  ( 0.2926706434557576064, 1.735970642146159371, -1.164857044846574707 ) ) ;
#74598 = ORIENTED_EDGE ( 'NONE', *, *, #146528, .T. ) ;
#74597 = CARTESIAN_POINT ( 'NONE',  ( 5.280226139177822908, -1.012770463184736736, 1.518683248463777113 ) ) ;
#74599 = CARTESIAN_POINT ( 'NONE',  ( 6.889514614038635187, 11.18951748302043114, -0.7998128361456291469 ) ) ;
#74600 = CARTESIAN_POINT ( 'NONE',  ( 0.007338969819053441264, 14.55474275600908030, 11.95332390717406490 ) ) ;
#74601 =( LENGTH_UNIT ( ) NAMED_UNIT ( * ) SI_UNIT ( .MILLI., .METRE. ) );
#74602 = CARTESIAN_POINT ( 'NONE',  ( -11.66902918085182250, 4.335764935525111774, 5.185761432613135824 ) ) ;
#74603 = CARTESIAN_POINT ( 'NONE',  ( -1.364683531250000748, 11.42187500034139802, 0.000000000000000000 ) ) ;
#74604 = CARTESIAN_POINT ( 'NONE',  ( 6.076807558263135789, -1.348954070496380941, 1.355674883165632227 ) ) ;
#74605 = CARTESIAN_POINT ( 'NONE',  ( -8.025536864285518490, 11.45054454405341282, -1.199719254218446718 ) ) ;
#74606 = CARTESIAN_POINT ( 'NONE',  ( 7.169564303528210836, 7.258913197071374945, -0.7998128361456281477 ) ) ;
#74607 = CARTESIAN_POINT ( 'NONE',  ( -1.360316468750013108, 2.921875000341411788, -1.734723475976807094E-14 ) ) ;
#74608 = CARTESIAN_POINT ( 'NONE',  ( 3.999292125906911188, 4.728557570721922509, 1.082531754730560403 ) ) ;
#74609 = CARTESIAN_POINT ( 'NONE',  ( 4.521807925357579805, 5.234196320127330715, -1.199719254218452047 ) ) ;
#74610 = VERTEX_POINT ( 'NONE', #20973 ) ;
#74611 = CARTESIAN_POINT ( 'NONE',  ( -7.422162748838431412, 7.623887726591770608, -0.7998128361456362523 ) ) ;
#74612 = CARTESIAN_POINT ( 'NONE',  ( 5.255482535091188012, 1.942537579172060047, -0.5405093616211650298 ) ) ;
#74613 = DIRECTION ( 'NONE',  ( -0.000000000000000000, -1.000000000000000000, -0.000000000000000000 ) ) ;
#74614 = AXIS2_PLACEMENT_3D ( 'NONE', #113987, #11057, #46803 ) ;
#74615 = DIRECTION ( 'NONE',  ( 1.735552045436534953E-14, 0.6004703560067730095, -0.7996470168499969500 ) ) ;
#74616 = CARTESIAN_POINT ( 'NONE',  ( -0.1399997263889836974, 2.022132088033218533, -2.415689637818136948 ) ) ;
#74617 = CARTESIAN_POINT ( 'NONE',  ( -4.419594888374909658, 8.100018436505289188, 0.7216878364870458196 ) ) ;
#74618 = VECTOR ( 'NONE', #191708, 1000.000000000000000 ) ;
#74619 = CARTESIAN_POINT ( 'NONE',  ( 8.568389894156670294, 12.94027927658408217, -0.7216878364870257245 ) ) ;
#74620 = CARTESIAN_POINT ( 'NONE',  ( 2.096482953606861432, 1.947282536051987201, 0.2939031187191037398 ) ) ;
#74622 = CARTESIAN_POINT ( 'NONE',  ( 3.251577527157409886, 1.966640965408305686, -0.4445242805125593222 ) ) ;
#74621 = B_SPLINE_CURVE_WITH_KNOTS ( 'NONE', 3,
 ( #146844, #85000, #49326, #100189, #199804, #67649, #213910 ),
 .UNSPECIFIED., .F., .F.,
 ( 4, 3, 4 ),
 ( 0.0001932309589017193582, 0.0009000000022123051842, 0.002089081127711805118 ),
 .UNSPECIFIED. ) ;
#74623 = CARTESIAN_POINT ( 'NONE',  ( -6.157374318900681764, 10.33535380535947290, 0.7998128361456481317 ) ) ;
#74624 = CARTESIAN_POINT ( 'NONE',  ( 6.827182134110199030, 1.215541611938670608, 2.400477883804314150 ) ) ;
#74625 = CARTESIAN_POINT ( 'NONE',  ( 4.154361996720875361, -1.624486827992781990, 1.471056368041193219 ) ) ;
#74626 = PRESENTATION_STYLE_ASSIGNMENT (( #123473 ) ) ;
#74627 = CARTESIAN_POINT ( 'NONE',  ( 2.748949809783503451, -1.602600522849004339, 1.068665135549841771 ) ) ;
#74628 = CARTESIAN_POINT ( 'NONE',  ( -7.914208982075130905, 10.25632978388623684, -1.599625672291263179 ) ) ;
#74629 = LINE ( 'NONE', #140734, #131487 ) ;
#74630 = CARTESIAN_POINT ( 'NONE',  ( -7.817119696385909755, 14.48014712537941406, 9.115431373065430165 ) ) ;
#74631 = CARTESIAN_POINT ( 'NONE',  ( 5.847644326195776010, 5.716673223516856694, -0.7998128361456281477 ) ) ;
#74632 = CARTESIAN_POINT ( 'NONE',  ( 3.719872605471109761, 6.605953636083950364, -2.420000000000002149 ) ) ;
#74633 = CARTESIAN_POINT ( 'NONE',  ( 4.570507181582611267, 8.346359121906111511, 0.000000000000000000 ) ) ;
#74634 = EDGE_LOOP ( 'NONE', ( #167008, #5692, #20566, #70736 ) ) ;
#74636 = CARTESIAN_POINT ( 'NONE',  ( 3.211590615979207364, 1.588433223196554778, 1.236618793847492626 ) ) ;
#74635 = CARTESIAN_POINT ( 'NONE',  ( 6.093280168761200599, -0.6138376400152152357, 1.736067454429328416 ) ) ;
#74637 = CARTESIAN_POINT ( 'NONE',  ( 5.044420649243852139, 2.147057653193120252, -0.8206418397275447862 ) ) ;
#74639 = CARTESIAN_POINT ( 'NONE',  ( 3.309261503611124144, -1.518638105539332317, -1.075258281928012094 ) ) ;
#74638 = DIRECTION ( 'NONE',  ( -0.9486832980505139901, -0.3162277660168373861, 3.312310031615527941E-15 ) ) ;
#74640 = CARTESIAN_POINT ( 'NONE',  ( 3.285556943750000514, -1.013541666188710888, 1.896917185911906500 ) ) ;
#74641 = CARTESIAN_POINT ( 'NONE',  ( -1.403499169903600574, 7.376709478543776122, 4.304123474983186703 ) ) ;
#74642 = FACE_OUTER_BOUND ( 'NONE', #16517, .T. ) ;
#74643 = CARTESIAN_POINT ( 'NONE',  ( -8.179646747746328828, 8.437342715325849341, -0.7998128361456291469 ) ) ;
#74644 = EDGE_CURVE ( 'NONE', #71536, #110540, #38613, .T. ) ;
#74645 = CARTESIAN_POINT ( 'NONE',  ( -4.909461021924285795, 6.821066840368686712, 1.443375672974058777 ) ) ;
#74646 = CARTESIAN_POINT ( 'NONE',  ( 5.829650940335100451, 1.029561424092540589, -1.819573902328343484 ) ) ;
#74647 = CARTESIAN_POINT ( 'NONE',  ( 6.331294547901813452, 6.488857848747989543, 1.040834085586084257E-14 ) ) ;
#74648 = CARTESIAN_POINT ( 'NONE',  ( -1.426745631514137802, 7.396214564682365378, 4.272608017055013363 ) ) ;
#74650 = CARTESIAN_POINT ( 'NONE',  ( 5.366329872910639232, 5.155139694684188534, 1.040834085586084257E-14 ) ) ;
#74649 = DIRECTION ( 'NONE',  ( -0.6507913734559641616, -0.7592566023653004592, 0.000000000000000000 ) ) ;
#74651 = CARTESIAN_POINT ( 'NONE',  ( 5.795441377679017236, 1.310440327830458385, 1.121692192092491380 ) ) ;
#74652 = CARTESIAN_POINT ( 'NONE',  ( -6.261168011412601153, 6.199117522936475666, 1.040834085586084257E-14 ) ) ;
#74653 = CARTESIAN_POINT ( 'NONE',  ( 1.740413025836908156, 1.729532991921935325, -0.1275185469355680501 ) ) ;
#74654 = SURFACE_STYLE_USAGE ( .BOTH. , #89858 ) ;
#74655 = CARTESIAN_POINT ( 'NONE',  ( 0.000000000000000000, -0.02379966007286238305, 0.000000000000000000 ) ) ;
#74656 = SURFACE_SIDE_STYLE ('',( #108291 ) ) ;
#74657 = CARTESIAN_POINT ( 'NONE',  ( 6.174718801439761151, 1.464035886807094844, -1.603313688547292726 ) ) ;
#74658 = CARTESIAN_POINT ( 'NONE',  ( 4.846238042176662653, 1.821038859956089606, 0.1311717439725426648 ) ) ;
#74659 = CARTESIAN_POINT ( 'NONE',  ( 1.797631089865757259, -1.417250949620936895, -1.356651810197152086 ) ) ;
#74660 = PRESENTATION_STYLE_ASSIGNMENT (( #191585 ) ) ;
#74661 = CARTESIAN_POINT ( 'NONE',  ( 1.499999999999961586, 5.545833333333349380, -0.8660254037844482555 ) ) ;
#74662 = CARTESIAN_POINT ( 'NONE',  ( 9.237182729612253951, 9.671134694169463586, 0.7998128361456462443 ) ) ;
#74663 = CARTESIAN_POINT ( 'NONE',  ( 4.037823014030429647, -2.028772383530423884, 0.6168223452112443494 ) ) ;
#74664 = EDGE_CURVE ( 'NONE', #95488, #31644, #187340, .T. ) ;
#74665 = CARTESIAN_POINT ( 'NONE',  ( 0.000000000000000000, 4.000007913748540922, 1.105031132475055157E-32 ) ) ;
#74666 = COLOUR_RGB ( '', 0.40784314, 0.44705882, 0.49803922) ;
#74667 = CARTESIAN_POINT ( 'NONE',  ( -4.485938484121875902, 7.064193607440066636, -1.134896524841392473 ) ) ;
#74668 = CARTESIAN_POINT ( 'NONE',  ( 1.569279613544020568, 1.823957739939351619, 0.9794188589333228112 ) ) ;
#74670 = CARTESIAN_POINT ( 'NONE',  ( -0.7500000000000179856, 14.82291666734946567, 1.299038105676658228 ) ) ;
#74669 = CARTESIAN_POINT ( 'NONE',  ( -0.08000000000000714873, -5.907420853759267843, 10.91970695577494865 ) ) ;
#74672 = ORIENTED_EDGE ( 'NONE', *, *, #58676, .T. ) ;
#74671 = CARTESIAN_POINT ( 'NONE',  ( 3.774281487401151214, 2.204430612424528757, -0.2728622730414613784 ) ) ;
#74673 = CARTESIAN_POINT ( 'NONE',  ( 1.266696122786495904, 2.121433860451333420, -0.8855928530677835697 ) ) ;
#74675 = CARTESIAN_POINT ( 'NONE',  ( 6.754736851877535031, -0.5442653458712517489, -1.989433905422931748 ) ) ;
#74674 = CARTESIAN_POINT ( 'NONE',  ( 8.270110514656021650, 11.63191745286530576, 1.082531754730557072 ) ) ;
#74677 = CARTESIAN_POINT ( 'NONE',  ( -3.285556943750000070, -3.959374999522043304, 0.000000000000000000 ) ) ;
#74676 = CARTESIAN_POINT ( 'NONE',  ( 4.686278372178935392, 5.496354851410763409, 1.199719254218452047 ) ) ;
#74678 = CARTESIAN_POINT ( 'NONE',  ( 0.000000000000000000, 13.49999999999999822, 0.000000000000000000 ) ) ;
#74679 = CARTESIAN_POINT ( 'NONE',  ( 6.427308110136687347, -1.208249125052461181, -1.389453836245766016 ) ) ;
#74681 = SURFACE_SIDE_STYLE ('',( #8598 ) ) ;
#74680 = COLOUR_RGB ( '', 0.08235294, 0.09019608, 0.10196078) ;
#74682 = EDGE_CURVE ( 'NONE', #114917, #45649, #88144, .T. ) ;
#74683 = CARTESIAN_POINT ( 'NONE',  ( -0.1104750535120251204, 2.866086309876151539, -2.591737134608104842 ) ) ;
#74684 = CARTESIAN_POINT ( 'NONE',  ( 3.487030103973333794, 1.559624344477263502, -0.7367539641185815169 ) ) ;
#74685 = CARTESIAN_POINT ( 'NONE',  ( 1.833220611596135363, -1.622487599052296670, -1.197302888167578683 ) ) ;
#74686 = CARTESIAN_POINT ( 'NONE',  ( 3.411010488035473909, -1.370397956465055245, -1.845398096504316410 ) ) ;
#74687 = CARTESIAN_POINT ( 'NONE',  ( 3.321791363677785380, -2.181432725256218674, 0.5997193178089550436 ) ) ;
#74688 = CARTESIAN_POINT ( 'NONE',  ( 5.567048526788405560, -1.903460050192711028, -0.9016015758830184801 ) ) ;
#74689 = CARTESIAN_POINT ( 'NONE',  ( -7.119440060951841787, 7.478637290631501067, 0.000000000000000000 ) ) ;
#74690 = CARTESIAN_POINT ( 'NONE',  ( 3.813518172763687986, -1.743905005666521291, 0.3001630661942331080 ) ) ;
#74692 = CARTESIAN_POINT ( 'NONE',  ( 5.952705545545641463, -1.964087939335951827, -1.181845259310390306 ) ) ;
#74691 = CARTESIAN_POINT ( 'NONE',  ( 7.095713291905693332, 9.371694488680407886, 1.599625672291268286 ) ) ;
#74693 = CARTESIAN_POINT ( 'NONE',  ( 5.999929499617846496, -0.6670042279848520383, -1.716255146773135287 ) ) ;
#74694 = CARTESIAN_POINT ( 'NONE',  ( -3.327636637150278798, 5.969660945728899826, -1.199719254218452935 ) ) ;
#74695 = CARTESIAN_POINT ( 'NONE',  ( -1.201851678989727383E-14, 2.962500000000025224, 1.732050807568877637 ) ) ;
#74696 = CARTESIAN_POINT ( 'NONE',  ( 5.613277516225614328, -2.138688192980051639, 0.4772630486022874652 ) ) ;
#74697 = CARTESIAN_POINT ( 'NONE',  ( -3.704402285031864306, 5.344888637335695414, -1.599625672291256295 ) ) ;
#74698 = CARTESIAN_POINT ( 'NONE',  ( -3.492292736374302820, 15.44799614855975989, 11.44281500427524989 ) ) ;
#74699 = CARTESIAN_POINT ( 'NONE',  ( 5.459458695672200435, 1.690470114046587646, 1.195012289465044564 ) ) ;
#74700 = CARTESIAN_POINT ( 'NONE',  ( 0.6203277878081385754, 1.987498645412737908, 0.3399528957561820386 ) ) ;
#74701 = CARTESIAN_POINT ( 'NONE',  ( -1.001543065824772872E-14, 4.321875000341417916, 1.575800808251672791 ) ) ;
#74702 = CARTESIAN_POINT ( 'NONE',  ( 4.389231790275191614, 1.720148140252445668, -0.8676111672119514173 ) ) ;
#74703 = CARTESIAN_POINT ( 'NONE',  ( -1.402160292154681736E-14, 9.921875000341401574, 1.575800808251682339 ) ) ;
#74704 = FACE_OUTER_BOUND ( 'NONE', #31557, .T. ) ;
#74705 = CARTESIAN_POINT ( 'NONE',  ( 6.533471381225442798, -0.1521382079053348602, 2.086446650026114735 ) ) ;
#74707 = ORIENTED_EDGE ( 'NONE', *, *, #103236, .T. ) ;
#74706 = CARTESIAN_POINT ( 'NONE',  ( 4.255647627037052709E-16, 0.5000000000000004441, 3.475000000000000089 ) ) ;
#74709 = CARTESIAN_POINT ( 'NONE',  ( -7.884707905546937567, -7.003075417673640501, 7.228805602686603216 ) ) ;
#74708 = CARTESIAN_POINT ( 'NONE',  ( 1.500000000000039524, 6.999999999999999112, 10.89724735885167561 ) ) ;
#74710 = CARTESIAN_POINT ( 'NONE',  ( 3.999819011231439347, 4.625209253646830554, 1.199719254218464037 ) ) ;
#74711 = CARTESIAN_POINT ( 'NONE',  ( 4.706088717274896638, 7.544168365912456764, 1.082531754730548412 ) ) ;
#74712 = CARTESIAN_POINT ( 'NONE',  ( 3.913815762669449416, 7.330443837381343641, -0.8582294057540799104 ) ) ;
#74713 = DIRECTION ( 'NONE',  ( 1.000000000000000000, 0.000000000000000000, 0.000000000000000000 ) ) ;
#74714 = CARTESIAN_POINT ( 'NONE',  ( 10.66990370383054731, 11.55056853066490952, 0.7216878364870317197 ) ) ;
#74715 = CARTESIAN_POINT ( 'NONE',  ( 1.697631272820496307, -1.418720726069604865, -1.355276769646639901 ) ) ;
#74716 = CARTESIAN_POINT ( 'NONE',  ( -1.364683531250014514, 0.8010416670080889867, -0.7879004041258289570 ) ) ;
#74717 = CARTESIAN_POINT ( 'NONE',  ( 9.261794192842835116, -6.948429295162968700, 9.269928574751061333E-15 ) ) ;
#74718 = CARTESIAN_POINT ( 'NONE',  ( 5.195737816846159873, -1.386088135442983260, -1.388664821390848347 ) ) ;
#74719 = CARTESIAN_POINT ( 'NONE',  ( -7.160677686311960777, 11.50587440067263678, -0.7998128361456291469 ) ) ;
#74720 = CARTESIAN_POINT ( 'NONE',  ( -6.195713011320807873, 6.330679389403470303, -0.7216878364870267237 ) ) ;
#74721 = CARTESIAN_POINT ( 'NONE',  ( 0.2864612384333536932, -1.063250325806489149, 1.997138572869002537 ) ) ;
#74723 = EDGE_LOOP ( 'NONE', ( #175076, #84856, #20194, #93988 ) ) ;
#74722 = CARTESIAN_POINT ( 'NONE',  ( -0.4000000000000357714, 2.999999999999975131, -0.3423093779010444870 ) ) ;
#74724 = CARTESIAN_POINT ( 'NONE',  ( -1.364683531250010295, 5.530208333674751842, 0.7879004041258379498 ) ) ;
#74725 = CARTESIAN_POINT ( 'NONE',  ( 0.7373108528737730705, -1.318359053027039263, -1.327247110734230962 ) ) ;
#74726 = CARTESIAN_POINT ( 'NONE',  ( 5.852856049955673434, -0.7765510095132116541, 1.550312759826449671 ) ) ;
#74728 = CARTESIAN_POINT ( 'NONE',  ( 2.894263506066748093, -0.6386881658498286818, -2.096408367471907841 ) ) ;
#74727 = CARTESIAN_POINT ( 'NONE',  ( -1.360316468750044860, 1.411458333674720622, 0.7853790794158801436 ) ) ;
#74729 = CARTESIAN_POINT ( 'NONE',  ( 4.577368073103933455, 0.004851830007264032810, -2.307758714736147798 ) ) ;
#74730 = CARTESIAN_POINT ( 'NONE',  ( 0.4794588345870378632, 1.923154262159839201, -0.7412630403166396986 ) ) ;
#74731 = CARTESIAN_POINT ( 'NONE',  ( 2.115084705647510610, -1.883649903580833174, 0.4717843263111404783 ) ) ;
#74732 = CARTESIAN_POINT ( 'NONE',  ( -4.229780737339226881, 7.878568593630327577, 1.040834085586084257E-14 ) ) ;
#74733 = PRODUCT ( 'rubber for base', 'rubber for base', '', ( #85090 ) ) ;
#74734 = DIRECTION ( 'NONE',  ( -0.6507913734559640506, -0.7592566023653004592, 0.000000000000000000 ) ) ;
#74735 = CARTESIAN_POINT ( 'NONE',  ( 4.693665235656380830, 1.977662049654808740, -0.7657889336421249693 ) ) ;
#74736 = CARTESIAN_POINT ( 'NONE',  ( 0.6801582343749900117, 0.05729166700808169255, -1.178068619123848526 ) ) ;
#74737 = CARTESIAN_POINT ( 'NONE',  ( 3.428361437285933455, -1.528740797599713153, -1.314997250469025936 ) ) ;
#74738 = CARTESIAN_POINT ( 'NONE',  ( -5.273758565591545988, 6.215435083687305351, 1.082531754730546636 ) ) ;
#74739 = CARTESIAN_POINT ( 'NONE',  ( -5.433785704026946384, 9.561443431331920095, 0.000000000000000000 ) ) ;
#74741 =( BOUNDED_SURFACE ( )  B_SPLINE_SURFACE ( 1, 2, ( 
 ( #85360, #52861, #151442, #150376, #3013, #53935, #86432, #100541, #1946, #70151, #83210, #84290, #49659, #200156, #117928, #82147, #136262, #69083, #118994, #199079, #120071, #201220, #184973, #36598, #149293, #33404, #186047, #102685, #168743, #20346, #116850, #17134, #202282, #115782, #103759, #37682, #165541, #181771, #16063, #148239, #214241, #65871, #198030, #874, #122227, #189262, #104833, #137334, #89652, #203351, #153572, #173031, #107006, #57132, #5142, #55003, #157849, #75514, #38752, #74453, #21398, #121154, #191377, #108083, #140557, #125411, #24613, #174112, #170878, #188187, #39822, #90722, #73365, #8370, #87508, #139470, #23543, #187119, #156784, #206571, #25684, #205499, #124356, #123299, #88581, #40901, #43043, #6220, #154639, #22470, #207635, #58198, #190314, #41972, #72289, #138397, #204415, #56071, #169808, #59253, #105930, #171954, #91793, #9443, #155706, #71217, #7287, #141625, #61399, #128624, #44100, #76572, #28905, #142684, #92856, #112352, #46235, #210835, #158902, #208694, #97125, #14762, #192445, #13700, #175168, #60321, #130737, #47308, #79774, #64596, #178365, #113422, #110220, #127562, #193530, #29973, #12631, #162111, #26755, #78702, #177291, #126481, #96058, #145886, #179428, #144828, #63534, #62462, #27830, #194591, #196730, #159967, #109156, #10499, #111285, #211897, #176227, #93926, #129689, #94990, #195672, #31049, #163177, #11572, #80852, #146943, #212958, #77642, #143764, #209758, #45173, #161036, #2757, #184716, #66680, #131774, #149037, #183668, #69887, #48370, #17944, #19020, #198831, #115535, #67747, #36340, #3816, #1693, #200955, #151185, #86173, #167428, #199904, #85100, #133897, #182591, #117674, #152243, #118732, #132827, #34214, #102418, #181530, #50476, #81905, #100287, #150120, #114483, #168486, #116597, #68826, #165288, #136000, #612, #134948, #166354, #197777, #15820, #84031, #147993, #32099, #51550, #35271, #101349, #98184, #214003, #20085, #180480, #49415, #52603, #164232, #65624, #33158, #99239, #16882, #82963, #139203, #140297, #137068, #5956, #154379 ),
 ( #121958, #72027, #24348, #74203, #186862, #156524, #203093, #105656, #55804, #202013, #187925, #138139, #54738, #204148, #107830, #120888, #38492, #39555, #171684, #21136, #104570, #23281, #206316, #90458, #91537, #89393, #119804, #57940, #155441, #103493, #4879, #87239, #7026, #169554, #73102, #25431, #123050, #170615, #22202, #205233, #56874, #53672, #173855, #153304, #189001, #88315, #40644, #106747, #172774, #8115, #124105, #190068, #41720, #157596, #9191, #75262, #185783, #37417, #70958, #44920, #144574, #42789, #10249, #45984, #111028, #177033, #94737, #160783, #174921, #12376, #192190, #175979, #29724, #26501, #63277, #76325, #142431, #77389, #109968, #195422, #194343, #13452, #28650, #126229, #128375, #30796, #210588, #208439, #62218, #141376, #92608, #158651, #145646, #60073, #143505, #209502, #78456, #43854, #108898, #61142, #27572, #125164, #112105, #178108, #95806, #191123, #93670, #129439, #47052, #159713, #161862, #207387, #11311, #162925, #79528, #211642, #96875, #113168, #179172, #127304, #193275, #14506, #59008, #198581, #136553, #212709, #53154, #148793, #180235, #86718, #152787, #87789, #119283, #37974, #185269, #213757, #36892, #105126, #131526, #171166, #196483, #82716, #102974, #80597, #146693, #4367, #363, #54226, #169032, #120364, #130496, #186339, #20629, #70437, #170093, #202574, #39041, #81654, #181282, #104047, #5432, #98986, #163992, #32908, #21679, #64350, #48125, #153863, #71511, #16632, #147741, #137623, #203640, #114237, #55291, #121441, #187410, #31859, #97934, #15567, #65380, #197529, #66436, #49174, #115291, #165039, #132578, #8660, #159181, #89943, #107301, #56356, #74739, #124644, #88873, #93144, #24903, #125703, #139765, #60613, #189546, #191662, #41194, #155994, #40112, #126772, #42259, #75802, #206856, #205791, #23836, #57421, #122519, #110506, #192730, #106223, #188482, #207922, #141910, #123583, #22755, #154927, #190601, #173325, #140844, #6512, #142976, #204706, #25973, #91009, #58488, #157071, #108372, #73666, #174395, #10782, #92079, #158136, #9727, #59543, #43326 ) ),
 .UNSPECIFIED., .F., .F., .F. ) 
 B_SPLINE_SURFACE_WITH_KNOTS ( ( 2, 2 ),
 ( 3, 2, 2, 2, 2, 2, 2, 2, 2, 2, 2, 2, 2, 2, 2, 2, 2, 2, 2, 2, 2, 2, 2, 2, 2, 2, 2, 2, 2, 2, 2, 2, 2, 2, 2, 2, 2, 2, 2, 2, 2, 2, 2, 2, 2, 2, 2, 2, 2, 2, 2, 2, 2, 2, 2, 2, 2, 2, 2, 2, 2, 2, 2, 2, 2, 2, 2, 2, 2, 2, 2, 2, 2, 2, 2, 2, 2, 2, 2, 2, 2, 2, 2, 2, 2, 2, 2, 2, 2, 2, 2, 2, 2, 2, 2, 2, 2, 2, 2, 2, 2, 2, 2, 2, 2, 2, 2, 2, 2, 2, 2, 2, 2, 2, 2, 2, 2, 2, 2, 2, 3 ),
 ( 0.000000000000000000, 1.000000000000000000 ),
 ( 0.000000000000000000, 0.008333333333333333218, 0.01666666666666666644, 0.02500000000000000139, 0.03333333333333333287, 0.04166666666666666435, 0.05000000000000000278, 0.05833333333333333426, 0.06666666666666666574, 0.07499999999999999722, 0.08333333333333332871, 0.09166666666666666019, 0.1000000000000000056, 0.1083333333333333370, 0.1166666666666666685, 0.1250000000000000000, 0.1333333333333333315, 0.1416666666666666630, 0.1499999999999999944, 0.1583333333333333259, 0.1666666666666666574, 0.1749999999999999889, 0.1833333333333333204, 0.1916666666666666796, 0.2000000000000000111, 0.2083333333333333426, 0.2166666666666666741, 0.2250000000000000056, 0.2333333333333333370, 0.2416666666666666685, 0.2500000000000000000, 0.2583333333333333592, 0.2666666666666666630, 0.2750000000000000222, 0.2833333333333333259, 0.2916666666666666852, 0.2999999999999999889, 0.3083333333333333481, 0.3166666666666666519, 0.3250000000000000111, 0.3333333333333333148, 0.3416666666666666741, 0.3499999999999999778, 0.3583333333333333370, 0.3666666666666666408, 0.3750000000000000000, 0.3833333333333333592, 0.3916666666666666630, 0.4000000000000000222, 0.4083333333333333259, 0.4166666666666666852, 0.4249999999999999889, 0.4333333333333333481, 0.4416666666666666519, 0.4500000000000000111, 0.4583333333333333148, 0.4666666666666666741, 0.4749999999999999778, 0.4833333333333333370, 0.4916666666666666408, 0.5000000000000000000, 0.5083333333333333037, 0.5166666666666667185, 0.5250000000000000222, 0.5333333333333333259, 0.5416666666666666297, 0.5500000000000000444, 0.5583333333333333481, 0.5666666666666666519, 0.5749999999999999556, 0.5833333333333333703, 0.5916666666666666741, 0.5999999999999999778, 0.6083333333333332815, 0.6166666666666666963, 0.6250000000000000000, 0.6333333333333333037, 0.6416666666666667185, 0.6500000000000000222, 0.6583333333333333259, 0.6666666666666666297, 0.6750000000000000444, 0.6833333333333333481, 0.6916666666666666519, 0.6999999999999999556, 0.7083333333333333703, 0.7166666666666666741, 0.7249999999999999778, 0.7333333333333332815, 0.7416666666666666963, 0.7500000000000000000, 0.7583333333333333037, 0.7666666666666667185, 0.7750000000000000222, 0.7833333333333333259, 0.7916666666666666297, 0.8000000000000000444, 0.8083333333333333481, 0.8166666666666666519, 0.8249999999999999556, 0.8333333333333333703, 0.8416666666666666741, 0.8499999999999999778, 0.8583333333333332815, 0.8666666666666666963, 0.8750000000000000000, 0.8833333333333333037, 0.8916666666666667185, 0.9000000000000000222, 0.9083333333333333259, 0.9166666666666666297, 0.9250000000000000444, 0.9333333333333333481, 0.9416666666666666519, 0.9499999999999999556, 0.9583333333333333703, 0.9666666666666666741, 0.9749999999999999778, 0.9833333333333332815, 0.9916666666666666963, 1.000000000000000000 ),
 .UNSPECIFIED. ) 
 GEOMETRIC_REPRESENTATION_ITEM ( )  RATIONAL_B_SPLINE_SURFACE ( (
 ( 1.000000000000000000, 0.8660254037844387076, 1.000000000000000000, 0.8660254037844387076, 1.000000000000000000, 0.8660254037844387076, 1.000000000000000000, 0.8660254037844387076, 1.000000000000000000, 0.8660254037844387076, 1.000000000000000000, 0.8660254037844387076, 1.000000000000000000, 0.8660254037844387076, 1.000000000000000000, 0.8660254037844387076, 1.000000000000000000, 0.8660254037844387076, 1.000000000000000000, 0.8660254037844387076, 1.000000000000000000, 0.8660254037844387076, 1.000000000000000000, 0.8660254037844387076, 1.000000000000000000, 0.8660254037844387076, 1.000000000000000000, 0.8660254037844387076, 1.000000000000000000, 0.8660254037844387076, 1.000000000000000000, 0.8660254037844387076, 1.000000000000000000, 0.8660254037844387076, 1.000000000000000000, 0.8660254037844387076, 1.000000000000000000, 0.8660254037844387076, 1.000000000000000000, 0.8660254037844387076, 1.000000000000000000, 0.8660254037844387076, 1.000000000000000000, 0.8660254037844387076, 1.000000000000000000, 0.8660254037844387076, 1.000000000000000000, 0.8660254037844387076, 1.000000000000000000, 0.8660254037844387076, 1.000000000000000000, 0.8660254037844387076, 1.000000000000000000, 0.8660254037844387076, 1.000000000000000000, 0.8660254037844387076, 1.000000000000000000, 0.8660254037844387076, 1.000000000000000000, 0.8660254037844387076, 1.000000000000000000, 0.8660254037844387076, 1.000000000000000000, 0.8660254037844387076, 1.000000000000000000, 0.8660254037844387076, 1.000000000000000000, 0.8660254037844387076, 1.000000000000000000, 0.8660254037844387076, 1.000000000000000000, 0.8660254037844387076, 1.000000000000000000, 0.8660254037844387076, 1.000000000000000000, 0.8660254037844387076, 1.000000000000000000, 0.8660254037844387076, 1.000000000000000000, 0.8660254037844387076, 1.000000000000000000, 0.8660254037844387076, 1.000000000000000000, 0.8660254037844387076, 1.000000000000000000, 0.8660254037844387076, 1.000000000000000000, 0.8660254037844387076, 1.000000000000000000, 0.8660254037844387076, 1.000000000000000000, 0.8660254037844387076, 1.000000000000000000, 0.8660254037844387076, 1.000000000000000000, 0.8660254037844387076, 1.000000000000000000, 0.8660254037844387076, 1.000000000000000000, 0.8660254037844387076, 1.000000000000000000, 0.8660254037844387076, 1.000000000000000000, 0.8660254037844387076, 1.000000000000000000, 0.8660254037844387076, 1.000000000000000000, 0.8660254037844387076, 1.000000000000000000, 0.8660254037844387076, 1.000000000000000000, 0.8660254037844387076, 1.000000000000000000, 0.8660254037844387076, 1.000000000000000000, 0.8660254037844387076, 1.000000000000000000, 0.8660254037844387076, 1.000000000000000000, 0.8660254037844387076, 1.000000000000000000, 0.8660254037844387076, 1.000000000000000000, 0.8660254037844387076, 1.000000000000000000, 0.8660254037844387076, 1.000000000000000000, 0.8660254037844387076, 1.000000000000000000, 0.8660254037844387076, 1.000000000000000000, 0.8660254037844387076, 1.000000000000000000, 0.8660254037844387076, 1.000000000000000000, 0.8660254037844387076, 1.000000000000000000, 0.8660254037844387076, 1.000000000000000000, 0.8660254037844387076, 1.000000000000000000, 0.8660254037844387076, 1.000000000000000000, 0.8660254037844387076, 1.000000000000000000, 0.8660254037844387076, 1.000000000000000000, 0.8660254037844387076, 1.000000000000000000, 0.8660254037844387076, 1.000000000000000000, 0.8660254037844387076, 1.000000000000000000, 0.8660254037844387076, 1.000000000000000000, 0.8660254037844387076, 1.000000000000000000, 0.8660254037844387076, 1.000000000000000000, 0.8660254037844387076, 1.000000000000000000, 0.8660254037844387076, 1.000000000000000000, 0.8660254037844387076, 1.000000000000000000, 0.8660254037844387076, 1.000000000000000000, 0.8660254037844387076, 1.000000000000000000, 0.8660254037844387076, 1.000000000000000000, 0.8660254037844387076, 1.000000000000000000, 0.8660254037844387076, 1.000000000000000000, 0.8660254037844387076, 1.000000000000000000, 0.8660254037844387076, 1.000000000000000000, 0.8660254037844387076, 1.000000000000000000, 0.8660254037844387076, 1.000000000000000000, 0.8660254037844387076, 1.000000000000000000, 0.8660254037844387076, 1.000000000000000000, 0.8660254037844387076, 1.000000000000000000, 0.8660254037844387076, 1.000000000000000000, 0.8660254037844387076, 1.000000000000000000, 0.8660254037844387076, 1.000000000000000000, 0.8660254037844387076, 1.000000000000000000, 0.8660254037844387076, 1.000000000000000000, 0.8660254037844387076, 1.000000000000000000, 0.8660254037844387076, 1.000000000000000000, 0.8660254037844387076, 1.000000000000000000, 0.8660254037844387076, 1.000000000000000000, 0.8660254037844387076, 1.000000000000000000, 0.8660254037844387076, 1.000000000000000000, 0.8660254037844387076, 1.000000000000000000, 0.8660254037844387076, 1.000000000000000000, 0.8660254037844387076, 1.000000000000000000, 0.8660254037844387076, 1.000000000000000000, 0.8660254037844387076, 1.000000000000000000, 0.8660254037844387076, 1.000000000000000000, 0.8660254037844387076, 1.000000000000000000, 0.8660254037844387076, 1.000000000000000000, 0.8660254037844387076, 1.000000000000000000, 0.8660254037844387076, 1.000000000000000000, 0.8660254037844387076, 1.000000000000000000, 0.8660254037844387076, 1.000000000000000000, 0.8660254037844387076, 1.000000000000000000, 0.8660254037844387076, 1.000000000000000000, 0.8660254037844387076, 1.000000000000000000),
 ( 1.000000000000000000, 0.8660254037844387076, 1.000000000000000000, 0.8660254037844387076, 1.000000000000000000, 0.8660254037844387076, 1.000000000000000000, 0.8660254037844387076, 1.000000000000000000, 0.8660254037844387076, 1.000000000000000000, 0.8660254037844387076, 1.000000000000000000, 0.8660254037844387076, 1.000000000000000000, 0.8660254037844387076, 1.000000000000000000, 0.8660254037844387076, 1.000000000000000000, 0.8660254037844387076, 1.000000000000000000, 0.8660254037844387076, 1.000000000000000000, 0.8660254037844387076, 1.000000000000000000, 0.8660254037844387076, 1.000000000000000000, 0.8660254037844387076, 1.000000000000000000, 0.8660254037844387076, 1.000000000000000000, 0.8660254037844387076, 1.000000000000000000, 0.8660254037844387076, 1.000000000000000000, 0.8660254037844387076, 1.000000000000000000, 0.8660254037844387076, 1.000000000000000000, 0.8660254037844387076, 1.000000000000000000, 0.8660254037844387076, 1.000000000000000000, 0.8660254037844387076, 1.000000000000000000, 0.8660254037844387076, 1.000000000000000000, 0.8660254037844387076, 1.000000000000000000, 0.8660254037844387076, 1.000000000000000000, 0.8660254037844387076, 1.000000000000000000, 0.8660254037844387076, 1.000000000000000000, 0.8660254037844387076, 1.000000000000000000, 0.8660254037844387076, 1.000000000000000000, 0.8660254037844387076, 1.000000000000000000, 0.8660254037844387076, 1.000000000000000000, 0.8660254037844387076, 1.000000000000000000, 0.8660254037844387076, 1.000000000000000000, 0.8660254037844387076, 1.000000000000000000, 0.8660254037844387076, 1.000000000000000000, 0.8660254037844387076, 1.000000000000000000, 0.8660254037844387076, 1.000000000000000000, 0.8660254037844387076, 1.000000000000000000, 0.8660254037844387076, 1.000000000000000000, 0.8660254037844387076, 1.000000000000000000, 0.8660254037844387076, 1.000000000000000000, 0.8660254037844387076, 1.000000000000000000, 0.8660254037844387076, 1.000000000000000000, 0.8660254037844387076, 1.000000000000000000, 0.8660254037844387076, 1.000000000000000000, 0.8660254037844387076, 1.000000000000000000, 0.8660254037844387076, 1.000000000000000000, 0.8660254037844387076, 1.000000000000000000, 0.8660254037844387076, 1.000000000000000000, 0.8660254037844387076, 1.000000000000000000, 0.8660254037844387076, 1.000000000000000000, 0.8660254037844387076, 1.000000000000000000, 0.8660254037844387076, 1.000000000000000000, 0.8660254037844387076, 1.000000000000000000, 0.8660254037844387076, 1.000000000000000000, 0.8660254037844387076, 1.000000000000000000, 0.8660254037844387076, 1.000000000000000000, 0.8660254037844387076, 1.000000000000000000, 0.8660254037844387076, 1.000000000000000000, 0.8660254037844387076, 1.000000000000000000, 0.8660254037844387076, 1.000000000000000000, 0.8660254037844387076, 1.000000000000000000, 0.8660254037844387076, 1.000000000000000000, 0.8660254037844387076, 1.000000000000000000, 0.8660254037844387076, 1.000000000000000000, 0.8660254037844387076, 1.000000000000000000, 0.8660254037844387076, 1.000000000000000000, 0.8660254037844387076, 1.000000000000000000, 0.8660254037844387076, 1.000000000000000000, 0.8660254037844387076, 1.000000000000000000, 0.8660254037844387076, 1.000000000000000000, 0.8660254037844387076, 1.000000000000000000, 0.8660254037844387076, 1.000000000000000000, 0.8660254037844387076, 1.000000000000000000, 0.8660254037844387076, 1.000000000000000000, 0.8660254037844387076, 1.000000000000000000, 0.8660254037844387076, 1.000000000000000000, 0.8660254037844387076, 1.000000000000000000, 0.8660254037844387076, 1.000000000000000000, 0.8660254037844387076, 1.000000000000000000, 0.8660254037844387076, 1.000000000000000000, 0.8660254037844387076, 1.000000000000000000, 0.8660254037844387076, 1.000000000000000000, 0.8660254037844387076, 1.000000000000000000, 0.8660254037844387076, 1.000000000000000000, 0.8660254037844387076, 1.000000000000000000, 0.8660254037844387076, 1.000000000000000000, 0.8660254037844387076, 1.000000000000000000, 0.8660254037844387076, 1.000000000000000000, 0.8660254037844387076, 1.000000000000000000, 0.8660254037844387076, 1.000000000000000000, 0.8660254037844387076, 1.000000000000000000, 0.8660254037844387076, 1.000000000000000000, 0.8660254037844387076, 1.000000000000000000, 0.8660254037844387076, 1.000000000000000000, 0.8660254037844387076, 1.000000000000000000, 0.8660254037844387076, 1.000000000000000000, 0.8660254037844387076, 1.000000000000000000, 0.8660254037844387076, 1.000000000000000000, 0.8660254037844387076, 1.000000000000000000, 0.8660254037844387076, 1.000000000000000000, 0.8660254037844387076, 1.000000000000000000, 0.8660254037844387076, 1.000000000000000000, 0.8660254037844387076, 1.000000000000000000, 0.8660254037844387076, 1.000000000000000000, 0.8660254037844387076, 1.000000000000000000, 0.8660254037844387076, 1.000000000000000000, 0.8660254037844387076, 1.000000000000000000, 0.8660254037844387076, 1.000000000000000000, 0.8660254037844387076, 1.000000000000000000, 0.8660254037844387076, 1.000000000000000000, 0.8660254037844387076, 1.000000000000000000, 0.8660254037844387076, 1.000000000000000000, 0.8660254037844387076, 1.000000000000000000, 0.8660254037844387076, 1.000000000000000000, 0.8660254037844387076, 1.000000000000000000, 0.8660254037844387076, 1.000000000000000000, 0.8660254037844387076, 1.000000000000000000, 0.8660254037844387076, 1.000000000000000000, 0.8660254037844387076, 1.000000000000000000) ) ) 
 REPRESENTATION_ITEM ( '' )  SURFACE ( )  );
#74740 = CARTESIAN_POINT ( 'NONE',  ( 10.73535870392234237, 11.41900666419791399, 0.000000000000000000 ) ) ;
#74742 = CARTESIAN_POINT ( 'NONE',  ( 1.084280211047653264, -1.780658692889337091, -0.4022698149812459212 ) ) ;
#74743 = CARTESIAN_POINT ( 'NONE',  ( -4.762657100150483380, 8.778460060142702304, 0.000000000000000000 ) ) ;
#74745 = AXIS2_PLACEMENT_3D ( 'NONE', #212815, #130597, #30906 ) ;
#74744 = CARTESIAN_POINT ( 'NONE',  ( 5.829642864196179275, 5.903597551091400497, 0.7216878364870262796 ) ) ;
#74746 = DIRECTION ( 'NONE',  ( 0.000000000000000000, 0.000000000000000000, -1.000000000000000000 ) ) ;
#74747 = EDGE_LOOP ( 'NONE', ( #65021, #196594, #12735, #212142 ) ) ;
#74748 = CARTESIAN_POINT ( 'NONE',  ( 6.104382415481349966, -0.7394567487006579176, -1.923849829731038019 ) ) ;
#74749 = CARTESIAN_POINT ( 'NONE',  ( -5.275531169048895741, 9.168887107283438809, -0.7216878364870338292 ) ) ;
#74750 = UNCERTAINTY_MEASURE_WITH_UNIT (LENGTH_MEASURE( 1.000000000000000082E-05 ), #117905, 'distance_accuracy_value', 'NONE');
#74751 = CARTESIAN_POINT ( 'NONE',  ( 6.495764994278795612, 9.632124022417032805, 1.082531754730549078 ) ) ;
#74752 = CARTESIAN_POINT ( 'NONE',  ( -4.334856428067329404, 6.080418470877079429, -1.599625672291256295 ) ) ;
#74753 = CARTESIAN_POINT ( 'NONE',  ( -4.085803189671902480, 5.860132702740892263, -1.599625672291271394 ) ) ;
#74754 = CARTESIAN_POINT ( 'NONE',  ( 4.670572394037289854, 0.7749771354828223213, 1.865277368486473630 ) ) ;
#74755 = CARTESIAN_POINT ( 'NONE',  ( 6.094412736144367848, -1.190704872505081946, 1.875028197947399278 ) ) ;
#74757 = CARTESIAN_POINT ( 'NONE',  ( 8.541273586929342798, 11.94827437051752206, -1.082531754730543083 ) ) ;
#74756 = CARTESIAN_POINT ( 'NONE',  ( -2.979759899953417612, 6.698413326579433225, 0.7998128361456352531 ) ) ;
#74758 = CARTESIAN_POINT ( 'NONE',  ( 5.686755365928134687, 8.721966129303114101, 1.199719254218462483 ) ) ;
#74759 = CARTESIAN_POINT ( 'NONE',  ( 4.381749043697905854, 1.344797980244310631, 1.561758987969330992 ) ) ;
#74760 = CARTESIAN_POINT ( 'NONE',  ( 4.131482539099665452, 0.5404898895830790861, 1.942541833525657680 ) ) ;
#74761 = ORIENTED_EDGE ( 'NONE', *, *, #163416, .F. ) ;
#74762 = CARTESIAN_POINT ( 'NONE',  ( 0.000000000000000000, 4.518459255872631530, 0.000000000000000000 ) ) ;
#74763 = CARTESIAN_POINT ( 'NONE',  ( 3.005103603723342953, 6.657704637652544832, -0.7998128361456291469 ) ) ;
#74765 = ORIENTED_EDGE ( 'NONE', *, *, #3537, .T. ) ;
#74764 = CARTESIAN_POINT ( 'NONE',  ( -7.065734331377342414, 8.272386803808890576, -1.199719254218452047 ) ) ;
#74766 = CARTESIAN_POINT ( 'NONE',  ( 5.599868899865946936, 7.382462344760764239, -1.240035354157904779 ) ) ;
#74767 = CARTESIAN_POINT ( 'NONE',  ( 4.429064430395744267, 0.9478954142983322395, 1.779353956671766657 ) ) ;
#74768 = CARTESIAN_POINT ( 'NONE',  ( 2.642321604431462578, -1.530645349967133972, 1.022873098850234141 ) ) ;
#74769 = CARTESIAN_POINT ( 'NONE',  ( 1.225685606067970612, -0.05223309053147862785, 2.307267396272806970 ) ) ;
#74770 = CARTESIAN_POINT ( 'NONE',  ( 3.736153849017632922, 6.516540702899320081, -1.199719254218453823 ) ) ;
#74771 = ADVANCED_FACE ( 'NONE', ( #171518 ), #122880, .T. ) ;
#74772 = CARTESIAN_POINT ( 'NONE',  ( 3.725982817344280829, -1.284327275973631277, -1.738548686538298416 ) ) ;
#74773 = CARTESIAN_POINT ( 'NONE',  ( -4.577849422908604637, 8.492574760035358494, -0.7998128361456281477 ) ) ;
#74774 = CARTESIAN_POINT ( 'NONE',  ( 3.515276618313140311, 2.298542322452525877, 0.003563541299675049897 ) ) ;
#74775 = EDGE_CURVE ( 'NONE', #85578, #79740, #14466, .T. ) ;
#74776 = ORIENTED_EDGE ( 'NONE', *, *, #168724, .F. ) ;
#74777 =( GEOMETRIC_REPRESENTATION_CONTEXT ( 3 ) GLOBAL_UNCERTAINTY_ASSIGNED_CONTEXT ( ( #154936 ) ) GLOBAL_UNIT_ASSIGNED_CONTEXT ( ( #44739, #62044, #147561 ) ) REPRESENTATION_CONTEXT ( 'NONE', 'WORKASPACE' ) );
#74778 = CARTESIAN_POINT ( 'NONE',  ( 3.486133158594716510E-16, 2.312499999999992006, 1.224999999999971889 ) ) ;
#74779 = CARTESIAN_POINT ( 'NONE',  ( 2.904993682805886213, 1.579364189935757778, 1.002181356900035070 ) ) ;
#74780 = CARTESIAN_POINT ( 'NONE',  ( 6.121945800013044447, -1.094813031782817303, -1.639340605029938835 ) ) ;
#74781 = MECHANICAL_DESIGN_GEOMETRIC_PRESENTATION_REPRESENTATION (  '', ( #154403 ), #102443 ) ;
#74783 = CARTESIAN_POINT ( 'NONE',  ( 7.741342523278686549, 11.97539067722642869, 0.7216878364870438212 ) ) ;
#74782 = CARTESIAN_POINT ( 'NONE',  ( -0.6823417656250212460, 4.301041667008085767, 1.181850606188767472 ) ) ;
#74785 = CARTESIAN_POINT ( 'NONE',  ( 0.5400322017136415242, -1.563516176313231920, -1.557742479837947558 ) ) ;
#74784 = CARTESIAN_POINT ( 'NONE',  ( -6.911959384868566758, 6.958374125301778790, 1.040834085586084257E-14 ) ) ;
#74786 = CARTESIAN_POINT ( 'NONE',  ( 2.943528747942701695, 6.448217615992859919, 0.000000000000000000 ) ) ;
#74787 = CARTESIAN_POINT ( 'NONE',  ( 5.681030059326015014, 6.586622143090519188, -1.199719254218445830 ) ) ;
#74788 = CARTESIAN_POINT ( 'NONE',  ( -4.900382456335551140, 7.804531068111707270, 1.199719254218464037 ) ) ;
#74789 = CARTESIAN_POINT ( 'NONE',  ( -1.734723475976807094E-15, -8.407420853759283830, -10.91970695577494332 ) ) ;
#74790 = CARTESIAN_POINT ( 'NONE',  ( 5.700065208342940615, -1.971640594297157989, -0.0006100080248323812597 ) ) ;
#74791 = CARTESIAN_POINT ( 'NONE',  ( 5.742881039954627731, 0.4445991233769739925, 2.264314392639497520 ) ) ;
#74793 = EDGE_CURVE ( 'NONE', #126491, #88615, #206722, .T. ) ;
#74792 = CARTESIAN_POINT ( 'NONE',  ( 5.687920738472253213, -1.181023890769626217, -1.438316992653262627 ) ) ;
#74794 = CARTESIAN_POINT ( 'NONE',  ( 2.922777048086916629, -1.425580663919909563, 1.490811266603887963 ) ) ;
#74795 = CARTESIAN_POINT ( 'NONE',  ( 5.165293337126522388, 8.969999960048859577, 1.040834085586084257E-14 ) ) ;
#74796 = CARTESIAN_POINT ( 'NONE',  ( 6.668631453075247073, 8.873432343378178544, -1.599625672291281386 ) ) ;
#74797 = CARTESIAN_POINT ( 'NONE',  ( 7.578644679914718019, 7.944099669429731669, 0.7216878364870317197 ) ) ;
#74798 = CARTESIAN_POINT ( 'NONE',  ( -0.6823417656250003738, 2.780208333674753618, -1.181850606188749264 ) ) ;
#74799 = CARTESIAN_POINT ( 'NONE',  ( -5.919011879825667677, 14.55276648670623807, 10.39766294871059316 ) ) ;
#74800 = CARTESIAN_POINT ( 'NONE',  ( 6.005898860729467437, 7.069598761348265370, -1.082531754730543083 ) ) ;
#74801 = CARTESIAN_POINT ( 'NONE',  ( 5.213404077426219807, -1.831445439253748031, -1.165863444158367290 ) ) ;
#74803 = CARTESIAN_POINT ( 'NONE',  ( 3.790429961727882713, 1.553415782126759792, -0.9881970032953185656 ) ) ;
#74802 = CARTESIAN_POINT ( 'NONE',  ( -3.687454593236990430, 4.364747115940301292, 1.082531754730560403 ) ) ;
#74805 = FACE_OUTER_BOUND ( 'NONE', #186012, .T. ) ;
#74804 = CARTESIAN_POINT ( 'NONE',  ( -1.734723475976807094E-15, 2.999999999999988898, -6.938893903907228378E-15 ) ) ;
#74806 = CARTESIAN_POINT ( 'NONE',  ( 6.427279137517246888, -1.429865906218323435, -1.660902671979214595 ) ) ;
#74807 = CARTESIAN_POINT ( 'NONE',  ( 0.4396062811529514169, 3.163270344466244666, 1.951136887981155033 ) ) ;
#74808 = CARTESIAN_POINT ( 'NONE',  ( 0.6676899448993807162, 0.2205636587761065359, -2.251657551468993379 ) ) ;
#74809 = CARTESIAN_POINT ( 'NONE',  ( -4.391370929004954959, 7.351591927832363815, -1.215465595245905250 ) ) ;
#74810 = CARTESIAN_POINT ( 'NONE',  ( 11.55950211276791251, 11.37999999999999901, -3.221476510067114329 ) ) ;
#74811 = CARTESIAN_POINT ( 'NONE',  ( 6.454463653088309272, 6.866155873091829953, 0.6733577401037347254 ) ) ;
#74812 = CARTESIAN_POINT ( 'NONE',  ( -4.136646265500958819, 7.840188053144158786, -0.7216878364870458196 ) ) ;
#74813 = CARTESIAN_POINT ( 'NONE',  ( -0.005422908085399994089, -1.854866876809873943, -0.4647201794698225252 ) ) ;
#74814 = CARTESIAN_POINT ( 'NONE',  ( 0.6547154952327862709, -1.491839214215221698, -0.9519326369243490404 ) ) ;
#74815 = CIRCLE ( 'NONE', #182244, 0.08000000000000032085 ) ;
#74816 = CARTESIAN_POINT ( 'NONE',  ( 5.408844923620411471, -0.4912159631041897456, -1.952115566551455572 ) ) ;
#74817 = CARTESIAN_POINT ( 'NONE',  ( 5.738125327081736060, 7.717565519727259904, 1.599625672291267398 ) ) ;
#74818 = CARTESIAN_POINT ( 'NONE',  ( 4.700279962202062123, -2.105436441984291029, -0.05427613729028049616 ) ) ;
#74820 = CARTESIAN_POINT ( 'NONE',  ( 3.058105062934213692, -1.138753297271431375, 1.540237303602323804 ) ) ;
#74819 = CARTESIAN_POINT ( 'NONE',  ( -3.104453987404963478, 5.605318171072321221, -1.082531754730549078 ) ) ;
#74821 = CARTESIAN_POINT ( 'NONE',  ( 3.708318708537623021, 4.285125567170706695, -1.199719254218446718 ) ) ;
#74822 = CARTESIAN_POINT ( 'NONE',  ( 4.668383401541156275, -0.8401123053542228769, -1.781513398035587281 ) ) ;
#74823 = CARTESIAN_POINT ( 'NONE',  ( 5.467059065379825888, -1.589572006150547168, 1.245957840514285042 ) ) ;
#74824 = CARTESIAN_POINT ( 'NONE',  ( 2.975316878787794828, 1.776827963633962559, -0.5852370025475408521 ) ) ;
#74826 = VERTEX_POINT ( 'NONE', #9021 ) ;
#74825 = CARTESIAN_POINT ( 'NONE',  ( 5.654863297658344834, -1.355735166614827625, 1.066293663406183256 ) ) ;
#74828 = CARTESIAN_POINT ( 'NONE',  ( 5.694061328059515148, 5.745419092265303007, -0.7216878364870207285 ) ) ;
#74827 = CARTESIAN_POINT ( 'NONE',  ( 2.614145488985010424, -2.182733025630137824, 0.3247920039054427721 ) ) ;
#74829 = VECTOR ( 'NONE', #74734, 1000.000000000000000 ) ;
#74830 = CARTESIAN_POINT ( 'NONE',  ( 1.364683531249988535, 3.176041667008084435, 0.7879004041258500513 ) ) ;
#74831 = CARTESIAN_POINT ( 'NONE',  ( 6.443807124430430910, 1.351966286592180211, 1.421895456074427688 ) ) ;
#74832 = CARTESIAN_POINT ( 'NONE',  ( 8.613507663383630941, 8.943513783569379427, -0.7998128361456221525 ) ) ;
#74833 = CARTESIAN_POINT ( 'NONE',  ( -8.292783513053063160, 12.82666453187061073, 0.7998128361456481317 ) ) ;
#74834 = CARTESIAN_POINT ( 'NONE',  ( 6.856061878569608298E-15, 0.1875000000000181521, -1.225000000000034950 ) ) ;
#74835 = CARTESIAN_POINT ( 'NONE',  ( -0.1380770317961217131, 2.619511416136325987, -2.074674745642052898 ) ) ;
#74836 = DIRECTION ( 'NONE',  ( 1.000000000000000000, -7.771561172376097755E-16, -4.440892098500627148E-16 ) ) ;
#74837 = ORIENTED_EDGE ( 'NONE', *, *, #51769, .T. ) ;
#74838 = CARTESIAN_POINT ( 'NONE',  ( 2.313015868914463091, -1.601887806243259771, 1.311650804931147274 ) ) ;
#74839 = CARTESIAN_POINT ( 'NONE',  ( 1.499999999999989120, 2.754166666666688190, 0.8660254037844524744 ) ) ;
#74840 = CARTESIAN_POINT ( 'NONE',  ( 5.113396490648394632, 9.117379672398465473, 1.040834085586084257E-14 ) ) ;
#74841 = CARTESIAN_POINT ( 'NONE',  ( 4.577813143269636065, 5.369812084349879555, -1.199719254218450271 ) ) ;
#74843 = EDGE_CURVE ( 'NONE', #130986, #140091, #75096, .T. ) ;
#74842 = CARTESIAN_POINT ( 'NONE',  ( 6.287751673603878544, 2.029294879081492198, -0.6150919484220889188 ) ) ;
#74844 = CARTESIAN_POINT ( 'NONE',  ( 1.364683531249988535, 4.155208333674753618, -0.7879004041258239610 ) ) ;
#74845 = CIRCLE ( 'NONE', #213185, 0.05000000000000056483 ) ;
#74846 = ADVANCED_FACE ( 'NONE', ( #76156 ), #89095, .F. ) ;
#74848 = CARTESIAN_POINT ( 'NONE',  ( 9.625925876022625616, 11.29296361252366765, -1.082531754730537088 ) ) ;
#74847 = CARTESIAN_POINT ( 'NONE',  ( -0.4809368265653611307, 3.139971263792674439, -0.4000000000000453748 ) ) ;
#74849 = CARTESIAN_POINT ( 'NONE',  ( 5.378279760196133630, -0.2985789616767355326, 1.993766414912321094 ) ) ;
#74850 = CARTESIAN_POINT ( 'NONE',  ( 4.803869215722607500, -1.030175745946705801, -1.614969243545740785 ) ) ;
#74851 = CARTESIAN_POINT ( 'NONE',  ( -1.387358672534890536, 7.315968950354793776, -4.254625267136668221 ) ) ;
#74852 = CARTESIAN_POINT ( 'NONE',  ( 2.296645709751913955, 1.758124065145909798, -1.308193547052277861 ) ) ;
#74853 = CARTESIAN_POINT ( 'NONE',  ( 0.7499999999999902300, 1.764583334016148086, 1.299038105676657340 ) ) ;
#74854 = CARTESIAN_POINT ( 'NONE',  ( 2.039183100597967258, 0.003605121848727563250, 1.912571728241836633 ) ) ;
#74855 = CARTESIAN_POINT ( 'NONE',  ( -6.728924311084075960, 6.744833205886536120, 1.040834085586084257E-14 ) ) ;
#74857 = CARTESIAN_POINT ( 'NONE',  ( 0.3863424973270003226, -0.6820169105002243937, -1.897691504806876761 ) ) ;
#74856 = CARTESIAN_POINT ( 'NONE',  ( -3.307826292054316664, 4.882216645528547616, -1.443375672974059665 ) ) ;
#74858 = CARTESIAN_POINT ( 'NONE',  ( 0.6823417656249969321, 9.838541667008065872, -1.181850606188757036 ) ) ;
#74860 = CARTESIAN_POINT ( 'NONE',  ( -7.144220599758281054, 7.299621885998258897, 0.7998128361456341429 ) ) ;
#74859 = CARTESIAN_POINT ( 'NONE',  ( 2.964485117831549665, -1.932750628810533389, -0.7978010075700513459 ) ) ;
#74862 = EDGE_LOOP ( 'NONE', ( #163817, #97670, #163779, #55403 ) ) ;
#74861 = CARTESIAN_POINT ( 'NONE',  ( 2.344387759578896890, 0.3747227385639141373, 1.683394173241028913 ) ) ;
#74863 = CARTESIAN_POINT ( 'NONE',  ( 6.486587849989844834, -1.303813291173651301, 1.673118453357678392 ) ) ;
#74864 = CARTESIAN_POINT ( 'NONE',  ( 6.634017235788401301, 6.634108284708264414, 0.7998128361456341429 ) ) ;
#74865 = PRESENTATION_STYLE_ASSIGNMENT (( #202700 ) ) ;
#74866 = CARTESIAN_POINT ( 'NONE',  ( -1.737499999999997824, -2.347916665710752415, 3.009438278150925683 ) ) ;
#74867 = CARTESIAN_POINT ( 'NONE',  ( 6.169123589417988995, 7.156064594864501416, -1.199719254218445830 ) ) ;
#74868 = CARTESIAN_POINT ( 'NONE',  ( -11.87815913191694150, 13.80307820631414550, -1.708869976696544724 ) ) ;
#74869 = ORIENTED_EDGE ( 'NONE', *, *, #74775, .T. ) ;
#74870 = CARTESIAN_POINT ( 'NONE',  ( 3.352039220170324185, 0.8117645143102337757, -1.619458714540458866 ) ) ;
#74871 = ORIENTED_EDGE ( 'NONE', *, *, #30522, .T. ) ;
#74872 = CARTESIAN_POINT ( 'NONE',  ( 8.530051201292206287, 13.10347683481629488, 0.000000000000000000 ) ) ;
#74873 = CARTESIAN_POINT ( 'NONE',  ( 5.032011289327418702, 5.899709921417326974, 1.199719254218452935 ) ) ;
#74874 = CARTESIAN_POINT ( 'NONE',  ( 3.686021078551263930, 1.009145865423091815, 1.504116352017518476 ) ) ;
#74875 = CARTESIAN_POINT ( 'NONE',  ( 6.539320575229236709, 2.970193638644866851, 2.450124720169952752 ) ) ;
#74876 = FACE_OUTER_BOUND ( 'NONE', #88435, .T. ) ;
#74877 = CARTESIAN_POINT ( 'NONE',  ( 5.671489233189207724, 6.113434141373025099, 0.7590443732325997672 ) ) ;
#74879 = CARTESIAN_POINT ( 'NONE',  ( 1.364683531249997417, 14.23437500034140157, 2.602085213965210642E-15 ) ) ;
#74878 = CARTESIAN_POINT ( 'NONE',  ( 4.474962758555542486, 1.701137449889396747, 0.7551977096921670407 ) ) ;
#74880 = CARTESIAN_POINT ( 'NONE',  ( 1.018978518071847583, -1.731272710380473923, 0.8202338080745846804 ) ) ;
#74881 = CARTESIAN_POINT ( 'NONE',  ( 1.149113351018778539, -1.436424422225426767, -1.126575773451453433 ) ) ;
#74882 = DIRECTION ( 'NONE',  ( 0.000000000000000000, 0.000000000000000000, -1.000000000000000000 ) ) ;
#74883 = CARTESIAN_POINT ( 'NONE',  ( 1.387358672531703974, 7.315968950352358391, 4.254625267140708544 ) ) ;
#74884 = CARTESIAN_POINT ( 'NONE',  ( 5.975194856099406593, 7.098212677808693805, 1.080521340106417982 ) ) ;
#74885 = CARTESIAN_POINT ( 'NONE',  ( 9.571964790107170273, 13.80900892610533859, 8.297589824372789025 ) ) ;
#74886 = CARTESIAN_POINT ( 'NONE',  ( -1.566537053174817062, 8.754671357082440153, -2.463935854687004490 ) ) ;
#74887 = CARTESIAN_POINT ( 'NONE',  ( 3.475000000000000533, -2.581249999044084475, 0.000000000000000000 ) ) ;
#74888 = CARTESIAN_POINT ( 'NONE',  ( 7.673551755654734130, 9.015193805427763607, -1.082531754730537976 ) ) ;
#74889 = CARTESIAN_POINT ( 'NONE',  ( 5.506690373602650901, 0.5681407172444596920, 1.885743917740757114 ) ) ;
#74890 = CARTESIAN_POINT ( 'NONE',  ( -2.605138072120212200, 6.191078184115536232, -0.7998128361456281477 ) ) ;
#74891 = DIRECTION ( 'NONE',  ( 0.000000000000000000, -1.000000000000000000, 0.000000000000000000 ) ) ;
#74892 = CARTESIAN_POINT ( 'NONE',  ( 1.253981223613403806, 0.8486778832286197005, 1.910818189544212675 ) ) ;
#74893 = CARTESIAN_POINT ( 'NONE',  ( 6.686557393816916495, -1.889396554722815758, -0.3748701224956552669 ) ) ;
#74894 = CARTESIAN_POINT ( 'NONE',  ( -4.530395885260773525, 8.437212299446219532, 0.7998128361456481317 ) ) ;
#74895 = CARTESIAN_POINT ( 'NONE',  ( 1.817148636465517164, -0.2269042555285011864, 1.811363274943120549 ) ) ;
#74896 = CARTESIAN_POINT ( 'NONE',  ( 2.825073394047578734, 2.078234123670623212, 0.7428476018367863309 ) ) ;
#74897 = CARTESIAN_POINT ( 'NONE',  ( -2.788906526875773208E-15, 9.968750000682797818, -1.499999999999998446 ) ) ;
#74898 = CARTESIAN_POINT ( 'NONE',  ( 1.177825114000274898, 1.883588471398514264, -0.3297955356276888184 ) ) ;
#74899 = CARTESIAN_POINT ( 'NONE',  ( 1.082395645157930852, 1.176005852300557653, -1.579744537442813401 ) ) ;
#74900 = CARTESIAN_POINT ( 'NONE',  ( 2.630336588288070043, 0.2403035443280654992, 1.927090367541855365 ) ) ;
#74901 = AXIS2_PLACEMENT_3D ( 'NONE', #90064, #7708, #73791 ) ;
#74902 = VERTEX_POINT ( 'NONE', #49783 ) ;
#74903 = DIRECTION ( 'NONE',  ( 0.000000000000000000, 0.000000000000000000, -1.000000000000000000 ) ) ;
#74905 = CARTESIAN_POINT ( 'NONE',  ( 6.192234700126073577, 0.9181466042854893317, -1.618627059862162376 ) ) ;
#74904 = CARTESIAN_POINT ( 'NONE',  ( -5.492988512192097161, 6.437516681426083132, 1.199719254218452935 ) ) ;
#74906 = CARTESIAN_POINT ( 'NONE',  ( 3.562760505341037831, 7.378580699531681830, -1.734723475976807094E-15 ) ) ;
#74907 = CARTESIAN_POINT ( 'NONE',  ( 1.333449616921242198, 8.249651149236383318, -11.01993490927446828 ) ) ;
#74908 = CARTESIAN_POINT ( 'NONE',  ( 1.347111479062088405E-15, 6.999999999999999112, 11.00000000000000000 ) ) ;
#74909 = CARTESIAN_POINT ( 'NONE',  ( -4.925354943514475003, 8.968274210734028529, 0.000000000000000000 ) ) ;
#74910 = CARTESIAN_POINT ( 'NONE',  ( 2.613028500285840661, -0.2118117899099076218, 2.181281865515646068 ) ) ;
#74911 = CARTESIAN_POINT ( 'NONE',  ( 3.036575945257459885, 6.282152860354720758, -0.6783893874775955846 ) ) ;
#74912 = CARTESIAN_POINT ( 'NONE',  ( 10.99970480911018100, -6.304485801116100241, 0.08058605610353185289 ) ) ;
#74913 = DIRECTION ( 'NONE',  ( -0.6260462619842731558, -0.7797859179643593652, 0.000000000000000000 ) ) ;
#74914 = CARTESIAN_POINT ( 'NONE',  ( 2.771877994228102882, 0.9767612972278701955, 1.542236413651025151 ) ) ;
#74915 = DIRECTION ( 'NONE',  ( 0.000000000000000000, -1.000000000000000000, 0.000000000000000000 ) ) ;
#74916 = CARTESIAN_POINT ( 'NONE',  ( -3.898132859128961236, 4.506575409527250997, -1.199719254218452047 ) ) ;
#74917 = CARTESIAN_POINT ( 'NONE',  ( -4.612885993627734216, 8.463679738117141582, -0.3448095128447264957 ) ) ;
#74918 = CARTESIAN_POINT ( 'NONE',  ( 9.074484886248265880, 9.481320543578137361, 0.7998128361456462443 ) ) ;
#74919 = CARTESIAN_POINT ( 'NONE',  ( 0.9438256413601053829, 0.7817106414217175336, -1.760949446298063936 ) ) ;
#74920 = CARTESIAN_POINT ( 'NONE',  ( 6.051606296966551390, 1.483190043545830283, 1.284043323103729595 ) ) ;
#74921 = CARTESIAN_POINT ( 'NONE',  ( -1.402160292154681736E-14, 14.56249999999999645, 1.732050807568881190 ) ) ;
#74922 = CARTESIAN_POINT ( 'NONE',  ( -6.367525699912501835, 10.58053041653993098, -0.7998128361456291469 ) ) ;
#74923 = CARTESIAN_POINT ( 'NONE',  ( 4.497554271431305040, 6.270232621468402989, -1.599625672291256295 ) ) ;
#74924 = CARTESIAN_POINT ( 'NONE',  ( -4.245111494410291897, 7.006361605903701495, 1.082531754730549967 ) ) ;
#74925 = AXIS2_PLACEMENT_3D ( 'NONE', #62831, #111659, #126863 ) ;
#74926 = STYLED_ITEM ( 'NONE', ( #60043 ), #196809 ) ;
#74927 = CARTESIAN_POINT ( 'NONE',  ( -4.650083499807246668, 5.295740330745369207, -2.420000000000000373 ) ) ;
#74928 = CARTESIAN_POINT ( 'NONE',  ( -2.331639231870358930, 5.664070170583284103, -0.7216878364870267237 ) ) ;
#74929 = CARTESIAN_POINT ( 'NONE',  ( 5.366107254901440804, -2.060797467674013284, 0.1973761227843511823 ) ) ;
#74931 = CARTESIAN_POINT ( 'NONE',  ( 1.364683531249988535, 2.967708333674755394, -0.7879004041258239610 ) ) ;
#74930 = CARTESIAN_POINT ( 'NONE',  ( -2.373851744317279522, 1.000000000000000888, 11.76285798163022100 ) ) ;
#74932 = CARTESIAN_POINT ( 'NONE',  ( 5.625696599388652963, 0.4453364752643809155, 2.255009244304376992 ) ) ;
#74933 = CARTESIAN_POINT ( 'NONE',  ( 5.151735183512854199, 8.954182114166247430, -0.7216878364870257245 ) ) ;
#74935 = CARTESIAN_POINT ( 'NONE',  ( -2.788906526875773208E-15, 10.96875000068279427, -1.499999999999998446 ) ) ;
#74934 = CARTESIAN_POINT ( 'NONE',  ( 5.153507786970260796, 7.105788066255672497, -1.443375672974078761 ) ) ;
#74936 = CARTESIAN_POINT ( 'NONE',  ( 6.614806897001766828, -0.1637801000826353548, 2.256214727502181994 ) ) ;
#74937 = CARTESIAN_POINT ( 'NONE',  ( 7.712474369503314442, -6.289226506789199256, -7.712474369503347305 ) ) ;
#74938 = CARTESIAN_POINT ( 'NONE',  ( -6.936931872047518155, 8.122117267924091166, 1.199719254218452047 ) ) ;
#74939 = CARTESIAN_POINT ( 'NONE',  ( 5.367111071781861753, 1.871067490511884479, -0.5196462679451731015 ) ) ;
#74940 = ORIENTED_EDGE ( 'NONE', *, *, #87487, .T. ) ;
#74941 = CARTESIAN_POINT ( 'NONE',  ( 10.01911233037458260, 10.79131192829960462, 0.7216878364870438212 ) ) ;
#74942 = VERTEX_POINT ( 'NONE', #35654 ) ;
#74943 = CARTESIAN_POINT ( 'NONE',  ( 5.765855477156511810, 0.5488314196105298359, -1.831976909803390896 ) ) ;
#74944 = CARTESIAN_POINT ( 'NONE',  ( 6.528329376709017140, 0.9880424216301281204, -1.413504571246849695 ) ) ;
#74945 = CARTESIAN_POINT ( 'NONE',  ( 6.034388706570055660, 0.6371486477873434806, 1.913263546360920220 ) ) ;
#74947 = DIRECTION ( 'NONE',  ( 0.000000000000000000, 1.000000000000000000, 0.000000000000000000 ) ) ;
#74946 = CARTESIAN_POINT ( 'NONE',  ( -7.479294296233107708, 11.87759377891399204, 0.7998128361456481317 ) ) ;
#74948 = CARTESIAN_POINT ( 'NONE',  ( 3.285556943750000070, -1.771874999522041083, 0.000000000000000000 ) ) ;
#74950 = CARTESIAN_POINT ( 'NONE',  ( 6.802016525601501051, -1.769270574432443510, 0.04669485764256275928 ) ) ;
#74949 = CARTESIAN_POINT ( 'NONE',  ( 1.166094707548096965, -1.325134400199390550, 1.617025002462493921 ) ) ;
#74951 = CARTESIAN_POINT ( 'NONE',  ( 6.258435431136967431, 1.928752767684217106, -0.5880170417187426946 ) ) ;
#74953 = CARTESIAN_POINT ( 'NONE',  ( 2.695625570186571895, -0.7177931702126126856, 2.177047689787997342 ) ) ;
#74952 = CARTESIAN_POINT ( 'NONE',  ( 5.571474780572990504, 5.464751763615448787, 0.7998128361456352531 ) ) ;
#74954 = CARTESIAN_POINT ( 'NONE',  ( 1.956607802488403269, 0.2990611944714368642, -1.714256857270479051 ) ) ;
#74955 = CARTESIAN_POINT ( 'NONE',  ( 2.601940685209406467, 1.502730264585940168, 1.496503045097858919 ) ) ;
#74956 = PLANE ( 'NONE',  #93693 ) ;
#74957 = CARTESIAN_POINT ( 'NONE',  ( 2.055574482508758738, 1.511248224151232167, -0.8496982089122394610 ) ) ;
#74958 = CARTESIAN_POINT ( 'NONE',  ( -1.360316468750048635, 1.942708333674827204, 0.7853790794158580502 ) ) ;
#74959 = CARTESIAN_POINT ( 'NONE',  ( 1.996334026009699558, 1.840204857836050367, 0.2769876585018010706 ) ) ;
#74960 = CARTESIAN_POINT ( 'NONE',  ( 2.225261637991797325, -1.984409513266917502, -0.8813929409505830703 ) ) ;
#74961 = CARTESIAN_POINT ( 'NONE',  ( 3.432827581131673522, -1.645759781613131967, 1.164986487700324425 ) ) ;
#74962 = CARTESIAN_POINT ( 'NONE',  ( 4.468750000000002665, 0.7852924748297492874, -1.895863743164178494 ) ) ;
#74963 = CARTESIAN_POINT ( 'NONE',  ( -1.402160292154681736E-14, 2.618750000682819490, -1.732050807568863648 ) ) ;
#74964 = CARTESIAN_POINT ( 'NONE',  ( 1.536025370465494921, 0.9519229637394033272, -1.674701244428679292 ) ) ;
#74965 = CARTESIAN_POINT ( 'NONE',  ( 1.364683531250000303, 14.25520833367473372, -0.7879004041258355073 ) ) ;
#74966 = CARTESIAN_POINT ( 'NONE',  ( 3.305138010220570521, -0.4367349056570711263, -2.177900917948209614 ) ) ;
#74967 = VERTEX_POINT ( 'NONE', #33531 ) ;
#74968 = CARTESIAN_POINT ( 'NONE',  ( -0.2110808730066961458, 1.402160971018800995, -2.056005932258188285 ) ) ;
#74969 = CARTESIAN_POINT ( 'NONE',  ( -0.7500000000000006661, 0.8583333333333567072, -1.299038105676652011 ) ) ;
#74970 = CARTESIAN_POINT ( 'NONE',  ( 8.762647353133951711, 9.117510088278095282, 1.040834085586084257E-14 ) ) ;
#74971 = CARTESIAN_POINT ( 'NONE',  ( -0.6823417656250246877, -0.6989583329919113464, 1.181850606188755259 ) ) ;
#74972 = CARTESIAN_POINT ( 'NONE',  ( 6.047183177241617358, 0.2169752325061699572, 2.210822359046988428 ) ) ;
#74974 = CARTESIAN_POINT ( 'NONE',  ( 4.791432466842789673, -1.794507165602466037, 0.7932701521168731285 ) ) ;
#74973 = AXIS2_PLACEMENT_3D ( 'NONE', #6254, #138430, #155737 ) ;
#74976 = CARTESIAN_POINT ( 'NONE',  ( -5.233084105194862445, 9.049089189461916760, 0.7216878364870458196 ) ) ;
#74975 = CARTESIAN_POINT ( 'NONE',  ( 10.22248463502393001, 11.02857961705718282, 0.7216878364870438212 ) ) ;
#74977 = ADVANCED_FACE ( 'NONE', ( #51927 ), #186167, .T. ) ;
#74978 = CARTESIAN_POINT ( 'NONE',  ( -15.75000000000000000, 13.39999999999998259, 3.199999999999997957 ) ) ;
#74979 = CARTESIAN_POINT ( 'NONE',  ( 5.835331047353732536, -2.048883276207621229, 0.9597388403507837173 ) ) ;
#74980 = CARTESIAN_POINT ( 'NONE',  ( -5.126391479742927970, 8.994890803093138487, 0.7216878364870267237 ) ) ;
#74981 = CARTESIAN_POINT ( 'NONE',  ( 1.873554394494097997, -0.2548139927673950256, 2.046832928722150058 ) ) ;
#74982 = CARTESIAN_POINT ( 'NONE',  ( -6.338600509588822263, 7.353787668397130162, -1.199719254218446718 ) ) ;
#74983 = ORIENTED_EDGE ( 'NONE', *, *, #105361, .F. ) ;
#74984 = CARTESIAN_POINT ( 'NONE',  ( -1.500000000000013101, 3.160416667349486008, -0.8660254037844313801 ) ) ;
#74985 = CARTESIAN_POINT ( 'NONE',  ( 0.6823417656249917140, 3.905208333674754950, 1.181850606188765695 ) ) ;
#74986 = CARTESIAN_POINT ( 'NONE',  ( 4.710133486059870478, -0.7981590245086762625, -1.691823354513532163 ) ) ;
#74987 = CARTESIAN_POINT ( 'NONE',  ( 3.392920078539514162, -0.7062313252990999324, -1.584032799413936710 ) ) ;
#74988 = CARTESIAN_POINT ( 'NONE',  ( 2.753125985903591477, 1.731854804227653366, -0.1727350219371779905 ) ) ;
#74989 = CARTESIAN_POINT ( 'NONE',  ( 0.9082674546003096649, -1.036902680258915854, -2.044550831922228085 ) ) ;
#74990 = CARTESIAN_POINT ( 'NONE',  ( 0.8157880970438775581, -0.3219574891645953785, 2.183050487710703536 ) ) ;
#74991 = CARTESIAN_POINT ( 'NONE',  ( 4.142189164857057015, 0.5595570048471016911, 2.014385595549014418 ) ) ;
#74992 = CARTESIAN_POINT ( 'NONE',  ( 5.490160960519338218, -0.4736594950825470107, -1.883182239726274076 ) ) ;
#74993 = PRESENTATION_LAYER_ASSIGNMENT (  '', '', ( #109697 ) ) ;
#74995 = VERTEX_POINT ( 'NONE', #132145 ) ;
#74994 = CARTESIAN_POINT ( 'NONE',  ( -8.283668668269720925, 8.766627655843896250, 1.056142170575426150E-14 ) ) ;
#74996 = CARTESIAN_POINT ( 'NONE',  ( 0.05336153386781630759, -1.314994204386025434, 1.528742563917218078 ) ) ;
#74997 = CARTESIAN_POINT ( 'NONE',  ( -0.1929003719821283658, -0.4722129235960635940, -2.074948700427194481 ) ) ;
#74998 = DIRECTION ( 'NONE',  ( 1.000000000000000000, -0.000000000000000000, -0.000000000000000000 ) ) ;
#74999 =( NAMED_UNIT ( * ) SI_UNIT ( $, .STERADIAN. ) SOLID_ANGLE_UNIT ( ) );
#75000 = CARTESIAN_POINT ( 'NONE',  ( -8.799405390469187793, 10.22472669609091689, -1.199719254218446718 ) ) ;
#75001 = CARTESIAN_POINT ( 'NONE',  ( 6.470265622219697477, 8.571729197388226140, -1.599625672291262513 ) ) ;
#75002 = FACE_OUTER_BOUND ( 'NONE', #159534, .T. ) ;
#75003 = CARTESIAN_POINT ( 'NONE',  ( 4.230939532379584200, 0.09184734775685021724, 1.823503176236190626 ) ) ;
#75004 = CARTESIAN_POINT ( 'NONE',  ( 2.362605853119781774, 0.9431403173822919817, 1.995201469058570432 ) ) ;
#75005 = ORIENTED_EDGE ( 'NONE', *, *, #115899, .F. ) ;
#75006 = CARTESIAN_POINT ( 'NONE',  ( -6.071018923869249129, 10.30488218781460574, 0.7998128361456291469 ) ) ;
#75007 = CARTESIAN_POINT ( 'NONE',  ( -3.285556943750000070, -2.646874999522041971, 0.000000000000000000 ) ) ;
#75008 = CARTESIAN_POINT ( 'NONE',  ( -9.169391961543940539, 9.592045464756413509, 1.040834085586084257E-14 ) ) ;
#75009 = CARTESIAN_POINT ( 'NONE',  ( 1.283469775389501910, 0.1441914389909859651, -2.014673257830889685 ) ) ;
#75010 = CARTESIAN_POINT ( 'NONE',  ( -8.752560982293191572, 13.99999996919062539, -9.356054898126068053 ) ) ;
#75011 = CARTESIAN_POINT ( 'NONE',  ( -5.147255595043616516, 6.034161611419515125, 1.199719254218452935 ) ) ;
#75012 = CARTESIAN_POINT ( 'NONE',  ( 3.344433574756133787, -1.832611177030788685, -0.3225857369167430821 ) ) ;
#75013 = CARTESIAN_POINT ( 'NONE',  ( 2.866659414285625651, 5.431854185720147221, -1.199719254218446718 ) ) ;
#75014 = CARTESIAN_POINT ( 'NONE',  ( -4.903732577545095950, 4.837283930932079201, 0.1501914610188368471 ) ) ;
#75015 = ORIENTED_EDGE ( 'NONE', *, *, #4605, .F. ) ;
#75016 = ORIENTED_EDGE ( 'NONE', *, *, #70198, .F. ) ;
#75017 = CARTESIAN_POINT ( 'NONE',  ( -4.283486466913726254, 7.084819080452935403, -1.199719254218452047 ) ) ;
#75018 = CARTESIAN_POINT ( 'NONE',  ( -9.104463846776669200, 10.58062822844965645, -1.199719254218441611 ) ) ;
#75019 = CARTESIAN_POINT ( 'NONE',  ( 3.686012862905340803, -0.8985999850123352894, 1.589152278004740237 ) ) ;
#75021 = CARTESIAN_POINT ( 'NONE',  ( -5.688173390364544169, 6.286868445634342883, -1.126660468825124273 ) ) ;
#75020 = CARTESIAN_POINT ( 'NONE',  ( -5.354544322754380303, 5.211666229493680191, 0.7998128361456281477 ) ) ;
#75022 = CARTESIAN_POINT ( 'NONE',  ( 6.567098404289990476, 6.791591158854626720, -0.3517435911668670423 ) ) ;
#75023 = CARTESIAN_POINT ( 'NONE',  ( 0.8778075154764168886, -0.2618308253583972456, 1.713820766736633194 ) ) ;
#75024 = CARTESIAN_POINT ( 'NONE',  ( 5.630750141678076304, -1.662707896839428434, 0.7909858098210584831 ) ) ;
#75025 = CARTESIAN_POINT ( 'NONE',  ( 4.283989073270632275, 1.505461842163426933, 1.749087475023381133 ) ) ;
#75026 = CARTESIAN_POINT ( 'NONE',  ( 4.390861645979372341, 6.216034235099629157, -1.599625672291269396 ) ) ;
#75027 = CARTESIAN_POINT ( 'NONE',  ( 6.679002375395027613, -0.09866081283815136826, -2.159460157733564145 ) ) ;
#75028 = CARTESIAN_POINT ( 'NONE',  ( 6.239697403921985241, -2.179564881273305943, -0.7296402976008103947 ) ) ;
#75029 = CYLINDRICAL_SURFACE ( 'NONE', #110319, 0.08000000000000020983 ) ;
#75030 = CARTESIAN_POINT ( 'NONE',  ( -5.354544322754380303, 5.211666229493680191, 0.7998128361456281477 ) ) ;
#75031 = CARTESIAN_POINT ( 'NONE',  ( 5.717618200960680852, -1.824738551054584379, 0.4112096411929695439 ) ) ;
#75032 = VERTEX_POINT ( 'NONE', #199206 ) ;
#75034 = CARTESIAN_POINT ( 'NONE',  ( -3.610214042988883598, 7.433943160120816351, 0.7998128361456352531 ) ) ;
#75033 = CARTESIAN_POINT ( 'NONE',  ( 2.461071540317420592, -1.587761714688111780, 1.065645112462119570 ) ) ;
#75035 = CARTESIAN_POINT ( 'NONE',  ( 3.826972293661185187, 2.095320012007126476, 0.6930106488920934060 ) ) ;
#75036 = CARTESIAN_POINT ( 'NONE',  ( 4.663340677796647071, 1.974402194736598837, -0.7651654921337573967 ) ) ;
#75037 = CARTESIAN_POINT ( 'NONE',  ( 1.224999999999979217, 0.2083333340161329650, -0.7072540797572937077 ) ) ;
#75038 = CARTESIAN_POINT ( 'NONE',  ( 6.983263157960365675, 7.629137130509066722, 2.646189081643287810 ) ) ;
#75039 = CARTESIAN_POINT ( 'NONE',  ( 4.814553946184248368, 7.670711132973337065, -1.082531754730548412 ) ) ;
#75040 = CARTESIAN_POINT ( 'NONE',  ( -5.329763783503577379, 6.351050847909847086, 1.082531754730549078 ) ) ;
#75041 = CARTESIAN_POINT ( 'NONE',  ( 2.872455039471259575, 1.233635154574242554, 1.949979759383664524 ) ) ;
#75043 = EDGE_CURVE ( 'NONE', #107467, #190376, #17859, .T. ) ;
#75042 = CARTESIAN_POINT ( 'NONE',  ( 3.139059813392345077, -0.1416510307416830594, -1.956792864499560691 ) ) ;
#75044 = CARTESIAN_POINT ( 'NONE',  ( -4.111865726694519552, 8.019203457777400956, 0.000000000000000000 ) ) ;
#75045 = CARTESIAN_POINT ( 'NONE',  ( 6.912941059211402894, -1.598140348199797556, 1.303530876689311224 ) ) ;
#75046 = CARTESIAN_POINT ( 'NONE',  ( 3.389175213736292047, 5.937492935125556315, 1.082531754730558626 ) ) ;
#75047 = CARTESIAN_POINT ( 'NONE',  ( 5.415556014015861841, 5.282846535965431300, -0.7998128361456481317 ) ) ;
#75048 = ORIENTED_EDGE ( 'NONE', *, *, #11640, .F. ) ;
#75049 = CARTESIAN_POINT ( 'NONE',  ( 4.557827498477605488, 1.164984774316142113, 1.645760986912048640 ) ) ;
#75050 = CARTESIAN_POINT ( 'NONE',  ( -9.806625181386236179, 10.33548422123910449, -0.7998128361456291469 ) ) ;
#75051 = CARTESIAN_POINT ( 'NONE',  ( -4.489185348024023803, 8.251483745236578571, -0.001312355330887114441 ) ) ;
#75052 = CARTESIAN_POINT ( 'NONE',  ( -10.50659947519749693, 5.359800460605414152, -5.105385958519358169 ) ) ;
#75053 = CARTESIAN_POINT ( 'NONE',  ( 9.935427640716063991, 10.48575375712389679, -0.7998128361456281477 ) ) ;
#75055 = CIRCLE ( 'NONE', #74901, 0.07999999999999998779 ) ;
#75054 = CARTESIAN_POINT ( 'NONE',  ( 1.499139249613313574, 0.4210003976099167544, 2.129699363925404487 ) ) ;
#75056 = CARTESIAN_POINT ( 'NONE',  ( 5.876533236880477240, 5.820653295974182129, 0.7998128361456350310 ) ) ;
#75057 = CARTESIAN_POINT ( 'NONE',  ( -7.120058533108549526, 14.48019278289345024, -9.669703555270844575 ) ) ;
#75058 = CARTESIAN_POINT ( 'NONE',  ( -2.788906526875773208E-15, 10.43750000000000000, -1.499999999999998446 ) ) ;
#75059 = CARTESIAN_POINT ( 'NONE',  ( 5.084740326411086642, 7.951855545768795608, 1.193092838546747414 ) ) ;
#75060 = CARTESIAN_POINT ( 'NONE',  ( 1.089218918643636069, 1.818803954151678726, -0.9688405272365168130 ) ) ;
#75062 = CARTESIAN_POINT ( 'NONE',  ( 0.000000000000000000, 14.55347103577515000, 0.000000000000000000 ) ) ;
#75061 = CARTESIAN_POINT ( 'NONE',  ( -11.41157692552970815, 13.75910337086999746, -3.404533818002362100 ) ) ;
#75063 = CARTESIAN_POINT ( 'NONE',  ( -0.6823417656250212460, 0.8010416670080899859, 1.181850606188755259 ) ) ;
#75064 = ADVANCED_FACE ( 'NONE', ( #50853 ), #121733, .T. ) ;
#75065 = ORIENTED_EDGE ( 'NONE', *, *, #137524, .T. ) ;
#75066 = CARTESIAN_POINT ( 'NONE',  ( 3.563058999304801411, -1.561743426874351970, 1.103242700682869781 ) ) ;
#75067 = CARTESIAN_POINT ( 'NONE',  ( 5.190226478415982392, -1.756784752911320302, -0.2140884780794347908 ) ) ;
#75068 = CARTESIAN_POINT ( 'NONE',  ( 6.225128807330042591, 7.291680359087043151, -1.199719254218452047 ) ) ;
#75069 = CARTESIAN_POINT ( 'NONE',  ( -5.440899717785814715, 5.242137847038546461, 0.7998128361456341429 ) ) ;
#75071 = CARTESIAN_POINT ( 'NONE',  ( 6.064071300241554496, -1.020233025338047383, 1.621115200587377014 ) ) ;
#75070 = DIRECTION ( 'NONE',  ( -0.5131086435338335638, 0.8583236685137312083, 5.079270337660091961E-15 ) ) ;
#75072 = CARTESIAN_POINT ( 'NONE',  ( -1.402160292154681736E-14, -0.1624999999999815481, -1.732050807568870754 ) ) ;
#75073 = CARTESIAN_POINT ( 'NONE',  ( 1.152881054890652957, -0.5012615762394446728, -2.008655542368184221 ) ) ;
#75074 = CARTESIAN_POINT ( 'NONE',  ( 1.364683531249986537, -0.7822916663252464931, -0.7879004041258309554 ) ) ;
#75075 = CARTESIAN_POINT ( 'NONE',  ( 6.209813078548920728, -1.856259414618817383, 0.2309603555875269776 ) ) ;
#75076 = CARTESIAN_POINT ( 'NONE',  ( 1.928079105319381314, 1.052063804484974385, -1.491885150056403431 ) ) ;
#75078 = CARTESIAN_POINT ( 'NONE',  ( 4.855733865602142707, 8.067643820953190215, 0.9155131637919884380 ) ) ;
#75077 = CARTESIAN_POINT ( 'NONE',  ( 5.479209177496175087, -0.05098606815037013545, -2.206463706674952618 ) ) ;
#75079 = CARTESIAN_POINT ( 'NONE',  ( -1.364683531250014514, -0.01145833299191483488, -0.7879004041258359514 ) ) ;
#75080 = CARTESIAN_POINT ( 'NONE',  ( 3.332538901969614553, -1.230775513943611399, 1.655089866650825581 ) ) ;
#75081 = CARTESIAN_POINT ( 'NONE',  ( -7.888146445052511169, 8.097259028849730811, 1.040834085586084257E-14 ) ) ;
#75082 = CARTESIAN_POINT ( 'NONE',  ( 9.576136569953906275, 10.06658084123472641, 0.000000000000000000 ) ) ;
#75083 = CARTESIAN_POINT ( 'NONE',  ( 3.493197133815315603, 7.227147089426516402, -0.7998128361456291469 ) ) ;
#75084 = CARTESIAN_POINT ( 'NONE',  ( 0.2808502495336914206, -2.096634173354972486, -0.5254431554712820640 ) ) ;
#75085 = CARTESIAN_POINT ( 'NONE',  ( 6.099189001301251523, 8.209082816308541197, 1.599625672291268286 ) ) ;
#75086 = AXIS2_PLACEMENT_3D ( 'NONE', #209757, #97123, #14761 ) ;
#75087 = CARTESIAN_POINT ( 'NONE',  ( 5.477033855465498924, 1.911541192706748715, 0.7957256658025002594 ) ) ;
#75088 = CARTESIAN_POINT ( 'NONE',  ( 0.6823417656249882723, -0.5947916663252492686, 1.181850606188755259 ) ) ;
#75089 = CARTESIAN_POINT ( 'NONE',  ( 2.882270108570818223, -1.113908571083363164, 1.852364028112465810 ) ) ;
#75090 = CARTESIAN_POINT ( 'NONE',  ( -4.719039639065737646, 8.241789607316443167, 0.6479098462880685805 ) ) ;
#75093 = ADVANCED_FACE ( 'NONE', ( #67066 ), #36547, .F. ) ;
#75092 = CARTESIAN_POINT ( 'NONE',  ( 1.838261372102001800, -1.052240823716396267, 1.655630454418555830 ) ) ;
#75091 = CARTESIAN_POINT ( 'NONE',  ( 3.106122398345218638, -0.8164384046550461349, 1.847479848726358398 ) ) ;
#75094 = CARTESIAN_POINT ( 'NONE',  ( 11.92619526913699879, 10.19999999999999929, -1.328859060402686199 ) ) ;
#75095 = EDGE_CURVE ( 'NONE', #93554, #31644, #120319, .T. ) ;
#75098 = CARTESIAN_POINT ( 'NONE',  ( 7.307481608085759639, 7.627742752295940676, 1.040834085586084257E-14 ) ) ;
#75097 = CARTESIAN_POINT ( 'NONE',  ( 3.475000000000000533, -0.5250000000000011324, 0.000000000000000000 ) ) ;
#75096 = LINE ( 'NONE', #92444, #83604 ) ;
#75099 = CARTESIAN_POINT ( 'NONE',  ( -7.944151662964566540, 8.232874793072271657, 0.000000000000000000 ) ) ;
#75100 = CARTESIAN_POINT ( 'NONE',  ( 0.8664231474371618669, -1.968446048378743152, -0.4370742218882398000 ) ) ;
#75102 = CARTESIAN_POINT ( 'NONE',  ( 5.917560222199001352, -1.216239291071326001, -1.822900893127032962 ) ) ;
#75101 = CARTESIAN_POINT ( 'NONE',  ( -5.915435094264120508, 5.795762452929912101, 0.000000000000000000 ) ) ;
#75103 = CARTESIAN_POINT ( 'NONE',  ( -1.500000000000011324, 5.660416667349481123, -0.8660254037844313801 ) ) ;
#75104 = CARTESIAN_POINT ( 'NONE',  ( 6.152599605923961157, 1.892562589925715466, 0.2737767527046449101 ) ) ;
#75105 = CARTESIAN_POINT ( 'NONE',  ( -3.277320446201389181, 4.846626492033466072, 1.599625672291267398 ) ) ;
#75106 = CARTESIAN_POINT ( 'NONE',  ( 4.650083499362864359, 7.408552601689905259, 1.082531754730558626 ) ) ;
#75108 = CARTESIAN_POINT ( 'NONE',  ( 3.075796161730546707, -0.8146103074460913085, 1.844718345957757188 ) ) ;
#75107 = CARTESIAN_POINT ( 'NONE',  ( -8.663296969008007054, 9.209527340038563992, 0.7216878364870438212 ) ) ;
#75109 = CARTESIAN_POINT ( 'NONE',  ( -1.499999999999997780, 4.150000000000021672, 1.214306433183764966E-14 ) ) ;
#75110 = CARTESIAN_POINT ( 'NONE',  ( -1.364683531250010295, 13.94270833367473195, 0.7879004041258445001 ) ) ;
#75111 = CARTESIAN_POINT ( 'NONE',  ( 6.756889588843246308, -1.328954913838266361, 1.099249449767102593 ) ) ;
#75112 = CARTESIAN_POINT ( 'NONE',  ( 5.176180785367283654, 9.260904359562321275, -0.7998128361456481317 ) ) ;
#75113 = CARTESIAN_POINT ( 'NONE',  ( 7.944714827928039291, 11.25228915168265864, 1.082531754730557072 ) ) ;
#75114 = CARTESIAN_POINT ( 'NONE',  ( -0.3868389748196900402, 3.100956225802461663, 0.4583768147623411560 ) ) ;
#75115 = CARTESIAN_POINT ( 'NONE',  ( 4.780451015977909002, -1.813929833846049666, -0.4561423458772846939 ) ) ;
#75116 = CARTESIAN_POINT ( 'NONE',  ( -4.081922216054144847, 7.264673858714298937, 0.8994561575802516584 ) ) ;
#75117 = VERTEX_POINT ( 'NONE', #119239 ) ;
#75118 = AXIS2_PLACEMENT_3D ( 'NONE', #43998, #209654, #175066 ) ;
#75119 = CARTESIAN_POINT ( 'NONE',  ( 1.534126288888465917, 1.230018689141991306, 1.665114864061276512 ) ) ;
#75120 = CARTESIAN_POINT ( 'NONE',  ( -7.892254816486440561, 8.380254505421877553, 0.000000000000000000 ) ) ;
#75121 = ORIENTED_EDGE ( 'NONE', *, *, #189935, .F. ) ;
#75122 = CARTESIAN_POINT ( 'NONE',  ( 4.848976215542928792, 5.686169002002086970, 1.199719254218452047 ) ) ;
#75123 = CARTESIAN_POINT ( 'NONE',  ( -0.1409997244346088141, -0.002808977843308038680, -2.000147647483838220 ) ) ;
#75124 = CARTESIAN_POINT ( 'NONE',  ( 0.3865838573892222962, -1.705918499434391444, -0.6100900862041622741 ) ) ;
#75125 = CARTESIAN_POINT ( 'NONE',  ( 5.031484404002891431, 5.042689024191078673, 0.7216878364870328300 ) ) ;
#75126 = CARTESIAN_POINT ( 'NONE',  ( 9.843899315504291536, 11.91674516233577563, 6.865790592497620359 ) ) ;
#75127 = ORIENTED_EDGE ( 'NONE', *, *, #87363, .T. ) ;
#75128 = AXIS2_PLACEMENT_3D ( 'NONE', #167220, #55596, #51337 ) ;
#75129 = CARTESIAN_POINT ( 'NONE',  ( 8.771762197917315262, 10.29643932140079166, -1.082531754730543083 ) ) ;
#75131 = CARTESIAN_POINT ( 'NONE',  ( 7.507464373665139412, 9.781794407407920389, 1.599625672291281386 ) ) ;
#75130 = CARTESIAN_POINT ( 'NONE',  ( 1.644895634054041933, -0.2845770130874228365, -1.940982728367894206 ) ) ;
#75132 = CARTESIAN_POINT ( 'NONE',  ( 6.011341193797766103, -1.801927099207595084, 0.6504362055675115828 ) ) ;
#75133 = CARTESIAN_POINT ( 'NONE',  ( -11.33772463945043718, 13.39999999999999147, 3.600000000000075140 ) ) ;
#75134 = CARTESIAN_POINT ( 'NONE',  ( -5.395781948114519722, 5.397426482329451325, 0.000000000000000000 ) ) ;
#75135 = CARTESIAN_POINT ( 'NONE',  ( 6.727182134110234024, -0.002100931800118066312, 2.089081857379894824 ) ) ;
#75137 = ORIENTED_EDGE ( 'NONE', *, *, #84764, .T. ) ;
#75136 = CARTESIAN_POINT ( 'NONE',  ( 3.687454593236936251, 7.245854758844324728, -0.7216878364870267237 ) ) ;
#75138 = CARTESIAN_POINT ( 'NONE',  ( -7.185458225562757484, 11.32685899655781903, 0.7216878364870458196 ) ) ;
#75139 = CARTESIAN_POINT ( 'NONE',  ( 2.694378501574711926, -2.155843008138720762, -0.1600555415394027403 ) ) ;
#75140 = CARTESIAN_POINT ( 'NONE',  ( -3.786470039966538970, 7.639575156594750283, 0.000000000000000000 ) ) ;
#75141 = CARTESIAN_POINT ( 'NONE',  ( 2.878073747850912412, 6.579779482459851003, -0.7998128361456362523 ) ) ;
#75142 = CARTESIAN_POINT ( 'NONE',  ( 0.2113915902133573221, 1.759560880827226947, -1.183302968686468226 ) ) ;
#75143 = CARTESIAN_POINT ( 'NONE',  ( 5.420859398437725574, 1.687492901312273474, 0.6969783729503381542 ) ) ;
#75144 = CARTESIAN_POINT ( 'NONE',  ( 9.935043313833721967, 9.392192033208111468, 7.152792536608178153 ) ) ;
#75145 = CARTESIAN_POINT ( 'NONE',  ( 1.212115688179933759, -0.8827433895065642799, -1.762721879769993283 ) ) ;
#75146 = CARTESIAN_POINT ( 'NONE',  ( 3.972844611716894736, -1.413603510852480927, 1.288168406687495215 ) ) ;
#75147 = ORIENTED_EDGE ( 'NONE', *, *, #57540, .F. ) ;
#75148 = CARTESIAN_POINT ( 'NONE',  ( 0.2999999999999846123, 4.000000000000008882, 0.9782388782688751228 ) ) ;
#75149 = CARTESIAN_POINT ( 'NONE',  ( 4.791434771068385778, -1.801603960925775016, 0.7962418042333998525 ) ) ;
#75150 = EDGE_LOOP ( 'NONE', ( #154670, #57966, #79949, #66862 ) ) ;
#75151 = CARTESIAN_POINT ( 'NONE',  ( 6.532770933798597746, -1.732582191135303651, 0.8775855664264734513 ) ) ;
#75152 = ORIENTED_EDGE ( 'NONE', *, *, #94600, .F. ) ;
#75153 = CARTESIAN_POINT ( 'NONE',  ( -6.635789839245807897, 6.706452665400368218, 0.7998128361456341429 ) ) ;
#75155 = CARTESIAN_POINT ( 'NONE',  ( -0.6125000000000210276, 1.354166667349498976, 1.060881119635887604 ) ) ;
#75154 = CARTESIAN_POINT ( 'NONE',  ( -5.632486471834530661, 5.535932070087196344, -0.7998128361456362523 ) ) ;
#75156 = CARTESIAN_POINT ( 'NONE',  ( 7.634649897826744080, 9.040084647953621655, 1.082531754730549078 ) ) ;
#75158 = ORIENTED_EDGE ( 'NONE', *, *, #111631, .F. ) ;
#75157 = CARTESIAN_POINT ( 'NONE',  ( 4.424404876070213710, -0.8207606565990737124, -1.727334472114170794 ) ) ;
#75159 = CARTESIAN_POINT ( 'NONE',  ( -1.854049621773892653, 5.499999999999998224, -0.7500000000000015543 ) ) ;
#75160 = CARTESIAN_POINT ( 'NONE',  ( 9.651540038386254849, 3.878167290971859860, -7.130941910101068260 ) ) ;
#75161 = CARTESIAN_POINT ( 'NONE',  ( 6.129547061768469085, -0.2442746830248194168, 1.998141925448652989 ) ) ;
#75163 =( BOUNDED_SURFACE ( )  B_SPLINE_SURFACE ( 1, 2, ( 
 ( #62589, #30103, #94064, #92997, #212024, #13830, #195803, #175306, #45302, #79905, #160104, #44238, #142826, #146013, #26893, #159041, #125558, #179558, #194725, #111421, #147071, #11707, #77781, #143902, #209895, #177425, #208833, #95126, #60463, #12761, #31179, #161175, #59402, #78835, #144956, #210962, #128752, #46364, #63667, #191519, #129821, #47440, #113555, #97252, #163306, #14887, #80982, #213092, #66821, #200046, #35419, #20230, #33289, #148130, #52743, #182735, #51697, #98304, #184863, #118877, #99373, #755, #117819, #181662, #183809, #165425, #34354, #168627, #64722, #164369, #150266, #132964, #116736, #130864, #214131, #17023, #36490, #32233, #198967, #135089, #114617, #67893, #196860, #102567, #48498, #180608, #86315, #100427, #167567, #2897, #166498, #18089, #15953, #50611, #83099, #65759, #131906, #101497, #82036, #201103, #197914, #49542, #151329, #115668, #84177, #149179, #1834, #134038, #19167, #85241, #68970, #137224, #72177, #202166, #203244, #40792, #54888, #106897, #188074, #156669, #58087, #6107, #155593, #7178, #8261, #103645, #138285, #53824, #190207, #122109, #154528, #204300, #139356, #121042, #187009, #169697, #38640, #136149, #5031, #71106, #21285, #55956, #153458, #104719, #170767, #107976, #22356, #41867, #88468, #174005, #189153, #25576, #124249, #39703, #152387, #105812, #3965, #70033, #119954, #171838, #23431, #24499, #185929, #89542, #205386, #87391, #57025, #172923, #73249, #123192, #90610, #37565, #74345, #140449, #206460, #42932, #194485, #95952, #92749, #60214, #158793, #93816, #176122, #109042, #78598, #175061, #144718, #209649, #43993, #157740, #210730, #63426, #179322, #47201, #113316, #10390, #159857, #193422, #62356, #76465, #59150, #91687, #128517, #129578, #9337, #142574, #46128, #160931, #29869, #13596, #211788, #112245, #195565, #26648, #75410, #178256, #208581, #162007, #79670, #45066, #143654, #11460, #141523, #12525, #126375, #145785, #192334, #207531, #125308, #110111, #27722, #77533, #61290, #127451, #111177, #191266, #177179, #28795, #94879, #147885, #30943, #182480, #117559, #97018, #101237, #163072, #164133, #115433, #148935, #100180, #15717, #130633, #14653, #166245, #80747, #146835, #81802, #150009, #17835, #51440, #183554, #212854, #67640, #64491, #213901, #196625, #50368, #35161, #48264, #83918, #116491, #114378, #132717, #507, #49316, #197672, #180373, #65524, #31997, #181424, #98078, #131669, #34108, #33054, #198722, #99132, #165181, #16775, #82859, #66575, #1579, #133787, #199795, #58378, #109336, #10672, #208867, #112517, #77816, #111459, #26926, #174286, #28006, #91971, #30141, #207809, #143938, #45340, #175346, #25861, #78872, #177463, #62624, #190492, #126656, #95163, #43219, #59438, #158029, #29078, #108264, #42150, #206749, #46401, #61572, #60497, #13867, #93034, #125594, #191555, #159076, #76743, #124534, #142865, #9617, #94103, #178531, #192623, #140737, #44275, #75693, #141805, #209933, #128785, #110396, #194764, #144995, #176401, #160142, #11742, #127739, #193696, #161212, #96229, #162280, #12799, #211000, #49582, #114655, #131943, #64762, #34389, #115707, #84214, #200082, #148166, #83138, #149216, #150302, #31216, #214169, #129856, #117852, #181697, #82074, #65794, #66858, #130904, #196897, #97290, #48536, #63702, #147107, #213131, #163347, #197954, #81018, #180649, #32273, #35456, #98340, #183844, #164405, #101534, #116775, #167604, #51730, #15989, #79945, #33327, #146049, #212062, #195840, #99409, #165462, #166537, #47481, #17057, #133004, #14924, #199004, #100461, #791, #50648, #182772, #113592, #18125, #1868, #67928, #134073, #179595, #23470, #20269, #202205, #86353, #21321, #103683, #36523, #6141, #184899, #72211, #137258, #185969, #85281, #138318, #205422, #106935, #189188, #40825, #152424, #87428, #121076, #204334, #4003, #201141, #19202, #55992, #57060, #151367, #70072, #122143, #88502, #171873, #155627, #139389, #188111, #123224, #102610, #2936, #203278, #39742, #89578, #187043, #54924, #69008, #153495, #169732, #136185, #168665, #105846, #135125, #53859, #52779, #118918, #5065, #7212, #119992, #154565, #37602, #71141, #38675 ),
 ( #104754, #73286, #170803, #22393, #111213, #25611, #10426, #124283, #172958, #192371, #127488, #128551, #62386, #157774, #193459, #142610, #207562, #76498, #9372, #45103, #208618, #177215, #78630, #26683, #176158, #27758, #28828, #190243, #92785, #8296, #210766, #60252, #175096, #158830, #159891, #75443, #141555, #41901, #59185, #156706, #91723, #125340, #108012, #126409, #174038, #191303, #42971, #194516, #109081, #46164, #44027, #24537, #209685, #90645, #144755, #110145, #74381, #93854, #140482, #206494, #58124, #11499, #77570, #94917, #143693, #61329, #160966, #12556, #16806, #66606, #213934, #164164, #180409, #95986, #33089, #129613, #181459, #63459, #540, #116522, #113350, #80782, #179355, #114409, #196657, #195599, #99163, #47235, #165216, #15750, #64523, #178294, #82892, #83954, #199832, #67675, #133819, #30977, #32027, #65555, #148967, #97052, #79702, #112277, #163106, #132752, #198755, #131701, #81834, #98113, #162038, #50404, #14686, #182513, #146870, #34143, #100212, #212892, #130669, #48298, #147917, #197706, #49348, #166281, #115467, #17870, #150044, #1615, #29901, #13629, #145817, #211822, #6951, #73032, #184646, #53597, #153231, #22124, #36266, #18943, #51473, #104496, #23205, #139130, #52528, #88236, #120811, #204076, #187853, #171611, #154307, #89319, #68754, #117597, #169479, #5879, #55728, #4801, #21063, #183588, #119732, #135922, #118663, #200883, #71953, #167356, #39479, #134876, #105578, #121883, #102344, #103418, #2683, #35197, #70882, #138063, #101271, #155366, #168415, #85028, #87160, #86098, #136994, #20012, #151116, #203021, #152172, #3741, #185710, #54663, #186788, #69816, #201942, #37344, #38415, #170539, #174850, #207314, #125094, #192119, #41645, #107759, #8034, #173785, #188929, #57866, #124028, #74125, #191052, #206240, #189995, #25360, #160710, #91460, #28579, #157522, #12304, #27500, #94668, #110956, #9117, #78385, #75192, #205158, #56800, #176963, #26429, #141304, #77320, #122969, #58937, #43784, #42717, #156450, #40566, #10178, #159644, #106674, #172697, #108825, #11242, #92539, #158579, #76252, #142362, #143433, #208371, #209429, #24275, #60003, #126156, #109897, #61074, #140220, #175909, #90381, #93600, #127233, #193203, #44850, #131459, #195347, #46980, #161790, #113096, #128307, #211571, #63205, #13381, #64279, #145573, #129369, #179101, #99974, #30724, #182272, #96807, #166040, #181213, #33896, #50159, #162855, #17624, #14434, #144505, #210512, #116281, #114169, #80523, #16561, #62148, #146621, #197460, #79456, #49102, #98917, #31788, #196411, #212638, #194269, #65310, #130426, #213688, #95739, #32840, #148728, #48056, #180162, #97861, #163923, #15499, #81586, #115222, #147670, #164970, #82645, #297, #45915, #66368, #112033, #178036, #29653, #132515, #198513, #85854, #185473, #54428, #2435, #51226, #83709, #136750, #55488, #105330, #84783, #120569, #152990, #21882, #5629, #203842, #186546, #121642, #101023, #149798, #201709, #38176, #87989, #37095, #53352, #1372, #151929, #168173, #150871, #18701, #104248, #199583, #71710, #167114, #137823, #154064, #68510, #19772, #3504, #187610, #20824, #170294, #184405, #117350, #103173, #34952, #39237, #134637, #86922, #202777, #118419, #183347, #171366, #67433, #133577, #200642, #69574, #52290, #36025, #102103, #135684, #119486, #169235, #4564, #70639, #143187, #158336, #91210, #110705, #205991, #90139, #73874, #57627, #139969, #6714, #189744, #188685, #190803, #209178, #8862, #22960, #123785, #172449, #138891, #174600, #41396, #191868, #89075, #204910, #107506, #156206, #40320, #155132, #175654, #173535, #72790, #157272, #9930, #59750, #44591, #25108, #24036, #77057, #207058, #76004, #122723, #60817, #126978, #74941, #141052, #142108, #58689, #208121, #124837, #42463, #192937, #56563, #106426, #26176, #108572, #92292, #7782, #125910, #43528, #109651, #27241, #93348, #159384, #10983, #31531, #176705, #66109, #28317, #144258, #45, #113913, #97606, #210251, #47800, #179908, #12061, #49900, #78128, #178854, #212379, #61889, #128052, #82387, #177780, #194007, #45656, #163664, #15246, #81334, #111773, #65061, #132251, #14172 ) ),
 .UNSPECIFIED., .F., .F., .T. ) 
 B_SPLINE_SURFACE_WITH_KNOTS ( ( 2, 2 ),
 ( 3, 2, 2, 2, 2, 2, 2, 2, 2, 2, 2, 2, 2, 2, 2, 2, 2, 2, 2, 2, 2, 2, 2, 2, 2, 2, 2, 2, 2, 2, 2, 2, 2, 2, 2, 2, 2, 2, 2, 2, 2, 2, 2, 2, 2, 2, 2, 2, 2, 2, 2, 2, 2, 2, 2, 2, 2, 2, 2, 2, 2, 2, 2, 2, 2, 2, 2, 2, 2, 2, 2, 2, 2, 2, 2, 2, 2, 2, 2, 2, 2, 2, 2, 2, 2, 2, 2, 2, 2, 2, 2, 2, 2, 2, 2, 2, 2, 2, 2, 2, 2, 2, 2, 2, 2, 2, 2, 2, 2, 2, 2, 2, 2, 2, 2, 2, 2, 2, 2, 2, 2, 2, 2, 2, 2, 2, 2, 2, 2, 2, 2, 2, 2, 2, 2, 2, 2, 2, 2, 2, 2, 2, 2, 2, 2, 2, 2, 2, 2, 2, 2, 2, 2, 2, 2, 2, 2, 2, 2, 2, 2, 2, 2, 2, 2, 2, 2, 2, 2, 2, 2, 2, 2, 2, 2, 2, 2, 2, 2, 2, 2, 2, 2, 2, 2, 2, 2, 2, 2, 2, 2, 2, 2, 2, 2, 2, 2, 2, 2, 2, 2, 2, 2, 2, 2, 2, 2, 2, 2, 2, 2, 2, 2, 2, 2, 2, 2, 2, 2, 2, 2, 2, 2, 2, 2, 2, 2, 2, 2, 2, 2, 2, 2, 2, 2, 2, 2, 2, 2, 2, 3 ),
 ( 0.000000000000000000, 1.000000000000000000 ),
 ( 0.000000000000000000, 0.004166666666666666609, 0.008333333333333333218, 0.01250000000000000069, 0.01666666666666666644, 0.02083333333333333218, 0.02500000000000000139, 0.02916666666666666713, 0.03333333333333333287, 0.03749999999999999861, 0.04166666666666666435, 0.04583333333333333010, 0.05000000000000000278, 0.05416666666666666852, 0.05833333333333333426, 0.06250000000000000000, 0.06666666666666666574, 0.07083333333333333148, 0.07499999999999999722, 0.07916666666666666297, 0.08333333333333332871, 0.08749999999999999445, 0.09166666666666666019, 0.09583333333333333981, 0.1000000000000000056, 0.1041666666666666713, 0.1083333333333333370, 0.1125000000000000028, 0.1166666666666666685, 0.1208333333333333343, 0.1250000000000000000, 0.1291666666666666796, 0.1333333333333333315, 0.1375000000000000111, 0.1416666666666666630, 0.1458333333333333426, 0.1499999999999999944, 0.1541666666666666741, 0.1583333333333333259, 0.1625000000000000056, 0.1666666666666666574, 0.1708333333333333370, 0.1749999999999999889, 0.1791666666666666685, 0.1833333333333333204, 0.1875000000000000000, 0.1916666666666666796, 0.1958333333333333315, 0.2000000000000000111, 0.2041666666666666630, 0.2083333333333333426, 0.2124999999999999944, 0.2166666666666666741, 0.2208333333333333259, 0.2250000000000000056, 0.2291666666666666574, 0.2333333333333333370, 0.2374999999999999889, 0.2416666666666666685, 0.2458333333333333204, 0.2500000000000000000, 0.2541666666666666519, 0.2583333333333333592, 0.2625000000000000111, 0.2666666666666666630, 0.2708333333333333148, 0.2750000000000000222, 0.2791666666666666741, 0.2833333333333333259, 0.2874999999999999778, 0.2916666666666666852, 0.2958333333333333370, 0.2999999999999999889, 0.3041666666666666408, 0.3083333333333333481, 0.3125000000000000000, 0.3166666666666666519, 0.3208333333333333592, 0.3250000000000000111, 0.3291666666666666630, 0.3333333333333333148, 0.3375000000000000222, 0.3416666666666666741, 0.3458333333333333259, 0.3499999999999999778, 0.3541666666666666852, 0.3583333333333333370, 0.3624999999999999889, 0.3666666666666666408, 0.3708333333333333481, 0.3750000000000000000, 0.3791666666666666519, 0.3833333333333333592, 0.3875000000000000111, 0.3916666666666666630, 0.3958333333333333148, 0.4000000000000000222, 0.4041666666666666741, 0.4083333333333333259, 0.4124999999999999778, 0.4166666666666666852, 0.4208333333333333370, 0.4249999999999999889, 0.4291666666666666408, 0.4333333333333333481, 0.4375000000000000000, 0.4416666666666666519, 0.4458333333333333592, 0.4500000000000000111, 0.4541666666666666630, 0.4583333333333333148, 0.4625000000000000222, 0.4666666666666666741, 0.4708333333333333259, 0.4749999999999999778, 0.4791666666666666852, 0.4833333333333333370, 0.4874999999999999889, 0.4916666666666666408, 0.4958333333333333481, 0.5000000000000000000, 0.5041666666666666519, 0.5083333333333333037, 0.5124999999999999556, 0.5166666666666667185, 0.5208333333333333703, 0.5250000000000000222, 0.5291666666666666741, 0.5333333333333333259, 0.5374999999999999778, 0.5416666666666666297, 0.5458333333333332815, 0.5500000000000000444, 0.5541666666666666963, 0.5583333333333333481, 0.5625000000000000000, 0.5666666666666666519, 0.5708333333333333037, 0.5749999999999999556, 0.5791666666666667185, 0.5833333333333333703, 0.5875000000000000222, 0.5916666666666666741, 0.5958333333333333259, 0.5999999999999999778, 0.6041666666666666297, 0.6083333333333332815, 0.6125000000000000444, 0.6166666666666666963, 0.6208333333333333481, 0.6250000000000000000, 0.6291666666666666519, 0.6333333333333333037, 0.6374999999999999556, 0.6416666666666667185, 0.6458333333333333703, 0.6500000000000000222, 0.6541666666666666741, 0.6583333333333333259, 0.6624999999999999778, 0.6666666666666666297, 0.6708333333333332815, 0.6750000000000000444, 0.6791666666666666963, 0.6833333333333333481, 0.6875000000000000000, 0.6916666666666666519, 0.6958333333333333037, 0.6999999999999999556, 0.7041666666666667185, 0.7083333333333333703, 0.7125000000000000222, 0.7166666666666666741, 0.7208333333333333259, 0.7249999999999999778, 0.7291666666666666297, 0.7333333333333332815, 0.7375000000000000444, 0.7416666666666666963, 0.7458333333333333481, 0.7500000000000000000, 0.7541666666666666519, 0.7583333333333333037, 0.7624999999999999556, 0.7666666666666667185, 0.7708333333333333703, 0.7750000000000000222, 0.7791666666666666741, 0.7833333333333333259, 0.7874999999999999778, 0.7916666666666666297, 0.7958333333333332815, 0.8000000000000000444, 0.8041666666666666963, 0.8083333333333333481, 0.8125000000000000000, 0.8166666666666666519, 0.8208333333333333037, 0.8249999999999999556, 0.8291666666666667185, 0.8333333333333333703, 0.8375000000000000222, 0.8416666666666666741, 0.8458333333333333259, 0.8499999999999999778, 0.8541666666666666297, 0.8583333333333332815, 0.8625000000000000444, 0.8666666666666666963, 0.8708333333333333481, 0.8750000000000000000, 0.8791666666666666519, 0.8833333333333333037, 0.8874999999999999556, 0.8916666666666667185, 0.8958333333333333703, 0.9000000000000000222, 0.9041666666666666741, 0.9083333333333333259, 0.9124999999999999778, 0.9166666666666666297, 0.9208333333333332815, 0.9250000000000000444, 0.9291666666666666963, 0.9333333333333333481, 0.9375000000000000000, 0.9416666666666666519, 0.9458333333333333037, 0.9499999999999999556, 0.9541666666666667185, 0.9583333333333333703, 0.9625000000000000222, 0.9666666666666666741, 0.9708333333333333259, 0.9749999999999999778, 0.9791666666666666297, 0.9833333333333332815, 0.9875000000000000444, 0.9916666666666666963, 0.9958333333333333481, 1.000000000000000000 ),
 .UNSPECIFIED. ) 
 GEOMETRIC_REPRESENTATION_ITEM ( )  RATIONAL_B_SPLINE_SURFACE ( (
 ( 1.000000000000000000, 0.8660254037844387076, 1.000000000000000000, 0.8660254037844387076, 1.000000000000000000, 0.8660254037844387076, 1.000000000000000000, 0.8660254037844387076, 1.000000000000000000, 0.8660254037844387076, 1.000000000000000000, 0.8660254037844387076, 1.000000000000000000, 0.8660254037844387076, 1.000000000000000000, 0.8660254037844387076, 1.000000000000000000, 0.8660254037844387076, 1.000000000000000000, 0.8660254037844387076, 1.000000000000000000, 0.8660254037844387076, 1.000000000000000000, 0.8660254037844387076, 1.000000000000000000, 0.8660254037844387076, 1.000000000000000000, 0.8660254037844387076, 1.000000000000000000, 0.8660254037844387076, 1.000000000000000000, 0.8660254037844387076, 1.000000000000000000, 0.8660254037844387076, 1.000000000000000000, 0.8660254037844387076, 1.000000000000000000, 0.8660254037844387076, 1.000000000000000000, 0.8660254037844387076, 1.000000000000000000, 0.8660254037844387076, 1.000000000000000000, 0.8660254037844387076, 1.000000000000000000, 0.8660254037844387076, 1.000000000000000000, 0.8660254037844387076, 1.000000000000000000, 0.8660254037844387076, 1.000000000000000000, 0.8660254037844387076, 1.000000000000000000, 0.8660254037844387076, 1.000000000000000000, 0.8660254037844387076, 1.000000000000000000, 0.8660254037844387076, 1.000000000000000000, 0.8660254037844387076, 1.000000000000000000, 0.8660254037844387076, 1.000000000000000000, 0.8660254037844387076, 1.000000000000000000, 0.8660254037844387076, 1.000000000000000000, 0.8660254037844387076, 1.000000000000000000, 0.8660254037844387076, 1.000000000000000000, 0.8660254037844387076, 1.000000000000000000, 0.8660254037844387076, 1.000000000000000000, 0.8660254037844387076, 1.000000000000000000, 0.8660254037844387076, 1.000000000000000000, 0.8660254037844387076, 1.000000000000000000, 0.8660254037844387076, 1.000000000000000000, 0.8660254037844387076, 1.000000000000000000, 0.8660254037844387076, 1.000000000000000000, 0.8660254037844387076, 1.000000000000000000, 0.8660254037844387076, 1.000000000000000000, 0.8660254037844387076, 1.000000000000000000, 0.8660254037844387076, 1.000000000000000000, 0.8660254037844387076, 1.000000000000000000, 0.8660254037844387076, 1.000000000000000000, 0.8660254037844387076, 1.000000000000000000, 0.8660254037844387076, 1.000000000000000000, 0.8660254037844387076, 1.000000000000000000, 0.8660254037844387076, 1.000000000000000000, 0.8660254037844387076, 1.000000000000000000, 0.8660254037844387076, 1.000000000000000000, 0.8660254037844387076, 1.000000000000000000, 0.8660254037844387076, 1.000000000000000000, 0.8660254037844387076, 1.000000000000000000, 0.8660254037844387076, 1.000000000000000000, 0.8660254037844387076, 1.000000000000000000, 0.8660254037844387076, 1.000000000000000000, 0.8660254037844387076, 1.000000000000000000, 0.8660254037844387076, 1.000000000000000000, 0.8660254037844387076, 1.000000000000000000, 0.8660254037844387076, 1.000000000000000000, 0.8660254037844387076, 1.000000000000000000, 0.8660254037844387076, 1.000000000000000000, 0.8660254037844387076, 1.000000000000000000, 0.8660254037844387076, 1.000000000000000000, 0.8660254037844387076, 1.000000000000000000, 0.8660254037844387076, 1.000000000000000000, 0.8660254037844387076, 1.000000000000000000, 0.8660254037844387076, 1.000000000000000000, 0.8660254037844387076, 1.000000000000000000, 0.8660254037844387076, 1.000000000000000000, 0.8660254037844387076, 1.000000000000000000, 0.8660254037844387076, 1.000000000000000000, 0.8660254037844387076, 1.000000000000000000, 0.8660254037844387076, 1.000000000000000000, 0.8660254037844387076, 1.000000000000000000, 0.8660254037844387076, 1.000000000000000000, 0.8660254037844387076, 1.000000000000000000, 0.8660254037844387076, 1.000000000000000000, 0.8660254037844387076, 1.000000000000000000, 0.8660254037844387076, 1.000000000000000000, 0.8660254037844387076, 1.000000000000000000, 0.8660254037844387076, 1.000000000000000000, 0.8660254037844387076, 1.000000000000000000, 0.8660254037844387076, 1.000000000000000000, 0.8660254037844387076, 1.000000000000000000, 0.8660254037844387076, 1.000000000000000000, 0.8660254037844387076, 1.000000000000000000, 0.8660254037844387076, 1.000000000000000000, 0.8660254037844387076, 1.000000000000000000, 0.8660254037844387076, 1.000000000000000000, 0.8660254037844387076, 1.000000000000000000, 0.8660254037844387076, 1.000000000000000000, 0.8660254037844387076, 1.000000000000000000, 0.8660254037844387076, 1.000000000000000000, 0.8660254037844387076, 1.000000000000000000, 0.8660254037844387076, 1.000000000000000000, 0.8660254037844387076, 1.000000000000000000, 0.8660254037844387076, 1.000000000000000000, 0.8660254037844387076, 1.000000000000000000, 0.8660254037844387076, 1.000000000000000000, 0.8660254037844387076, 1.000000000000000000, 0.8660254037844387076, 1.000000000000000000, 0.8660254037844387076, 1.000000000000000000, 0.8660254037844387076, 1.000000000000000000, 0.8660254037844387076, 1.000000000000000000, 0.8660254037844387076, 1.000000000000000000, 0.8660254037844387076, 1.000000000000000000, 0.8660254037844387076, 1.000000000000000000, 0.8660254037844387076, 1.000000000000000000, 0.8660254037844387076, 1.000000000000000000, 0.8660254037844387076, 1.000000000000000000, 0.8660254037844387076, 1.000000000000000000, 0.8660254037844387076, 1.000000000000000000, 0.8660254037844387076, 1.000000000000000000, 0.8660254037844387076, 1.000000000000000000, 0.8660254037844387076, 1.000000000000000000, 0.8660254037844387076, 1.000000000000000000, 0.8660254037844387076, 1.000000000000000000, 0.8660254037844387076, 1.000000000000000000, 0.8660254037844387076, 1.000000000000000000, 0.8660254037844387076, 1.000000000000000000, 0.8660254037844387076, 1.000000000000000000, 0.8660254037844387076, 1.000000000000000000, 0.8660254037844387076, 1.000000000000000000, 0.8660254037844387076, 1.000000000000000000, 0.8660254037844387076, 1.000000000000000000, 0.8660254037844387076, 1.000000000000000000, 0.8660254037844387076, 1.000000000000000000, 0.8660254037844387076, 1.000000000000000000, 0.8660254037844387076, 1.000000000000000000, 0.8660254037844387076, 1.000000000000000000, 0.8660254037844387076, 1.000000000000000000, 0.8660254037844387076, 1.000000000000000000, 0.8660254037844387076, 1.000000000000000000, 0.8660254037844387076, 1.000000000000000000, 0.8660254037844387076, 1.000000000000000000, 0.8660254037844387076, 1.000000000000000000, 0.8660254037844387076, 1.000000000000000000, 0.8660254037844387076, 1.000000000000000000, 0.8660254037844387076, 1.000000000000000000, 0.8660254037844387076, 1.000000000000000000, 0.8660254037844387076, 1.000000000000000000, 0.8660254037844387076, 1.000000000000000000, 0.8660254037844387076, 1.000000000000000000, 0.8660254037844387076, 1.000000000000000000, 0.8660254037844387076, 1.000000000000000000, 0.8660254037844387076, 1.000000000000000000, 0.8660254037844387076, 1.000000000000000000, 0.8660254037844387076, 1.000000000000000000, 0.8660254037844387076, 1.000000000000000000, 0.8660254037844387076, 1.000000000000000000, 0.8660254037844387076, 1.000000000000000000, 0.8660254037844387076, 1.000000000000000000, 0.8660254037844387076, 1.000000000000000000, 0.8660254037844387076, 1.000000000000000000, 0.8660254037844387076, 1.000000000000000000, 0.8660254037844387076, 1.000000000000000000, 0.8660254037844387076, 1.000000000000000000, 0.8660254037844387076, 1.000000000000000000, 0.8660254037844387076, 1.000000000000000000, 0.8660254037844387076, 1.000000000000000000, 0.8660254037844387076, 1.000000000000000000, 0.8660254037844387076, 1.000000000000000000, 0.8660254037844387076, 1.000000000000000000, 0.8660254037844387076, 1.000000000000000000, 0.8660254037844387076, 1.000000000000000000, 0.8660254037844387076, 1.000000000000000000, 0.8660254037844387076, 1.000000000000000000, 0.8660254037844387076, 1.000000000000000000, 0.8660254037844387076, 1.000000000000000000, 0.8660254037844387076, 1.000000000000000000, 0.8660254037844387076, 1.000000000000000000, 0.8660254037844387076, 1.000000000000000000, 0.8660254037844387076, 1.000000000000000000, 0.8660254037844387076, 1.000000000000000000, 0.8660254037844387076, 1.000000000000000000, 0.8660254037844387076, 1.000000000000000000, 0.8660254037844387076, 1.000000000000000000, 0.8660254037844387076, 1.000000000000000000, 0.8660254037844387076, 1.000000000000000000, 0.8660254037844387076, 1.000000000000000000, 0.8660254037844387076, 1.000000000000000000, 0.8660254037844387076, 1.000000000000000000, 0.8660254037844387076, 1.000000000000000000, 0.8660254037844387076, 1.000000000000000000, 0.8660254037844387076, 1.000000000000000000, 0.8660254037844387076, 1.000000000000000000, 0.8660254037844387076, 1.000000000000000000, 0.8660254037844387076, 1.000000000000000000, 0.8660254037844387076, 1.000000000000000000, 0.8660254037844387076, 1.000000000000000000, 0.8660254037844387076, 1.000000000000000000, 0.8660254037844387076, 1.000000000000000000, 0.8660254037844387076, 1.000000000000000000, 0.8660254037844387076, 1.000000000000000000, 0.8660254037844387076, 1.000000000000000000, 0.8660254037844387076, 1.000000000000000000, 0.8660254037844387076, 1.000000000000000000, 0.8660254037844387076, 1.000000000000000000, 0.8660254037844387076, 1.000000000000000000, 0.8660254037844387076, 1.000000000000000000, 0.8660254037844387076, 1.000000000000000000, 0.8660254037844387076, 1.000000000000000000, 0.8660254037844387076, 1.000000000000000000, 0.8660254037844387076, 1.000000000000000000, 0.8660254037844387076, 1.000000000000000000, 0.8660254037844387076, 1.000000000000000000, 0.8660254037844387076, 1.000000000000000000, 0.8660254037844387076, 1.000000000000000000, 0.8660254037844387076, 1.000000000000000000, 0.8660254037844387076, 1.000000000000000000, 0.8660254037844387076, 1.000000000000000000, 0.8660254037844387076, 1.000000000000000000, 0.8660254037844387076, 1.000000000000000000, 0.8660254037844387076, 1.000000000000000000, 0.8660254037844387076, 1.000000000000000000, 0.8660254037844387076, 1.000000000000000000, 0.8660254037844387076, 1.000000000000000000, 0.8660254037844387076, 1.000000000000000000, 0.8660254037844387076, 1.000000000000000000, 0.8660254037844387076, 1.000000000000000000, 0.8660254037844387076, 1.000000000000000000, 0.8660254037844387076, 1.000000000000000000, 0.8660254037844387076, 1.000000000000000000, 0.8660254037844387076, 1.000000000000000000, 0.8660254037844387076, 1.000000000000000000, 0.8660254037844387076, 1.000000000000000000, 0.8660254037844387076, 1.000000000000000000, 0.8660254037844387076, 1.000000000000000000, 0.8660254037844387076, 1.000000000000000000, 0.8660254037844387076, 1.000000000000000000, 0.8660254037844387076, 1.000000000000000000, 0.8660254037844387076, 1.000000000000000000, 0.8660254037844387076, 1.000000000000000000, 0.8660254037844387076, 1.000000000000000000),
 ( 1.000000000000000000, 0.8660254037844387076, 1.000000000000000000, 0.8660254037844387076, 1.000000000000000000, 0.8660254037844387076, 1.000000000000000000, 0.8660254037844387076, 1.000000000000000000, 0.8660254037844387076, 1.000000000000000000, 0.8660254037844387076, 1.000000000000000000, 0.8660254037844387076, 1.000000000000000000, 0.8660254037844387076, 1.000000000000000000, 0.8660254037844387076, 1.000000000000000000, 0.8660254037844387076, 1.000000000000000000, 0.8660254037844387076, 1.000000000000000000, 0.8660254037844387076, 1.000000000000000000, 0.8660254037844387076, 1.000000000000000000, 0.8660254037844387076, 1.000000000000000000, 0.8660254037844387076, 1.000000000000000000, 0.8660254037844387076, 1.000000000000000000, 0.8660254037844387076, 1.000000000000000000, 0.8660254037844387076, 1.000000000000000000, 0.8660254037844387076, 1.000000000000000000, 0.8660254037844387076, 1.000000000000000000, 0.8660254037844387076, 1.000000000000000000, 0.8660254037844387076, 1.000000000000000000, 0.8660254037844387076, 1.000000000000000000, 0.8660254037844387076, 1.000000000000000000, 0.8660254037844387076, 1.000000000000000000, 0.8660254037844387076, 1.000000000000000000, 0.8660254037844387076, 1.000000000000000000, 0.8660254037844387076, 1.000000000000000000, 0.8660254037844387076, 1.000000000000000000, 0.8660254037844387076, 1.000000000000000000, 0.8660254037844387076, 1.000000000000000000, 0.8660254037844387076, 1.000000000000000000, 0.8660254037844387076, 1.000000000000000000, 0.8660254037844387076, 1.000000000000000000, 0.8660254037844387076, 1.000000000000000000, 0.8660254037844387076, 1.000000000000000000, 0.8660254037844387076, 1.000000000000000000, 0.8660254037844387076, 1.000000000000000000, 0.8660254037844387076, 1.000000000000000000, 0.8660254037844387076, 1.000000000000000000, 0.8660254037844387076, 1.000000000000000000, 0.8660254037844387076, 1.000000000000000000, 0.8660254037844387076, 1.000000000000000000, 0.8660254037844387076, 1.000000000000000000, 0.8660254037844387076, 1.000000000000000000, 0.8660254037844387076, 1.000000000000000000, 0.8660254037844387076, 1.000000000000000000, 0.8660254037844387076, 1.000000000000000000, 0.8660254037844387076, 1.000000000000000000, 0.8660254037844387076, 1.000000000000000000, 0.8660254037844387076, 1.000000000000000000, 0.8660254037844387076, 1.000000000000000000, 0.8660254037844387076, 1.000000000000000000, 0.8660254037844387076, 1.000000000000000000, 0.8660254037844387076, 1.000000000000000000, 0.8660254037844387076, 1.000000000000000000, 0.8660254037844387076, 1.000000000000000000, 0.8660254037844387076, 1.000000000000000000, 0.8660254037844387076, 1.000000000000000000, 0.8660254037844387076, 1.000000000000000000, 0.8660254037844387076, 1.000000000000000000, 0.8660254037844387076, 1.000000000000000000, 0.8660254037844387076, 1.000000000000000000, 0.8660254037844387076, 1.000000000000000000, 0.8660254037844387076, 1.000000000000000000, 0.8660254037844387076, 1.000000000000000000, 0.8660254037844387076, 1.000000000000000000, 0.8660254037844387076, 1.000000000000000000, 0.8660254037844387076, 1.000000000000000000, 0.8660254037844387076, 1.000000000000000000, 0.8660254037844387076, 1.000000000000000000, 0.8660254037844387076, 1.000000000000000000, 0.8660254037844387076, 1.000000000000000000, 0.8660254037844387076, 1.000000000000000000, 0.8660254037844387076, 1.000000000000000000, 0.8660254037844387076, 1.000000000000000000, 0.8660254037844387076, 1.000000000000000000, 0.8660254037844387076, 1.000000000000000000, 0.8660254037844387076, 1.000000000000000000, 0.8660254037844387076, 1.000000000000000000, 0.8660254037844387076, 1.000000000000000000, 0.8660254037844387076, 1.000000000000000000, 0.8660254037844387076, 1.000000000000000000, 0.8660254037844387076, 1.000000000000000000, 0.8660254037844387076, 1.000000000000000000, 0.8660254037844387076, 1.000000000000000000, 0.8660254037844387076, 1.000000000000000000, 0.8660254037844387076, 1.000000000000000000, 0.8660254037844387076, 1.000000000000000000, 0.8660254037844387076, 1.000000000000000000, 0.8660254037844387076, 1.000000000000000000, 0.8660254037844387076, 1.000000000000000000, 0.8660254037844387076, 1.000000000000000000, 0.8660254037844387076, 1.000000000000000000, 0.8660254037844387076, 1.000000000000000000, 0.8660254037844387076, 1.000000000000000000, 0.8660254037844387076, 1.000000000000000000, 0.8660254037844387076, 1.000000000000000000, 0.8660254037844387076, 1.000000000000000000, 0.8660254037844387076, 1.000000000000000000, 0.8660254037844387076, 1.000000000000000000, 0.8660254037844387076, 1.000000000000000000, 0.8660254037844387076, 1.000000000000000000, 0.8660254037844387076, 1.000000000000000000, 0.8660254037844387076, 1.000000000000000000, 0.8660254037844387076, 1.000000000000000000, 0.8660254037844387076, 1.000000000000000000, 0.8660254037844387076, 1.000000000000000000, 0.8660254037844387076, 1.000000000000000000, 0.8660254037844387076, 1.000000000000000000, 0.8660254037844387076, 1.000000000000000000, 0.8660254037844387076, 1.000000000000000000, 0.8660254037844387076, 1.000000000000000000, 0.8660254037844387076, 1.000000000000000000, 0.8660254037844387076, 1.000000000000000000, 0.8660254037844387076, 1.000000000000000000, 0.8660254037844387076, 1.000000000000000000, 0.8660254037844387076, 1.000000000000000000, 0.8660254037844387076, 1.000000000000000000, 0.8660254037844387076, 1.000000000000000000, 0.8660254037844387076, 1.000000000000000000, 0.8660254037844387076, 1.000000000000000000, 0.8660254037844387076, 1.000000000000000000, 0.8660254037844387076, 1.000000000000000000, 0.8660254037844387076, 1.000000000000000000, 0.8660254037844387076, 1.000000000000000000, 0.8660254037844387076, 1.000000000000000000, 0.8660254037844387076, 1.000000000000000000, 0.8660254037844387076, 1.000000000000000000, 0.8660254037844387076, 1.000000000000000000, 0.8660254037844387076, 1.000000000000000000, 0.8660254037844387076, 1.000000000000000000, 0.8660254037844387076, 1.000000000000000000, 0.8660254037844387076, 1.000000000000000000, 0.8660254037844387076, 1.000000000000000000, 0.8660254037844387076, 1.000000000000000000, 0.8660254037844387076, 1.000000000000000000, 0.8660254037844387076, 1.000000000000000000, 0.8660254037844387076, 1.000000000000000000, 0.8660254037844387076, 1.000000000000000000, 0.8660254037844387076, 1.000000000000000000, 0.8660254037844387076, 1.000000000000000000, 0.8660254037844387076, 1.000000000000000000, 0.8660254037844387076, 1.000000000000000000, 0.8660254037844387076, 1.000000000000000000, 0.8660254037844387076, 1.000000000000000000, 0.8660254037844387076, 1.000000000000000000, 0.8660254037844387076, 1.000000000000000000, 0.8660254037844387076, 1.000000000000000000, 0.8660254037844387076, 1.000000000000000000, 0.8660254037844387076, 1.000000000000000000, 0.8660254037844387076, 1.000000000000000000, 0.8660254037844387076, 1.000000000000000000, 0.8660254037844387076, 1.000000000000000000, 0.8660254037844387076, 1.000000000000000000, 0.8660254037844387076, 1.000000000000000000, 0.8660254037844387076, 1.000000000000000000, 0.8660254037844387076, 1.000000000000000000, 0.8660254037844387076, 1.000000000000000000, 0.8660254037844387076, 1.000000000000000000, 0.8660254037844387076, 1.000000000000000000, 0.8660254037844387076, 1.000000000000000000, 0.8660254037844387076, 1.000000000000000000, 0.8660254037844387076, 1.000000000000000000, 0.8660254037844387076, 1.000000000000000000, 0.8660254037844387076, 1.000000000000000000, 0.8660254037844387076, 1.000000000000000000, 0.8660254037844387076, 1.000000000000000000, 0.8660254037844387076, 1.000000000000000000, 0.8660254037844387076, 1.000000000000000000, 0.8660254037844387076, 1.000000000000000000, 0.8660254037844387076, 1.000000000000000000, 0.8660254037844387076, 1.000000000000000000, 0.8660254037844387076, 1.000000000000000000, 0.8660254037844387076, 1.000000000000000000, 0.8660254037844387076, 1.000000000000000000, 0.8660254037844387076, 1.000000000000000000, 0.8660254037844387076, 1.000000000000000000, 0.8660254037844387076, 1.000000000000000000, 0.8660254037844387076, 1.000000000000000000, 0.8660254037844387076, 1.000000000000000000, 0.8660254037844387076, 1.000000000000000000, 0.8660254037844387076, 1.000000000000000000, 0.8660254037844387076, 1.000000000000000000, 0.8660254037844387076, 1.000000000000000000, 0.8660254037844387076, 1.000000000000000000, 0.8660254037844387076, 1.000000000000000000, 0.8660254037844387076, 1.000000000000000000, 0.8660254037844387076, 1.000000000000000000, 0.8660254037844387076, 1.000000000000000000, 0.8660254037844387076, 1.000000000000000000, 0.8660254037844387076, 1.000000000000000000, 0.8660254037844387076, 1.000000000000000000, 0.8660254037844387076, 1.000000000000000000, 0.8660254037844387076, 1.000000000000000000, 0.8660254037844387076, 1.000000000000000000, 0.8660254037844387076, 1.000000000000000000, 0.8660254037844387076, 1.000000000000000000, 0.8660254037844387076, 1.000000000000000000, 0.8660254037844387076, 1.000000000000000000, 0.8660254037844387076, 1.000000000000000000, 0.8660254037844387076, 1.000000000000000000, 0.8660254037844387076, 1.000000000000000000, 0.8660254037844387076, 1.000000000000000000, 0.8660254037844387076, 1.000000000000000000, 0.8660254037844387076, 1.000000000000000000, 0.8660254037844387076, 1.000000000000000000, 0.8660254037844387076, 1.000000000000000000, 0.8660254037844387076, 1.000000000000000000, 0.8660254037844387076, 1.000000000000000000, 0.8660254037844387076, 1.000000000000000000, 0.8660254037844387076, 1.000000000000000000, 0.8660254037844387076, 1.000000000000000000, 0.8660254037844387076, 1.000000000000000000, 0.8660254037844387076, 1.000000000000000000, 0.8660254037844387076, 1.000000000000000000, 0.8660254037844387076, 1.000000000000000000, 0.8660254037844387076, 1.000000000000000000, 0.8660254037844387076, 1.000000000000000000, 0.8660254037844387076, 1.000000000000000000, 0.8660254037844387076, 1.000000000000000000, 0.8660254037844387076, 1.000000000000000000, 0.8660254037844387076, 1.000000000000000000, 0.8660254037844387076, 1.000000000000000000, 0.8660254037844387076, 1.000000000000000000, 0.8660254037844387076, 1.000000000000000000, 0.8660254037844387076, 1.000000000000000000, 0.8660254037844387076, 1.000000000000000000, 0.8660254037844387076, 1.000000000000000000, 0.8660254037844387076, 1.000000000000000000, 0.8660254037844387076, 1.000000000000000000, 0.8660254037844387076, 1.000000000000000000, 0.8660254037844387076, 1.000000000000000000, 0.8660254037844387076, 1.000000000000000000, 0.8660254037844387076, 1.000000000000000000, 0.8660254037844387076, 1.000000000000000000, 0.8660254037844387076, 1.000000000000000000, 0.8660254037844387076, 1.000000000000000000, 0.8660254037844387076, 1.000000000000000000, 0.8660254037844387076, 1.000000000000000000) ) ) 
 REPRESENTATION_ITEM ( '' )  SURFACE ( )  );
#75162 = CARTESIAN_POINT ( 'NONE',  ( -7.065207446497166366, 9.336104335703744539, 0.000000000000000000 ) ) ;
#75165 = CARTESIAN_POINT ( 'NONE',  ( 5.665250009225348826, 1.861346387706263261, -0.7762253298396750711 ) ) ;
#75164 = CARTESIAN_POINT ( 'NONE',  ( 5.865807274569020180, 1.797851641234180509, -0.3166982042408575948 ) ) ;
#75166 = CARTESIAN_POINT ( 'NONE',  ( 6.727182134110231360, 6.039168392632435989, 2.405853653942996218 ) ) ;
#75167 = CARTESIAN_POINT ( 'NONE',  ( 1.574760213118006735, 1.391939136705011348, -1.532762857463897843 ) ) ;
#75168 = CARTESIAN_POINT ( 'NONE',  ( -7.562750758324527922, 7.717630727667075696, 1.040834085586084257E-14 ) ) ;
#75169 = CARTESIAN_POINT ( 'NONE',  ( -5.872679487624441030, 7.188158700483015195, -1.149102218512105145 ) ) ;
#75170 = CARTESIAN_POINT ( 'NONE',  ( 1.244123718695673952, 2.848244533904600750, -0.7749999999999926947 ) ) ;
#75171 = CARTESIAN_POINT ( 'NONE',  ( 1.642778471875000035, -2.676041666188708756, -2.845375778867859751 ) ) ;
#75172 = CARTESIAN_POINT ( 'NONE',  ( 5.286789834324991055, 8.255339675766103724, -1.199719254218452935 ) ) ;
#75173 = CARTESIAN_POINT ( 'NONE',  ( 4.879147978569815969, 4.879180288469956217, -0.1512534140984626019 ) ) ;
#75174 = CARTESIAN_POINT ( 'NONE',  ( 4.340018570150304456, 6.156717313299049366, -1.443375672974068769 ) ) ;
#75175 = CARTESIAN_POINT ( 'NONE',  ( 0.000000000000000000, -0.4330127018922214077, 0.000000000000000000 ) ) ;
#75176 = CARTESIAN_POINT ( 'NONE',  ( -1.402160292154681736E-14, 11.73437500034140335, 1.575800808251682339 ) ) ;
#75178 = CARTESIAN_POINT ( 'NONE',  ( -6.469175572376043348, 7.576401584974034265, 1.199719254218452047 ) ) ;
#75177 = CARTESIAN_POINT ( 'NONE',  ( 6.925078400183574345, 6.038986730273901316, 2.350556043039519150 ) ) ;
#75179 = CARTESIAN_POINT ( 'NONE',  ( 4.887242738553729815, -0.5912784195612891258, -1.630374673469140223 ) ) ;
#75180 = CARTESIAN_POINT ( 'NONE',  ( -4.741601036477307574, 6.554953847355395880, 1.599625672291267398 ) ) ;
#75181 = CARTESIAN_POINT ( 'NONE',  ( 2.729418486472269922, 0.1060373921930452268, -2.067687848736274869 ) ) ;
#75182 = CARTESIAN_POINT ( 'NONE',  ( 3.181382749799996468, 1.670748044588391990, 1.300414933884207480 ) ) ;
#75183 = CARTESIAN_POINT ( 'NONE',  ( 5.913327553854682783, 10.05063257947248800, -0.7998128361456291469 ) ) ;
#75184 = CARTESIAN_POINT ( 'NONE',  ( 0.08058608058607655278, -9.900000000000005684, 10.99970480893082225 ) ) ;
#75185 = CARTESIAN_POINT ( 'NONE',  ( 1.885543262503614592, -1.856164082770836110, 0.6587638493158411990 ) ) ;
#75186 = CARTESIAN_POINT ( 'NONE',  ( 6.108949960370312127, 6.019453914259918825, -0.1454340903971618193 ) ) ;
#75188 = CARTESIAN_POINT ( 'NONE',  ( 11.89829993707161471, 12.27080771748874177, -1.561606677374349772 ) ) ;
#75187 = CARTESIAN_POINT ( 'NONE',  ( 0.000000000000000000, -1.837499999999999911, -4.012584370867899430 ) ) ;
#75189 = CARTESIAN_POINT ( 'NONE',  ( 4.172042307184393728, -1.321354948109268346, 1.872925066384116377 ) ) ;
#75190 = CARTESIAN_POINT ( 'NONE',  ( 1.752308680507021155, 0.5713779359179693706, 1.734036872924920702 ) ) ;
#75191 = CARTESIAN_POINT ( 'NONE',  ( 5.692444392891300886, 7.734547439830227411, -1.599625672291281386 ) ) ;
#75192 = CARTESIAN_POINT ( 'NONE',  ( 5.287316719205157334, 9.112360572473935605, 1.040834085586084257E-14 ) ) ;
#75193 = CARTESIAN_POINT ( 'NONE',  ( -8.290974629956718189, 9.631557475493025322, -1.199719254218446718 ) ) ;
#75194 = CARTESIAN_POINT ( 'NONE',  ( 2.601816991827472947, 1.426658649466717943, 1.420685320369071025 ) ) ;
#75195 = CARTESIAN_POINT ( 'NONE',  ( 1.885527806591394961, -1.848987351811198998, 0.6559936482007987513 ) ) ;
#75196 = CARTESIAN_POINT ( 'NONE',  ( -8.483651433849100698, 10.92067931095586886, 1.599625672291269396 ) ) ;
#75197 = VECTOR ( 'NONE', #99739, 1000.000000000000000 ) ;
#75198 = CARTESIAN_POINT ( 'NONE',  ( -6.898401231254901234, 6.942556279419168419, -0.7998128361456291469 ) ) ;
#75199 = CARTESIAN_POINT ( 'NONE',  ( -3.578989363883261277, 7.119311991265024453, 1.040834085586084257E-14 ) ) ;
#75201 = CARTESIAN_POINT ( 'NONE',  ( 4.223360090310752213, -1.693420319160190646, 0.5144795390387302270 ) ) ;
#75200 = CARTESIAN_POINT ( 'NONE',  ( 4.505862177948306346, -0.8935697331868618365, -1.890194782795044492 ) ) ;
#75202 = CARTESIAN_POINT ( 'NONE',  ( -9.898321827459618305, 15.00000000000623857, 7.924999999990495425 ) ) ;
#75203 = CARTESIAN_POINT ( 'NONE',  ( 0.4807640440005828131, -0.2721776580492247799, -2.174417363000572756 ) ) ;
#75204 = CARTESIAN_POINT ( 'NONE',  ( 5.472502228039195060, -0.04848951148075366507, -1.739831344048385908 ) ) ;
#75205 = ADVANCED_FACE ( 'NONE', ( #182025 ), #87149, .F. ) ;
#75206 = CARTESIAN_POINT ( 'NONE',  ( 6.740374924288304648, 11.01552117831172062, 1.040834085586084257E-14 ) ) ;
#75207 = CARTESIAN_POINT ( 'NONE',  ( 5.994848186622900421, -2.281820642442307090, 0.2777966721622132096 ) ) ;
#75208 = CARTESIAN_POINT ( 'NONE',  ( 2.970662972610667918, 6.571530881558488524, 0.4515752934304059218 ) ) ;
#75209 = CARTESIAN_POINT ( 'NONE',  ( 5.694640849732851784, -1.102317705797692726, -1.338331167630167684 ) ) ;
#75210 = CARTESIAN_POINT ( 'NONE',  ( 6.232918786939658062, -2.059688491082920070, -0.6869823432723211054 ) ) ;
#75211 = CARTESIAN_POINT ( 'NONE',  ( -1.225000000000018074, 2.979166666666678065, -0.7072540797572998139 ) ) ;
#75212 = CARTESIAN_POINT ( 'NONE',  ( 0.2865162857260491469, -0.7196341243457348158, -1.991407047551809750 ) ) ;
#75213 = CARTESIAN_POINT ( 'NONE',  ( 3.593750000000001776, -1.895863743164161841, -0.7852924748297959168 ) ) ;
#75214 = CARTESIAN_POINT ( 'NONE',  ( 6.827182134110205247, 2.955377424523279117, 2.541486622063714673 ) ) ;
#75215 = CARTESIAN_POINT ( 'NONE',  ( 4.858382476810707118, 0.7369543258428765675, 1.780043821814878413 ) ) ;
#75216 = CARTESIAN_POINT ( 'NONE',  ( -1.500000000000015099, 10.76041666734946389, -0.8660254037844309360 ) ) ;
#75217 = CARTESIAN_POINT ( 'NONE',  ( 1.770501988737150922, 2.215049892327343173, -0.1675478377428234744 ) ) ;
#75218 = ORIENTED_EDGE ( 'NONE', *, *, #55286, .T. ) ;
#75219 = CARTESIAN_POINT ( 'NONE',  ( -1.500000000000011324, 3.920833333333357817, 0.8660254037844403729 ) ) ;
#75220 = CARTESIAN_POINT ( 'NONE',  ( 5.495132332240461714, 5.305409230568988832, 0.7998128361456341429 ) ) ;
#75221 = CARTESIAN_POINT ( 'NONE',  ( 5.957918438201454059, 9.038323046955323292, -1.199719254218440723 ) ) ;
#75222 = ADVANCED_FACE ( 'NONE', ( #102928 ), #1134, .T. ) ;
#75223 = CARTESIAN_POINT ( 'NONE',  ( 2.666879960053496479, 0.7507478997158049117, 2.090701262698462681 ) ) ;
#75224 = CARTESIAN_POINT ( 'NONE',  ( 6.236387472606139681, 8.298871356172400127, -1.443375672974057666 ) ) ;
#75225 = ADVANCED_FACE ( 'NONE', ( #105084 ), #26993, .F. ) ;
#75226 = CARTESIAN_POINT ( 'NONE',  ( -9.503902493055310430, 11.15060299906175167, 1.082531754730558626 ) ) ;
#75227 = CARTESIAN_POINT ( 'NONE',  ( 7.051649292883499953, 7.399548061218447437, -0.7216878364870317197 ) ) ;
#75228 = AXIS2_PLACEMENT_3D ( 'NONE', #104478, #103401, #173765 ) ;
#75229 = CARTESIAN_POINT ( 'NONE',  ( 1.178361531996233280, 1.528742360773158282, 1.314995429398260196 ) ) ;
#75231 = CARTESIAN_POINT ( 'NONE',  ( 6.877413164483755281, -0.1458786163922053403, 2.030295828278828374 ) ) ;
#75230 = CARTESIAN_POINT ( 'NONE',  ( 8.378048858240820351, 11.86180853700128601, -1.199719254218446718 ) ) ;
#75232 = CARTESIAN_POINT ( 'NONE',  ( 5.682275777458829502, 9.643422483761748154, 0.7216878364870317197 ) ) ;
#75233 = CARTESIAN_POINT ( 'NONE',  ( -2.093795543908766543, 0.9691415390508352212, 11.71227324440729234 ) ) ;
#75234 = CARTESIAN_POINT ( 'NONE',  ( -1.364683531250014514, 0.7385416670080887647, -0.7879004041258289570 ) ) ;
#75235 = CARTESIAN_POINT ( 'NONE',  ( 0.8601951712396675997, -1.287299901140761316, 1.214705651989380852 ) ) ;
#75236 = CARTESIAN_POINT ( 'NONE',  ( 0.4400775573648734174, -1.704940109561555950, -1.076314675215600314 ) ) ;
#75237 = CARTESIAN_POINT ( 'NONE',  ( 5.231891002347484054, 1.715934187082169604, 0.2900348964059005774 ) ) ;
#75238 = CARTESIAN_POINT ( 'NONE',  ( 4.001757606804694056, -2.286216240038071668, 0.1689928914557006778 ) ) ;
#75239 = CARTESIAN_POINT ( 'NONE',  ( 1.364683531249988757, -0.8656249996585805295, 0.000000000000000000 ) ) ;
#75240 = CARTESIAN_POINT ( 'NONE',  ( 1.886409237429786279, 1.602333580200336671, -0.9066872629178088783 ) ) ;
#75241 = CARTESIAN_POINT ( 'NONE',  ( 10.57266086055835075, 11.22919251360659310, 0.000000000000000000 ) ) ;
#75242 = CARTESIAN_POINT ( 'NONE',  ( 2.766400663125650361, -1.260407102598060103, 1.320874842943790872 ) ) ;
#75243 = CARTESIAN_POINT ( 'NONE',  ( 4.360000113718985659, -0.002809843368253156070, -2.016597020062675050 ) ) ;
#75244 = CARTESIAN_POINT ( 'NONE',  ( -9.829825065107822724, 11.42688298316931572, 1.199719254218462483 ) ) ;
#75246 = CARTESIAN_POINT ( 'NONE',  ( 0.000000000000000000, 4.500000000000003553, 0.000000000000000000 ) ) ;
#75245 = CARTESIAN_POINT ( 'NONE',  ( 2.325404209529509103, -2.741642530189327160E-05, 2.262689075223401236 ) ) ;
#75247 = CARTESIAN_POINT ( 'NONE',  ( 5.737368847912779124, -1.905360455185100887, 0.8973202462331535401 ) ) ;
#75248 = CARTESIAN_POINT ( 'NONE',  ( -11.86239285000045918, 13.88000000000000078, -1.812080536912752837 ) ) ;
#75249 = CARTESIAN_POINT ( 'NONE',  ( 2.770052221688572125, -2.048192801557855436, 0.3012726569043902569 ) ) ;
#75250 = CARTESIAN_POINT ( 'NONE',  ( 3.680148631105580215, 6.380924938676771241, -1.199719254218446718 ) ) ;
#75251 = CARTESIAN_POINT ( 'NONE',  ( -1.360316468750044860, 1.151041667008095404, -0.7853790794159261068 ) ) ;
#75252 = CARTESIAN_POINT ( 'NONE',  ( 4.231183009085410340, 1.939187816756043237, 0.8583030597293441755 ) ) ;
#75253 = CARTESIAN_POINT ( 'NONE',  ( 0.6274103741727736772, -1.829744589303895275, 0.6030480328435404713 ) ) ;
#75254 = CARTESIAN_POINT ( 'NONE',  ( -3.817502770699643388, 6.611447778194983194, 1.199719254218452935 ) ) ;
#75255 = CARTESIAN_POINT ( 'NONE',  ( 8.934986926605834157, 10.38290515491702770, -1.199719254218446718 ) ) ;
#75256 = CARTESIAN_POINT ( 'NONE',  ( 4.977251789548238214, 7.860525283564661514, -1.082531754730548412 ) ) ;
#75257 = CARTESIAN_POINT ( 'NONE',  ( 4.388421827844267042, 7.126904390760538277, 1.074283327121795528 ) ) ;
#75258 = CARTESIAN_POINT ( 'NONE',  ( -3.474999999999998312, -0.6270833323774197554, 2.006292185433951047 ) ) ;
#75259 = CARTESIAN_POINT ( 'NONE',  ( -3.469997250093771246, 6.135748327496311383, -1.199719254218452935 ) ) ;
#75260 = CARTESIAN_POINT ( 'NONE',  ( 5.888958097455845753, -2.014202512972632420, -0.6635655960139997811 ) ) ;
#75261 = CARTESIAN_POINT ( 'NONE',  ( 2.169099057653073093, -1.925109178590768799, -0.8542606987168609445 ) ) ;
#75262 = CARTESIAN_POINT ( 'NONE',  ( -5.679940009482361774, 5.591294530676332641, 0.7998128361456281477 ) ) ;
#75263 = CARTESIAN_POINT ( 'NONE',  ( 6.591235234537977661, 10.84152487360300299, 0.7998128361456462443 ) ) ;
#75264 = CARTESIAN_POINT ( 'NONE',  ( 6.508657375787280763, 0.5831478024676381988, 1.767317905175052051 ) ) ;
#75265 = CARTESIAN_POINT ( 'NONE',  ( 6.252281394196331554, 10.44607872653774372, 1.040834085586084257E-14 ) ) ;
#75266 = FILL_AREA_STYLE_COLOUR ( '', #112725 ) ;
#75267 = CARTESIAN_POINT ( 'NONE',  ( -3.284818356260900796, 7.054314858938165678, 0.7998128361456352531 ) ) ;
#75269 = CARTESIAN_POINT ( 'NONE',  ( -9.666600336863641729, 10.38004793587015584, 1.040834085586084257E-14 ) ) ;
#75268 = AXIS2_PLACEMENT_3D ( 'NONE', #76914, #192791, #206918 ) ;
#75270 = CARTESIAN_POINT ( 'NONE',  ( 0.08834397731360790762, 1.226219587655341448, 1.729930300845914815 ) ) ;
#75271 = CARTESIAN_POINT ( 'NONE',  ( 0.6224592253955643084, -4.250299932362443300, 0.9218689959748729290 ) ) ;
#75273 = CARTESIAN_POINT ( 'NONE',  ( 3.385159196556942085, 0.04556868695702701727, 1.961494628812537444 ) ) ;
#75272 = CARTESIAN_POINT ( 'NONE',  ( -4.757329562667670667E-14, -0.9374999999999723554, 1.414508159514539454 ) ) ;
#75274 = CARTESIAN_POINT ( 'NONE',  ( 1.235488887756378551, -1.954010380348418119, 0.9248176494114216384 ) ) ;
#75276 = CARTESIAN_POINT ( 'NONE',  ( -4.957065645985164970, 6.648394846229956023, -1.245809975726259067 ) ) ;
#75275 = CARTESIAN_POINT ( 'NONE',  ( -5.309953438407606363, 6.223975762010839574, 1.199719254218452935 ) ) ;
#75277 = CARTESIAN_POINT ( 'NONE',  ( 0.6823417656249899377, 2.342708333674753618, 1.181850606188767472 ) ) ;
#75278 = CARTESIAN_POINT ( 'NONE',  ( 3.011345489304529277, -0.8582029173807427247, -1.513924679874333767 ) ) ;
#75279 = CARTESIAN_POINT ( 'NONE',  ( 5.653386867218496370, 9.539442411822841805, 1.040834085586084257E-14 ) ) ;
#75280 = CARTESIAN_POINT ( 'NONE',  ( -11.58081452147585289, 6.132683923455591213, -5.154482061493088629 ) ) ;
#75281 = CIRCLE ( 'NONE', #9559, 0.08000000000000020983 ) ;
#75282 = CARTESIAN_POINT ( 'NONE',  ( 1.757185253014027282, -2.006138798620077157, -0.2004061740628823030 ) ) ;
#75283 = CARTESIAN_POINT ( 'NONE',  ( -11.00605293250196226, 12.49074738641556870, -1.443095658425808114 ) ) ;
#75284 = CARTESIAN_POINT ( 'NONE',  ( -4.065465959251405081, 5.836405933916976707, -1.599625672291271394 ) ) ;
#75285 = CARTESIAN_POINT ( 'NONE',  ( 1.973447535326333879, 1.887181058671667966, -0.5703184155462033278 ) ) ;
#75287 = CARTESIAN_POINT ( 'NONE',  ( -4.177320726786319049, 6.927272377009067839, -1.082531754730551743 ) ) ;
#75286 = CARTESIAN_POINT ( 'NONE',  ( 5.431871263539022721, -1.864374737420209760, 0.4251265778823994368 ) ) ;
#75288 = AXIS2_PLACEMENT_3D ( 'NONE', #125697, #60606, #46510 ) ;
#75289 = CARTESIAN_POINT ( 'NONE',  ( -4.611181641979265500, 8.393812659035525314, 0.000000000000000000 ) ) ;
#75290 = CARTESIAN_POINT ( 'NONE',  ( 6.119526231721748033, 8.232809585132461194, 1.599625672291269396 ) ) ;
#75291 = CARTESIAN_POINT ( 'NONE',  ( -5.956828388357799042, 8.042995434541133193, 1.599625672291263179 ) ) ;
#75292 = CARTESIAN_POINT ( 'NONE',  ( 2.772133559515827184, 2.009754670806723098, -0.2000300323863890006 ) ) ;
#75293 = CARTESIAN_POINT ( 'NONE',  ( -1.346800533732415817, 4.238484701306172830, 0.3345042947240802755 ) ) ;
#75294 = CARTESIAN_POINT ( 'NONE',  ( 5.210162647842351724, -2.297074225899544242, 0.2200332968223562558 ) ) ;
#75296 = ADVANCED_FACE ( 'NONE', ( #59502 ), #30904, .T. ) ;
#75295 = CARTESIAN_POINT ( 'NONE',  ( 6.619590441841329387, 0.3365870006281460047, -1.932621868259084330 ) ) ;
#75297 = CARTESIAN_POINT ( 'NONE',  ( 3.362109073961420780, -1.959717995770013932, 0.09162775335717905645 ) ) ;
#75298 = CARTESIAN_POINT ( 'NONE',  ( 9.596473800374404561, 10.09030761005864285, 0.000000000000000000 ) ) ;
#75299 = CARTESIAN_POINT ( 'NONE',  ( 0.8795299900376440938, -0.4926441280813895762, -1.955172062459667126 ) ) ;
#75300 = EDGE_LOOP ( 'NONE', ( #161082, #103614, #105795, #152290 ) ) ;
#75301 = CARTESIAN_POINT ( 'NONE',  ( 1.886098781581479145, -2.116736904955533571, 0.05756534462913154987 ) ) ;
#75303 = CARTESIAN_POINT ( 'NONE',  ( -5.859094939400033120, 9.987361195942037639, -0.7998128361456231517 ) ) ;
#75302 = CARTESIAN_POINT ( 'NONE',  ( -2.611917148927046295, 6.198987107056845858, 1.040834085586084257E-14 ) ) ;
#75304 = CARTESIAN_POINT ( 'NONE',  ( 2.484105014303281234, -0.3146448974087300288, -1.813890345909507928 ) ) ;
#75305 = VERTEX_POINT ( 'NONE', #207416 ) ;
#75306 = CARTESIAN_POINT ( 'NONE',  ( -8.971744963941075568, 11.49012176272984931, 1.599625672291269396 ) ) ;
#75307 = CARTESIAN_POINT ( 'NONE',  ( -1.483013432600015502, 7.294277089886564092, 4.259227663825926768 ) ) ;
#75308 = CARTESIAN_POINT ( 'NONE',  ( 3.164422831683691761, 2.120778211551369807, -0.003951117757632071313 ) ) ;
#75309 = CARTESIAN_POINT ( 'NONE',  ( 1.499999999999989120, 4.285416667349482900, 0.8660254037844524744 ) ) ;
#75310 = CARTESIAN_POINT ( 'NONE',  ( 6.577677080924314801, 10.82570702772039262, 1.040834085586084257E-14 ) ) ;
#75311 = CARTESIAN_POINT ( 'NONE',  ( 6.688968683495743583, 8.897159112202094988, -1.599625672291283607 ) ) ;
#75312 = CARTESIAN_POINT ( 'NONE',  ( 3.866525002278593526, -1.386861471309716265, 1.524430686435477522 ) ) ;
#75314 = CARTESIAN_POINT ( 'NONE',  ( 1.083273795380396143, -0.8277460070302902206, 1.644747122058511035 ) ) ;
#75313 = CARTESIAN_POINT ( 'NONE',  ( -7.823218330285243383, 9.085841792542966644, -1.199719254218446718 ) ) ;
#75315 = CARTESIAN_POINT ( 'NONE',  ( -1.201851678989727383E-14, 4.446875000341417916, -1.575800808251660134 ) ) ;
#75316 = SURFACE_STYLE_USAGE ( .BOTH. , #42844 ) ;
#75317 = CARTESIAN_POINT ( 'NONE',  ( -9.499671278040539235, -9.915617081696053603, 0.07902916658837459696 ) ) ;
#75318 = CARTESIAN_POINT ( 'NONE',  ( 0.000000000000000000, 15.50000000000019362, 0.000000000000000000 ) ) ;
#75319 = CARTESIAN_POINT ( 'NONE',  ( 0.8915962724085277902, 1.944627461026976034, -1.043433064090833140 ) ) ;
#75320 = CARTESIAN_POINT ( 'NONE',  ( 2.618781011676008852, 1.479506999046651838, -1.711640912222348376 ) ) ;
#75321 = CARTESIAN_POINT ( 'NONE',  ( -7.863365906246054138, 11.15738207638699464, -1.082531754730543971 ) ) ;
#75322 = CARTESIAN_POINT ( 'NONE',  ( 3.902463391467089426, -1.792703881930355347, -0.2598333579746092692 ) ) ;
#75323 = CARTESIAN_POINT ( 'NONE',  ( 3.380013747803870316, -1.913774515330651127, -0.08860483629866824917 ) ) ;
#75324 = CARTESIAN_POINT ( 'NONE',  ( 4.035645461687249913, 1.950487776689105557, -0.6946759356915442885 ) ) ;
#75325 = CARTESIAN_POINT ( 'NONE',  ( 1.364683531249988535, 2.676041667008082214, 0.7879004041258500513 ) ) ;
#75326 = CARTESIAN_POINT ( 'NONE',  ( 3.274254179156810274, -1.175395456433829144, 1.582609504276990320 ) ) ;
#75327 = CARTESIAN_POINT ( 'NONE',  ( 0.6043602652519001195, -0.6458173669235712788, -1.815047198766789327 ) ) ;
#75328 = CARTESIAN_POINT ( 'NONE',  ( 3.854256360616271415, 0.6726810918341770140, 1.745705178215435582 ) ) ;
#75330 = CARTESIAN_POINT ( 'NONE',  ( 5.088145468715395303, 7.830155539619080507, -1.136959649167136543 ) ) ;
#75329 = CARTESIAN_POINT ( 'NONE',  ( 2.596638674903679167, -2.301597171833298372, -0.1684899434626195847 ) ) ;
#75331 = CARTESIAN_POINT ( 'NONE',  ( 3.859670702416746924, -0.5421201558965526024, 1.780318336934373802 ) ) ;
#75332 = CARTESIAN_POINT ( 'NONE',  ( 1.364683531249988535, 4.363541667008090208, 0.7879004041258500513 ) ) ;
#75333 = CARTESIAN_POINT ( 'NONE',  ( -4.086893239515592136, 6.855460315155083251, 1.199719254218464037 ) ) ;
#75334 = CARTESIAN_POINT ( 'NONE',  ( 5.937581207780954884, 9.014596278131406848, -1.199719254218440723 ) ) ;
#75335 = FACE_OUTER_BOUND ( 'NONE', #156752, .T. ) ;
#75336 = CARTESIAN_POINT ( 'NONE',  ( 1.102331697304242297, -2.106257354988652075, 0.001776637707836397316 ) ) ;
#75338 = CARTESIAN_POINT ( 'NONE',  ( 5.510910596163088569E-16, 10.00000000000000888, 4.500000000000000000 ) ) ;
#75337 = CARTESIAN_POINT ( 'NONE',  ( 0.6823417656249917140, 4.655208333674755394, 1.181850606188765695 ) ) ;
#75339 = CARTESIAN_POINT ( 'NONE',  ( 6.872347393157318685, -1.336039616365672700, 1.699942530728588919 ) ) ;
#75340 = CARTESIAN_POINT ( 'NONE',  ( 2.320699612028754188, -0.8158636990020677882, -1.957571985684476212 ) ) ;
#75342 = EDGE_CURVE ( 'NONE', #113976, #201530, #90585, .T. ) ;
#75341 = CARTESIAN_POINT ( 'NONE',  ( 6.199869188016119637, 1.394352454258035001, 1.461346697781773507 ) ) ;
#75343 = CARTESIAN_POINT ( 'NONE',  ( -1.364683531250000748, -0.4906249996585801409, 0.000000000000000000 ) ) ;
#75344 = CARTESIAN_POINT ( 'NONE',  ( -4.121315508874269007, 5.831287398485176077, -1.443375672974053447 ) ) ;
#75345 = CARTESIAN_POINT ( 'NONE',  ( 4.286349120214771879, 8.152491073559232859, -0.7998128361456221525 ) ) ;
#75346 = CARTESIAN_POINT ( 'NONE',  ( 0.9663661119345479111, 1.064502738163356721, 1.881203019380036867 ) ) ;
#75347 = EDGE_CURVE ( 'NONE', #59570, #208182, #169589, .T. ) ;
#75350 = CARTESIAN_POINT ( 'NONE',  ( 2.548569689688999329, 5.917155704705049146, -0.7216878364870267237 ) ) ;
#75349 = CARTESIAN_POINT ( 'NONE',  ( 6.925078400183515726, -0.002206826874838820583, 1.955452213090567160 ) ) ;
#75348 = CARTESIAN_POINT ( 'NONE',  ( 6.873057527484919937, 6.983264968346048818, 0.7998128361456352531 ) ) ;
#75351 =( BOUNDED_SURFACE ( )  B_SPLINE_SURFACE ( 1, 2, ( 
 ( #4575, #105340, #171378, #89087, #189755, #137833, #203854, #169246, #138902, #136760, #139980, #202788, #106437, #70649, #107517, #73887, #172460, #24047, #173546, #20834, #5640, #25120, #90150, #91224, #55499, #88002, #206002, #201719, #121653, #157284, #8873, #185481, #86933, #135694, #53361, #119495, #37107, #54438, #186557, #38186, #10995, #141063, #109663, #95501, #190814, #93360, #30477, #74952, #43540, #111787, #178866, #159396, #175665, #174612, #162609, #96562, #42474, #207070, #27252, #112851, #192950, #108584, #26188, #76016, #92303, #211331, #61903, #60830, #58700, #45670, #78141, #124849, #142119, #158347, #9941, #208133, #129125, #209190, #59761, #177793, #125921, #191880, #77071, #13135, #143200, #44602, #12073, #144272, #126991, #110717, #176717, #28330, #94426, #160466, #210265, #128064, #194020, #29410, #161548, #62956, #79212, #145330, #195102, #46738, #84534, #197215, #48855, #1128, #101855, #130178, #16312, #49911, #199331, #17379, #97618, #15258, #150624, #52045, #99723, #81345, #179920, #148487, #34710, #2185, #113924, #33649, #18457, #68261, #183099, #67190, #134393, #55, #132261, #116032, #65072, #200396, #114969, #180969, #133327, #14185, #196171, #82397, #182019, #50976, #83462, #163675, #147425, #118171, #184158, #165795, #213449, #31542, #66118, #100780, #35779, #131227, #149542, #80278, #146376, #166862, #117098, #198268, #212390, #64032, #47811, #164723, #32591, #98668, #168983, #172201, #20583, #171116, #185216, #73615, #188430, #22709, #6462, #155947, #135434, #186287, #89896, #72539, #7532, #87736, #136504, #154879, #19522, #37925, #105078, #54173, #3256, #201456, #153811, #55243, #85598, #121390, #122470, #103999, #5383, #170042, #151686, #202524, #40065, #69324, #21628, #123535, #167923, #120313, #204659, #57372, #71460, #137573, #53100, #41145, #189500, #119233, #36840, #203591, #205739, #187363, #102922, #86668, #152735, #4317, #139715, #138637, #38993, #70387, #56309, #88824, #106175, #23789, #157022, #62687, #174345, #161276, #26986, #74691, #209994, #173275, #140794 ),
 ( #25923, #61636, #193757, #95226, #24855, #142926, #144002, #206806, #42208, #92031, #90957, #77880, #125652, #194828, #12863, #192681, #158089, #207873, #9677, #8608, #108325, #109397, #107255, #75753, #58439, #124594, #141863, #127803, #45404, #78937, #190552, #208926, #111520, #59495, #191614, #43276, #176457, #177526, #60561, #175402, #93093, #159134, #10736, #29139, #76806, #126720, #44334, #110456, #28069, #145059, #94163, #160203, #11805, #211062, #128846, #96294, #147171, #166607, #130971, #129923, #149283, #134140, #179662, #50716, #148233, #115773, #63763, #98405, #32337, #195910, #214234, #65862, #97357, #67998, #178597, #48601, #146114, #47546, #34461, #49650, #132012, #113658, #13929, #46463, #114719, #198022, #196963, #164470, #213198, #81084, #181763, #163414, #18196, #33396, #80009, #14990, #162346, #31282, #165533, #16056, #212125, #133072, #112586, #64827, #1938, #66930, #180714, #99474, #82140, #864, #17126, #83201, #30207, #199070, #116842, #100533, #182843, #84281, #150368, #187108, #171943, #153562, #37672, #184963, #22460, #170870, #103748, #36589, #3005, #89642, #88572, #188178, #154630, #39812, #203340, #122216, #152489, #202273, #5133, #136254, #169799, #86423, #20336, #121145, #102676, #105918, #71208, #167668, #168735, #101600, #69074, #104824, #21388, #19269, #72279, #7277, #4071, #155695, #6210, #70141, #38742, #35523, #138388, #120061, #137324, #51801, #53924, #204406, #23534, #56059, #87497, #186036, #73354, #200147, #54993, #117919, #183913, #85351, #151432, #135194, #201211, #52850, #118984, #27820, #127550, #93917, #193521, #142672, #61391, #91781, #58188, #123290, #110209, #157838, #12620, #45162, #10489, #124346, #25674, #41961, #40893, #140547, #141616, #139457, #190304, #173022, #106997, #206560, #159958, #11562, #111276, #205489, #175159, #176218, #24603, #74444, #108073, #208683, #143754, #92848, #57123, #207626, #59244, #9435, #77632, #189253, #125402, #75505, #174101, #191367, #177279, #43034, #90712, #192434, #109146, #26745, #156774, #158892, #28895, #76562, #8360 ) ),
 .UNSPECIFIED., .F., .F., .T. ) 
 B_SPLINE_SURFACE_WITH_KNOTS ( ( 2, 2 ),
 ( 3, 2, 2, 2, 2, 2, 2, 2, 2, 2, 2, 2, 2, 2, 2, 2, 2, 2, 2, 2, 2, 2, 2, 2, 2, 2, 2, 2, 2, 2, 2, 2, 2, 2, 2, 2, 2, 2, 2, 2, 2, 2, 2, 2, 2, 2, 2, 2, 2, 2, 2, 2, 2, 2, 2, 2, 2, 2, 2, 2, 2, 2, 2, 2, 2, 2, 2, 2, 2, 2, 2, 2, 2, 2, 2, 2, 2, 2, 2, 2, 2, 2, 2, 2, 2, 2, 2, 2, 2, 2, 2, 2, 2, 2, 2, 2, 2, 2, 2, 2, 2, 2, 2, 2, 2, 2, 2, 2, 2, 2, 2, 2, 2, 2, 2, 2, 2, 2, 2, 2, 3 ),
 ( 0.000000000000000000, 1.000000000000000000 ),
 ( 0.000000000000000000, 0.008333333333333333218, 0.01666666666666666644, 0.02500000000000000139, 0.03333333333333333287, 0.04166666666666666435, 0.05000000000000000278, 0.05833333333333333426, 0.06666666666666666574, 0.07499999999999999722, 0.08333333333333332871, 0.09166666666666666019, 0.1000000000000000056, 0.1083333333333333370, 0.1166666666666666685, 0.1250000000000000000, 0.1333333333333333315, 0.1416666666666666630, 0.1499999999999999944, 0.1583333333333333259, 0.1666666666666666574, 0.1749999999999999889, 0.1833333333333333204, 0.1916666666666666796, 0.2000000000000000111, 0.2083333333333333426, 0.2166666666666666741, 0.2250000000000000056, 0.2333333333333333370, 0.2416666666666666685, 0.2500000000000000000, 0.2583333333333333592, 0.2666666666666666630, 0.2750000000000000222, 0.2833333333333333259, 0.2916666666666666852, 0.2999999999999999889, 0.3083333333333333481, 0.3166666666666666519, 0.3250000000000000111, 0.3333333333333333148, 0.3416666666666666741, 0.3499999999999999778, 0.3583333333333333370, 0.3666666666666666408, 0.3750000000000000000, 0.3833333333333333592, 0.3916666666666666630, 0.4000000000000000222, 0.4083333333333333259, 0.4166666666666666852, 0.4249999999999999889, 0.4333333333333333481, 0.4416666666666666519, 0.4500000000000000111, 0.4583333333333333148, 0.4666666666666666741, 0.4749999999999999778, 0.4833333333333333370, 0.4916666666666666408, 0.5000000000000000000, 0.5083333333333333037, 0.5166666666666667185, 0.5250000000000000222, 0.5333333333333333259, 0.5416666666666666297, 0.5500000000000000444, 0.5583333333333333481, 0.5666666666666666519, 0.5749999999999999556, 0.5833333333333333703, 0.5916666666666666741, 0.5999999999999999778, 0.6083333333333332815, 0.6166666666666666963, 0.6250000000000000000, 0.6333333333333333037, 0.6416666666666667185, 0.6500000000000000222, 0.6583333333333333259, 0.6666666666666666297, 0.6750000000000000444, 0.6833333333333333481, 0.6916666666666666519, 0.6999999999999999556, 0.7083333333333333703, 0.7166666666666666741, 0.7249999999999999778, 0.7333333333333332815, 0.7416666666666666963, 0.7500000000000000000, 0.7583333333333333037, 0.7666666666666667185, 0.7750000000000000222, 0.7833333333333333259, 0.7916666666666666297, 0.8000000000000000444, 0.8083333333333333481, 0.8166666666666666519, 0.8249999999999999556, 0.8333333333333333703, 0.8416666666666666741, 0.8499999999999999778, 0.8583333333333332815, 0.8666666666666666963, 0.8750000000000000000, 0.8833333333333333037, 0.8916666666666667185, 0.9000000000000000222, 0.9083333333333333259, 0.9166666666666666297, 0.9250000000000000444, 0.9333333333333333481, 0.9416666666666666519, 0.9499999999999999556, 0.9583333333333333703, 0.9666666666666666741, 0.9749999999999999778, 0.9833333333333332815, 0.9916666666666666963, 1.000000000000000000 ),
 .UNSPECIFIED. ) 
 GEOMETRIC_REPRESENTATION_ITEM ( )  RATIONAL_B_SPLINE_SURFACE ( (
 ( 1.000000000000000000, 0.8660254037844387076, 1.000000000000000000, 0.8660254037844387076, 1.000000000000000000, 0.8660254037844387076, 1.000000000000000000, 0.8660254037844387076, 1.000000000000000000, 0.8660254037844387076, 1.000000000000000000, 0.8660254037844387076, 1.000000000000000000, 0.8660254037844387076, 1.000000000000000000, 0.8660254037844387076, 1.000000000000000000, 0.8660254037844387076, 1.000000000000000000, 0.8660254037844387076, 1.000000000000000000, 0.8660254037844387076, 1.000000000000000000, 0.8660254037844387076, 1.000000000000000000, 0.8660254037844387076, 1.000000000000000000, 0.8660254037844387076, 1.000000000000000000, 0.8660254037844387076, 1.000000000000000000, 0.8660254037844387076, 1.000000000000000000, 0.8660254037844387076, 1.000000000000000000, 0.8660254037844387076, 1.000000000000000000, 0.8660254037844387076, 1.000000000000000000, 0.8660254037844387076, 1.000000000000000000, 0.8660254037844387076, 1.000000000000000000, 0.8660254037844387076, 1.000000000000000000, 0.8660254037844387076, 1.000000000000000000, 0.8660254037844387076, 1.000000000000000000, 0.8660254037844387076, 1.000000000000000000, 0.8660254037844387076, 1.000000000000000000, 0.8660254037844387076, 1.000000000000000000, 0.8660254037844387076, 1.000000000000000000, 0.8660254037844387076, 1.000000000000000000, 0.8660254037844387076, 1.000000000000000000, 0.8660254037844387076, 1.000000000000000000, 0.8660254037844387076, 1.000000000000000000, 0.8660254037844387076, 1.000000000000000000, 0.8660254037844387076, 1.000000000000000000, 0.8660254037844387076, 1.000000000000000000, 0.8660254037844387076, 1.000000000000000000, 0.8660254037844387076, 1.000000000000000000, 0.8660254037844387076, 1.000000000000000000, 0.8660254037844387076, 1.000000000000000000, 0.8660254037844387076, 1.000000000000000000, 0.8660254037844387076, 1.000000000000000000, 0.8660254037844387076, 1.000000000000000000, 0.8660254037844387076, 1.000000000000000000, 0.8660254037844387076, 1.000000000000000000, 0.8660254037844387076, 1.000000000000000000, 0.8660254037844387076, 1.000000000000000000, 0.8660254037844387076, 1.000000000000000000, 0.8660254037844387076, 1.000000000000000000, 0.8660254037844387076, 1.000000000000000000, 0.8660254037844387076, 1.000000000000000000, 0.8660254037844387076, 1.000000000000000000, 0.8660254037844387076, 1.000000000000000000, 0.8660254037844387076, 1.000000000000000000, 0.8660254037844387076, 1.000000000000000000, 0.8660254037844387076, 1.000000000000000000, 0.8660254037844387076, 1.000000000000000000, 0.8660254037844387076, 1.000000000000000000, 0.8660254037844387076, 1.000000000000000000, 0.8660254037844387076, 1.000000000000000000, 0.8660254037844387076, 1.000000000000000000, 0.8660254037844387076, 1.000000000000000000, 0.8660254037844387076, 1.000000000000000000, 0.8660254037844387076, 1.000000000000000000, 0.8660254037844387076, 1.000000000000000000, 0.8660254037844387076, 1.000000000000000000, 0.8660254037844387076, 1.000000000000000000, 0.8660254037844387076, 1.000000000000000000, 0.8660254037844387076, 1.000000000000000000, 0.8660254037844387076, 1.000000000000000000, 0.8660254037844387076, 1.000000000000000000, 0.8660254037844387076, 1.000000000000000000, 0.8660254037844387076, 1.000000000000000000, 0.8660254037844387076, 1.000000000000000000, 0.8660254037844387076, 1.000000000000000000, 0.8660254037844387076, 1.000000000000000000, 0.8660254037844387076, 1.000000000000000000, 0.8660254037844387076, 1.000000000000000000, 0.8660254037844387076, 1.000000000000000000, 0.8660254037844387076, 1.000000000000000000, 0.8660254037844387076, 1.000000000000000000, 0.8660254037844387076, 1.000000000000000000, 0.8660254037844387076, 1.000000000000000000, 0.8660254037844387076, 1.000000000000000000, 0.8660254037844387076, 1.000000000000000000, 0.8660254037844387076, 1.000000000000000000, 0.8660254037844387076, 1.000000000000000000, 0.8660254037844387076, 1.000000000000000000, 0.8660254037844387076, 1.000000000000000000, 0.8660254037844387076, 1.000000000000000000, 0.8660254037844387076, 1.000000000000000000, 0.8660254037844387076, 1.000000000000000000, 0.8660254037844387076, 1.000000000000000000, 0.8660254037844387076, 1.000000000000000000, 0.8660254037844387076, 1.000000000000000000, 0.8660254037844387076, 1.000000000000000000, 0.8660254037844387076, 1.000000000000000000, 0.8660254037844387076, 1.000000000000000000, 0.8660254037844387076, 1.000000000000000000, 0.8660254037844387076, 1.000000000000000000, 0.8660254037844387076, 1.000000000000000000, 0.8660254037844387076, 1.000000000000000000, 0.8660254037844387076, 1.000000000000000000, 0.8660254037844387076, 1.000000000000000000, 0.8660254037844387076, 1.000000000000000000, 0.8660254037844387076, 1.000000000000000000, 0.8660254037844387076, 1.000000000000000000, 0.8660254037844387076, 1.000000000000000000, 0.8660254037844387076, 1.000000000000000000, 0.8660254037844387076, 1.000000000000000000, 0.8660254037844387076, 1.000000000000000000, 0.8660254037844387076, 1.000000000000000000, 0.8660254037844387076, 1.000000000000000000, 0.8660254037844387076, 1.000000000000000000, 0.8660254037844387076, 1.000000000000000000, 0.8660254037844387076, 1.000000000000000000, 0.8660254037844387076, 1.000000000000000000, 0.8660254037844387076, 1.000000000000000000, 0.8660254037844387076, 1.000000000000000000, 0.8660254037844387076, 1.000000000000000000, 0.8660254037844387076, 1.000000000000000000),
 ( 1.000000000000000000, 0.8660254037844387076, 1.000000000000000000, 0.8660254037844387076, 1.000000000000000000, 0.8660254037844387076, 1.000000000000000000, 0.8660254037844387076, 1.000000000000000000, 0.8660254037844387076, 1.000000000000000000, 0.8660254037844387076, 1.000000000000000000, 0.8660254037844387076, 1.000000000000000000, 0.8660254037844387076, 1.000000000000000000, 0.8660254037844387076, 1.000000000000000000, 0.8660254037844387076, 1.000000000000000000, 0.8660254037844387076, 1.000000000000000000, 0.8660254037844387076, 1.000000000000000000, 0.8660254037844387076, 1.000000000000000000, 0.8660254037844387076, 1.000000000000000000, 0.8660254037844387076, 1.000000000000000000, 0.8660254037844387076, 1.000000000000000000, 0.8660254037844387076, 1.000000000000000000, 0.8660254037844387076, 1.000000000000000000, 0.8660254037844387076, 1.000000000000000000, 0.8660254037844387076, 1.000000000000000000, 0.8660254037844387076, 1.000000000000000000, 0.8660254037844387076, 1.000000000000000000, 0.8660254037844387076, 1.000000000000000000, 0.8660254037844387076, 1.000000000000000000, 0.8660254037844387076, 1.000000000000000000, 0.8660254037844387076, 1.000000000000000000, 0.8660254037844387076, 1.000000000000000000, 0.8660254037844387076, 1.000000000000000000, 0.8660254037844387076, 1.000000000000000000, 0.8660254037844387076, 1.000000000000000000, 0.8660254037844387076, 1.000000000000000000, 0.8660254037844387076, 1.000000000000000000, 0.8660254037844387076, 1.000000000000000000, 0.8660254037844387076, 1.000000000000000000, 0.8660254037844387076, 1.000000000000000000, 0.8660254037844387076, 1.000000000000000000, 0.8660254037844387076, 1.000000000000000000, 0.8660254037844387076, 1.000000000000000000, 0.8660254037844387076, 1.000000000000000000, 0.8660254037844387076, 1.000000000000000000, 0.8660254037844387076, 1.000000000000000000, 0.8660254037844387076, 1.000000000000000000, 0.8660254037844387076, 1.000000000000000000, 0.8660254037844387076, 1.000000000000000000, 0.8660254037844387076, 1.000000000000000000, 0.8660254037844387076, 1.000000000000000000, 0.8660254037844387076, 1.000000000000000000, 0.8660254037844387076, 1.000000000000000000, 0.8660254037844387076, 1.000000000000000000, 0.8660254037844387076, 1.000000000000000000, 0.8660254037844387076, 1.000000000000000000, 0.8660254037844387076, 1.000000000000000000, 0.8660254037844387076, 1.000000000000000000, 0.8660254037844387076, 1.000000000000000000, 0.8660254037844387076, 1.000000000000000000, 0.8660254037844387076, 1.000000000000000000, 0.8660254037844387076, 1.000000000000000000, 0.8660254037844387076, 1.000000000000000000, 0.8660254037844387076, 1.000000000000000000, 0.8660254037844387076, 1.000000000000000000, 0.8660254037844387076, 1.000000000000000000, 0.8660254037844387076, 1.000000000000000000, 0.8660254037844387076, 1.000000000000000000, 0.8660254037844387076, 1.000000000000000000, 0.8660254037844387076, 1.000000000000000000, 0.8660254037844387076, 1.000000000000000000, 0.8660254037844387076, 1.000000000000000000, 0.8660254037844387076, 1.000000000000000000, 0.8660254037844387076, 1.000000000000000000, 0.8660254037844387076, 1.000000000000000000, 0.8660254037844387076, 1.000000000000000000, 0.8660254037844387076, 1.000000000000000000, 0.8660254037844387076, 1.000000000000000000, 0.8660254037844387076, 1.000000000000000000, 0.8660254037844387076, 1.000000000000000000, 0.8660254037844387076, 1.000000000000000000, 0.8660254037844387076, 1.000000000000000000, 0.8660254037844387076, 1.000000000000000000, 0.8660254037844387076, 1.000000000000000000, 0.8660254037844387076, 1.000000000000000000, 0.8660254037844387076, 1.000000000000000000, 0.8660254037844387076, 1.000000000000000000, 0.8660254037844387076, 1.000000000000000000, 0.8660254037844387076, 1.000000000000000000, 0.8660254037844387076, 1.000000000000000000, 0.8660254037844387076, 1.000000000000000000, 0.8660254037844387076, 1.000000000000000000, 0.8660254037844387076, 1.000000000000000000, 0.8660254037844387076, 1.000000000000000000, 0.8660254037844387076, 1.000000000000000000, 0.8660254037844387076, 1.000000000000000000, 0.8660254037844387076, 1.000000000000000000, 0.8660254037844387076, 1.000000000000000000, 0.8660254037844387076, 1.000000000000000000, 0.8660254037844387076, 1.000000000000000000, 0.8660254037844387076, 1.000000000000000000, 0.8660254037844387076, 1.000000000000000000, 0.8660254037844387076, 1.000000000000000000, 0.8660254037844387076, 1.000000000000000000, 0.8660254037844387076, 1.000000000000000000, 0.8660254037844387076, 1.000000000000000000, 0.8660254037844387076, 1.000000000000000000, 0.8660254037844387076, 1.000000000000000000, 0.8660254037844387076, 1.000000000000000000, 0.8660254037844387076, 1.000000000000000000, 0.8660254037844387076, 1.000000000000000000, 0.8660254037844387076, 1.000000000000000000, 0.8660254037844387076, 1.000000000000000000, 0.8660254037844387076, 1.000000000000000000, 0.8660254037844387076, 1.000000000000000000, 0.8660254037844387076, 1.000000000000000000, 0.8660254037844387076, 1.000000000000000000, 0.8660254037844387076, 1.000000000000000000, 0.8660254037844387076, 1.000000000000000000, 0.8660254037844387076, 1.000000000000000000, 0.8660254037844387076, 1.000000000000000000, 0.8660254037844387076, 1.000000000000000000, 0.8660254037844387076, 1.000000000000000000, 0.8660254037844387076, 1.000000000000000000, 0.8660254037844387076, 1.000000000000000000) ) ) 
 REPRESENTATION_ITEM ( '' )  SURFACE ( )  );
#75352 = CARTESIAN_POINT ( 'NONE',  ( -5.029148636026397945, 4.832037928311032182, 0.7998128361456281477 ) ) ;
#75353 = CARTESIAN_POINT ( 'NONE',  ( 4.698454014923811428, 1.387101836239763131, -1.463925544105355803 ) ) ;
#75355 = CARTESIAN_POINT ( 'NONE',  ( -7.404161286394468355, 7.810812053647902431, 0.000000000000000000 ) ) ;
#75354 = CARTESIAN_POINT ( 'NONE',  ( -9.653042183249972652, 10.36423008998754192, -0.7216878364870267237 ) ) ;
#75356 = EDGE_CURVE ( 'NONE', #197889, #202349, #123081, .T. ) ;
#75357 = SURFACE_STYLE_FILL_AREA ( #9284 ) ;
#75359 = CARTESIAN_POINT ( 'NONE',  ( 1.364683531249996529, 10.46354166700806765, 0.7879004041258403923 ) ) ;
#75358 = CARTESIAN_POINT ( 'NONE',  ( 0.1282872750541429741, -1.395696511722638977, -1.781683957999291579 ) ) ;
#75360 = CARTESIAN_POINT ( 'NONE',  ( -8.839026081105473054, 12.39961529701003684, -1.199719254218446718 ) ) ;
#75362 = CARTESIAN_POINT ( 'NONE',  ( 6.521112179100128969, -1.799899466697444383, 0.9092066555835758290 ) ) ;
#75361 = CARTESIAN_POINT ( 'NONE',  ( -5.544921637864838715, 6.531792001339513654, -1.082531754730543971 ) ) ;
#75363 = CARTESIAN_POINT ( 'NONE',  ( 1.364683531249986537, 0.9677083336747538400, -0.7879004041258239610 ) ) ;
#75364 = DIRECTION ( 'NONE',  ( 0.7613463080411785322, -0.000000000000000000, 0.6483454320283801309 ) ) ;
#75365 = CARTESIAN_POINT ( 'NONE',  ( -1.500000000000008216, 8.750000000000000000, 3.469446951953614189E-15 ) ) ;
#75366 = CARTESIAN_POINT ( 'NONE',  ( 3.140908386031955324, -1.520905784971425589, 0.8136546746303519040 ) ) ;
#75367 = CARTESIAN_POINT ( 'NONE',  ( 5.259637247458703868, 5.100941308315409373, 0.000000000000000000 ) ) ;
#75368 = CARTESIAN_POINT ( 'NONE',  ( 4.694866332082116678, 8.699370830729650450, 0.7998128361456341429 ) ) ;
#75369 = CARTESIAN_POINT ( 'NONE',  ( 0.6843625024184678551, -0.2082719882288592839, -1.757362784332392458 ) ) ;
#75370 = CARTESIAN_POINT ( 'NONE',  ( 2.139316306618759711, 0.002201468654887753229, 2.013265973851806834 ) ) ;
#75371 = CARTESIAN_POINT ( 'NONE',  ( 4.067547972739316897, 0.2730280005818259137, -2.189760481282684967 ) ) ;
#75372 = VECTOR ( 'NONE', #32811, 1000.000000000000000 ) ;
#75373 = VERTEX_POINT ( 'NONE', #7060 ) ;
#75374 = CARTESIAN_POINT ( 'NONE',  ( 4.543917759235442944, 5.330267469643351852, 1.199719254218452935 ) ) ;
#75375 = CARTESIAN_POINT ( 'NONE',  ( 8.148087131688683371, 10.52918762510205042, -1.443375672974063439 ) ) ;
#75377 = CARTESIAN_POINT ( 'NONE',  ( 2.618767733003044551, 0.2496279305150179983, 2.000855661889962445 ) ) ;
#75376 = CARTESIAN_POINT ( 'NONE',  ( 4.793665170694914046, 1.978287127071875151, -0.7638792978137475265 ) ) ;
#75379 = EDGE_LOOP ( 'NONE', ( #46617, #72603, #160665, #173742, #107950 ) ) ;
#75378 = CARTESIAN_POINT ( 'NONE',  ( 3.427799431637909233, -1.783865866189004556, 0.3147462633073249139 ) ) ;
#75380 = CARTESIAN_POINT ( 'NONE',  ( 6.008198349511364000, 7.038594824965278995, 1.199719254218453823 ) ) ;
#75381 = ORIENTED_EDGE ( 'NONE', *, *, #172230, .T. ) ;
#75382 = CARTESIAN_POINT ( 'NONE',  ( 0.3560485870845608858, 0.7116971694140910021, 1.730184004908103867 ) ) ;
#75383 = CARTESIAN_POINT ( 'NONE',  ( 4.111146893441827821, 5.819424013814004759, 1.599625672291267398 ) ) ;
#75384 = EDGE_CURVE ( 'NONE', #211051, #133272, #172807, .T. ) ;
#75385 = CARTESIAN_POINT ( 'NONE',  ( 5.848246728868278232, 1.823843535133644389, 0.08496628090458313576 ) ) ;
#75387 = CARTESIAN_POINT ( 'NONE',  ( 2.008866915445167045, 0.004233813517278902337, 1.915903396628533706 ) ) ;
#75386 = CARTESIAN_POINT ( 'NONE',  ( -2.103486388414573138, 5.605817886458954291, 1.040834085586084257E-14 ) ) ;
#75389 = AXIS2_PLACEMENT_3D ( 'NONE', #124009, #90364, #8016 ) ;
#75388 = AXIS2_PLACEMENT_3D ( 'NONE', #55230, #108314, #207861 ) ;
#75390 = CARTESIAN_POINT ( 'NONE',  ( 1.123270288250311610, 3.172697346350006331, 0.7749999999993734123 ) ) ;
#75391 = FILL_AREA_STYLE ('',( #25556 ) ) ;
#75392 = CARTESIAN_POINT ( 'NONE',  ( -0.6823417656250003738, 1.530208333674752730, -1.181850606188749264 ) ) ;
#75393 = CARTESIAN_POINT ( 'NONE',  ( 7.838022202476093270, 8.316983122409855156, 0.7216878364870267237 ) ) ;
#75394 = CARTESIAN_POINT ( 'NONE',  ( -4.584065335196305213, 6.441438539186039591, 1.443375672974058777 ) ) ;
#75395 = CARTESIAN_POINT ( 'NONE',  ( -7.262327558775498737, 8.501745569106741840, 1.199719254218452047 ) ) ;
#75396 = CARTESIAN_POINT ( 'NONE',  ( 3.322626870553476941, -0.8629183168706102691, -1.937285153019531414 ) ) ;
#75398 = CARTESIAN_POINT ( 'NONE',  ( -10.91435215633265621, 5.922423255477170301, -6.337208484649258899 ) ) ;
#75397 = CARTESIAN_POINT ( 'NONE',  ( -5.820051620566758288, 5.754758076941462797, 0.6671413377488121244 ) ) ;
#75399 = CARTESIAN_POINT ( 'NONE',  ( 4.657473197611246896, 0.4347632249906174806, -1.922659379041303129 ) ) ;
#75400 = CARTESIAN_POINT ( 'NONE',  ( 0.05298979808228323346, 0.3483158054882686261, 1.982706882182909025 ) ) ;
#75401 = ORIENTED_EDGE ( 'NONE', *, *, #146195, .T. ) ;
#75402 = CARTESIAN_POINT ( 'NONE',  ( 0.3513568635829470432, 0.2028739153508585802, -2.107475566755373730 ) ) ;
#75403 = CARTESIAN_POINT ( 'NONE',  ( 9.276324370484291038, 11.45277045833113405, 7.615689369730119118 ) ) ;
#75404 = CARTESIAN_POINT ( 'NONE',  ( 1.486871883557450369, 1.994755712061954123, 0.5540851298423480342 ) ) ;
#75405 = CARTESIAN_POINT ( 'NONE',  ( 2.695178803863579997, -0.6086341500050916897, 1.844178105057793893 ) ) ;
#75406 = EDGE_LOOP ( 'NONE', ( #176531, #20652, #168942, #204974 ) ) ;
#75407 = CARTESIAN_POINT ( 'NONE',  ( 6.540882763950133238, 6.595727744222092959, 0.000000000000000000 ) ) ;
#75408 = CARTESIAN_POINT ( 'NONE',  ( 6.282224075085741433, 8.422623735723785643, 1.599625672291268286 ) ) ;
#75410 = CARTESIAN_POINT ( 'NONE',  ( 6.602984505055297326, 7.662235663108029726, 1.199719254218462483 ) ) ;
#75409 = CARTESIAN_POINT ( 'NONE',  ( 3.679701837385487284, -1.030134525132427203, 1.819138145232774839 ) ) ;
#75411 = CARTESIAN_POINT ( 'NONE',  ( 3.241808126998965811, 6.796210224891872542, 0.7216878364870257245 ) ) ;
#75413 = ORIENTED_EDGE ( 'NONE', *, *, #63569, .T. ) ;
#75412 = CARTESIAN_POINT ( 'NONE',  ( 0.8030048707254822116, 1.598173448761495585, -0.8528199064772985505 ) ) ;
#75414 = CARTESIAN_POINT ( 'NONE',  ( 5.426482453889071245, 1.317083479513626587, -1.770629405693980640 ) ) ;
#75415 = SURFACE_STYLE_FILL_AREA ( #174010 ) ;
#75416 = CARTESIAN_POINT ( 'NONE',  ( 3.751171811254182753, -1.805526059370649028, 1.268566889074909554 ) ) ;
#75417 = CARTESIAN_POINT ( 'NONE',  ( 8.132193210098487057, 8.381980254736715708, 1.040834085586084257E-14 ) ) ;
#75418 = CARTESIAN_POINT ( 'NONE',  ( 3.619663824724254741, 6.206396314611513532, -1.082531754730543971 ) ) ;
#75419 = CARTESIAN_POINT ( 'NONE',  ( 3.158751774003202950, 0.4669426847015486493, 1.854258104404989060 ) ) ;
#75420 = CARTESIAN_POINT ( 'NONE',  ( 8.072990401933337168, 11.50590700464255356, -1.199719254218446718 ) ) ;
#75421 = CARTESIAN_POINT ( 'NONE',  ( 5.529760519541640384, 1.996289034380031913, -0.5486624943154896350 ) ) ;
#75423 = CARTESIAN_POINT ( 'NONE',  ( 2.430746436576446179, 2.096607243605509208, 0.5259719050795114148 ) ) ;
#75422 = DIRECTION ( 'NONE',  ( 1.000000000000000000, 3.451266460341926649E-31, 8.638326563840810896E-31 ) ) ;
#75424 = CARTESIAN_POINT ( 'NONE',  ( 4.704715985517350596, 1.906866092115505840, 1.080010033982371498 ) ) ;
#75425 = ORIENTED_EDGE ( 'NONE', *, *, #35088, .T. ) ;
#75426 = TOROIDAL_SURFACE ( 'NONE', #172224, 0.8300000000000010703, 0.08000000000000000167 ) ;
#75427 = CARTESIAN_POINT ( 'NONE',  ( -9.521443730523930782, -8.144690279336726846, 0.3123298761244260313 ) ) ;
#75428 = CARTESIAN_POINT ( 'NONE',  ( 9.498884434226638973, -9.954196546781650667, -0.1657939142878195604 ) ) ;
#75429 = CARTESIAN_POINT ( 'NONE',  ( 4.115782150200256950, 6.959440387612411349, 1.199719254218452047 ) ) ;
#75430 = CARTESIAN_POINT ( 'NONE',  ( -8.012344526598182026E-15, 15.10937500034140157, -1.575800808251669460 ) ) ;
#75431 =( LENGTH_UNIT ( ) NAMED_UNIT ( * ) SI_UNIT ( .MILLI., .METRE. ) );
#75432 = CARTESIAN_POINT ( 'NONE',  ( -8.432808358020034589, 10.86136238915529084, 1.443375672974064550 ) ) ;
#75433 = CARTESIAN_POINT ( 'NONE',  ( 5.574337433874081427, 6.532423756721743580, -1.199719254218452047 ) ) ;
#75434 = CARTESIAN_POINT ( 'NONE',  ( 6.139524545372063713, 1.915082402702467101, -0.7868883245659707981 ) ) ;
#75435 = CARTESIAN_POINT ( 'NONE',  ( 4.899011302651929078, 1.600714092801895472, -1.071686876026227475 ) ) ;
#75436 = CARTESIAN_POINT ( 'NONE',  ( 0.3863424973270003226, -0.6820169105002243937, -1.897691504806876761 ) ) ;
#75437 = CARTESIAN_POINT ( 'NONE',  ( 5.671053392266061977, 9.838255734277600695, 0.7998128361456331437 ) ) ;
#75438 = CARTESIAN_POINT ( 'NONE',  ( -4.174586609897826150, 3.976382069392089047, -0.6022320305223278769 ) ) ;
#75439 = CARTESIAN_POINT ( 'NONE',  ( 5.014487319174643964, 0.7500019944287477092, 1.821250405324719823 ) ) ;
#75440 = CARTESIAN_POINT ( 'NONE',  ( 6.703114550498504798, -0.5130225571751775293, 2.242675272849779411 ) ) ;
#75441 = CARTESIAN_POINT ( 'NONE',  ( 4.863791234866603475, 1.805334366393744450, -0.2710410529033688842 ) ) ;
#75442 = CARTESIAN_POINT ( 'NONE',  ( 4.570507181582611267, 8.346359121906111511, 0.000000000000000000 ) ) ;
#75443 = CARTESIAN_POINT ( 'NONE',  ( 4.650083499362880346, 4.527444958785877382, 0.7216878364870317197 ) ) ;
#75444 = CARTESIAN_POINT ( 'NONE',  ( -4.294900800479008574, 8.232744377192641849, 0.000000000000000000 ) ) ;
#75445 = CARTESIAN_POINT ( 'NONE',  ( 5.401997860402196316, 5.267028690082820930, 0.000000000000000000 ) ) ;
#75446 = ORIENTED_EDGE ( 'NONE', *, *, #190752, .T. ) ;
#75448 = CARTESIAN_POINT ( 'NONE',  ( -0.04036574886347610303, -1.557478217179044888, -1.275100411523772737 ) ) ;
#75447 = CARTESIAN_POINT ( 'NONE',  ( 2.700538275128167687, 1.556679782967337999, 0.9830204120172959525 ) ) ;
#75449 = CARTESIAN_POINT ( 'NONE',  ( 1.089736160853293168, 1.367490553916232754, -1.847165887925501515 ) ) ;
#75450 = CARTESIAN_POINT ( 'NONE',  ( 0.3032578436052570936, -1.433215674808469009, -1.186817810889209124 ) ) ;
#75451 = CARTESIAN_POINT ( 'NONE',  ( -5.742041750587549842, 6.657802449562273850, 1.199719254218450271 ) ) ;
#75452 = CARTESIAN_POINT ( 'NONE',  ( -5.980802423990385641, 6.150226714305422782, 9.481663569016276247E-06 ) ) ;
#75453 = CARTESIAN_POINT ( 'NONE',  ( -3.297657676621885692, 4.870353260857385180, 1.599625672291267398 ) ) ;
#75454 = CARTESIAN_POINT ( 'NONE',  ( 3.673940397442059868E-16, -3.517800438942085606, -3.000000000000000000 ) ) ;
#75455 = CARTESIAN_POINT ( 'NONE',  ( -3.959863383643135393, 6.777535159962392086, 1.199719254218452935 ) ) ;
#75457 = CARTESIAN_POINT ( 'NONE',  ( 0.8131078318618142342, -0.2785150557334699073, 1.849687307983488571 ) ) ;
#75456 = CARTESIAN_POINT ( 'NONE',  ( 2.753556666441462131, 2.080443298914707917, -0.2074443561481206788 ) ) ;
#75458 = CARTESIAN_POINT ( 'NONE',  ( 2.354842093047845530, -0.8645933883619570937, 1.821462535208747457 ) ) ;
#75459 = ORIENTED_EDGE ( 'NONE', *, *, #157556, .F. ) ;
#75460 = CARTESIAN_POINT ( 'NONE',  ( 1.364683531249988535, 3.676041667008087099, 0.7879004041258499402 ) ) ;
#75461 = CARTESIAN_POINT ( 'NONE',  ( 2.014833872101874146, -1.687939792665555494, 0.4236265878580796618 ) ) ;
#75462 = PRESENTATION_LAYER_ASSIGNMENT (  '', '', ( #206871 ) ) ;
#75463 = CARTESIAN_POINT ( 'NONE',  ( 5.148345644887269756, 7.029489223833707001, -1.599625672291256295 ) ) ;
#75465 = DIRECTION ( 'NONE',  ( 0.000000000000000000, -3.330669073875420317E-16, -1.000000000000000000 ) ) ;
#75464 = DIRECTION ( 'NONE',  ( 0.000000000000000000, 0.000000000000000000, 1.000000000000000000 ) ) ;
#75466 = CARTESIAN_POINT ( 'NONE',  ( 2.560839114378242076, -1.500511350262800470, -0.8505237462590549136 ) ) ;
#75467 = CARTESIAN_POINT ( 'NONE',  ( 2.595491417077447238, -0.6846416945752286098, 2.081959150545972914 ) ) ;
#75468 = CARTESIAN_POINT ( 'NONE',  ( 5.022202109028018668, -1.178465353167540197, -1.865713892744431446 ) ) ;
#75469 = CARTESIAN_POINT ( 'NONE',  ( -10.78926753850537423, 5.463497890167042570, -6.588879020148982413 ) ) ;
#75470 = CARTESIAN_POINT ( 'NONE',  ( 2.536178501573463695, 1.332599179293973091, 1.713937585783622541 ) ) ;
#75471 = CARTESIAN_POINT ( 'NONE',  ( 0.9436603434208358232, 0.7422609627109194586, -1.668170528445270140 ) ) ;
#75472 = CARTESIAN_POINT ( 'NONE',  ( 3.468056730359007744, -1.039945921192251266, 1.844253657775334121 ) ) ;
#75473 = CARTESIAN_POINT ( 'NONE',  ( 0.000000000000000000, -6.836568542494925182, 0.000000000000000000 ) ) ;
#75474 = ORIENTED_EDGE ( 'NONE', *, *, #214379, .F. ) ;
#75475 = MECHANICAL_DESIGN_GEOMETRIC_PRESENTATION_REPRESENTATION (  '', ( #206887 ), #186158 ) ;
#75477 = CARTESIAN_POINT ( 'NONE',  ( -1.201851678989727383E-14, 1.634375000341421025, 1.575800808251672791 ) ) ;
#75476 = CARTESIAN_POINT ( 'NONE',  ( 3.808379203468327034, 1.620604861375672945, -1.621544036339316985 ) ) ;
#75478 = CARTESIAN_POINT ( 'NONE',  ( 0.3282377607280986820, 0.07366454968464808406, 1.224999999999942801 ) ) ;
#75479 = CARTESIAN_POINT ( 'NONE',  ( 3.167801447087334576, 6.847518788243868393, -0.7998128361456291469 ) ) ;
#75480 = EDGE_CURVE ( 'NONE', #42393, #32144, #57972, .T. ) ;
#75481 = CARTESIAN_POINT ( 'NONE',  ( 5.479204513921561492, -2.007303783262293972, -0.9515056986081956714 ) ) ;
#75482 = CARTESIAN_POINT ( 'NONE',  ( -5.083944415444539899, 8.875092884753202682, 0.000000000000000000 ) ) ;
#75483 = CARTESIAN_POINT ( 'NONE',  ( 4.880572111239557920, 4.796348339308675435, -0.7216878364870197293 ) ) ;
#75484 = CARTESIAN_POINT ( 'NONE',  ( -5.531363484251157203, 9.397081798360927607, 0.000000000000000000 ) ) ;
#75485 = CARTESIAN_POINT ( 'NONE',  ( 6.825078400183555161, 2.980425674467933828, 2.309322343017068402 ) ) ;
#75486 = ORIENTED_EDGE ( 'NONE', *, *, #211675, .T. ) ;
#75487 = CARTESIAN_POINT ( 'NONE',  ( 4.324842380567116784, 0.8596320953860696612, -1.824118450417112847 ) ) ;
#75489 = CARTESIAN_POINT ( 'NONE',  ( 2.799736005369108049, -1.525370932871713547, -1.388464765246626875 ) ) ;
#75488 = CARTESIAN_POINT ( 'NONE',  ( 7.461064606222022277, 7.598996883547496139, 1.040834085586084257E-14 ) ) ;
#75490 = CARTESIAN_POINT ( 'NONE',  ( -5.317278910447152285, 7.722098771695092623, -1.369991256297370619 ) ) ;
#75491 = CARTESIAN_POINT ( 'NONE',  ( 5.221298554594243413, 5.264138866547622975, -0.7216878364870458196 ) ) ;
#75492 = CARTESIAN_POINT ( 'NONE',  ( -3.285556943749998737, -2.530208332855374831, 1.896917185911908499 ) ) ;
#75493 = CARTESIAN_POINT ( 'NONE',  ( 6.562441972333600937, -2.001882313047067985, -0.8919867065708479981 ) ) ;
#75494 = CARTESIAN_POINT ( 'NONE',  ( 3.199842427594956185, 1.824118962040650604, 0.8596310190432245868 ) ) ;
#75495 = CARTESIAN_POINT ( 'NONE',  ( 2.665370095338463585, 0.9869154847663293983, 1.554228294351194473 ) ) ;
#75496 = CARTESIAN_POINT ( 'NONE',  ( 5.621827251160867789, 9.710548892996357040, 1.040834085586084257E-14 ) ) ;
#75497 = EDGE_CURVE ( 'NONE', #138365, #56380, #180547, .T. ) ;
#75498 = CARTESIAN_POINT ( 'NONE',  ( 6.106453908201667780, -0.6597477751954274883, -1.702385593799011110 ) ) ;
#75499 = CARTESIAN_POINT ( 'NONE',  ( -0.01642261062154842799, -2.298356651571492826, -0.04744217504730821600 ) ) ;
#75500 = CARTESIAN_POINT ( 'NONE',  ( -7.497822643557261024, 8.706213491360317747, -1.199719254218446718 ) ) ;
#75501 = CARTESIAN_POINT ( 'NONE',  ( 6.069232182892009497, 0.1736634173518056545, -2.255917496054614446 ) ) ;
#75502 = CARTESIAN_POINT ( 'NONE',  ( 1.506614580823143701, -0.7594792294695625889, -1.964545455775383642 ) ) ;
#75503 = CARTESIAN_POINT ( 'NONE',  ( -6.771371375382467583, 6.864631124226471037, -0.7998128361456362523 ) ) ;
#75504 = CARTESIAN_POINT ( 'NONE',  ( 8.776205506747620788, 9.133327934160710981, -0.7998128361456221525 ) ) ;
#75505 = CARTESIAN_POINT ( 'NONE',  ( 7.960045584554727327, 8.459343734834927631, 0.7216878364870267237 ) ) ;
#75506 = CARTESIAN_POINT ( 'NONE',  ( -7.015454420067433361, 10.27211502579893754, 1.199719254218453823 ) ) ;
#75507 = CARTESIAN_POINT ( 'NONE',  ( 6.234224025626348364, -6.938199013094628498, 6.849482339516216989 ) ) ;
#75508 = CARTESIAN_POINT ( 'NONE',  ( 8.554831740098663317, 9.082984572977682802, 0.7216878364870458196 ) ) ;
#75509 = CARTESIAN_POINT ( 'NONE',  ( 4.114373074986557910, 7.676947195153840831, 0.7202382532921544067 ) ) ;
#75510 = CARTESIAN_POINT ( 'NONE',  ( -5.935772324684618795, 5.819489221753827657, 0.000000000000000000 ) ) ;
#75512 = CARTESIAN_POINT ( 'NONE',  ( 4.183969649472300212, 2.154223736155444602, -0.5416631952432825470 ) ) ;
#75511 = CARTESIAN_POINT ( 'NONE',  ( 2.057031522680652369, 0.4693188842763912905, 2.067847215655476134 ) ) ;
#75513 = CARTESIAN_POINT ( 'NONE',  ( 0.1181803206181560040, -2.163391993613572151, 0.4351206515559591370 ) ) ;
#75514 = CARTESIAN_POINT ( 'NONE',  ( -4.634908411025374875, 6.500755460986618495, 1.599625672291263179 ) ) ;
#75515 = CARTESIAN_POINT ( 'NONE',  ( 5.015626762051672571, 7.938982758113895422, 1.199719254218462483 ) ) ;
#75516 = CARTESIAN_POINT ( 'NONE',  ( 4.228923158279327410, -1.829750178516520442, -0.7082015076659909925 ) ) ;
#75517 = CARTESIAN_POINT ( 'NONE',  ( 8.727698198895078363, 11.20540053684285553, -1.599625672291257406 ) ) ;
#75518 = CARTESIAN_POINT ( 'NONE',  ( -5.012544637203120601, 6.604931577287184830, 1.238112577840282169 ) ) ;
#75519 = CARTESIAN_POINT ( 'NONE',  ( 0.000000000000000000, -7.154544010627095219, 0.000000000000000000 ) ) ;
#75520 = CARTESIAN_POINT ( 'NONE',  ( -0.6823417656250003738, 0.4677083336747517306, -1.181850606188749264 ) ) ;
#75521 = CARTESIAN_POINT ( 'NONE',  ( -4.556949027968976829, 5.449433633119473264, 1.082531754730549078 ) ) ;
#75523 = ORIENTED_EDGE ( 'NONE', *, *, #87121, .F. ) ;
#75522 = CARTESIAN_POINT ( 'NONE',  ( -6.127922243696855453, 7.211959374810172463, 1.082531754730549967 ) ) ;
#75525 = CARTESIAN_POINT ( 'NONE',  ( 3.428091063814618700, -2.088597262255381448, 0.3661859999234198249 ) ) ;
#75524 = VECTOR ( 'NONE', #49604, 1000.000000000000114 ) ;
#75526 = CARTESIAN_POINT ( 'NONE',  ( -5.204350862799341115, 7.165104988056252289, -1.599625672291271394 ) ) ;
#75527 = CARTESIAN_POINT ( 'NONE',  ( 5.418883921851007202, 1.995750516393671514, 0.8311057252617033431 ) ) ;
#75528 = CARTESIAN_POINT ( 'NONE',  ( 3.843160323004328305, 0.6166970922517556186, -1.735048075492843234 ) ) ;
#75529 = CARTESIAN_POINT ( 'NONE',  ( 4.962125165302472496, -1.116212726388360998, 1.679221540125563905 ) ) ;
#75530 = CARTESIAN_POINT ( 'NONE',  ( -5.526177461252244960, 6.240421959547291841, 0.9601993850730760061 ) ) ;
#75531 = CARTESIAN_POINT ( 'NONE',  ( -1.364683531250014514, 1.051041667008090208, -0.7879004041258289570 ) ) ;
#75532 = CARTESIAN_POINT ( 'NONE',  ( 6.685563754570789996, -0.7372397036040450047, 1.575249959525576005 ) ) ;
#75533 = CARTESIAN_POINT ( 'NONE',  ( 6.827182134110198142, 0.003888933837258023996, 1.810856214465889069 ) ) ;
#75534 = CARTESIAN_POINT ( 'NONE',  ( 3.714570900464278846, 5.356752022006865843, 1.443375672974062551 ) ) ;
#75535 = CARTESIAN_POINT ( 'NONE',  ( 11.84101807917483740, 13.61021500260877559, -1.444039656437080543 ) ) ;
#75536 = CARTESIAN_POINT ( 'NONE',  ( 3.643588467267334874, -1.635511012911139650, -1.413612897787956513 ) ) ;
#75537 = CARTESIAN_POINT ( 'NONE',  ( 5.852888695852590750, -0.9090035733541059759, 1.799648235488074732 ) ) ;
#75538 = CARTESIAN_POINT ( 'NONE',  ( -8.690413276235355866, 10.20153224610512943, 1.082531754730558626 ) ) ;
#75539 = CIRCLE ( 'NONE', #41068, 1.220000000000001750 ) ;
#75540 = CARTESIAN_POINT ( 'NONE',  ( 3.221700144506876917, -2.083771231579465866, 0.5749860669421112958 ) ) ;
#75541 = CARTESIAN_POINT ( 'NONE',  ( 3.426987366535645396, 0.04501397872612270673, 1.970993176858675699 ) ) ;
#75542 = B_SPLINE_CURVE_WITH_KNOTS ( 'NONE', 3,
 ( #1379, #33901, #53356, #169242, #98922, #2441, #166045, #118425, #69579, #150878, #103182, #4571, #37102, #83715, #19778, #20830 ),
 .UNSPECIFIED., .F., .F.,
 ( 4, 2, 2, 2, 2, 2, 2, 4 ),
 ( 0.3501333200791456046, 0.3551713324458994903, 0.3602093448126533759, 0.3702853695461611472, 0.3803518226137216351, 0.3853850491475018791, 0.3879016624143920011, 0.3904182756812821231 ),
 .UNSPECIFIED. ) ;
#75543 = DIRECTION ( 'NONE',  ( -1.000000000000000000, 0.000000000000000000, 0.000000000000000000 ) ) ;
#75544 = CARTESIAN_POINT ( 'NONE',  ( 1.466329616580586581, 2.273096917617071888, -0.3966160293069305731 ) ) ;
#75545 = CARTESIAN_POINT ( 'NONE',  ( 2.741540247014317533, -1.524689737823584190, -1.386575092742351245 ) ) ;
#75546 = CARTESIAN_POINT ( 'NONE',  ( 5.882362869737407074, -0.2893225776206589384, -1.920288418758001159 ) ) ;
#75549 = ORIENTED_EDGE ( 'NONE', *, *, #183283, .T. ) ;
#75548 = CARTESIAN_POINT ( 'NONE',  ( -1.123270288250342919, 3.096052654332833054, 0.7749999999993751887 ) ) ;
#75547 = CARTESIAN_POINT ( 'NONE',  ( -7.009202228140739344, 11.12122699956546334, -0.7216878364870267237 ) ) ;
#75550 = CARTESIAN_POINT ( 'NONE',  ( -6.903036488013351679, 8.082572653217566128, -1.199719254218452047 ) ) ;
#75552 = ORIENTED_EDGE ( 'NONE', *, *, #75384, .T. ) ;
#75551 = CARTESIAN_POINT ( 'NONE',  ( -5.143339171537843590, 7.093924681584509173, 1.599625672291263179 ) ) ;
#75553 = CARTESIAN_POINT ( 'NONE',  ( -7.497295758232731089, 8.809561808435409702, -1.082531754730543083 ) ) ;
#75554 = CARTESIAN_POINT ( 'NONE',  ( 2.538337413235943973, 1.040872164564849767, -1.945885072647230318 ) ) ;
#75556 = EDGE_CURVE ( 'NONE', #94442, #69312, #156555, .T. ) ;
#75555 = CARTESIAN_POINT ( 'NONE',  ( -3.285556943749998737, -0.4302083328553760744, 1.896917185911908499 ) ) ;
#75557 = CARTESIAN_POINT ( 'NONE',  ( 6.455910365318025868, -0.6640748382394038307, 1.846044136633723243 ) ) ;
#75558 = CARTESIAN_POINT ( 'NONE',  ( 6.539320575229233157, 0.001224430076711413356, 2.103502572931112091 ) ) ;
#75559 = CARTESIAN_POINT ( 'NONE',  ( -1.499999999999997780, 4.681250000682819490, 1.214306433183764966E-14 ) ) ;
#75560 = CARTESIAN_POINT ( 'NONE',  ( -9.516020521605595306, -8.176244038173962281, 0.3909723190919960900 ) ) ;
#75562 = DIRECTION ( 'NONE',  ( -1.000000000000000000, 0.000000000000000000, 1.465138070926357285E-17 ) ) ;
#75561 = CARTESIAN_POINT ( 'NONE',  ( 0.000000000000000000, 2.880000000000021210, 1.214306433183764966E-14 ) ) ;
#75563 = CARTESIAN_POINT ( 'NONE',  ( 5.314338895140061858, 1.702579029208791450, 0.7012131971957938914 ) ) ;
#75564 = EDGE_LOOP ( 'NONE', ( #120258, #76725, #143550, #126903 ) ) ;
#75565 = CARTESIAN_POINT ( 'NONE',  ( 2.079048039887823052, -0.09986672515850322784, -2.058587512739398662 ) ) ;
#75566 = CARTESIAN_POINT ( 'NONE',  ( -0.6801582343749917881, 0.4322916670080681478, 1.178068619123841643 ) ) ;
#75567 = CARTESIAN_POINT ( 'NONE',  ( -7.477485413136760073, 8.682486722536401302, -1.199719254218446718 ) ) ;
#75568 = CARTESIAN_POINT ( 'NONE',  ( 10.91910517057295316, -9.994362614652946064, -0.1236848126708652712 ) ) ;
#75569 = CARTESIAN_POINT ( 'NONE',  ( 11.97297122925985313, 11.29874920673088567, 0.8121202983519475449 ) ) ;
#75570 = CARTESIAN_POINT ( 'NONE',  ( 8.790438134619869004, 13.29428800202395955, -8.101059483297389008 ) ) ;
#75571 = CARTESIAN_POINT ( 'NONE',  ( 3.974511587100456822, 7.788680618259193444, 1.040834085586084257E-14 ) ) ;
#75572 = CARTESIAN_POINT ( 'NONE',  ( 0.7782833776110262836, -1.145455985629862505, 1.713024904945841254 ) ) ;
#75575 = CARTESIAN_POINT ( 'NONE',  ( 4.985823801847525161, -1.827980399782932697, -0.2200341325891697619 ) ) ;
#75574 = CARTESIAN_POINT ( 'NONE',  ( 1.767777038385684785, -1.847514956963384414, 0.2233714002321494363 ) ) ;
#75573 = CARTESIAN_POINT ( 'NONE',  ( -9.811039896441892338, -7.242250812739402299, 9.077051502758969193E-18 ) ) ;
#75576 = CARTESIAN_POINT ( 'NONE',  ( 6.500244582748090139, 9.671036882259738121, 1.199719254218460707 ) ) ;
#75577 = CARTESIAN_POINT ( 'NONE',  ( -4.999100218102086046, 8.030536425943571643, -1.156731540297722738 ) ) ;
#75578 = CARTESIAN_POINT ( 'NONE',  ( -5.281783360975562225, 8.319775133516907673, 1.199719254218452935 ) ) ;
#75580 = EDGE_LOOP ( 'NONE', ( #37311, #108091, #63421, #121333 ) ) ;
#75579 = CARTESIAN_POINT ( 'NONE',  ( -11.25751254300905480, -6.452016313277408877, 1.138412281109779656E-15 ) ) ;
#75581 = CARTESIAN_POINT ( 'NONE',  ( 4.530015419921377351, -1.356323209173672106, -1.740806116466916409 ) ) ;
#75582 = CARTESIAN_POINT ( 'NONE',  ( 0.5444778865218368180, 2.155786741090206959, 0.1595364878888144988 ) ) ;
#75583 = CARTESIAN_POINT ( 'NONE',  ( -6.100805936469506641, 6.219954468743612352, 0.7216878364870317197 ) ) ;
#75584 = CARTESIAN_POINT ( 'NONE',  ( -0.1405747822309927342, -1.479430311965252542, -1.211566217618691210 ) ) ;
#75585 = CARTESIAN_POINT ( 'NONE',  ( 6.509000000000050967, 0.007656933339270000430, 1.900274884395843022 ) ) ;
#75586 = VECTOR ( 'NONE', #67647, 1000.000000000000000 ) ;
#75587 = CARTESIAN_POINT ( 'NONE',  ( 0.000000000000000000, 1.551257596039481879, 0.000000000000000000 ) ) ;
#75588 = CARTESIAN_POINT ( 'NONE',  ( 9.244366848620945376, 14.19092405134642298, -7.651760635101037877 ) ) ;
#75589 = CARTESIAN_POINT ( 'NONE',  ( 5.690081826675051246, 1.142623417513729089, 1.533212917768103534 ) ) ;
#75590 = CARTESIAN_POINT ( 'NONE',  ( 1.164687902950040321, -1.689591380799923215, -0.8031939614948147010 ) ) ;
#75591 = CARTESIAN_POINT ( 'NONE',  ( 2.184780103950241248, 1.616692242240840960, -1.205043568535242304 ) ) ;
#75593 = CARTESIAN_POINT ( 'NONE',  ( 3.440152538952054861, 0.9466726917620759130, -1.881381795136138679 ) ) ;
#75592 = CARTESIAN_POINT ( 'NONE',  ( -7.343712760096452463, 11.71941532008788833, -0.7998128361456291469 ) ) ;
#75594 = CARTESIAN_POINT ( 'NONE',  ( 8.769426429940780920, 9.125419011219408461, 0.7998128361456462443 ) ) ;
#75596 = CARTESIAN_POINT ( 'NONE',  ( -8.097244055859620815, 10.46987070330147063, -1.599625672291263179 ) ) ;
#75595 = CARTESIAN_POINT ( 'NONE',  ( -1.500000000000001332, -0.3499999999999753308, 0.000000000000000000 ) ) ;
#75597 = CARTESIAN_POINT ( 'NONE',  ( 11.44779963594995564, 10.19999999999997442, 3.600000000000075140 ) ) ;
#75599 = EDGE_CURVE ( 'NONE', #139393, #175615, #10922, .T. ) ;
#75598 = CARTESIAN_POINT ( 'NONE',  ( 4.148698013468838930, 1.981613772426650266, 0.3898967627796907642 ) ) ;
#75600 = CARTESIAN_POINT ( 'NONE',  ( 0.6823417656249899377, 4.176041667008085767, -1.181850606188754593 ) ) ;
#75601 = CARTESIAN_POINT ( 'NONE',  ( 8.405692050792682224, 12.75046512599275772, -0.7216878364870328300 ) ) ;
#75602 = CARTESIAN_POINT ( 'NONE',  ( 4.534552404040613105, 2.118918870418550870, 0.4265773709258223190 ) ) ;
#75603 = CARTESIAN_POINT ( 'NONE',  ( -1.946706258588004168, 3.753940929402450610, 0.4616008842494395692 ) ) ;
#75604 = CARTESIAN_POINT ( 'NONE',  ( -0.7500000000000215383, 5.691666666666685082, 1.299038105676671107 ) ) ;
#75606 = DIRECTION ( 'NONE',  ( 0.000000000000000000, 1.000000000000000000, 0.000000000000000000 ) ) ;
#75605 = CARTESIAN_POINT ( 'NONE',  ( 6.042093733545556233, 7.078139439671806699, -1.199719254218452047 ) ) ;
#75607 = CARTESIAN_POINT ( 'NONE',  ( 8.012505595552012139, 11.33137838057728786, -1.082531754730543083 ) ) ;
#75609 = CARTESIAN_POINT ( 'NONE',  ( -2.750656850324853409, 2.940527718787148803, -2.453100388279096933 ) ) ;
#75608 = CARTESIAN_POINT ( 'NONE',  ( 1.873705115703153679, -0.2670016379083521296, 2.154652869704001272 ) ) ;
#75611 = CARTESIAN_POINT ( 'NONE',  ( 1.118424870118275738, -0.04499623084481922664, 1.840855209834332928 ) ) ;
#75610 = CARTESIAN_POINT ( 'NONE',  ( -6.073689629242160493, 8.109057205581079231, -1.443375672974059665 ) ) ;
#75612 = EDGE_CURVE ( 'NONE', #46203, #79633, #52276, .T. ) ;
#75613 = CARTESIAN_POINT ( 'NONE',  ( 1.364683531249988757, 1.884375000341421913, 0.000000000000000000 ) ) ;
#75614 = CARTESIAN_POINT ( 'NONE',  ( 1.927518781310177509, -1.434474475899261581, -1.656937093973806396 ) ) ;
#75615 = CARTESIAN_POINT ( 'NONE',  ( 6.983263157960361234, 4.694303448529787204, 2.516403841208918912 ) ) ;
#75616 = CARTESIAN_POINT ( 'NONE',  ( 3.362467959171450360, 1.015586399080644187, 2.021831916694483144 ) ) ;
#75617 = CARTESIAN_POINT ( 'NONE',  ( -6.021792782764022078, 10.17717534653336209, -0.7998128361456291469 ) ) ;
#75618 = CARTESIAN_POINT ( 'NONE',  ( 4.575407832915947104, 1.497500392235491029, 1.350737390116145242 ) ) ;
#75620 = CIRCLE ( 'NONE', #61701, 0.08000000000000052902 ) ;
#75619 = CARTESIAN_POINT ( 'NONE',  ( -1.364683531250010295, 5.092708333674757171, 0.7879004041258379498 ) ) ;
#75621 = CARTESIAN_POINT ( 'NONE',  ( 6.396603524444617328, 6.809554808131969672, -0.5206029305389828776 ) ) ;
#75622 = CARTESIAN_POINT ( 'NONE',  ( -1.500000000000001110, 12.02083333333333748, 0.8660254037844419273 ) ) ;
#75623 = CARTESIAN_POINT ( 'NONE',  ( 5.533136088152891929, 9.469426179571447832, -0.7216878364870458196 ) ) ;
#75624 = CARTESIAN_POINT ( 'NONE',  ( 4.463939829769240752, 0.8331255105114807602, 1.561325262609781772 ) ) ;
#75625 = CARTESIAN_POINT ( 'NONE',  ( 9.423080456697809026, 10.95234760669099749, -1.199719254218446718 ) ) ;
#75626 = CARTESIAN_POINT ( 'NONE',  ( 0.6925746140923200178, -2.090094003047581861, -0.2575201054717362048 ) ) ;
#75628 = CARTESIAN_POINT ( 'NONE',  ( -0.7500000000000215383, 1.691666666666688634, 1.299038105676659116 ) ) ;
#75627 = CARTESIAN_POINT ( 'NONE',  ( -1.364683531250000748, 10.85937500034139802, 0.000000000000000000 ) ) ;
#75629 = CARTESIAN_POINT ( 'NONE',  ( 0.7132589462262963753, -1.661971685727476000, -1.056574055910926013 ) ) ;
#75630 = MECHANICAL_DESIGN_GEOMETRIC_PRESENTATION_REPRESENTATION (  '', ( #99744 ), #79023 ) ;
#75631 = CARTESIAN_POINT ( 'NONE',  ( -3.447516199624892419, 7.244129009529488350, 0.7998128361456352531 ) ) ;
#75632 = CARTESIAN_POINT ( 'NONE',  ( -0.4897149945007619465, 7.513091487862089579, -2.015070445391653475 ) ) ;
#75634 = ORIENTED_EDGE ( 'NONE', *, *, #75639, .T. ) ;
#75633 = CARTESIAN_POINT ( 'NONE',  ( 5.220911918456066836, 1.366450397884883428, -1.189473885788590035 ) ) ;
#75635 = CARTESIAN_POINT ( 'NONE',  ( 5.829642864196151741, 9.745074408296771296, 0.7216878364870438212 ) ) ;
#75636 = CARTESIAN_POINT ( 'NONE',  ( 4.504681594071535677, 1.446009304718363087, -1.186774495104812699 ) ) ;
#75637 = CARTESIAN_POINT ( 'NONE',  ( 4.293848342403890683, -1.423947089648310849, -1.503027170334819029 ) ) ;
#75638 = CARTESIAN_POINT ( 'NONE',  ( -0.6125000000000192513, 1.958333333333318826, -1.060881119635962211 ) ) ;
#75639 = EDGE_CURVE ( 'NONE', #74995, #139509, #107952, .T. ) ;
#75640 = CARTESIAN_POINT ( 'NONE',  ( -5.438229012412890917, 8.398332043573416783, -1.082531754730549967 ) ) ;
#75641 = PRESENTATION_STYLE_ASSIGNMENT (( #155828 ) ) ;
#75642 = CARTESIAN_POINT ( 'NONE',  ( 7.214910300766615769, 11.56914578420308715, -0.7998128361456291469 ) ) ;
#75643 = CARTESIAN_POINT ( 'NONE',  ( -10.32861409551237486, 10.94447128771960287, 1.040834085586084257E-14 ) ) ;
#75644 = CARTESIAN_POINT ( 'NONE',  ( 9.367496997597598352, 4.518459255872631530, 7.500000000000000000 ) ) ;
#75645 = CARTESIAN_POINT ( 'NONE',  ( 5.066578194877104480, 4.909125722664362534, -0.2447466197543680111 ) ) ;
#75646 = CARTESIAN_POINT ( 'NONE',  ( -1.201851678989727383E-14, 5.259375000341421469, -1.575800808251660134 ) ) ;
#75647 = CARTESIAN_POINT ( 'NONE',  ( 4.475024536774164119, 1.792854848340214025, 0.7970393728587571447 ) ) ;
#75648 = CARTESIAN_POINT ( 'NONE',  ( 1.546249734355091388, 1.863884247081739831, -0.7690006294575403301 ) ) ;
#75649 = CARTESIAN_POINT ( 'NONE',  ( -4.228163802615396705, 6.026220084508304708, -1.599625672291271394 ) ) ;
#75650 = CARTESIAN_POINT ( 'NONE',  ( 6.639320575229255006, 4.698690022235154196, 2.459427960261594048 ) ) ;
#75651 = CARTESIAN_POINT ( 'NONE',  ( 0.8603690976232807319, -1.359099942111790416, 1.285485254608226269 ) ) ;
#75652 = CARTESIAN_POINT ( 'NONE',  ( -0.6823417656249969321, 3.967708333674754950, -1.181850606188749264 ) ) ;
#75653 = CARTESIAN_POINT ( 'NONE',  ( 3.586193004068451540, 1.121915001286919233, 1.671427700405977212 ) ) ;
#75655 = CARTESIAN_POINT ( 'NONE',  ( 3.392305424709577188, -0.8603400307676151160, -1.934732246027433433 ) ) ;
#75654 = CARTESIAN_POINT ( 'NONE',  ( -7.049876689426121779, 7.327203680526343632, -0.7216878364870278340 ) ) ;
#75656 = CARTESIAN_POINT ( 'NONE',  ( 1.500000000000013545, 5.035416667349488229, 0.8660254037844385966 ) ) ;
#75657 = CARTESIAN_POINT ( 'NONE',  ( 4.369627354678314646, -0.3570511267821044332, 2.039192500141631115 ) ) ;
#75658 = CARTESIAN_POINT ( 'NONE',  ( 5.494797395288433250, 9.632623737803665875, 0.000000000000000000 ) ) ;
#75660 = CARTESIAN_POINT ( 'NONE',  ( 6.620655732516684822, 7.052296306484477029, 2.671890196246820004 ) ) ;
#75659 = CARTESIAN_POINT ( 'NONE',  ( 6.580031098407260082, -2.049997751086956921, -0.4092652541880793526 ) ) ;
#75662 = VERTEX_POINT ( 'NONE', #141408 ) ;
#75661 = CARTESIAN_POINT ( 'NONE',  ( 4.858326754937916547, 0.6996357133068830114, 1.686392194618462570 ) ) ;
#75663 = CARTESIAN_POINT ( 'NONE',  ( 8.589254009457354400, 9.979550084910457031, -1.199719254218446718 ) ) ;
#75664 = CARTESIAN_POINT ( 'NONE',  ( 1.299038105676669330, 6.499999999999999112, 0.7500000000000006661 ) ) ;
#75665 = CARTESIAN_POINT ( 'NONE',  ( 9.681426354872456841, 13.43812210156014508, -8.165041025796162089 ) ) ;
#75666 = CARTESIAN_POINT ( 'NONE',  ( -10.76112648294250462, 4.189587671054875173, 6.709456861673908534 ) ) ;
#75667 = CARTESIAN_POINT ( 'NONE',  ( -0.6823417656250003738, 12.46354166700806765, 1.181850606188754593 ) ) ;
#75668 = CARTESIAN_POINT ( 'NONE',  ( 6.182274467271688501, 0.9872068455926674702, 1.637624497839342608 ) ) ;
#75669 = CARTESIAN_POINT ( 'NONE',  ( -8.941766003412679353, 10.39081407785832845, -1.199719254218446718 ) ) ;
#75670 = TOROIDAL_SURFACE ( 'NONE', #214011, 1.924999999999999822, 0.1000000000000000056 ) ;
#75671 = CARTESIAN_POINT ( 'NONE',  ( 6.494519276145969577, 7.535692896047149425, -1.199719254218446718 ) ) ;
#75672 = CARTESIAN_POINT ( 'NONE',  ( -11.78331023100045627, 11.29999999999999893, -1.800000000000001155 ) ) ;
#75673 = FACE_OUTER_BOUND ( 'NONE', #99300, .T. ) ;
#75674 = CARTESIAN_POINT ( 'NONE',  ( 3.337278367258157630, 7.045241861776501580, 0.7998128361456341429 ) ) ;
#75675 = VERTEX_POINT ( 'NONE', #137104 ) ;
#75676 = CARTESIAN_POINT ( 'NONE',  ( -6.505933609711270549, 8.683618192786854095, -1.599625672291271394 ) ) ;
#75677 = CARTESIAN_POINT ( 'NONE',  ( 5.396111305808362957, -0.9091601233324579923, -1.799916296964368279 ) ) ;
#75679 = CARTESIAN_POINT ( 'NONE',  ( 6.099189001301251523, 8.209082816308541197, 1.599625672291268286 ) ) ;
#75678 = CARTESIAN_POINT ( 'NONE',  ( 0.000000000000000000, -0.5000000000000004441, 0.000000000000000000 ) ) ;
#75680 = DIRECTION ( 'NONE',  ( 0.5131086435338284568, -0.8583236685137343169, -8.049116928532389848E-16 ) ) ;
#75681 = CARTESIAN_POINT ( 'NONE',  ( 0.1394461523057136665, 6.947783040739019533, -2.314776707679897516 ) ) ;
#75682 = CARTESIAN_POINT ( 'NONE',  ( -4.690757960648240577, 6.495636925554817864, 1.443375672974064550 ) ) ;
#75683 = CARTESIAN_POINT ( 'NONE',  ( 4.857899112398166075, 4.561970474086296079, 1.040834085586084257E-14 ) ) ;
#75684 = CARTESIAN_POINT ( 'NONE',  ( 2.201947278869041291, 0.7584239558163529127, -1.817761916770490149 ) ) ;
#75685 = CARTESIAN_POINT ( 'NONE',  ( 3.409779952838042583, -1.203371721269937744, -1.617806234278630573 ) ) ;
#75686 = CARTESIAN_POINT ( 'NONE',  ( -8.505042434474312074, 8.816971016508505343, -0.7998128361456291469 ) ) ;
#75687 = CARTESIAN_POINT ( 'NONE',  ( 6.727182134110196721, 6.033756510516266935, 2.783943001041962795 ) ) ;
#75688 = CARTESIAN_POINT ( 'NONE',  ( 3.591891977137162684, -2.188917585555647527, -0.1077332384093188100 ) ) ;
#75689 = CARTESIAN_POINT ( 'NONE',  ( 9.406473561382165727, 4.446947634372959257, -7.380697597781017194 ) ) ;
#75690 = CARTESIAN_POINT ( 'NONE',  ( 2.045805558669851365, 0.7393754583576680472, -1.779040955004469904 ) ) ;
#75691 = CARTESIAN_POINT ( 'NONE',  ( -7.133561379084627063, 11.47423870890741782, 0.7998128361456481317 ) ) ;
#75692 = CARTESIAN_POINT ( 'NONE',  ( 0.2333540202161427102, 1.346341334450983140, -2.298657068330804076 ) ) ;
#75693 = CARTESIAN_POINT ( 'NONE',  ( 7.259501185113382604, 10.55683625168592243, -1.199719254218441611 ) ) ;
#75694 = CARTESIAN_POINT ( 'NONE',  ( 5.392392409933256303, 7.314210449720692786, 1.599625672291267398 ) ) ;
#75695 = FACE_OUTER_BOUND ( 'NONE', #93870, .T. ) ;
#75696 = CARTESIAN_POINT ( 'NONE',  ( 4.584065335196261692, 7.401807753487379848, 1.082531754730549078 ) ) ;
#75697 = ORIENTED_EDGE ( 'NONE', *, *, #147938, .F. ) ;
#75699 = CARTESIAN_POINT ( 'NONE',  ( 3.422524054001755633, -0.8179560535927836717, -1.839607883820688405 ) ) ;
#75698 = CARTESIAN_POINT ( 'NONE',  ( 6.480030769895370746, -1.807141314969593848, -0.3518929191878711338 ) ) ;
#75700 = CARTESIAN_POINT ( 'NONE',  ( 4.587492961451061113, 1.418373992658492400, -1.808456645134959073 ) ) ;
#75702 = CARTESIAN_POINT ( 'NONE',  ( 3.361990069819278837, -1.859032935646281581, 0.08664877711485326206 ) ) ;
#75701 = CARTESIAN_POINT ( 'NONE',  ( -0.1288028175206361037, 4.078893953557697571, -2.828657143142800034 ) ) ;
#75703 = CARTESIAN_POINT ( 'NONE',  ( 5.854088466050551887, 10.05179665369283981, 0.7998128361456341429 ) ) ;
#75704 = CARTESIAN_POINT ( 'NONE',  ( 11.94655611907589865, 11.15200944546904083, -1.134828163062138628 ) ) ;
#75705 = CARTESIAN_POINT ( 'NONE',  ( 6.433860211133586304, -1.853236450885078712, 0.4715264990977630077 ) ) ;
#75706 = CARTESIAN_POINT ( 'NONE',  ( -8.182509401047415309, 9.505014708432145909, 1.199719254218462483 ) ) ;
#75707 = CARTESIAN_POINT ( 'NONE',  ( -4.177320726786315497, 7.887641591310407208, -0.7216878364870458196 ) ) ;
#75708 = CARTESIAN_POINT ( 'NONE',  ( 5.565992953457829628, -1.325659382304938960, 1.616758296502271097 ) ) ;
#75709 = CARTESIAN_POINT ( 'NONE',  ( 6.697364695470787943, 7.876308901879812474, -1.082531754730543083 ) ) ;
#75710 = EDGE_LOOP ( 'NONE', ( #24572, #144958 ) ) ;
#75711 = AXIS2_PLACEMENT_3D ( 'NONE', #113469, #130782, #143812 ) ;
#75712 = DIRECTION ( 'NONE',  ( 0.000000000000000000, 1.804652791718263484E-16, -1.000000000000000000 ) ) ;
#75713 = CARTESIAN_POINT ( 'NONE',  ( -3.380278471875000523, -0.05468749976102194044, 0.000000000000000000 ) ) ;
#75714 = CARTESIAN_POINT ( 'NONE',  ( 6.147054438156498435, -1.453121625630097613, 0.9290195162147057983 ) ) ;
#75715 = CARTESIAN_POINT ( 'NONE',  ( -3.927058049452637700, 7.733318157670055371, -0.7998128361456281477 ) ) ;
#75716 = CARTESIAN_POINT ( 'NONE',  ( 1.283399958720226497, 1.417952419849175305, -0.9979722560638002449 ) ) ;
#75717 = CARTESIAN_POINT ( 'NONE',  ( 0.000000000000000000, 13.49999999999999822, 0.000000000000000000 ) ) ;
#75718 = CARTESIAN_POINT ( 'NONE',  ( 1.284279953904119864, 3.296639714193937198, -0.7749999999999910294 ) ) ;
#75719 = CARTESIAN_POINT ( 'NONE',  ( 5.577072259002747501, 2.003115288890752410, 0.8377749483753393900 ) ) ;
#75720 = CARTESIAN_POINT ( 'NONE',  ( 4.107882937833263526, -1.820653182827164596, 0.1363937739093170898 ) ) ;
#75721 = CARTESIAN_POINT ( 'NONE',  ( 2.395295693335119935, -1.754585731169123752, 0.8775363634117984146 ) ) ;
#75722 =( NAMED_UNIT ( * ) PLANE_ANGLE_UNIT ( ) SI_UNIT ( $, .RADIAN. ) );
#75723 = CARTESIAN_POINT ( 'NONE',  ( -9.775592450653132204, 11.36361159963886891, -1.199719254218441611 ) ) ;
#75724 = CARTESIAN_POINT ( 'NONE',  ( 8.599949509769960088, 8.927695937686774386, 1.040834085586084257E-14 ) ) ;
#75725 = EDGE_CURVE ( 'NONE', #134523, #43808, #160859, .T. ) ;
#75726 = CARTESIAN_POINT ( 'NONE',  ( 2.789816089392273213, 2.012775272720100705, -0.6673941125509493810 ) ) ;
#75727 = DIRECTION ( 'NONE',  ( -1.000000000000000000, 0.000000000000000000, 0.000000000000000000 ) ) ;
#75728 = CIRCLE ( 'NONE', #51622, 0.08000000000000020983 ) ;
#75729 = CARTESIAN_POINT ( 'NONE',  ( -5.294420283343134415, 6.244149675475041406, 1.216503418957364246 ) ) ;
#75730 = CARTESIAN_POINT ( 'NONE',  ( -5.472563271839127275, 6.275773694203630626, -1.010060153610029321 ) ) ;
#75731 = CARTESIAN_POINT ( 'NONE',  ( 0.4267348894952603944, -1.354911996285239617, 1.565345633960464111 ) ) ;
#75733 = CARTESIAN_POINT ( 'NONE',  ( 1.500000000000001332, 13.90625000068279604, 0.000000000000000000 ) ) ;
#75732 = CARTESIAN_POINT ( 'NONE',  ( -10.56357071321730778, 4.163828001052541694, 5.599134949294604979 ) ) ;
#75735 = ORIENTED_EDGE ( 'NONE', *, *, #101217, .F. ) ;
#75734 = CARTESIAN_POINT ( 'NONE',  ( 3.334858576441266376, 1.407893888572855801, -1.718160706149525430 ) ) ;
#75736 = CARTESIAN_POINT ( 'NONE',  ( 0.7569315055401154568, 2.213468045025353881, -0.6199256774504552370 ) ) ;
#75738 = CARTESIAN_POINT ( 'NONE',  ( 6.561391914609854936, 1.711577788671992062, 1.150682440272139617 ) ) ;
#75737 = CARTESIAN_POINT ( 'NONE',  ( 2.184835310096557404, 5.700724961754617404, 1.040834085586084257E-14 ) ) ;
#75740 = CARTESIAN_POINT ( 'NONE',  ( -3.475000000000000533, -0.3499999999999996447, 0.000000000000000000 ) ) ;
#75739 = CARTESIAN_POINT ( 'NONE',  ( 5.065906673361608270, 5.939254536123854677, -1.199719254218450271 ) ) ;
#75741 = DIRECTION ( 'NONE',  ( 0.000000000000000000, -1.000000000000000000, 0.000000000000000000 ) ) ;
#75742 = CARTESIAN_POINT ( 'NONE',  ( 6.567912610837368881, -1.126952994821692533, 1.456688911285822119 ) ) ;
#75743 = FILL_AREA_STYLE_COLOUR ( '', #205041 ) ;
#75744 = CARTESIAN_POINT ( 'NONE',  ( -0.2104748580754183529, 0.2283854016844401591, -2.137091067173245929 ) ) ;
#75745 = CARTESIAN_POINT ( 'NONE',  ( 2.836578922267366742, 0.2088710044844780678, 1.711989638784001677 ) ) ;
#75746 = CARTESIAN_POINT ( 'NONE',  ( 1.042204282965590201, 0.8216761606248854655, 1.841732292558920570 ) ) ;
#75747 = CARTESIAN_POINT ( 'NONE',  ( 2.444286548701213757, -2.001697433659669567, -1.129998469374261072 ) ) ;
#75748 =( BOUNDED_CURVE ( )  B_SPLINE_CURVE ( 2, ( #164453, #100515, #135177, #166590, #134123, #200132, #51785 ),
 .UNSPECIFIED., .F., .T. ) 
 B_SPLINE_CURVE_WITH_KNOTS ( ( 3, 2, 2, 3 ),
 ( 0.4000000000000005773, 0.4083333333333336590, 0.4166666666666667407, 0.4249999999999998224 ),
 .UNSPECIFIED. ) 
 CURVE ( )  GEOMETRIC_REPRESENTATION_ITEM ( )  RATIONAL_B_SPLINE_CURVE ( ( 0.9999999999999911182, 0.8660254037844475894, 1.000000000000000000, 0.8660254037844387076, 1.000000000000000000, 0.8660254037844413721, 0.9999999999999973355 ) ) 
 REPRESENTATION_ITEM ( '' )  );
#75749 = CARTESIAN_POINT ( 'NONE',  ( 3.216390312923810502, -1.112095606969863759, -1.970117241612897363 ) ) ;
#75750 = CARTESIAN_POINT ( 'NONE',  ( 5.233084072137057063, 0.1537158111805384808, 2.100522205955375199 ) ) ;
#75751 = CARTESIAN_POINT ( 'NONE',  ( -6.455090533882206216, 7.663932056684933158, -1.082531754730549967 ) ) ;
#75752 = CARTESIAN_POINT ( 'NONE',  ( 3.549836697621409964, 1.769921775324476698, 0.002857994197370468913 ) ) ;
#75754 = CARTESIAN_POINT ( 'NONE',  ( 6.427265082780700745, -1.493544900618107185, -1.739104490089713462 ) ) ;
#75753 = CARTESIAN_POINT ( 'NONE',  ( 5.194182247366881278, 5.232503174782402233, 0.7216878364870328300 ) ) ;
#75755 = CARTESIAN_POINT ( 'NONE',  ( 5.156134521940135329, -1.331146486249596306, 1.272188372451001026 ) ) ;
#75756 = CARTESIAN_POINT ( 'NONE',  ( -5.773074481320628948, 5.629675071162500544, 0.000000000000000000 ) ) ;
#75757 = CIRCLE ( 'NONE', #58443, 2.750000000000008438 ) ;
#75758 = CARTESIAN_POINT ( 'NONE',  ( 4.460269348771534581, 8.147471973634706544, -0.7216878364870207285 ) ) ;
#75759 = CARTESIAN_POINT ( 'NONE',  ( 1.499999999999987121, 4.045833333333359150, -0.8660254037844323793 ) ) ;
#75760 = CARTESIAN_POINT ( 'NONE',  ( 4.171962795014371395, -1.262591954434747921, 1.790989659139609946 ) ) ;
#75761 = CARTESIAN_POINT ( 'NONE',  ( -3.541704441667874903, 5.155074486744371853, -1.599625672291256295 ) ) ;
#75762 = DIRECTION ( 'NONE',  ( 1.000000000000000000, -0.000000000000000000, -0.000000000000000000 ) ) ;
#75763 =( BOUNDED_SURFACE ( )  B_SPLINE_SURFACE ( 3, 2, ( 
 ( #109535, #23923, #175539 ),
 ( #5518, #90028, #147299 ),
 ( #81218, #64951, #15130 ),
 ( #112726, #127945, #178736 ),
 ( #27129, #95371, #111658 ),
 ( #31414, #160342, #79080 ) ),
 .UNSPECIFIED., .F., .F., .F. ) 
 B_SPLINE_SURFACE_WITH_KNOTS ( ( 4, 2, 4 ),
 ( 3, 3 ),
 ( 0.000000000000000000, 0.0003766405729503176413, 0.0007532811459006352826 ),
 ( 0.000000000000000000, 1.000000000000000000 ),
 .UNSPECIFIED. ) 
 GEOMETRIC_REPRESENTATION_ITEM ( )  RATIONAL_B_SPLINE_SURFACE ( (
 ( 1.000000000000000000, 0.7071067811865551223, 1.000000000000000000),
 ( 1.000000000000000000, 0.7211294902953071517, 1.000000000000000000),
 ( 1.000000000000000000, 0.7311181975231312302, 1.000000000000000000),
 ( 1.000000000000000000, 0.7429553055060466038, 1.000000000000000000),
 ( 1.000000000000000000, 0.7451698531058986719, 1.000000000000000000),
 ( 1.000000000000000000, 0.7452309222763021657, 1.000000000000000000) ) ) 
 REPRESENTATION_ITEM ( '' )  SURFACE ( )  );
#75764 = CARTESIAN_POINT ( 'NONE',  ( 5.881320641815353412, -0.05461762546566179682, 2.069818975884097689 ) ) ;
#75765 = CARTESIAN_POINT ( 'NONE',  ( -0.1003747550864658999, -1.976661868047492998, 0.3981153667176607902 ) ) ;
#75766 = CARTESIAN_POINT ( 'NONE',  ( -1.364683531250010295, 5.238541667008086655, -0.7879004041258300672 ) ) ;
#75767 = CARTESIAN_POINT ( 'NONE',  ( 3.563037003841040828, -1.699336121007990918, -0.9075540061579747686 ) ) ;
#75768 = CARTESIAN_POINT ( 'NONE',  ( 1.364683531250000303, 10.25520833367473017, -0.7879004041258355073 ) ) ;
#75769 = CARTESIAN_POINT ( 'NONE',  ( -3.226477370372317743, 4.787309570232886280, 1.443375672974064550 ) ) ;
#75770 = CARTESIAN_POINT ( 'NONE',  ( 6.416280414004661203, -2.120105685773795212, 0.05337830808049835035 ) ) ;
#75771 = ORIENTED_EDGE ( 'NONE', *, *, #54015, .F. ) ;
#75773 = CARTESIAN_POINT ( 'NONE',  ( -7.253242555595325491, -7.896420114627995979, 6.595517585942709538 ) ) ;
#75772 = CARTESIAN_POINT ( 'NONE',  ( -4.394251184604987870, 5.259619482528146150, 1.082531754730549078 ) ) ;
#75774 = CARTESIAN_POINT ( 'NONE',  ( 4.680589345215795838, 6.483773540883647435, -1.599625672291256295 ) ) ;
#75775 =( NAMED_UNIT ( * ) SI_UNIT ( $, .STERADIAN. ) SOLID_ANGLE_UNIT ( ) );
#75776 = CARTESIAN_POINT ( 'NONE',  ( -6.427974226210522168, 6.671927150099951298, 0.000000000000000000 ) ) ;
#75777 = AXIS2_PLACEMENT_3D ( 'NONE', #158239, #9828, #206959 ) ;
#75778 = CARTESIAN_POINT ( 'NONE',  ( 11.95134215679451373, 7.565930823690049323, -0.2097427604813490720 ) ) ;
#75779 = CARTESIAN_POINT ( 'NONE',  ( 8.690413276235306128, 13.08263988900915109, -0.7216878364870267237 ) ) ;
#75780 = CARTESIAN_POINT ( 'NONE',  ( 1.363640982571033611, -0.4799814350611387725, 1.902108589862220311 ) ) ;
#75781 = CARTESIAN_POINT ( 'NONE',  ( 1.364683531249986537, 1.467708333674748289, -0.7879004041258239610 ) ) ;
#75782 = DIRECTION ( 'NONE',  ( 0.8660254037844363761, 0.000000000000000000, -0.5000000000000041078 ) ) ;
#75783 = CARTESIAN_POINT ( 'NONE',  ( 5.846142468697441252, -0.8834969228576605715, 1.751761657833034613 ) ) ;
#75784 = CARTESIAN_POINT ( 'NONE',  ( -8.507905087775398556, 9.884643009614800135, 1.199719254218462483 ) ) ;
#75785 = CARTESIAN_POINT ( 'NONE',  ( -5.138177029454855216, 7.017625839162543677, 1.443375672974064550 ) ) ;
#75786 = CARTESIAN_POINT ( 'NONE',  ( 6.420800710400103917, 2.015122584031241004, 0.7829223626853940576 ) ) ;
#75788 = ORIENTED_EDGE ( 'NONE', *, *, #156207, .F. ) ;
#75787 = CARTESIAN_POINT ( 'NONE',  ( -0.1833053738655555376, -5.341077028191798526, -10.96562622554679578 ) ) ;
#75789 = CARTESIAN_POINT ( 'NONE',  ( 1.499999999999987121, -0.7145833326505161009, 0.8660254037844524744 ) ) ;
#75790 = CARTESIAN_POINT ( 'NONE',  ( 0.2099203756031532975, -0.7936979409460078738, -1.692237190125941648 ) ) ;
#75791 = CARTESIAN_POINT ( 'NONE',  ( 6.327464733921618567, -1.223274778582748246, 1.229020038707399065 ) ) ;
#75793 = CARTESIAN_POINT ( 'NONE',  ( 2.806388347806953121, 1.585463108415147149, -1.513251884624075672 ) ) ;
#75792 = CARTESIAN_POINT ( 'NONE',  ( -1.360316468750046859, 0.3697916670080757529, -0.7853790794159101196 ) ) ;
#75794 = CARTESIAN_POINT ( 'NONE',  ( 4.419161195688524835, 2.107920515157933661, 0.9393535314214102039 ) ) ;
#75795 = CARTESIAN_POINT ( 'NONE',  ( 6.766874334510889710, -1.882258232876810045, -0.8394616043497000746 ) ) ;
#75796 = CARTESIAN_POINT ( 'NONE',  ( 2.589705103518041618, -1.936761303218867969, -0.1426656448052856518 ) ) ;
#75797 = CARTESIAN_POINT ( 'NONE',  ( -4.975479186090865369, 6.827811688571220117, 1.443375672974064550 ) ) ;
#75798 = DIRECTION ( 'NONE',  ( -0.06183953750877529965, 0.9962285034897226943, -0.06086575749408236480 ) ) ;
#75799 = CARTESIAN_POINT ( 'NONE',  ( 5.379186226027963258, -1.918017450862268714, -0.9047448674902383026 ) ) ;
#75800 = CARTESIAN_POINT ( 'NONE',  ( 3.463517678199812266, -1.944071305346905643, -0.5350885120067662148 ) ) ;
#75801 = CARTESIAN_POINT ( 'NONE',  ( -4.067082893975237035, 7.688754443039000464, 1.040834085586084257E-14 ) ) ;
#75802 = CARTESIAN_POINT ( 'NONE',  ( -6.688968683495758683, 8.897159112202094988, -1.599625672291271394 ) ) ;
#75803 = CARTESIAN_POINT ( 'NONE',  ( 9.585778300061798873, 11.14216175728232550, -1.199719254218440723 ) ) ;
#75804 = CARTESIAN_POINT ( 'NONE',  ( 8.633759933988839975E-16, 0.000000000000000000, -7.049999999999999822 ) ) ;
#75805 = CARTESIAN_POINT ( 'NONE',  ( -6.961185525973791144, 7.086080966583015339, 0.7998128361456341429 ) ) ;
#75806 = CARTESIAN_POINT ( 'NONE',  ( -0.08011315927826534455, 15.51845603285927488, 11.99973258290723699 ) ) ;
#75807 = CARTESIAN_POINT ( 'NONE',  ( -10.37901820579008039, 4.889546506944066451, 5.358714317323078014 ) ) ;
#75808 = EDGE_LOOP ( 'NONE', ( #8156, #120746 ) ) ;
#75809 = CARTESIAN_POINT ( 'NONE',  ( 5.172756020173422620, -1.939746602593624081, -0.6965250322775017322 ) ) ;
#75810 = CARTESIAN_POINT ( 'NONE',  ( -5.261973015435229328, 9.153069261400824885, 0.000000000000000000 ) ) ;
#75811 = CARTESIAN_POINT ( 'NONE',  ( 8.136301581532414673, 8.664975731308866003, 0.000000000000000000 ) ) ;
#75812 = CARTESIAN_POINT ( 'NONE',  ( -5.413783410558481002, 5.210502155273325720, -0.7998128361456221525 ) ) ;
#75813 = FACE_OUTER_BOUND ( 'NONE', #7587, .T. ) ;
#75814 = CARTESIAN_POINT ( 'NONE',  ( 4.301429021398018193, 1.803172560858562701, -0.9099306128727399079 ) ) ;
#75816 = ORIENTED_EDGE ( 'NONE', *, *, #117680, .F. ) ;
#75815 = CARTESIAN_POINT ( 'NONE',  ( -1.500000000000001332, 0.6500000000000255573, 0.000000000000000000 ) ) ;
#75818 = CARTESIAN_POINT ( 'NONE',  ( 7.619319141200051604, 11.83303006480134911, 0.7216878364870438212 ) ) ;
#75817 = CARTESIAN_POINT ( 'NONE',  ( -6.005335696210345020, 5.970922831858983315, 0.7998128361456281477 ) ) ;
#75819 = CARTESIAN_POINT ( 'NONE',  ( 4.645640190976921602, 8.571663989448405019, 1.040834085586084257E-14 ) ) ;
#75820 = CARTESIAN_POINT ( 'NONE',  ( 3.977457805978751093, 1.941116309567689324, -0.6927405623450531014 ) ) ;
#75821 = CARTESIAN_POINT ( 'NONE',  ( 3.252577435111691617, 1.966644794889658820, -0.4445022851852917234 ) ) ;
#75822 = ORIENTED_EDGE ( 'NONE', *, *, #171420, .T. ) ;
#75823 = CARTESIAN_POINT ( 'NONE',  ( 2.855963913973019963, 6.483708332943829866, 0.000000000000000000 ) ) ;
#75824 =( BOUNDED_CURVE ( )  B_SPLINE_CURVE ( 3, ( #117464, #1480, #65423, #132618 ),
 .UNSPECIFIED., .F., .T. ) 
 B_SPLINE_CURVE_WITH_KNOTS ( ( 4, 4 ),
 ( 4.845169979278623806, 4.852380668139161912 ),
 .UNSPECIFIED. ) 
 CURVE ( )  GEOMETRIC_REPRESENTATION_ITEM ( )  RATIONAL_B_SPLINE_CURVE ( ( 1.000000000000000000, 0.9999956671685397147, 0.9999956671685397147, 1.000000000000000000 ) ) 
 REPRESENTATION_ITEM ( '' )  );
#75825 = MECHANICAL_DESIGN_GEOMETRIC_PRESENTATION_REPRESENTATION (  '', ( #30698 ), #48180 ) ;
#75827 = ORIENTED_EDGE ( 'NONE', *, *, #2635, .F. ) ;
#75826 = CARTESIAN_POINT ( 'NONE',  ( -11.55950211276791428, 9.719999999999982876, 3.221476510067114329 ) ) ;
#75828 = CARTESIAN_POINT ( 'NONE',  ( 5.772745519453025054, 7.247817053759448847, -1.191736586928717978 ) ) ;
#75829 = CARTESIAN_POINT ( 'NONE',  ( 2.548203688163702463, 1.844428314090811538, -0.8144999995377337765 ) ) ;
#75830 = CARTESIAN_POINT ( 'NONE',  ( 2.818100271072516261, 1.733748696238574416, 0.6199764264002775027 ) ) ;
#75831 = CARTESIAN_POINT ( 'NONE',  ( 0.8917866929778429652, 2.032703844138737725, -1.092514170908296833 ) ) ;
#75832 = CARTESIAN_POINT ( 'NONE',  ( 4.980641328173811999, 6.904110530993182948, 1.599625672291269396 ) ) ;
#75833 = CARTESIAN_POINT ( 'NONE',  ( 3.638091081701349871, 0.9754702174074175725, -1.929073278114090684 ) ) ;
#75834 = CARTESIAN_POINT ( 'NONE',  ( -6.063521013809733518, 8.097193820909906137, 1.599625672291283607 ) ) ;
#75835 = CARTESIAN_POINT ( 'NONE',  ( 2.988014862494779322, 2.163403104293510459, 0.7763308700806015317 ) ) ;
#75836 = VERTEX_POINT ( 'NONE', #121995 ) ;
#75837 = LINE ( 'NONE', #176540, #135719 ) ;
#75838 = CARTESIAN_POINT ( 'NONE',  ( 1.393192293617943944, 1.414286473764417185, 1.224485199485196629 ) ) ;
#75839 = CARTESIAN_POINT ( 'NONE',  ( 6.069206959712960980, 0.1456670527590266107, -1.966150735595481258 ) ) ;
#75841 = CARTESIAN_POINT ( 'NONE',  ( 9.544576953896278582, 10.23768732240824164, 0.000000000000000000 ) ) ;
#75840 = CARTESIAN_POINT ( 'NONE',  ( 0.6823417656249917140, 5.342708333674749177, 1.181850606188765695 ) ) ;
#75843 = CARTESIAN_POINT ( 'NONE',  ( 1.067327838873022516, -1.996528553209110379, -0.9406146916221403975 ) ) ;
#75842 = CARTESIAN_POINT ( 'NONE',  ( -7.074657228232555717, 7.148188275893099686, 1.040834085586084257E-14 ) ) ;
#75844 = DIRECTION ( 'NONE',  ( -0.8660254037844328234, 0.000000000000000000, 0.5000000000000102141 ) ) ;
#75845 = CARTESIAN_POINT ( 'NONE',  ( 5.250031796989762967, 7.148123067953287446, 1.599625672291267398 ) ) ;
#75846 = CARTESIAN_POINT ( 'NONE',  ( -5.599681137644054729, 6.491715067794862293, 1.199719254218450271 ) ) ;
#75847 = CARTESIAN_POINT ( 'NONE',  ( 6.639320575229257670, 3.688898292602959650, 2.617366112374151399 ) ) ;
#75848 = CARTESIAN_POINT ( 'NONE',  ( 4.575049868665863606, 0.0009985144121069796600, -1.971640593447765655 ) ) ;
#75849 = CARTESIAN_POINT ( 'NONE',  ( 5.760475268203285815, 0.9300522481428794563, 2.112166060234192511 ) ) ;
#75850 = CARTESIAN_POINT ( 'NONE',  ( 5.512096448594467901, 1.858919848428818300, -0.09134777953435403719 ) ) ;
#75851 = CARTESIAN_POINT ( 'NONE',  ( 3.555586659033848740, 1.623084692090390080, 1.272569074839409398 ) ) ;
#75852 = CARTESIAN_POINT ( 'NONE',  ( 5.992340707560147806, 8.974519344586754599, 1.082531754730558626 ) ) ;
#75853 = CARTESIAN_POINT ( 'NONE',  ( 2.925527285498711549, 6.635141943048991742, 0.7998128361456281477 ) ) ;
#75854 = CARTESIAN_POINT ( 'NONE',  ( 1.364683531249986537, 1.467708333674748289, -0.7879004041258239610 ) ) ;
#75855 = CARTESIAN_POINT ( 'NONE',  ( -0.006800380015319074101, 7.009756401597622144, 1.999988438674507485 ) ) ;
#75856 = CARTESIAN_POINT ( 'NONE',  ( 5.951666246274797345, 7.966696592119163256, 1.443375672974062551 ) ) ;
#75857 = CARTESIAN_POINT ( 'NONE',  ( 4.984931625306495029, 2.076298541577546342, 0.6347802954964998357 ) ) ;
#75859 = CARTESIAN_POINT ( 'NONE',  ( 3.825598141381767903, 0.9817388958630569595, -1.557492293685861284 ) ) ;
#75858 = CARTESIAN_POINT ( 'NONE',  ( -2.657034918598345730, 5.083329257464595408, -1.082531754730543971 ) ) ;
#75860 = B_SPLINE_CURVE_WITH_KNOTS ( 'NONE', 3,
 ( #112343, #196719, #180472, #144818, #32087, #165278 ),
 .UNSPECIFIED., .F., .F.,
 ( 4, 2, 4 ),
 ( 0.8940582275390620559, 0.9471490438394758460, 1.000239860139889636 ),
 .UNSPECIFIED. ) ;
#75861 = EDGE_CURVE ( 'NONE', #16624, #53408, #470, .T. ) ;
#75863 = CARTESIAN_POINT ( 'NONE',  ( 6.720655732516650716, 2.975630972093906923, 2.379814465338329743 ) ) ;
#75862 = DIRECTION ( 'NONE',  ( -1.000000000000000000, 0.000000000000000000, 0.000000000000000000 ) ) ;
#75864 = CARTESIAN_POINT ( 'NONE',  ( 6.163654587501778970, 1.125051486859941718, 1.880622087419632882 ) ) ;
#75865 = DIRECTION ( 'NONE',  ( -0.6507913734559640506, -0.7592566023653004592, 0.000000000000000000 ) ) ;
#75866 = CARTESIAN_POINT ( 'NONE',  ( 0.3337811221923889793, -2.067640401758659596, 0.9186946961548744239 ) ) ;
#75867 = CARTESIAN_POINT ( 'NONE',  ( -3.976511113072466408, 7.848157239995420476, -0.08586869108932922157 ) ) ;
#75868 = DIRECTION ( 'NONE',  ( 0.000000000000000000, 0.000000000000000000, 1.000000000000000000 ) ) ;
#75869 = CARTESIAN_POINT ( 'NONE',  ( 6.333059215844621725, 6.948315255594014417, 0.8781869475623119703 ) ) ;
#75870 = CARTESIAN_POINT ( 'NONE',  ( -5.167065940139584868, 6.161236697318522637, 1.082531754730549078 ) ) ;
#75871 = CARTESIAN_POINT ( 'NONE',  ( 11.89197415570408900, 13.79999999999999716, 0.8055989572471804472 ) ) ;
#75872 = CARTESIAN_POINT ( 'NONE',  ( 0.9183970251232485005, 1.633131562045697649, 0.6825882272994202582 ) ) ;
#75873 = CARTESIAN_POINT ( 'NONE',  ( 5.602202738069384402, -0.9032165795441854383, 1.799149290095316767 ) ) ;
#75874 = CARTESIAN_POINT ( 'NONE',  ( 6.505214776458575265, 6.483838748823460563, 1.040834085586084257E-14 ) ) ;
#75875 = CARTESIAN_POINT ( 'NONE',  ( 3.803828919190560764, -0.6134138247068477989, 2.014629399117270125 ) ) ;
#75876 = CARTESIAN_POINT ( 'NONE',  ( 3.128438982650301625, 0.4684375082077455454, 1.857299403769121060 ) ) ;
#75877 = CARTESIAN_POINT ( 'NONE',  ( -0.02244404828160087226, 1.323617703852699057, -2.440988974267483957 ) ) ;
#75878 = CARTESIAN_POINT ( 'NONE',  ( 4.562928411757408043, 1.523777916087779571, -1.247912438812292413 ) ) ;
#75879 = CARTESIAN_POINT ( 'NONE',  ( 5.625262229866254238, 1.783287769691415781, 0.9483128780355275511 ) ) ;
#75880 = CARTESIAN_POINT ( 'NONE',  ( 3.098369316282158614, -0.5415621961667067552, -1.790553177708480215 ) ) ;
#75883 = ORIENTED_EDGE ( 'NONE', *, *, #60288, .F. ) ;
#75882 = CARTESIAN_POINT ( 'NONE',  ( 0.8965662283535699162, -1.866366896104875162, -0.4163465257057268332 ) ) ;
#75881 = CARTESIAN_POINT ( 'NONE',  ( 5.531808922564334097, -1.099089406413750414, -1.329375763670269883 ) ) ;
#75885 = CARTESIAN_POINT ( 'NONE',  ( 3.050221373394638835, 6.502416002361635528, 0.000000000000000000 ) ) ;
#75884 = CARTESIAN_POINT ( 'NONE',  ( 1.875870136999336246, 2.111227540014638304, -0.6426800678154330759 ) ) ;
#75886 = CARTESIAN_POINT ( 'NONE',  ( -1.364683531250000748, 2.071875000341422357, 1.214306433183764966E-14 ) ) ;
#75887 = CARTESIAN_POINT ( 'NONE',  ( 6.830524215763060347, -1.208013408316032322, 1.546442907991877558 ) ) ;
#75889 = AXIS2_PLACEMENT_3D ( 'NONE', #178756, #209079, #30368 ) ;
#75888 = CARTESIAN_POINT ( 'NONE',  ( 6.265839547809997079, 10.46189657242035587, 0.7998128361456462443 ) ) ;
#75890 = CARTESIAN_POINT ( 'NONE',  ( -8.306341666666730461, 12.84248237775322643, 1.040834085586084257E-14 ) ) ;
#75891 = DIRECTION ( 'NONE',  ( 0.000000000000000000, 1.000000000000000000, 0.000000000000000000 ) ) ;
#75892 = CYLINDRICAL_SURFACE ( 'NONE', #79294, 1.500000000000000222 ) ;
#75893 = DIRECTION ( 'NONE',  ( 0.000000000000000000, 1.000000000000000000, 0.000000000000000000 ) ) ;
#75894 = EDGE_CURVE ( 'NONE', #5554, #180844, #119501, .T. ) ;
#75895 = EDGE_LOOP ( 'NONE', ( #121568, #43530, #50522, #210129 ) ) ;
#75896 = CARTESIAN_POINT ( 'NONE',  ( 1.891162872569674080, 0.2007839719405465906, 2.060584128686280714 ) ) ;
#75897 = CARTESIAN_POINT ( 'NONE',  ( -0.7500000000000006661, 2.608333333333358262, -1.299038105676652011 ) ) ;
#75898 = CARTESIAN_POINT ( 'NONE',  ( 4.852928918687680948, 7.749168607522574526, 1.199719254218462483 ) ) ;
#75899 = CARTESIAN_POINT ( 'NONE',  ( -6.877010230629689858, 9.046264573866535486, 1.599625672291283607 ) ) ;
#75900 = CARTESIAN_POINT ( 'NONE',  ( 5.063044020060520900, 4.871582543017558109, 0.7998128361456352531 ) ) ;
#75901 = CARTESIAN_POINT ( 'NONE',  ( 6.252600707356171128, 2.097339953035493476, 0.3115551810550786227 ) ) ;
#75902 = DIRECTION ( 'NONE',  ( 0.000000000000000000, 0.000000000000000000, -1.000000000000000000 ) ) ;
#75903 = CARTESIAN_POINT ( 'NONE',  ( -1.364683531250000748, 2.259375000341422357, 1.214306433183764966E-14 ) ) ;
#75905 = CARTESIAN_POINT ( 'NONE',  ( 9.029367117021314115, 12.51771682229149008, -1.082531754730543083 ) ) ;
#75904 = CYLINDRICAL_SURFACE ( 'NONE', #189882, 3.000000000000010214 ) ;
#75906 = CARTESIAN_POINT ( 'NONE',  ( 5.360703810585087048, -0.7282664037663032497, 1.880147357087233129 ) ) ;
#75907 = CARTESIAN_POINT ( 'NONE',  ( 4.592943030449060160, 1.669885041223855060, 0.9386680909919845606 ) ) ;
#75908 = CARTESIAN_POINT ( 'NONE',  ( -6.116136693540540570, 10.14959355252369910, 0.000000000000000000 ) ) ;
#75909 = CARTESIAN_POINT ( 'NONE',  ( 2.929422067023911502, -1.473737196803912797, -1.622193633833472814 ) ) ;
#75910 = CARTESIAN_POINT ( 'NONE',  ( -1.734723475976807094E-15, 4.518467169708413778, -12.00000000000000178 ) ) ;
#75911 = CARTESIAN_POINT ( 'NONE',  ( -1.402160292154681736E-14, 0.8687500006828192678, -1.732050807568863648 ) ) ;
#75912 = CARTESIAN_POINT ( 'NONE',  ( 5.115494517658178530, 1.648350763777502559, 1.155591226287083328 ) ) ;
#75913 = CARTESIAN_POINT ( 'NONE',  ( 1.757924209179074770, 0.7287868685415777037, -1.768279316124596656 ) ) ;
#75914 = CARTESIAN_POINT ( 'NONE',  ( -5.422371370461663176, 8.413518134592214537, -1.199719254218446718 ) ) ;
#75916 = CARTESIAN_POINT ( 'NONE',  ( 0.2632962822839111650, 1.880428227362867633, -0.7283992291491693249 ) ) ;
#75915 = CARTESIAN_POINT ( 'NONE',  ( -2.467220768007014176, 5.822248629409386922, 0.7216878364870317197 ) ) ;
#75917 = CARTESIAN_POINT ( 'NONE',  ( 1.364683531249996529, 9.776041667008064096, 0.7879004041258405033 ) ) ;
#75919 = CARTESIAN_POINT ( 'NONE',  ( -4.932134020321308654, 8.976183133675331050, 0.7998128361456291469 ) ) ;
#75918 = CARTESIAN_POINT ( 'NONE',  ( 3.228152448572230160, 2.040302950407224536, 0.4557642060307572907 ) ) ;
#75921 = VERTEX_POINT ( 'NONE', #212742 ) ;
#75920 = CARTESIAN_POINT ( 'NONE',  ( 1.817014216480263622, -0.2154200610367338342, 1.711195096342375210 ) ) ;
#75922 = CARTESIAN_POINT ( 'NONE',  ( 6.451439665316073935, -1.893653415279672902, 0.9546920624979161607 ) ) ;
#75923 = CARTESIAN_POINT ( 'NONE',  ( 4.937140493670735708, 8.911747675924535983, -0.7998128361456281477 ) ) ;
#75924 = CARTESIAN_POINT ( 'NONE',  ( -7.564733433744393665, -6.863455982311501558, -7.986233326679976763 ) ) ;
#75925 = CARTESIAN_POINT ( 'NONE',  ( 7.439168848973995551, -6.893137084989842123, 8.103009739378016718 ) ) ;
#75926 = CARTESIAN_POINT ( 'NONE',  ( 9.367496997597594799, 3.481548657788670731, -7.500000000000007105 ) ) ;
#75927 = CARTESIAN_POINT ( 'NONE',  ( 6.328958779480917229, 6.278206752349526631, 0.7998128361456341429 ) ) ;
#75928 = ORIENTED_EDGE ( 'NONE', *, *, #95054, .T. ) ;
#75929 = PLANE ( 'NONE',  #182546 ) ;
#75930 = ORIENTED_EDGE ( 'NONE', *, *, #63612, .F. ) ;
#75931 = CARTESIAN_POINT ( 'NONE',  ( 3.246531836744088295, 1.767876921188500150, 0.3942315000180166562 ) ) ;
#75932 = ORIENTED_EDGE ( 'NONE', *, *, #113105, .T. ) ;
#75933 = CARTESIAN_POINT ( 'NONE',  ( 2.866659414285625651, 5.431854185720147221, -1.199719254218446718 ) ) ;
#75934 = CARTESIAN_POINT ( 'NONE',  ( 4.115782150200256950, 6.959440387612411349, 1.199719254218452047 ) ) ;
#75935 = CARTESIAN_POINT ( 'NONE',  ( 3.510248027248025426, -1.809562450863181127, -0.08562717191654131699 ) ) ;
#75936 = CARTESIAN_POINT ( 'NONE',  ( 6.520158902582616101, 5.290451655907108197, 2.438235897557466281 ) ) ;
#75937 = CARTESIAN_POINT ( 'NONE',  ( -10.95855051086950027, -7.723431457505071762, 0.6286713519883972978 ) ) ;
#75938 = CARTESIAN_POINT ( 'NONE',  ( 5.766360146646302809, 6.053989883630594981, 0.5864573027323967125 ) ) ;
#75939 =( GEOMETRIC_REPRESENTATION_CONTEXT ( 3 ) GLOBAL_UNCERTAINTY_ASSIGNED_CONTEXT ( ( #94223 ) ) GLOBAL_UNIT_ASSIGNED_CONTEXT ( ( #192647, #78899, #14949 ) ) REPRESENTATION_CONTEXT ( 'NONE', 'WORKASPACE' ) );
#75940 = CARTESIAN_POINT ( 'NONE',  ( 4.281604344665800532, -1.781275985052663158, 0.5390932415961935398 ) ) ;
#75941 = CARTESIAN_POINT ( 'NONE',  ( 1.968237613432867184, -1.879027187823999245, -0.3716057669084034676 ) ) ;
#75942 = CARTESIAN_POINT ( 'NONE',  ( 1.113953379265147925, -0.8168401028521531382, -1.632710947565917170 ) ) ;
#75943 = CARTESIAN_POINT ( 'NONE',  ( 4.805106176720093103, 8.123399998552004675, 0.8388070820863163801 ) ) ;
#75944 = DIRECTION ( 'NONE',  ( -0.7771862570881746812, 0.6292706268317899143, 0.000000000000000000 ) ) ;
#75945 = CARTESIAN_POINT ( 'NONE',  ( 4.802738015080052492, 8.126035781178083894, 0.8349615142884360131 ) ) ;
#75946 = CARTESIAN_POINT ( 'NONE',  ( -9.579603127937250662, -9.746166700193986898, 0.08720040834116031536 ) ) ;
#75947 = DIRECTION ( 'NONE',  ( -0.2684563758389304500, 0.000000000000000000, -0.9632918427306581544 ) ) ;
#75948 = CARTESIAN_POINT ( 'NONE',  ( 0.9311234436981579154, -2.509380368602567302, -3.474999999999996536 ) ) ;
#75949 = CARTESIAN_POINT ( 'NONE',  ( 7.727784370109387346, 10.99920361756089093, -1.082531754730543083 ) ) ;
#75950 = CARTESIAN_POINT ( 'NONE',  ( 5.207841159657320418, 0.6216970817616838119, -1.868779976745947202 ) ) ;
#75951 = CARTESIAN_POINT ( 'NONE',  ( -3.893162665418476109, 7.693773542963529444, 1.040834085586084257E-14 ) ) ;
#75952 = DIRECTION ( 'NONE',  ( -0.000000000000000000, -1.000000000000000000, 0.000000000000000000 ) ) ;
#75953 = CARTESIAN_POINT ( 'NONE',  ( 0.2168896333464042925, -0.1002974801882359490, 2.088354908755992945 ) ) ;
#75954 = CARTESIAN_POINT ( 'NONE',  ( 8.121497709785879593, 9.433834401960398353, -1.199719254218445830 ) ) ;
#75955 = CARTESIAN_POINT ( 'NONE',  ( 5.174797004712035076, -1.813887718507047220, -0.6490126392820031453 ) ) ;
#75956 = CARTESIAN_POINT ( 'NONE',  ( -6.728924311084075960, 6.744833205886536120, 1.040834085586084257E-14 ) ) ;
#75957 = CARTESIAN_POINT ( 'NONE',  ( 1.834698128333624112, 0.1755570873784827179, 1.817110820650599923 ) ) ;
#75958 = CARTESIAN_POINT ( 'NONE',  ( 2.069229996397306426, -2.018448871333050842, -0.8927042923378907258 ) ) ;
#75959 = CARTESIAN_POINT ( 'NONE',  ( 11.97302537858650773, 12.30124010191982720, 0.8111997896468311486 ) ) ;
#75960 = CARTESIAN_POINT ( 'NONE',  ( 0.8262462788446511830, -0.8622288892402606431, -1.707089296137359158 ) ) ;
#75961 = ORIENTED_EDGE ( 'NONE', *, *, #147857, .T. ) ;
#75962 = CARTESIAN_POINT ( 'NONE',  ( 6.912958093653829295, -1.524444945649571004, 1.246696689375533795 ) ) ;
#75963 = CARTESIAN_POINT ( 'NONE',  ( 2.155715342533376155, 0.8324662149039625536, 1.754741561904197056 ) ) ;
#75964 = ORIENTED_EDGE ( 'NONE', *, *, #18607, .T. ) ;
#75965 = CARTESIAN_POINT ( 'NONE',  ( 0.6146109705059289441, 0.6351056948852469297, -1.913509406280079705 ) ) ;
#75967 = CARTESIAN_POINT ( 'NONE',  ( 0.1857038103042158439, -1.139949723551544114, -1.471474936012186596 ) ) ;
#75966 = CARTESIAN_POINT ( 'NONE',  ( -4.769436176957319695, 8.786368983084006601, 0.7998128361456281477 ) ) ;
#75968 = CARTESIAN_POINT ( 'NONE',  ( 5.061990249855835344, 6.999017606288844284, -1.599625672291273171 ) ) ;
#75969 = CARTESIAN_POINT ( 'NONE',  ( 0.1298625177950013254, -9.252181021551010076, -9.620122301472909143 ) ) ;
#75970 = CARTESIAN_POINT ( 'NONE',  ( 10.07387183015377197, 11.71160420905630062, -1.199719254218440723 ) ) ;
#75971 = CARTESIAN_POINT ( 'NONE',  ( -4.497554271431319250, 6.270232621468402989, -1.599625672291256295 ) ) ;
#75972 = CARTESIAN_POINT ( 'NONE',  ( -6.445975688654487001, 6.485002823043819475, -0.7998128361456362523 ) ) ;
#75973 = CARTESIAN_POINT ( 'NONE',  ( 2.437293137456029157, -1.626093413141915134, -1.469474007205706645 ) ) ;
#75974 = CARTESIAN_POINT ( 'NONE',  ( 3.050221373394638835, 6.502416002361635528, 0.000000000000000000 ) ) ;
#75975 = CARTESIAN_POINT ( 'NONE',  ( -10.51596412982177853, 12.48659081731577380, -3.553961965504329967 ) ) ;
#75976 = CARTESIAN_POINT ( 'NONE',  ( 0.5773502691896192918, -4.295408888568413630, 1.000000000000004441 ) ) ;
#75977 = CARTESIAN_POINT ( 'NONE',  ( 2.982817717652554101, -0.1347461720548545627, -1.820777111243766733 ) ) ;
#75978 = SURFACE_SIDE_STYLE ('',( #56532 ) ) ;
#75979 = CARTESIAN_POINT ( 'NONE',  ( -4.440459003675619520, 5.139289244831666714, 1.199719254218462483 ) ) ;
#75980 = CARTESIAN_POINT ( 'NONE',  ( -4.603205931398525408, 8.475712490939976362, -0.2800714110085516517 ) ) ;
#75981 = CARTESIAN_POINT ( 'NONE',  ( 4.858757509019057785, 5.629766575900002401, -2.420000000000000373 ) ) ;
#75982 = CARTESIAN_POINT ( 'NONE',  ( 9.426996880203592610, 9.892584536526015881, -0.7998128361456281477 ) ) ;
#75983 = CARTESIAN_POINT ( 'NONE',  ( 0.5922524703982982031, -1.911778602531236215, -0.2371815352125578036 ) ) ;
#75984 = CARTESIAN_POINT ( 'NONE',  ( 5.366048076001885825, -1.952644961629325548, 0.1885061251027941032 ) ) ;
#75985 = CARTESIAN_POINT ( 'NONE',  ( -0.7500000000000179856, 15.04166666666666785, 1.299038105676658228 ) ) ;
#75986 = CARTESIAN_POINT ( 'NONE',  ( -6.191269702934848240, 10.37489842006599616, 0.000000000000000000 ) ) ;
#75987 = CARTESIAN_POINT ( 'NONE',  ( 4.985647801523278133, 6.839675073242382553, -1.599625672291256295 ) ) ;
#75988 = EDGE_CURVE ( 'NONE', #12413, #60185, #111058, .T. ) ;
#75989 = CARTESIAN_POINT ( 'NONE',  ( 4.880524338131243312, -0.2681524694418158661, -2.175044001020635331 ) ) ;
#75990 = LINE ( 'NONE', #91195, #80537 ) ;
#75991 = CARTESIAN_POINT ( 'NONE',  ( 4.416890754593222113, -1.537527071031305814, 1.386575359339572655 ) ) ;
#75993 = CARTESIAN_POINT ( 'NONE',  ( 1.364683531249986537, 2.467708333674753174, -0.7879004041258239610 ) ) ;
#75992 = CARTESIAN_POINT ( 'NONE',  ( 8.216319294035601573, 14.20048435439411882, 8.685543064379698919 ) ) ;
#75994 = VERTEX_POINT ( 'NONE', #143539 ) ;
#75995 = CARTESIAN_POINT ( 'NONE',  ( 4.641406123262603600, 0.8788069589312655916, 2.124244668743579201 ) ) ;
#75996 = CARTESIAN_POINT ( 'NONE',  ( 5.504247177468168495, 9.365446107114122398, 0.7216878364870438212 ) ) ;
#75998 = DIRECTION ( 'NONE',  ( 0.000000000000000000, 0.000000000000000000, 1.000000000000000000 ) ) ;
#75997 = CARTESIAN_POINT ( 'NONE',  ( 6.048345925472191631, 6.229027465905275562, 0.7216878364870328300 ) ) ;
#75999 = CARTESIAN_POINT ( 'NONE',  ( 0.3402841477759439570, 2.286568017602428338, 0.1625022809590911665 ) ) ;
#76000 = CARTESIAN_POINT ( 'NONE',  ( 6.620655732516632419, 1.270823175217004941, 2.040803978124502205 ) ) ;
#76001 = CARTESIAN_POINT ( 'NONE',  ( -7.611976899429754084, 7.845337568948314022, 0.7998128361456341429 ) ) ;
#76002 = CARTESIAN_POINT ( 'NONE',  ( 5.015543440151827959, -1.040391601716946557, -1.639569664018299289 ) ) ;
#76003 = ORIENTED_EDGE ( 'NONE', *, *, #107910, .F. ) ;
#76005 = EDGE_CURVE ( 'NONE', #177940, #33705, #108929, .T. ) ;
#76004 = CARTESIAN_POINT ( 'NONE',  ( 8.066738210006668908, 12.35501897840907581, 0.7216878364870438212 ) ) ;
#76006 = ORIENTED_EDGE ( 'NONE', *, *, #7130, .F. ) ;
#76007 = CARTESIAN_POINT ( 'NONE',  ( 4.658414424252744546, 1.907665749568526747, 0.1350064596054162680 ) ) ;
#76008 = CARTESIAN_POINT ( 'NONE',  ( 6.088827306860007837, -0.2580713809433569650, -1.705207211698676062 ) ) ;
#76009 = CARTESIAN_POINT ( 'NONE',  ( 5.243375144629232487, 0.3886363430659240392, -1.978554426619572926 ) ) ;
#76011 = CYLINDRICAL_SURFACE ( 'NONE', #71031, 1.500000000000000222 ) ;
#76010 = CARTESIAN_POINT ( 'NONE',  ( -9.341731535015849630, 10.85744053139533349, 1.199719254218462483 ) ) ;
#76012 = CARTESIAN_POINT ( 'NONE',  ( -3.285556943750000070, -0.8968749995220438587, 0.000000000000000000 ) ) ;
#76014 = CARTESIAN_POINT ( 'NONE',  ( 6.766889846978989986, -1.619426471845460069, -0.7142080874563813131 ) ) ;
#76013 = CARTESIAN_POINT ( 'NONE',  ( 1.500065138910465334, -0.7538795759346494929, -1.950162888426725250 ) ) ;
#76015 = CARTESIAN_POINT ( 'NONE',  ( 5.344375030997434273, 0.3906003880304632636, -1.978050218768567792 ) ) ;
#76017 = CARTESIAN_POINT ( 'NONE',  ( 2.888958383575964017, 1.965592292480751402, -1.179159595035377261 ) ) ;
#76016 = CARTESIAN_POINT ( 'NONE',  ( 4.736594563127852098, 6.619389305106191834, -1.599625672291273171 ) ) ;
#76018 = CARTESIAN_POINT ( 'NONE',  ( 1.903882329689795094, 1.290680248512179551, -1.167607185883823728 ) ) ;
#76019 = VECTOR ( 'NONE', #149125, 1000.000000000000000 ) ;
#76020 = CARTESIAN_POINT ( 'NONE',  ( -2.630984769852970917, -0.3922140236936322299, -0.1649412225328064641 ) ) ;
#76021 = CARTESIAN_POINT ( 'NONE',  ( 2.635775109972549490, 0.08874582706053059378, -1.731711113058966633 ) ) ;
#76022 = CARTESIAN_POINT ( 'NONE',  ( -1.360316468750038643, 1.651041667008089853, -0.7853790794159041244 ) ) ;
#76023 = CARTESIAN_POINT ( 'NONE',  ( 1.627181624537884286, 0.1412763417478210271, -1.855766238205541097 ) ) ;
#76024 = CARTESIAN_POINT ( 'NONE',  ( 2.805323142837768291, -1.806386208845015995, 1.204286856753070456 ) ) ;
#76025 = CARTESIAN_POINT ( 'NONE',  ( 3.520720487665735643, 0.3006478860226591276, 1.993893439002386581 ) ) ;
#76026 = CARTESIAN_POINT ( 'NONE',  ( 4.750000000000003553, 2.703060497845378561E-13, 2.052068128417943171 ) ) ;
#76027 = CARTESIAN_POINT ( 'NONE',  ( 1.499999999999989120, 1.806250000682817269, 0.000000000000000000 ) ) ;
#76028 = CARTESIAN_POINT ( 'NONE',  ( 6.375613808387889492, 1.842787572768100457, -0.5617375553943514399 ) ) ;
#76029 = CARTESIAN_POINT ( 'NONE',  ( 1.364683531249996529, 14.46354166700806410, 0.7879004041258405033 ) ) ;
#76030 = CARTESIAN_POINT ( 'NONE',  ( 3.023905552101690208, -0.4295200811062405699, 2.179336035515607950 ) ) ;
#76031 = ORIENTED_EDGE ( 'NONE', *, *, #48405, .F. ) ;
#76032 = CARTESIAN_POINT ( 'NONE',  ( -0.2110808730066962846, 5.724502961415374180, -2.391230805320884834 ) ) ;
#76033 = CARTESIAN_POINT ( 'NONE',  ( 1.499999999999985123, 0.04583333333335545129, -0.8660254037844323793 ) ) ;
#76035 = EDGE_CURVE ( 'NONE', #86850, #37826, #44950, .T. ) ;
#76034 = CARTESIAN_POINT ( 'NONE',  ( 7.781490099239519509, 11.16582331816642260, 1.199719254218460707 ) ) ;
#76036 = CARTESIAN_POINT ( 'NONE',  ( 0.6823417656249882723, 0.09270833367475139752, 1.181850606188755259 ) ) ;
#76037 = CARTESIAN_POINT ( 'NONE',  ( 6.433822955411669930, -2.155103329387221933, 0.5382066023030105395 ) ) ;
#76038 = CARTESIAN_POINT ( 'NONE',  ( 4.334394203492665909, -1.131343785558375226, 1.602600411086833931 ) ) ;
#76040 = CARTESIAN_POINT ( 'NONE',  ( -6.724481002698138532, 6.947575379343695623, -0.7216878364870278340 ) ) ;
#76039 = CARTESIAN_POINT ( 'NONE',  ( 4.369805582306193870, 3.992528022312320957, 1.214306433183764966E-14 ) ) ;
#76041 = CIRCLE ( 'NONE', #41580, 0.2000000000000005107 ) ;
#76042 = CARTESIAN_POINT ( 'NONE',  ( 0.000000000000000000, 1.000000000000000888, 0.000000000000000000 ) ) ;
#76043 = CARTESIAN_POINT ( 'NONE',  ( 6.221994747346401233, -1.249160343739505352, -1.886125069868335613 ) ) ;
#76044 = CARTESIAN_POINT ( 'NONE',  ( 2.330602656244503468, -1.270745551583628785, 1.624662076113972065 ) ) ;
#76045 = CARTESIAN_POINT ( 'NONE',  ( -6.205881626753225966, 8.263281202677319470, 1.599625672291283607 ) ) ;
#76046 = ORIENTED_EDGE ( 'NONE', *, *, #211660, .T. ) ;
#76048 = EDGE_CURVE ( 'NONE', #52005, #179471, #108104, .T. ) ;
#76047 = CARTESIAN_POINT ( 'NONE',  ( -0.7500000000000006661, 2.139583334016155636, -1.299038105676652011 ) ) ;
#76049 = CARTESIAN_POINT ( 'NONE',  ( 3.796049943699483453, -1.868292110373217518, -0.09463876624429126694 ) ) ;
#76050 = CARTESIAN_POINT ( 'NONE',  ( 2.461176475124981611, -1.659910965455011267, -0.5019686038148748475 ) ) ;
#76051 = CARTESIAN_POINT ( 'NONE',  ( 0.1172542576415449567, -0.1040641125494116137, 2.290134469065004730 ) ) ;
#76052 = CARTESIAN_POINT ( 'NONE',  ( 1.536444635327537833, 1.086998388645914027, -1.920427013416255768 ) ) ;
#76053 = CARTESIAN_POINT ( 'NONE',  ( 5.384693163835662766, 1.711646917711911353, -0.9173020705802971131 ) ) ;
#76054 = ADVANCED_FACE ( 'NONE', ( #95838 ), #161894, .T. ) ;
#76056 = VERTEX_POINT ( 'NONE', #174950 ) ;
#76055 = DIRECTION ( 'NONE',  ( 0.6507913734559640506, -0.7592566023653004592, 0.000000000000000000 ) ) ;
#76057 = CARTESIAN_POINT ( 'NONE',  ( 0.3521856818783953846, 0.1948384997633167970, -2.006960225185448810 ) ) ;
#76058 = CARTESIAN_POINT ( 'NONE',  ( -0.03470293633787284449, -1.699275230904277789, 1.268407768021381221 ) ) ;
#76059 = DIRECTION ( 'NONE',  ( 0.000000000000000000, 0.000000000000000000, 1.000000000000000000 ) ) ;
#76060 = CARTESIAN_POINT ( 'NONE',  ( 6.469375277500488686, -1.978045142091336306, -0.3906011616893814709 ) ) ;
#76061 = CARTESIAN_POINT ( 'NONE',  ( -9.989660255170729641, 10.54902514065433827, -0.7998128361456291469 ) ) ;
#76062 = CARTESIAN_POINT ( 'NONE',  ( 7.793239369756836510, 7.986534107671458216, 0.7998128361456341429 ) ) ;
#76063 = CARTESIAN_POINT ( 'NONE',  ( 4.523580528814945545, 5.306540700819438960, 1.199719254218452047 ) ) ;
#76064 = CARTESIAN_POINT ( 'NONE',  ( 4.318856058802469811, 1.670182456744148336, 0.7377305746401884301 ) ) ;
#76065 = CARTESIAN_POINT ( 'NONE',  ( 2.309865001130634976, -0.4838574416936823885, 2.152911442350906146 ) ) ;
#76066 = ORIENTED_EDGE ( 'NONE', *, *, #140054, .T. ) ;
#76067 = CARTESIAN_POINT ( 'NONE',  ( -7.391130018105325661, 8.652015104991543026, -1.199719254218452047 ) ) ;
#76068 = CARTESIAN_POINT ( 'NONE',  ( -1.642778471874998480, -2.938541666188707602, 2.845375778867863303 ) ) ;
#76069 = CARTESIAN_POINT ( 'NONE',  ( -6.672584156219988571, 10.93643194889866521, -0.7998128361456291469 ) ) ;
#76070 = CARTESIAN_POINT ( 'NONE',  ( 1.459246395511590189, -1.704040126542965661, 1.084046338683493982 ) ) ;
#76071 = B_SPLINE_CURVE_WITH_KNOTS ( 'NONE', 3,
 ( #148653, #116207, #182193, #209620 ),
 .UNSPECIFIED., .F., .F.,
 ( 4, 4 ),
 ( 1.226634733346700890E-18, 0.002003498272494348524 ),
 .UNSPECIFIED. ) ;
#76072 = CARTESIAN_POINT ( 'NONE',  ( -1.000000000000014433, 6.468705557303653819, 4.925226524755080604 ) ) ;
#76073 = CARTESIAN_POINT ( 'NONE',  ( -5.418418667316934112, 6.350518529071726981, -1.199719254218453823 ) ) ;
#76074 = CARTESIAN_POINT ( 'NONE',  ( 2.518200207203071805, 0.7905618127436510045, 1.684796146788158699 ) ) ;
#76075 = CARTESIAN_POINT ( 'NONE',  ( 3.541704441667858472, 5.155074486744371853, -1.599625672291262513 ) ) ;
#76076 = CARTESIAN_POINT ( 'NONE',  ( 10.50000000000000178, 12.69999999999999929, -3.600000000000000977 ) ) ;
#76077 = VERTEX_POINT ( 'NONE', #76354 ) ;
#76078 = ORIENTED_EDGE ( 'NONE', *, *, #113661, .T. ) ;
#76079 = CARTESIAN_POINT ( 'NONE',  ( -7.309817376062285099, 11.67987070538135264, 0.000000000000000000 ) ) ;
#76080 = CARTESIAN_POINT ( 'NONE',  ( 4.353998665852670591, 1.825246345946249571, -0.04724550102237072557 ) ) ;
#76082 = CARTESIAN_POINT ( 'NONE',  ( -5.094707486240121597, 6.719114383638050469, -1.440239009331502062 ) ) ;
#76081 = CARTESIAN_POINT ( 'NONE',  ( -4.736594563127865420, 6.619389305106191834, -1.599625672291271394 ) ) ;
#76083 = CARTESIAN_POINT ( 'NONE',  ( 5.894874513638865388, 7.262872338272549300, -1.253420816524719150 ) ) ;
#76084 = CARTESIAN_POINT ( 'NONE',  ( 6.696638777208028692, -1.314797947003863543, -1.528504179509587280 ) ) ;
#76085 = CARTESIAN_POINT ( 'NONE',  ( 6.246043375366982175, 0.5822610321466625827, 1.746719530172704538 ) ) ;
#76086 = CARTESIAN_POINT ( 'NONE',  ( 4.319161277787673114, 2.108828969982502688, 0.9375607936791326980 ) ) ;
#76087 = CARTESIAN_POINT ( 'NONE',  ( 5.578253857379852576, 5.472660686556754861, -0.7998128361456481317 ) ) ;
#76088 = CARTESIAN_POINT ( 'NONE',  ( 0.2103215893997134323, -0.8792329509940269849, -1.862182962916396844 ) ) ;
#76089 = CARTESIAN_POINT ( 'NONE',  ( 6.551614543901692400, 8.666636272683888365, 1.599625672291281386 ) ) ;
#76090 = CARTESIAN_POINT ( 'NONE',  ( 1.997508135846944421, -1.941589802808607157, 0.04981292379131925518 ) ) ;
#76091 = CARTESIAN_POINT ( 'NONE',  ( 5.308124166105086417, -1.975000179191854111, 1.175378216249231222 ) ) ;
#76092 = CYLINDRICAL_SURFACE ( 'NONE', #193271, 2.725000000000000089 ) ;
#76093 = CARTESIAN_POINT ( 'NONE',  ( -7.262327558775498737, 8.501745569106741840, 1.199719254218452047 ) ) ;
#76094 = CARTESIAN_POINT ( 'NONE',  ( 5.102362337376947998, -0.6309395149336484154, -1.761181640970375106 ) ) ;
#76095 = B_SPLINE_CURVE_WITH_KNOTS ( 'NONE', 3,
 ( #112919, #162679, #194088, #111856, #193014 ),
 .UNSPECIFIED., .F., .F.,
 ( 4, 1, 4 ),
 ( 0.003112877374997422876, 0.003157543106160180107, 0.003202208837322937773 ),
 .UNSPECIFIED. ) ;
#76097 = CARTESIAN_POINT ( 'NONE',  ( -5.795184315198522285, 5.725746220678519904, -0.7998128361456362523 ) ) ;
#76096 = CARTESIAN_POINT ( 'NONE',  ( 2.636851627972558454, 1.802111047976437508, 0.6404684511054498097 ) ) ;
#76098 = CARTESIAN_POINT ( 'NONE',  ( 3.405080638938757343, 1.739790774466195789, -1.357627211771177178 ) ) ;
#76099 = CARTESIAN_POINT ( 'NONE',  ( -1.225000000000048939, 0.06250000068282191013, -4.336808689942017736E-14 ) ) ;
#76100 = CARTESIAN_POINT ( 'NONE',  ( -10.60583023524544544, 4.240113626697339377, 5.518324045435343272 ) ) ;
#76101 = CARTESIAN_POINT ( 'NONE',  ( 5.844973620822844218, 5.991759777147701804, 0.7216878364870328300 ) ) ;
#76102 = CARTESIAN_POINT ( 'NONE',  ( -6.170369307550858551, 8.292126506933035657, 1.443375672974058777 ) ) ;
#76103 = CARTESIAN_POINT ( 'NONE',  ( 1.598833994113032730, 1.614015922016404536, -1.131664812120122487 ) ) ;
#76104 = CARTESIAN_POINT ( 'NONE',  ( 2.011159220144568938, 1.709348158914993254, -1.550378056569144958 ) ) ;
#76105 = CARTESIAN_POINT ( 'NONE',  ( 2.629291921057617554, 0.09916324773191761976, -1.959495597191794225 ) ) ;
#76106 = DIRECTION ( 'NONE',  ( 0.000000000000000000, 8.546850786086437571E-32, 1.000000000000000000 ) ) ;
#76107 = CARTESIAN_POINT ( 'NONE',  ( 6.455934469078565385, -0.7002696157344409089, 1.940163012464599879 ) ) ;
#76108 = CARTESIAN_POINT ( 'NONE',  ( 2.412988153552339643, 5.758977245878946327, 0.7216878364870438212 ) ) ;
#76109 = CARTESIAN_POINT ( 'NONE',  ( 3.942592416894859841, -1.490970858180175940, 1.357867534901323614 ) ) ;
#76110 = CARTESIAN_POINT ( 'NONE',  ( 2.891631901464575272, 6.595597328342462262, 0.000000000000000000 ) ) ;
#76111 = ORIENTED_EDGE ( 'NONE', *, *, #193470, .T. ) ;
#76112 = CARTESIAN_POINT ( 'NONE',  ( 4.505092375653735992, -0.09411930587044713137, 2.014432893821124004 ) ) ;
#76113 = CARTESIAN_POINT ( 'NONE',  ( -8.784793466650835825, 12.33634391347959713, 1.199719254218462483 ) ) ;
#76114 = CARTESIAN_POINT ( 'NONE',  ( 11.84100621633422179, 13.61041574223334649, 1.444132586618105174 ) ) ;
#76115 = DIRECTION ( 'NONE',  ( -0.000000000000000000, 1.000000000000000000, -0.000000000000000000 ) ) ;
#76116 = CARTESIAN_POINT ( 'NONE',  ( 8.401248741962376698, 12.95320729893149370, 0.7998128361456462443 ) ) ;
#76117 = CARTESIAN_POINT ( 'NONE',  ( 2.395604216770229833, -1.940863096919882569, 0.9729980962204368700 ) ) ;
#76118 = SURFACE_STYLE_USAGE ( .BOTH. , #11101 ) ;
#76119 = ADVANCED_FACE ( 'NONE', ( #10279 ), #192221, .F. ) ;
#76120 =( NAMED_UNIT ( * ) SI_UNIT ( $, .STERADIAN. ) SOLID_ANGLE_UNIT ( ) );
#76121 = CARTESIAN_POINT ( 'NONE',  ( 5.756345505848640798, 6.148709499980903992, 0.8262799378709930753 ) ) ;
#76122 = CARTESIAN_POINT ( 'NONE',  ( 2.583089905966722277, 1.711919019956799737, -0.7542334906679578621 ) ) ;
#76123 = CARTESIAN_POINT ( 'NONE',  ( 0.1927530690809010350, -0.4471281949963988867, -2.018758496260419921 ) ) ;
#76125 = CARTESIAN_POINT ( 'NONE',  ( 3.511198596259283544, 6.271927390929319834, 1.164732466530402855 ) ) ;
#76124 = CARTESIAN_POINT ( 'NONE',  ( 0.07775346131142636674, 2.855377671833533970, -2.776861204146412021 ) ) ;
#76126 = CARTESIAN_POINT ( 'NONE',  ( -1.364683531250014514, 0.03020833367475737191, 0.7879004041258379498 ) ) ;
#76127 = FACE_OUTER_BOUND ( 'NONE', #10898, .T. ) ;
#76128 = CARTESIAN_POINT ( 'NONE',  ( 3.738835060935014276, 1.816739721148411757, 0.5971339541979634458 ) ) ;
#76129 = CIRCLE ( 'NONE', #148799, 12.00000000000000178 ) ;
#76130 = CARTESIAN_POINT ( 'NONE',  ( 4.434285456697817374, 1.735847377751572385, 0.3442416992474469084 ) ) ;
#76131 = CARTESIAN_POINT ( 'NONE',  ( 1.963391044528959295, -1.536740334223782867, -1.137898036029337812 ) ) ;
#76132 = CARTESIAN_POINT ( 'NONE',  ( -3.632695093457760649, 6.325562478087638496, -1.199719254218452047 ) ) ;
#76134 = CARTESIAN_POINT ( 'NONE',  ( 0.1455191377820958532, 1.894478286654190269, -0.2837363430458189062 ) ) ;
#76133 = FILL_AREA_STYLE ('',( #161668 ) ) ;
#76135 = CARTESIAN_POINT ( 'NONE',  ( -1.500000000000001332, 0.4000000000000253353, 0.000000000000000000 ) ) ;
#76136 = CARTESIAN_POINT ( 'NONE',  ( 1.381394743813993964, -0.05274132383669553892, 2.069866178704109938 ) ) ;
#76137 = CARTESIAN_POINT ( 'NONE',  ( -1.402160292154681736E-14, -0.6156249996585817508, 1.575800808251672791 ) ) ;
#76138 = CARTESIAN_POINT ( 'NONE',  ( 6.297708355432167338, -0.6282832542035889922, 1.762108908958268216 ) ) ;
#76139 = CARTESIAN_POINT ( 'NONE',  ( 2.156629195875509719, -1.411784796728832392, 1.157573153174975111 ) ) ;
#76141 = CARTESIAN_POINT ( 'NONE',  ( 4.763071791759735163, 8.170823326046956936, 0.7639991172946744014 ) ) ;
#76140 = CARTESIAN_POINT ( 'NONE',  ( 5.619807753665406302, -2.153844256707802440, 0.4802137346974973409 ) ) ;
#76142 = CARTESIAN_POINT ( 'NONE',  ( -0.6823417656250003738, -0.5322916663252491576, -1.181850606188749264 ) ) ;
#76143 = CARTESIAN_POINT ( 'NONE',  ( 2.559094272886554666, 1.658201776010211459, -1.226620081234103266 ) ) ;
#76144 = CARTESIAN_POINT ( 'NONE',  ( -8.227100285394159940, 8.492705175914988303, 0.7998128361456602331 ) ) ;
#76145 = CARTESIAN_POINT ( 'NONE',  ( 7.727257484784855635, 11.10255193463598111, -1.199719254218446718 ) ) ;
#76146 = CARTESIAN_POINT ( 'NONE',  ( 1.412279214364694946, 3.475718376301037527, 0.5092244867763745519 ) ) ;
#76147 = CARTESIAN_POINT ( 'NONE',  ( 2.580963302752299349, -0.4788041664876945269, 0.000000000000000000 ) ) ;
#76148 = CARTESIAN_POINT ( 'NONE',  ( 7.666209513884374438, 7.908608952478760834, 0.7998128361456281477 ) ) ;
#76149 = ORIENTED_EDGE ( 'NONE', *, *, #148914, .T. ) ;
#76150 = CARTESIAN_POINT ( 'NONE',  ( 4.949704645232674061, 1.531818663031824013, 1.392983054852282132 ) ) ;
#76151 = CARTESIAN_POINT ( 'NONE',  ( -1.364683531250012516, 0.5927083336747520637, 0.7879004041258379498 ) ) ;
#76152 = CARTESIAN_POINT ( 'NONE',  ( 2.425270691926323607, -0.002641788883844810656, 2.161773191836775521 ) ) ;
#76153 = CARTESIAN_POINT ( 'NONE',  ( -4.764376198328064582, 8.188698463893414825, 0.7498042881181687935 ) ) ;
#76154 = CARTESIAN_POINT ( 'NONE',  ( 2.666670786633594137, 0.6826474749901580985, 1.900933108274209360 ) ) ;
#76155 = CARTESIAN_POINT ( 'NONE',  ( 6.620655732516615544, 0.0004550665019913135447, 2.073887158236031425 ) ) ;
#76158 = CARTESIAN_POINT ( 'NONE',  ( 5.178851490740187913, 8.985817805931475277, 0.7216878364870438212 ) ) ;
#76157 = CARTESIAN_POINT ( 'NONE',  ( -1.737500000000000266, -1.108333333333332726, -3.009438278150923907 ) ) ;
#76156 = FACE_OUTER_BOUND ( 'NONE', #146736, .T. ) ;
#76159 = CARTESIAN_POINT ( 'NONE',  ( -6.420668264523499147, 9.648474187656182366, 1.199719254218452935 ) ) ;
#76160 = CARTESIAN_POINT ( 'NONE',  ( 1.253139057289072822, 0.1435168058863903473, -2.011451928166609893 ) ) ;
#76162 = CARTESIAN_POINT ( 'NONE',  ( 6.198795224570643470, 1.821041368708445907, 1.219022265761634971 ) ) ;
#76161 = CARTESIAN_POINT ( 'NONE',  ( -5.766295404513795297, 5.621766148221195358, 0.7998128361456341429 ) ) ;
#76163 = CARTESIAN_POINT ( 'NONE',  ( -1.001543065824772872E-14, 5.493750000682816825, 1.732050807568877637 ) ) ;
#76164 = CARTESIAN_POINT ( 'NONE',  ( 4.658414424252744546, 1.907665749568526747, 0.1350064596054162680 ) ) ;
#76165 = CARTESIAN_POINT ( 'NONE',  ( -2.117044542028253318, 5.621635732341564662, -0.7998128361456281477 ) ) ;
#76166 = CARTESIAN_POINT ( 'NONE',  ( 6.168596704093459060, 7.259412911939593371, -1.082531754730543083 ) ) ;
#76168 = CARTESIAN_POINT ( 'NONE',  ( 3.743767684670766371, 2.000855813463810140, -0.2496267151909299931 ) ) ;
#76167 = CARTESIAN_POINT ( 'NONE',  ( -8.297226821439000588, 12.62392235841345389, 1.040834085586084257E-14 ) ) ;
#76169 = CARTESIAN_POINT ( 'NONE',  ( -0.6823417656250039265, 13.63020833367473195, -1.181850606188755259 ) ) ;
#76170 = CARTESIAN_POINT ( 'NONE',  ( 5.227475398614537916, -1.636741361296644603, 0.5442337529403593610 ) ) ;
#76171 = CARTESIAN_POINT ( 'NONE',  ( 6.200875153403774043, 8.327716660428123419, -1.599625672291283607 ) ) ;
#76172 = CARTESIAN_POINT ( 'NONE',  ( 9.734391104931951588, 11.41950637958454706, 1.082531754730548412 ) ) ;
#76173 = CARTESIAN_POINT ( 'NONE',  ( -11.48767021851168124, 11.33004227463830738, -3.470194894594655910 ) ) ;
#76174 = CARTESIAN_POINT ( 'NONE',  ( 4.094877388769967652, 1.581529129216452612, -0.9985332613470513374 ) ) ;
#76175 = CARTESIAN_POINT ( 'NONE',  ( 0.07536363704235481131, 0.6997989235110781969, -2.226667633679416447 ) ) ;
#76176 = CARTESIAN_POINT ( 'NONE',  ( 1.094682738308445202, 2.038987083759949304, 0.3576228084290478115 ) ) ;
#76177 = CARTESIAN_POINT ( 'NONE',  ( -2.788906526875773208E-15, 8.718750000682796042, -1.499999999999998446 ) ) ;
#76178 = ORIENTED_EDGE ( 'NONE', *, *, #199418, .T. ) ;
#76179 = CARTESIAN_POINT ( 'NONE',  ( 6.604213110542080045, -0.7679849629102013520, 1.639316308541746592 ) ) ;
#76180 = CARTESIAN_POINT ( 'NONE',  ( 3.555981428534177091, 7.370671776590375757, 0.7998128361456271485 ) ) ;
#76181 = DIRECTION ( 'NONE',  ( 3.219646771412963434E-15, 1.665334536937739741E-16, 1.000000000000000000 ) ) ;
#76182 = CARTESIAN_POINT ( 'NONE',  ( 0.7733460811225587594, 0.3524055278083237930, -1.776778109436588204 ) ) ;
#76183 = CARTESIAN_POINT ( 'NONE',  ( 5.682275777458851707, 6.762314840857718501, 1.082531754730549078 ) ) ;
#76184 = CARTESIAN_POINT ( 'NONE',  ( 11.29023325225217533, 8.870178701907233787, -4.083937312904004635 ) ) ;
#76185 = ORIENTED_EDGE ( 'NONE', *, *, #10253, .F. ) ;
#76186 = CARTESIAN_POINT ( 'NONE',  ( 7.402388682937041331, 11.57994453016116587, 1.040834085586084257E-14 ) ) ;
#76187 = EDGE_CURVE ( 'NONE', #95626, #114534, #111495, .T. ) ;
#76189 = CARTESIAN_POINT ( 'NONE',  ( 8.911787042884274257, 9.291506392986812912, 0.7998128361456462443 ) ) ;
#76188 = CARTESIAN_POINT ( 'NONE',  ( 0.3616705494772323726, -0.5269360983083425376, 1.889693748445469224 ) ) ;
#76190 = CARTESIAN_POINT ( 'NONE',  ( 4.657778235022878022, 1.106396155499450140, 1.563574394034000115 ) ) ;
#76191 = CARTESIAN_POINT ( 'NONE',  ( -4.079286826253504472, 3.980871698815676041, -0.5338862410131425262 ) ) ;
#76192 = SURFACE_STYLE_FILL_AREA ( #10117 ) ;
#76194 = VERTEX_POINT ( 'NONE', #210619 ) ;
#76193 = CARTESIAN_POINT ( 'NONE',  ( 5.517805331081858888, 5.539787095791365523, 1.040834085586084257E-14 ) ) ;
#76195 = CARTESIAN_POINT ( 'NONE',  ( -9.219181267612684749, 10.81842823604534765, 1.082531754730558626 ) ) ;
#76196 = CARTESIAN_POINT ( 'NONE',  ( 2.290102563249151402, -0.9248296759884739870, 1.954025333243500695 ) ) ;
#76197 = CARTESIAN_POINT ( 'NONE',  ( -4.930325137224961907, 5.781076077297750970, -1.199719254218453823 ) ) ;
#76198 = CARTESIAN_POINT ( 'NONE',  ( 7.838022202476093270, 8.316983122409855156, 0.7216878364870267237 ) ) ;
#76199 = CARTESIAN_POINT ( 'NONE',  ( 0.03560581989598374242, -0.09759080014098624190, 2.118463022953632091 ) ) ;
#76200 = CARTESIAN_POINT ( 'NONE',  ( 4.436427218767265757, 1.790408935156896586, 0.3557191534368231434 ) ) ;
#76201 = CARTESIAN_POINT ( 'NONE',  ( 8.806674072578200452, 13.38234123322611602, 7.683694639725048958 ) ) ;
#76202 = CARTESIAN_POINT ( 'NONE',  ( 1.475783946021753446, 1.170879755915053666, 1.585848323755238320 ) ) ;
#76203 = CARTESIAN_POINT ( 'NONE',  ( 3.357576282340120066, -1.451192137084562628, -1.245647637661301044 ) ) ;
#76204 = ORIENTED_EDGE ( 'NONE', *, *, #214167, .F. ) ;
#76205 = CARTESIAN_POINT ( 'NONE',  ( 0.2999999999999866107, 3.975028841772350940, 0.9637995837462389748 ) ) ;
#76206 = CARTESIAN_POINT ( 'NONE',  ( 4.334397697284593676, -1.135867708366841367, 1.608802569665278348 ) ) ;
#76207 = ORIENTED_EDGE ( 'NONE', *, *, #124997, .F. ) ;
#76208 = CARTESIAN_POINT ( 'NONE',  ( 5.794467663293456638, 1.585267558806532362, -1.121583357746269050 ) ) ;
#76209 = EDGE_LOOP ( 'NONE', ( #10544, #79825, #177334, #156550 ) ) ;
#76210 = CARTESIAN_POINT ( 'NONE',  ( -4.749098946536820520, 8.762642214260091933, 0.7998128361456281477 ) ) ;
#76212 = CARTESIAN_POINT ( 'NONE',  ( 6.275647701495586261, 0.3610785225884837746, -2.089460823871174266 ) ) ;
#76211 = CARTESIAN_POINT ( 'NONE',  ( -3.786470039966538970, 7.639575156594750283, 0.000000000000000000 ) ) ;
#76213 = CARTESIAN_POINT ( 'NONE',  ( 5.506019780481205217, 9.437790487287811558, 0.000000000000000000 ) ) ;
#76214 = CARTESIAN_POINT ( 'NONE',  ( 4.178302048780179412, 0.9043031410675538284, 1.684961085834511874 ) ) ;
#76215 = ADVANCED_FACE ( 'NONE', ( #14535 ), #28415, .T. ) ;
#76216 = CARTESIAN_POINT ( 'NONE',  ( -9.611175950047638139, -6.604184692106415788, 0.3106162252735236162 ) ) ;
#76217 = CARTESIAN_POINT ( 'NONE',  ( 0.2709337360254741034, -1.439471777561899035, 1.672717458380864608 ) ) ;
#76218 = CARTESIAN_POINT ( 'NONE',  ( 7.347880794884118750E-16, -4.000000000000003553, 5.799999999999999822 ) ) ;
#76219 = CARTESIAN_POINT ( 'NONE',  ( 5.391275966583902957, -0.05175381893108904618, -2.012593086484148142 ) ) ;
#76220 = CARTESIAN_POINT ( 'NONE',  ( -5.000000000000013323, 11.39843543023555661, -0.7749999999999996891 ) ) ;
#76221 = CARTESIAN_POINT ( 'NONE',  ( 5.725187622324654946, -0.04035785615889506128, 1.825416780793003069 ) ) ;
#76222 = CARTESIAN_POINT ( 'NONE',  ( 1.627480586986803868, 0.1543294891723171747, -2.064685722993148342 ) ) ;
#76223 = CARTESIAN_POINT ( 'NONE',  ( -7.237355071596549116, 7.338002426484427687, 1.040834085586084257E-14 ) ) ;
#76224 = CARTESIAN_POINT ( 'NONE',  ( -6.237206930280429162, 6.931128591455327559, -0.8289643595828979361 ) ) ;
#76225 = FACE_BOUND ( 'NONE', #124265, .T. ) ;
#76226 = CARTESIAN_POINT ( 'NONE',  ( 6.350466393003619814, 0.5888352225367661230, 1.775644890098279749 ) ) ;
#76227 = CARTESIAN_POINT ( 'NONE',  ( 7.122110765880372618, 7.203550736482235095, 0.7998128361456341429 ) ) ;
#76228 = DIRECTION ( 'NONE',  ( 0.000000000000000000, 0.000000000000000000, 1.000000000000000000 ) ) ;
#76229 = B_SPLINE_CURVE_WITH_KNOTS ( 'NONE', 3,
 ( #157985, #59392, #191509, #140688, #57268, #143891, #11697, #58331, #160094, #77771 ),
 .UNSPECIFIED., .F., .F.,
 ( 4, 2, 2, 2, 4 ),
 ( 2.453269466693580506E-18, 0.0002503535593264591516, 0.0005007071186529159180, 0.0007510606779793734976, 0.001001414237305831186 ),
 .UNSPECIFIED. ) ;
#76230 = EDGE_CURVE ( 'NONE', #137780, #55298, #197851, .T. ) ;
#76231 = CARTESIAN_POINT ( 'NONE',  ( 4.746763178560261309, 5.670883475476017566, 1.082531754730549078 ) ) ;
#76232 = CIRCLE ( 'NONE', #155723, 0.7500000000000011102 ) ;
#76233 = CARTESIAN_POINT ( 'NONE',  ( 3.686212053427321056, 6.121915856213854923, 1.284222742053100941 ) ) ;
#76234 = CARTESIAN_POINT ( 'NONE',  ( -1.364683531250000748, 11.92187500034139980, 0.000000000000000000 ) ) ;
#76235 = CARTESIAN_POINT ( 'NONE',  ( -5.610376637956639101, 5.439860920571172542, 0.000000000000000000 ) ) ;
#76237 = CARTESIAN_POINT ( 'NONE',  ( -5.956828388357799042, 8.042995434541133193, 1.599625672291263179 ) ) ;
#76236 = CARTESIAN_POINT ( 'NONE',  ( 1.854512760316388897, 0.000000000000000000, 2.484105960264901825 ) ) ;
#76238 = CARTESIAN_POINT ( 'NONE',  ( 5.203642376314169482, 1.605325691485876671, 0.6564576239363513199 ) ) ;
#76239 = CARTESIAN_POINT ( 'NONE',  ( -5.416646063859567484, 6.278174148379618735, 1.199719254218450271 ) ) ;
#76240 = CARTESIAN_POINT ( 'NONE',  ( 2.571216573722459486, 1.847313327574741315, 0.9347662400437593000 ) ) ;
#76241 = CARTESIAN_POINT ( 'NONE',  ( 3.005573934588702034, -2.039760842771252136, 0.5671949335201897924 ) ) ;
#76242 = CARTESIAN_POINT ( 'NONE',  ( 8.938903350111612411, 9.323142084752035430, -0.7998128361456221525 ) ) ;
#76243 = DIRECTION ( 'NONE',  ( 0.000000000000000000, 1.000000000000000000, 0.000000000000000000 ) ) ;
#76244 = CARTESIAN_POINT ( 'NONE',  ( 1.692182146996668912, 0.9751594699732427651, -1.711024247558447842 ) ) ;
#76245 = CARTESIAN_POINT ( 'NONE',  ( 6.115260013507548109, 6.015528159276049891, -0.005231617032384894284 ) ) ;
#76246 = CARTESIAN_POINT ( 'NONE',  ( 4.419594888374914099, 5.218910793601261311, -1.082531754730548412 ) ) ;
#76248 = CARTESIAN_POINT ( 'NONE',  ( -0.05268457437105152075, -1.747710896673961622, 0.7768168958157274373 ) ) ;
#76247 = CARTESIAN_POINT ( 'NONE',  ( -3.474999999999998312, -1.370833333333331350, 2.006292185433951047 ) ) ;
#76249 = CARTESIAN_POINT ( 'NONE',  ( 3.996227152750064349, -0.7175114184741685497, -2.177131142417339849 ) ) ;
#76250 = CARTESIAN_POINT ( 'NONE',  ( 0.3635304476994546952, 1.806310985241452949, -0.2645042207462811046 ) ) ;
#76251 = CARTESIAN_POINT ( 'NONE',  ( 6.690022453700429139, 6.769724048930809701, 0.7998128361456331437 ) ) ;
#76253 = EDGE_CURVE ( 'NONE', #14247, #61589, #59942, .T. ) ;
#76252 = CARTESIAN_POINT ( 'NONE',  ( 6.521108698048765362, 8.631046119188804155, -1.443375672974058777 ) ) ;
#76254 = CARTESIAN_POINT ( 'NONE',  ( -7.635213062790267458, 12.05949900656400686, 0.000000000000000000 ) ) ;
#76255 = CARTESIAN_POINT ( 'NONE',  ( 1.353772324478102584, -1.461116690358499337, -1.385217879419877951 ) ) ;
#76256 = CARTESIAN_POINT ( 'NONE',  ( 2.694135368495911731, 0.9291169126603683326, -1.727816930623335967 ) ) ;
#76257 = CARTESIAN_POINT ( 'NONE',  ( -9.643927338022246332, 10.14567007064778004, -0.7998128361456291469 ) ) ;
#76258 = CARTESIAN_POINT ( 'NONE',  ( -5.768104287610143821, 8.816873204598778102, -1.199719254218440723 ) ) ;
#76259 = LINE ( 'NONE', #138069, #92121 ) ;
#76261 = CARTESIAN_POINT ( 'NONE',  ( 3.871743310845751296, 0.9831255770079703193, 1.471438590500689925 ) ) ;
#76260 = CARTESIAN_POINT ( 'NONE',  ( 5.085920031106448747, -2.074780370831377230, -0.2563659892118006489 ) ) ;
#76262 = CARTESIAN_POINT ( 'NONE',  ( -1.225000000000048939, 0.06250000068282191013, -4.336808689942017736E-14 ) ) ;
#76263 = CARTESIAN_POINT ( 'NONE',  ( 6.492113699461491194, -0.6046859696737926226, -2.211003196133090931 ) ) ;
#76264 = CARTESIAN_POINT ( 'NONE',  ( 5.806559702419027857, 1.537982464610265332, 0.8144831216923865691 ) ) ;
#76265 = CARTESIAN_POINT ( 'NONE',  ( 8.599949509769960088, 8.927695937686774386, 1.040834085586084257E-14 ) ) ;
#76266 = CARTESIAN_POINT ( 'NONE',  ( 6.328761054056312396, 0.8840516187795799397, -2.122072247225449626 ) ) ;
#76267 = CARTESIAN_POINT ( 'NONE',  ( 2.971635387262909767, 6.554378586761894887, 0.4847971991465233610 ) ) ;
#76268 = CARTESIAN_POINT ( 'NONE',  ( 5.026542006541363961, 1.714758565716298477, -0.2553409819617598053 ) ) ;
#76269 = MECHANICAL_DESIGN_GEOMETRIC_PRESENTATION_REPRESENTATION (  '', ( #180038 ), #110972 ) ;
#76270 = CARTESIAN_POINT ( 'NONE',  ( 6.215302479579098538, -1.858902078722439732, -1.121643639950772764 ) ) ;
#76271 = CARTESIAN_POINT ( 'NONE',  ( 1.500000000000053291, 7.750000000000000000, 15.74999999999999289 ) ) ;
#76272 = CARTESIAN_POINT ( 'NONE',  ( 0.005274918996244109745, -0.09700444455036473512, 2.115223206416060098 ) ) ;
#76273 = CARTESIAN_POINT ( 'NONE',  ( 4.812500000000003553, 1.451031289061308183, 1.451031289060921159 ) ) ;
#76274 = CARTESIAN_POINT ( 'NONE',  ( -0.7499999999999972244, 5.639583334016151639, -1.299038105676652899 ) ) ;
#76275 = CARTESIAN_POINT ( 'NONE',  ( 3.838824069632059910, 0.2817418319709265040, 1.905555271966542952 ) ) ;
#76276 = CARTESIAN_POINT ( 'NONE',  ( 1.500000000000001332, 11.15625000068279427, 0.000000000000000000 ) ) ;
#76277 = CARTESIAN_POINT ( 'NONE',  ( -0.09271296656673803926, -0.4979868145295326953, -2.173146351408902888 ) ) ;
#76278 = ORIENTED_EDGE ( 'NONE', *, *, #33969, .F. ) ;
#76279 = CARTESIAN_POINT ( 'NONE',  ( -0.7499999999999972244, 4.608333333333352932, -1.299038105676652011 ) ) ;
#76280 = CARTESIAN_POINT ( 'NONE',  ( 4.527533231959700366, 7.369540306339926516, 1.199719254218462483 ) ) ;
#76281 = CARTESIAN_POINT ( 'NONE',  ( 5.459129407796876166, 9.520734742405036144, 1.040834085586084257E-14 ) ) ;
#76282 = CARTESIAN_POINT ( 'NONE',  ( 2.877807283724475251, 0.3237236903097116536, -2.197462771414046223 ) ) ;
#76283 = CARTESIAN_POINT ( 'NONE',  ( -11.01135777277262129, 0.000000000000000000, 1.399999999999998579 ) ) ;
#76284 = CARTESIAN_POINT ( 'NONE',  ( 5.992340707560147806, 8.974519344586754599, 1.082531754730558626 ) ) ;
#76285 = CARTESIAN_POINT ( 'NONE',  ( -8.297226821439000588, 12.62392235841345389, 1.040834085586084257E-14 ) ) ;
#76286 = CARTESIAN_POINT ( 'NONE',  ( 5.058600711674583472, 8.915801573680086634, 0.000000000000000000 ) ) ;
#76287 = CARTESIAN_POINT ( 'NONE',  ( 1.248672897702383988, 1.986100274556975354, -0.3474695496914689818 ) ) ;
#76289 = CARTESIAN_POINT ( 'NONE',  ( 5.969198602517502117, 1.817331191306554850, 0.9757160385870704555 ) ) ;
#76288 = CARTESIAN_POINT ( 'NONE',  ( 9.901532256681887745, 10.44620914241737530, 0.000000000000000000 ) ) ;
#76290 = CARTESIAN_POINT ( 'NONE',  ( 7.065207446497155708, 9.336104335703744539, 0.000000000000000000 ) ) ;
#76291 = CARTESIAN_POINT ( 'NONE',  ( -2.981903720001798597, 5.566305875722335372, -1.199719254218446718 ) ) ;
#76293 = EDGE_CURVE ( 'NONE', #195170, #206877, #199759, .T. ) ;
#76292 = CARTESIAN_POINT ( 'NONE',  ( -2.312195109851927999, 5.463442068584685174, -0.7954731236790282267 ) ) ;
#76294 = CARTESIAN_POINT ( 'NONE',  ( -1.201851678989727383E-14, 1.321875000341419248, 1.575800808251672791 ) ) ;
#76295 = CARTESIAN_POINT ( 'NONE',  ( 0.1804953903597758258, -0.1286114524143982807, -1.740565225867502397 ) ) ;
#76296 = CARTESIAN_POINT ( 'NONE',  ( 5.977189187444425400, -1.726741413813812631, -0.1601111783383553921 ) ) ;
#76297 = CARTESIAN_POINT ( 'NONE',  ( 5.847135585344571673, 0.4968686550196474982, -1.668027988745724777 ) ) ;
#76298 = CARTESIAN_POINT ( 'NONE',  ( 2.771321709476880280, 2.175846111983824382, -0.7217205603756542409 ) ) ;
#76299 = CARTESIAN_POINT ( 'NONE',  ( -1.402160292154681736E-14, -0.8031249996585825279, -1.575800808251665908 ) ) ;
#76300 = CARTESIAN_POINT ( 'NONE',  ( 2.361056629804247020, 1.805642548105116596, -0.3588866333120652174 ) ) ;
#76301 = EDGE_CURVE ( 'NONE', #28244, #123589, #173519, .T. ) ;
#76302 = CARTESIAN_POINT ( 'NONE',  ( 8.615316546479974136, 12.13862083994696839, 1.199719254218450271 ) ) ;
#76303 = CARTESIAN_POINT ( 'NONE',  ( -10.96643471353314503, 6.136560960136473675, 4.903152034993116359 ) ) ;
#76304 = CARTESIAN_POINT ( 'NONE',  ( 2.660947563312371589, -1.587261545009664765, -0.9017329732442300738 ) ) ;
#76305 = CARTESIAN_POINT ( 'NONE',  ( 3.393204081532863459, -0.8197727808607684352, -1.842447475547980495 ) ) ;
#76306 = CARTESIAN_POINT ( 'NONE',  ( -2.602802303699316866, 5.980427087717073320, 1.040834085586084257E-14 ) ) ;
#76307 = CYLINDRICAL_SURFACE ( 'NONE', #155669, 10.24999999999998934 ) ;
#76308 = CARTESIAN_POINT ( 'NONE',  ( 5.579168075997259280, -0.04836659121091852614, -2.105573489274599197 ) ) ;
#76309 = CARTESIAN_POINT ( 'NONE',  ( 7.320800350271525758, 15.00158243878686726, 10.35317514277968343 ) ) ;
#76310 = CARTESIAN_POINT ( 'NONE',  ( 2.295452831283749440, -1.850383948470477602, 0.9288054807428181014 ) ) ;
#76311 = CARTESIAN_POINT ( 'NONE',  ( 3.842846474469570062, 6.570739089268092137, -1.199719254218452047 ) ) ;
#76312 = CARTESIAN_POINT ( 'NONE',  ( -2.353626204688216217E-14, 0.7343750003414536431, 1.570758158831780271 ) ) ;
#76313 = CARTESIAN_POINT ( 'NONE',  ( 4.828832153679845973, 1.461785933843419150, -1.536352341152541046 ) ) ;
#76314 = ITEM_DEFINED_TRANSFORMATION ( 'NONE', 'NONE', #135354,  #200407 ) ;
#76315 = CARTESIAN_POINT ( 'NONE',  ( 0.4164666496747080338, 1.329428171303851824, -1.394508830869565230 ) ) ;
#76316 = B_SPLINE_CURVE_WITH_KNOTS ( 'NONE', 3,
 ( #210280, #192966, #112866, #129141, #111803, #211347 ),
 .UNSPECIFIED., .F., .F.,
 ( 4, 2, 4 ),
 ( 2.054988457695394556E-16, 0.002406600572792993650, 0.004813201145585781736 ),
 .UNSPECIFIED. ) ;
#76317 = ORIENTED_EDGE ( 'NONE', *, *, #77886, .F. ) ;
#76318 = CARTESIAN_POINT ( 'NONE',  ( -5.340986169140711226, 5.195848383611072485, 0.000000000000000000 ) ) ;
#76319 = CARTESIAN_POINT ( 'NONE',  ( 7.425061681778431399, 11.81432239538354345, 0.7998128361456462443 ) ) ;
#76320 = CARTESIAN_POINT ( 'NONE',  ( 4.529832720297257254, 8.298905583739861314, 0.000000000000000000 ) ) ;
#76321 = CARTESIAN_POINT ( 'NONE',  ( 0.000000000000000000, -0.7437499990440860076, -4.012584370867899430 ) ) ;
#76322 = CARTESIAN_POINT ( 'NONE',  ( -4.367698041896780126, 8.247398148854895084, 0.7998128361456481317 ) ) ;
#76323 = CARTESIAN_POINT ( 'NONE',  ( 6.345950370838200350, -1.386202306585911925, -1.604841549997563455 ) ) ;
#76324 = CARTESIAN_POINT ( 'NONE',  ( 2.309725134170067307, -0.4624151122551781179, 2.054391039957529586 ) ) ;
#76325 = CARTESIAN_POINT ( 'NONE',  ( -4.899292406491858820, 6.809203455697518947, -1.599625672291271394 ) ) ;
#76326 = CARTESIAN_POINT ( 'NONE',  ( 8.613507663383630941, 8.943513783569379427, -0.7998128361456221525 ) ) ;
#76327 = CARTESIAN_POINT ( 'NONE',  ( 6.772303520102497920, -0.8766781706108403016, -1.641457522745570996 ) ) ;
#76328 = CARTESIAN_POINT ( 'NONE',  ( 5.926885707468349196, 10.06645042535509660, 1.040834085586084257E-14 ) ) ;
#76329 = LINE ( 'NONE', #9195, #209570 ) ;
#76330 = CARTESIAN_POINT ( 'NONE',  ( -4.984557751679625781, 5.844347460828191565, 1.199719254218452935 ) ) ;
#76331 = CARTESIAN_POINT ( 'NONE',  ( -10.46653140006992899, 11.31330084294416771, -0.7216878364870267237 ) ) ;
#76332 = CARTESIAN_POINT ( 'NONE',  ( -0.1401555495076401980, -1.643345231473653190, -1.339971704266910812 ) ) ;
#76333 = CARTESIAN_POINT ( 'NONE',  ( 0.000000000000000000, 0.5000000000000004441, 0.000000000000000000 ) ) ;
#76335 = CARTESIAN_POINT ( 'NONE',  ( 1.961309178647975715, 1.629323162926434199, 1.092499269706406428 ) ) ;
#76334 = CARTESIAN_POINT ( 'NONE',  ( 0.6124999999999828360, -0.9166666666666628549, 1.060881119635932679 ) ) ;
#76336 = CARTESIAN_POINT ( 'NONE',  ( 1.551884642779034262, 0.6273040060550126862, -2.068667048528524344 ) ) ;
#76338 = CARTESIAN_POINT ( 'NONE',  ( -5.968994907891031154, 6.102274133640173126, 0.7348006213908353512 ) ) ;
#76337 = CARTESIAN_POINT ( 'NONE',  ( -3.474632506852224356, 7.275764701294714420, -0.7998128361456481317 ) ) ;
#76339 = CARTESIAN_POINT ( 'NONE',  ( -1.364683531250000748, 1.509375000341421691, 0.000000000000000000 ) ) ;
#76340 = CARTESIAN_POINT ( 'NONE',  ( 2.730071887686904564, 0.2129287318765031578, 1.727178079207219552 ) ) ;
#76341 = CARTESIAN_POINT ( 'NONE',  ( 5.992340707560151358, 8.014150130285418783, 1.443375672974062551 ) ) ;
#76342 = CARTESIAN_POINT ( 'NONE',  ( -12.15542830485202153, 9.245334104615434256, -2.757920875862237775 ) ) ;
#76343 = CARTESIAN_POINT ( 'NONE',  ( 2.389999771189327937, -0.002812746694069029330, 2.016288306988550438 ) ) ;
#76344 = CARTESIAN_POINT ( 'NONE',  ( -11.01135777277262484, 12.59501355085106233, -1.400000000000001021 ) ) ;
#76345 = CARTESIAN_POINT ( 'NONE',  ( -5.307090785106547415, 5.156303768904543894, -0.7998128361456362523 ) ) ;
#76346 =( BOUNDED_CURVE ( )  B_SPLINE_CURVE ( 3, ( #206515, #74404, #188135, #124305 ),
 .UNSPECIFIED., .F., .T. ) 
 B_SPLINE_CURVE_WITH_KNOTS ( ( 4, 4 ),
 ( 4.576839133004759752, 4.599536981099443977 ),
 .UNSPECIFIED. ) 
 CURVE ( )  GEOMETRIC_REPRESENTATION_ITEM ( )  RATIONAL_B_SPLINE_CURVE ( ( 1.000000000000000000, 0.9999570677684579412, 0.9999570677684579412, 1.000000000000000000 ) ) 
 REPRESENTATION_ITEM ( '' )  );
#76347 = CARTESIAN_POINT ( 'NONE',  ( 1.797671122125501952, -0.6659361598389621495, 1.855707729256075522 ) ) ;
#76349 = CARTESIAN_POINT ( 'NONE',  ( -7.105881907338178038, 7.462819444748888920, -0.7216878364870338292 ) ) ;
#76348 = CARTESIAN_POINT ( 'NONE',  ( 5.801015586618943232, -0.2871438832755985326, -1.890612906794430614 ) ) ;
#76350 = CARTESIAN_POINT ( 'NONE',  ( -6.577113915960849155, 6.845923454808663600, -0.7216878364870338292 ) ) ;
#76351 = CARTESIAN_POINT ( 'NONE',  ( 7.049313524462606395, 7.188896964819984525, 0.000000000000000000 ) ) ;
#76352 = CARTESIAN_POINT ( 'NONE',  ( -6.957269102468015554, 8.145844036748005834, 1.199719254218452047 ) ) ;
#76353 = CARTESIAN_POINT ( 'NONE',  ( 1.559246255342447984, -1.705015668849844124, 1.082290385971399926 ) ) ;
#76354 = CARTESIAN_POINT ( 'NONE',  ( -4.217958839219735800, 3.978389137448586244, 0.5316758947214468289 ) ) ;
#76355 = CARTESIAN_POINT ( 'NONE',  ( 6.229535257468108433, -2.175718461381468405, 0.7693011637898824473 ) ) ;
#76356 = CARTESIAN_POINT ( 'NONE',  ( 5.389097038490845648, 0.1425914310585977562, 1.956722230749983193 ) ) ;
#76357 = CARTESIAN_POINT ( 'NONE',  ( 3.168751141962049545, 1.424179589570490512, -1.349414796185027576 ) ) ;
#76358 = CARTESIAN_POINT ( 'NONE',  ( 9.043452155515161905, 10.50944792197790889, 1.199719254218453823 ) ) ;
#76359 = CARTESIAN_POINT ( 'NONE',  ( 0.7564826839323666174, 1.942540863013635821, -0.5404934282097761944 ) ) ;
#76360 = ORIENTED_EDGE ( 'NONE', *, *, #150546, .T. ) ;
#76361 = CARTESIAN_POINT ( 'NONE',  ( 1.569685796324036264, 1.464237652897076414, 1.529633472619792656 ) ) ;
#76363 = CARTESIAN_POINT ( 'NONE',  ( -7.379715684540041565, 7.504089808251839244, 1.040834085586084257E-14 ) ) ;
#76362 = CARTESIAN_POINT ( 'NONE',  ( -2.435661151949389147, 5.993355110582911038, 0.7998128361456341429 ) ) ;
#76364 = CARTESIAN_POINT ( 'NONE',  ( 1.587592257565925813, -1.832131100469553520, -0.1817911664281982032 ) ) ;
#76365 = EDGE_LOOP ( 'NONE', ( #184802, #203798, #139967, #22478 ) ) ;
#76366 = CARTESIAN_POINT ( 'NONE',  ( 11.15514917209906365, 9.121482996107461716, -4.437425157417320243 ) ) ;
#76367 = CARTESIAN_POINT ( 'NONE',  ( 2.672263739372262137, 2.109986773948614225, -0.2121620573234672125 ) ) ;
#76368 = CARTESIAN_POINT ( 'NONE',  ( -0.7499999999999972244, 4.639583334016150751, -1.299038105676652899 ) ) ;
#76369 = CARTESIAN_POINT ( 'NONE',  ( 6.588372581236919601, 9.773852880496709972, -1.199719254218440723 ) ) ;
#76370 = CARTESIAN_POINT ( 'NONE',  ( 7.537407054554579489, 7.758339416593960536, 0.000000000000000000 ) ) ;
#76371 = CARTESIAN_POINT ( 'NONE',  ( 2.741540247014317533, -1.524689737823584190, -1.386575092742351245 ) ) ;
#76373 = CARTESIAN_POINT ( 'NONE',  ( 1.716098596715152746, 1.718394358364897068, 0.6617865747741287219 ) ) ;
#76372 = CARTESIAN_POINT ( 'NONE',  ( -6.353967546298838087, 10.56471257065732416, 0.000000000000000000 ) ) ;
#76374 = CARTESIAN_POINT ( 'NONE',  ( -0.6823417656249969321, 5.217708333674756283, -1.181850606188749264 ) ) ;
#76375 = CARTESIAN_POINT ( 'NONE',  ( -0.9311234436981564722, -2.728130369558482204, 3.474999999999996536 ) ) ;
#76376 = CARTESIAN_POINT ( 'NONE',  ( 1.478132491927091063, 4.278202457637306999, -0.2687277897297863372 ) ) ;
#76377 = CARTESIAN_POINT ( 'NONE',  ( 6.781144757626058173, -7.161464053357574855, -6.776370306708051849 ) ) ;
#76378 = CARTESIAN_POINT ( 'NONE',  ( 0.8564375766340023288, 2.204168734417511821, -0.1118928034387969561 ) ) ;
#76379 = CARTESIAN_POINT ( 'NONE',  ( 3.198750403210961490, -0.6533003841502099673, -2.166054703861711506 ) ) ;
#76380 = CARTESIAN_POINT ( 'NONE',  ( -8.432808358020034589, 10.86136238915529084, 1.443375672974064550 ) ) ;
#76381 = CARTESIAN_POINT ( 'NONE',  ( 2.056637812947777810, 0.3998733141725440698, 1.766706770180977548 ) ) ;
#76382 = CARTESIAN_POINT ( 'NONE',  ( 3.397576204589338733, -1.886455135561039942, 0.3326623127566808447 ) ) ;
#76383 = CARTESIAN_POINT ( 'NONE',  ( 4.791501694037465953, -1.894250426384593844, 0.8359921707915063394 ) ) ;
#76384 = CARTESIAN_POINT ( 'NONE',  ( 1.364683531249988535, 2.967708333674755394, -0.7879004041258239610 ) ) ;
#76385 = VECTOR ( 'NONE', #18158, 1000.000000000000000 ) ;
#76386 = CARTESIAN_POINT ( 'NONE',  ( 2.782053229633123959, -1.014971971657689709, 1.689997848710776740 ) ) ;
#76387 = CARTESIAN_POINT ( 'NONE',  ( 6.692047312239829182, -0.8199282357786542574, 1.741332009981966022 ) ) ;
#76388 = CARTESIAN_POINT ( 'NONE',  ( 3.889402362484274622, 1.354500474538382626, 1.290456140434749654 ) ) ;
#76390 = CARTESIAN_POINT ( 'NONE',  ( 4.623177087595867540, 8.455029494522658950, -0.3425024339245314464 ) ) ;
#76389 = CARTESIAN_POINT ( 'NONE',  ( 2.543975960257907953, -1.711040505396358657, -1.548661362299937228 ) ) ;
#76391 = CARTESIAN_POINT ( 'NONE',  ( 3.297144150320669542, -1.642529969829407577, 0.8749454559845524226 ) ) ;
#76392 = CARTESIAN_POINT ( 'NONE',  ( -0.6823417656249969321, 3.717708333674754506, -1.181850606188749264 ) ) ;
#76393 = CARTESIAN_POINT ( 'NONE',  ( -4.623494077460110319, 5.352830164246910272, 1.199719254218462483 ) ) ;
#76394 = CARTESIAN_POINT ( 'NONE',  ( 5.289652487626049115, 9.323011668872403845, 0.7998128361456462443 ) ) ;
#76395 = CARTESIAN_POINT ( 'NONE',  ( -1.430949710260827068, 4.025263519208237106, 0.4689103363400777824 ) ) ;
#76396 = CARTESIAN_POINT ( 'NONE',  ( 0.2761803097106649840, 1.214566955493846967, 1.720366990225271842 ) ) ;
#76397 = CARTESIAN_POINT ( 'NONE',  ( -0.6823417656249969321, 3.780208333674754506, -1.181850606188749264 ) ) ;
#76398 = CARTESIAN_POINT ( 'NONE',  ( 6.028642311625867833, 2.081422104948245533, 0.5829617784755269927 ) ) ;
#76399 = CARTESIAN_POINT ( 'NONE',  ( 0.1408863878445747453, 1.934039905153326799, 0.5823465565887532280 ) ) ;
#76400 = CARTESIAN_POINT ( 'NONE',  ( 0.6823417656249882723, -0.4072916663252490466, 1.181850606188755259 ) ) ;
#76401 = CARTESIAN_POINT ( 'NONE',  ( -3.619663825168619731, 7.166765529431275539, 1.040834085586084257E-14 ) ) ;
#76404 = CARTESIAN_POINT ( 'NONE',  ( 4.419594888374914099, 5.218910793601261311, -1.082531754730548412 ) ) ;
#76403 = CARTESIAN_POINT ( 'NONE',  ( 3.285556943749998737, -0.2552083328553768071, -1.896917185911906500 ) ) ;
#76402 = CARTESIAN_POINT ( 'NONE',  ( 6.225128807330042591, 7.291680359087043151, -1.199719254218452047 ) ) ;
#76405 = CARTESIAN_POINT ( 'NONE',  ( -4.411198876399886615, 6.239761003923544713, -1.599625672291271394 ) ) ;
#76406 = CARTESIAN_POINT ( 'NONE',  ( 4.557827498477605488, 1.164984774316142113, 1.645760986912048640 ) ) ;
#76408 = CARTESIAN_POINT ( 'NONE',  ( -7.255021596644144921, 7.636815748939187465, 0.7216878364870317197 ) ) ;
#76407 = CARTESIAN_POINT ( 'NONE',  ( -9.829298180227631576, 10.56986208646148384, 1.040834085586084257E-14 ) ) ;
#76410 = CARTESIAN_POINT ( 'NONE',  ( 1.364683531249996529, 11.21354166700806410, 0.7879004041258403923 ) ) ;
#76409 = CARTESIAN_POINT ( 'NONE',  ( 6.508665849870632236, 1.605377118863276387, -1.447859449074364591 ) ) ;
#76411 = CARTESIAN_POINT ( 'NONE',  ( -11.07599756093943988, 5.827638661946632936, 4.513623486852267774 ) ) ;
#76413 = CARTESIAN_POINT ( 'NONE',  ( -0.0005723727212556676321, -1.878494010790388913, 0.3742560964640674892 ) ) ;
#76412 = CARTESIAN_POINT ( 'NONE',  ( -7.185458225118419584, 7.485382138834033583, 1.040834085586084257E-14 ) ) ;
#76414 = CARTESIAN_POINT ( 'NONE',  ( 1.364683531249988757, 0.6968750003414209138, 0.000000000000000000 ) ) ;
#76415 = LINE ( 'NONE', #164874, #99353 ) ;
#76416 = EDGE_CURVE ( 'NONE', #156928, #124391, #104263, .T. ) ;
#76417 = CARTESIAN_POINT ( 'NONE',  ( -6.009258394948636914E-15, 8.687500000000001776, -1.732050807568875195 ) ) ;
#76418 = CARTESIAN_POINT ( 'NONE',  ( 1.734533752015484875, 0.1665512568347452815, 1.716820151450085596 ) ) ;
#76419 = CARTESIAN_POINT ( 'NONE',  ( 5.083381250481017410, 4.895309311841474553, 0.7998128361456352531 ) ) ;
#76420 = CARTESIAN_POINT ( 'NONE',  ( 4.532168488718122390, 8.509556680138327778, 0.7998128361456271485 ) ) ;
#76421 = CARTESIAN_POINT ( 'NONE',  ( -1.364683531250000748, -0.4281249996585800854, 0.000000000000000000 ) ) ;
#76422 = CARTESIAN_POINT ( 'NONE',  ( 0.6316679966703161453, 0.9168908782757211329, -1.513568585016269452 ) ) ;
#76423 =( BOUNDED_CURVE ( )  B_SPLINE_CURVE ( 2, ( #115443, #196634, #180382, #164141, #117569 ),
 .UNSPECIFIED., .F., .T. ) 
 B_SPLINE_CURVE_WITH_KNOTS ( ( 3, 2, 3 ),
 ( 0.1347995350948868465, 0.1375000000000000111, 0.1409922313975708053 ),
 .UNSPECIFIED. ) 
 CURVE ( )  GEOMETRIC_REPRESENTATION_ITEM ( )  RATIONAL_B_SPLINE_CURVE ( ( 0.9388907138593196589, 0.9131695131383610331, 1.000000000000000000, 0.8877111300685950335, 0.9636488443798445491 ) ) 
 REPRESENTATION_ITEM ( '' )  );
#76424 = CARTESIAN_POINT ( 'NONE',  ( 4.996905641018499544, 0.3326216897534995387, 1.940969171785451364 ) ) ;
#76425 = CARTESIAN_POINT ( 'NONE',  ( 2.438141639825658125, -1.160823251276057011, -1.644512180470799834 ) ) ;
#76426 =( LENGTH_UNIT ( ) NAMED_UNIT ( * ) SI_UNIT ( .MILLI., .METRE. ) );
#76427 = CARTESIAN_POINT ( 'NONE',  ( 3.979664642534729513, 2.078844338038158934, -0.7408291028327750327 ) ) ;
#76428 = CIRCLE ( 'NONE', #180185, 11.92000000000000171 ) ;
#76429 = CARTESIAN_POINT ( 'NONE',  ( 5.383699271828307431, -2.063871618437407740, 0.6740922461795120224 ) ) ;
#76430 = ORIENTED_EDGE ( 'NONE', *, *, #9755, .F. ) ;
#76431 = CARTESIAN_POINT ( 'NONE',  ( -1.500000000000015099, -0.6208333333333116988, -0.8660254037844383745 ) ) ;
#76433 = CARTESIAN_POINT ( 'NONE',  ( 7.253248993186720561, 10.44557901115111065, 1.082531754730558626 ) ) ;
#76432 = PRESENTATION_LAYER_ASSIGNMENT (  '', '', ( #180192 ) ) ;
#76435 = CARTESIAN_POINT ( 'NONE',  ( 3.128529964930274687, 0.4926631579876328271, 1.955168413974051056 ) ) ;
#76434 = CARTESIAN_POINT ( 'NONE',  ( 2.895306150831237879, -0.1582170333116576511, -2.114654843180157950 ) ) ;
#76437 = ORIENTED_EDGE ( 'NONE', *, *, #54068, .F. ) ;
#76436 = CARTESIAN_POINT ( 'NONE',  ( 3.902463391467089426, -1.792703881930355347, -0.2598333579746092692 ) ) ;
#76438 = CARTESIAN_POINT ( 'NONE',  ( 6.387826650694035990, 7.481494509678370264, -1.199719254218452047 ) ) ;
#76439 = EDGE_CURVE ( 'NONE', #136644, #169237, #80365, .T. ) ;
#76440 = ORIENTED_EDGE ( 'NONE', *, *, #188508, .T. ) ;
#76441 = CARTESIAN_POINT ( 'NONE',  ( 0.5845639792326964290, -0.2246964894469481722, -1.857040431621145959 ) ) ;
#76442 = ADVANCED_FACE ( 'NONE', ( #131559 ), #35348, .F. ) ;
#76443 = CARTESIAN_POINT ( 'NONE',  ( 5.672426548614882158, -1.154804106291613675, 1.414059844683832834 ) ) ;
#76444 = CARTESIAN_POINT ( 'NONE',  ( 1.463933648137748733, -1.021544554152100437, 1.620407321708102533 ) ) ;
#76445 = CARTESIAN_POINT ( 'NONE',  ( 1.203907071533382167, 3.212770253743141069, 0.7750000000000135669 ) ) ;
#76446 = CARTESIAN_POINT ( 'NONE',  ( -1.500000000000001110, 8.802083334016133520, 0.8660254037844418162 ) ) ;
#76447 = CARTESIAN_POINT ( 'NONE',  ( 1.364683531249986537, 1.467708333674748289, -0.7879004041258239610 ) ) ;
#76448 = DIRECTION ( 'NONE',  ( 0.3502638921866460531, -1.953969548649011959E-16, -0.9366510587354619499 ) ) ;
#76449 = CARTESIAN_POINT ( 'NONE',  ( 6.455090533882185788, 8.624301270986276080, -1.443375672974078761 ) ) ;
#76450 = CARTESIAN_POINT ( 'NONE',  ( -6.455090533882213322, 6.703562842383589349, -0.7216878364870338292 ) ) ;
#76451 = CARTESIAN_POINT ( 'NONE',  ( -7.286581212701773502, 7.465709267765667789, 0.7998128361456341429 ) ) ;
#76452 = CARTESIAN_POINT ( 'NONE',  ( 3.287459871768631636, 0.04819156399121089784, -2.120204644799832394 ) ) ;
#76454 = CARTESIAN_POINT ( 'NONE',  ( -10.93392920578941485, 5.995216197940580471, 6.296921006145307587 ) ) ;
#76453 = CARTESIAN_POINT ( 'NONE',  ( 5.934142066621461235E-15, -11.10000000000000853, -5.500000000000003553 ) ) ;
#76455 = CARTESIAN_POINT ( 'NONE',  ( 4.885985806860754010, -0.9320292603649924512, 1.737142539612034353 ) ) ;
#76456 = CARTESIAN_POINT ( 'NONE',  ( 6.293217207623316156, -0.1008467329366956045, -1.909883259500498198 ) ) ;
#76457 = ORIENTED_EDGE ( 'NONE', *, *, #89939, .T. ) ;
#76458 = CARTESIAN_POINT ( 'NONE',  ( 0.08772780073029294579, -0.5597381814076306528, 2.041856491864118439 ) ) ;
#76459 = CARTESIAN_POINT ( 'NONE',  ( 6.471393748265519719, 5.229711127717882491, -2.419999999999995044 ) ) ;
#76460 = CARTESIAN_POINT ( 'NONE',  ( 1.082579992370054311, 1.234693400583252609, -1.661741702728709802 ) ) ;
#76461 = CARTESIAN_POINT ( 'NONE',  ( 2.642442020880403586, -1.614326438788242557, 1.079121087018119152 ) ) ;
#76462 = CARTESIAN_POINT ( 'NONE',  ( 5.017399365509065845, 8.011327138806002779, -1.199719254218450271 ) ) ;
#76463 = CARTESIAN_POINT ( 'NONE',  ( 5.875479466675786355, 7.948088359245467416, -1.599625672291283607 ) ) ;
#76465 = CARTESIAN_POINT ( 'NONE',  ( 4.821896187954575197, 8.777295985922343391, 0.7998128361456462443 ) ) ;
#76464 = CARTESIAN_POINT ( 'NONE',  ( 3.750014218873336969, 0.7526759941024010470, 1.950626372838085265 ) ) ;
#76466 = CARTESIAN_POINT ( 'NONE',  ( 4.543390873910906791, 6.393985001019784953, 1.443375672974065660 ) ) ;
#76468 = EDGE_LOOP ( 'NONE', ( #113353, #41324, #42649, #75446, #119610, #132447, #22780, #148828, #29508, #5320 ) ) ;
#76467 = CARTESIAN_POINT ( 'NONE',  ( 0.4338566731940462495, -0.9675643781421030543, -1.531218756180543927 ) ) ;
#76469 = CARTESIAN_POINT ( 'NONE',  ( 5.531908139154323223, -1.397534428995873546, -1.707979418440738195 ) ) ;
#76470 = CARTESIAN_POINT ( 'NONE',  ( -1.020505294851980891E-14, -6.134628647623514119, -11.00029519899099029 ) ) ;
#76471 = CARTESIAN_POINT ( 'NONE',  ( 3.083271082906696048, -0.1608111237268796401, -2.200959079826501075 ) ) ;
#76472 = DIRECTION ( 'NONE',  ( 1.000000000000000000, 3.451266460341926649E-31, 8.638326563840809144E-31 ) ) ;
#76473 = CARTESIAN_POINT ( 'NONE',  ( 2.262237773093742188, 1.911903731097279513, 0.04523801603947830152 ) ) ;
#76474 = CARTESIAN_POINT ( 'NONE',  ( 9.043452155515161905, 10.50944792197790889, 1.199719254218453823 ) ) ;
#76475 = CARTESIAN_POINT ( 'NONE',  ( 5.687960312649480876, -1.310561514506687564, -1.602779375087557190 ) ) ;
#76477 = CARTESIAN_POINT ( 'NONE',  ( 2.518638242371186386, 1.412657066830936392, -1.636333507658905173 ) ) ;
#76476 = CARTESIAN_POINT ( 'NONE',  ( 1.534377212605017915, 8.695787254938599276, -2.514108538948821359 ) ) ;
#76478 = CARTESIAN_POINT ( 'NONE',  ( 4.265290774032561849, 2.125562838249666964, -0.5332280334861272397 ) ) ;
#76479 = ORIENTED_EDGE ( 'NONE', *, *, #91562, .T. ) ;
#76480 = FACE_OUTER_BOUND ( 'NONE', #82538, .T. ) ;
#76481 = CARTESIAN_POINT ( 'NONE',  ( -9.549252947205625119, -7.850763007174473174, 0.06856108760742210539 ) ) ;
#76482 = CARTESIAN_POINT ( 'NONE',  ( -0.4086240214900874745, 7.376738131363727469, 1.961326491624037160 ) ) ;
#76483 = CARTESIAN_POINT ( 'NONE',  ( 3.074666975249065626, 6.809138247757705820, 0.000000000000000000 ) ) ;
#76484 = CARTESIAN_POINT ( 'NONE',  ( -1.642778471875000035, -2.705208332855375986, -2.845375778867859751 ) ) ;
#76485 = CIRCLE ( 'NONE', #201076, 0.07999999999999948819 ) ;
#76486 = CARTESIAN_POINT ( 'NONE',  ( -9.503902493499651882, 10.19023378527882784, 1.040834085586084257E-14 ) ) ;
#76487 = CARTESIAN_POINT ( 'NONE',  ( 4.227110032410640095, 8.153655147779589996, 0.7998128361456271485 ) ) ;
#76488 = CARTESIAN_POINT ( 'NONE',  ( 5.700075226665620498, 0.8442301939139056355, -1.890501578402821847 ) ) ;
#76489 = CARTESIAN_POINT ( 'NONE',  ( 3.914609504329464418, 1.361597497701543480, -1.363134563274936761 ) ) ;
#76490 = CARTESIAN_POINT ( 'NONE',  ( 0.4390776481996219727, -1.704952938511293814, -1.076296438737800454 ) ) ;
#76491 = CARTESIAN_POINT ( 'NONE',  ( -4.905110356762790502, 4.827649200395154772, -0.06592220986076716138 ) ) ;
#76492 = CARTESIAN_POINT ( 'NONE',  ( 4.527533231959700366, 7.369540306339926516, 1.199719254218462483 ) ) ;
#76493 = CARTESIAN_POINT ( 'NONE',  ( 5.495418255317095380, 6.026204583819558813, -0.7979391942483995415 ) ) ;
#76494 = CARTESIAN_POINT ( 'NONE',  ( 4.944182365274345514, -0.9318649803399962073, 1.735062577953277563 ) ) ;
#76495 = CARTESIAN_POINT ( 'NONE',  ( 0.1643758432304382178, -1.428106194732338352, 1.662303017507735792 ) ) ;
#76496 = CARTESIAN_POINT ( 'NONE',  ( 5.004447790439923160, -0.6182884515001166870, -1.717943145347331280 ) ) ;
#76497 = CARTESIAN_POINT ( 'NONE',  ( 7.851580356089786328, 8.332800968292465527, 0.000000000000000000 ) ) ;
#76499 = EDGE_CURVE ( 'NONE', #153088, #68875, #42352, .T. ) ;
#76498 = CARTESIAN_POINT ( 'NONE',  ( 2.507895228403643539, 5.869702166538802501, -0.7216878364870267237 ) ) ;
#76500 = CARTESIAN_POINT ( 'NONE',  ( -4.847922445338252118, 7.813604065273374921, -1.199719254218453823 ) ) ;
#76501 = CARTESIAN_POINT ( 'NONE',  ( 4.472210567661338843, 6.310941310395290493, 1.599625672291261402 ) ) ;
#76502 = ORIENTED_EDGE ( 'NONE', *, *, #92489, .T. ) ;
#76504 = CARTESIAN_POINT ( 'NONE',  ( 5.906499476128409754, -2.003886227978883383, -0.1931989457738275962 ) ) ;
#76503 = CARTESIAN_POINT ( 'NONE',  ( 2.876309626556411203, -0.1380247437976732383, -1.836149222064882514 ) ) ;
#76505 = CARTESIAN_POINT ( 'NONE',  ( 0.7733716040702149908, -2.287020594544288521, 0.2280439049123609840 ) ) ;
#76506 = CARTESIAN_POINT ( 'NONE',  ( 5.910985094894211755, -1.548708053515185812, 1.204094020389692155 ) ) ;
#76507 = CARTESIAN_POINT ( 'NONE',  ( -5.311043488251275591, 7.219303374425030562, -1.599625672291256295 ) ) ;
#76508 = CARTESIAN_POINT ( 'NONE',  ( -4.001066012398721838, 7.682011088333574378, -6.818990669119789124E-05 ) ) ;
#76509 = CARTESIAN_POINT ( 'NONE',  ( -4.081167932913447594, 4.720116328942494555, -1.199719254218452047 ) ) ;
#76510 = CARTESIAN_POINT ( 'NONE',  ( 0.5376586404672692998, 1.932363751568724641, -0.7437053376125392079 ) ) ;
#76511 = CARTESIAN_POINT ( 'NONE',  ( -5.147255595043616516, 6.034161611419515125, 1.199719254218452935 ) ) ;
#76513 = CARTESIAN_POINT ( 'NONE',  ( 6.543818844511720023, 0.6727183027174578056, -1.637219817372371100 ) ) ;
#76512 = CARTESIAN_POINT ( 'NONE',  ( 1.927394988521138774, -1.368145043076029133, -1.581016005797744262 ) ) ;
#76514 = CARTESIAN_POINT ( 'NONE',  ( -8.948250016579809341, 1.813773193624685920, -7.995571895478096103 ) ) ;
#76515 = CARTESIAN_POINT ( 'NONE',  ( -1.164422670175135899, 3.300000000000025135, -0.7116747751938151678 ) ) ;
#76516 = CARTESIAN_POINT ( 'NONE',  ( 2.296107463031165086, 1.396982486531380463, -1.037807123096459838 ) ) ;
#76517 = PRESENTATION_LAYER_ASSIGNMENT (  '', '', ( #197721 ) ) ;
#76518 = CARTESIAN_POINT ( 'NONE',  ( 5.229694566569264680, 7.124396299129368337, 1.599625672291267398 ) ) ;
#76520 = CARTESIAN_POINT ( 'NONE',  ( 3.660338285565247762, 7.214219066560688454, 1.040834085586084257E-14 ) ) ;
#76519 = CARTESIAN_POINT ( 'NONE',  ( -11.52463353791760348, 13.88000000000000256, -3.346594096177641475 ) ) ;
#76521 = CARTESIAN_POINT ( 'NONE',  ( 2.297083607218278978, 1.332544580598886252, 1.095227982430951208 ) ) ;
#76523 = EDGE_CURVE ( 'NONE', #129981, #1117, #66402, .T. ) ;
#76522 = CARTESIAN_POINT ( 'NONE',  ( 2.841561854484982774, 0.7863008361240211297, -2.045831095052422555 ) ) ;
#76524 = CARTESIAN_POINT ( 'NONE',  ( 4.881566871873391555, 2.059980941486462047, -0.7921658822237286346 ) ) ;
#76525 = CARTESIAN_POINT ( 'NONE',  ( -10.77321989194975416, 5.423924896255240213, -6.620653902763565135 ) ) ;
#76526 = CARTESIAN_POINT ( 'NONE',  ( 2.852568495416502703, -2.164958695077593642, -0.1640175257638913364 ) ) ;
#76527 = CARTESIAN_POINT ( 'NONE',  ( 0.9612317138737861422, 0.3586375672061762887, -1.789940867121169843 ) ) ;
#76528 = CARTESIAN_POINT ( 'NONE',  ( 3.151669946411875589, 2.064753251683769442, -0.4682690128248386818 ) ) ;
#76529 = CARTESIAN_POINT ( 'NONE',  ( 6.539320575229249144, 0.007148032025052972194, 1.896977914940492393 ) ) ;
#76530 = ORIENTED_EDGE ( 'NONE', *, *, #31233, .T. ) ;
#76532 = CARTESIAN_POINT ( 'NONE',  ( -0.6823417656250003738, 1.780208333674752952, -1.181850606188749264 ) ) ;
#76531 = CARTESIAN_POINT ( 'NONE',  ( 3.439304851068147428, -1.736875716534720615, -1.496195766483783274 ) ) ;
#76533 = CARTESIAN_POINT ( 'NONE',  ( 11.33772463945037323, 11.00902469614648815, 3.599999999999998757 ) ) ;
#76534 = CARTESIAN_POINT ( 'NONE',  ( 4.891794496432329886, 4.601515088792824670, -0.7998128361456211532 ) ) ;
#76535 = TOROIDAL_SURFACE ( 'NONE', #197594, 11.29999999999999893, 0.2000000000000000111 ) ;
#76536 = CARTESIAN_POINT ( 'NONE',  ( 5.865950696152278709, 0.6470421894613547220, -2.124994868043238672 ) ) ;
#76537 = CARTESIAN_POINT ( 'NONE',  ( -6.412643469583822586, 6.583764924043652655, 1.040834085586084257E-14 ) ) ;
#76538 = CARTESIAN_POINT ( 'NONE',  ( 2.738383840280320669, 6.138605547061593448, 0.7216878364870338292 ) ) ;
#76539 = CARTESIAN_POINT ( 'NONE',  ( -7.009202228140764213, 7.279750142360097875, -0.7216878364870267237 ) ) ;
#76540 = CARTESIAN_POINT ( 'NONE',  ( 0.01492041558614315595, -9.953728265215222137, 10.91968477554610040 ) ) ;
#76541 = ORIENTED_EDGE ( 'NONE', *, *, #39803, .F. ) ;
#76542 = CARTESIAN_POINT ( 'NONE',  ( 3.973279856364997809, -1.994869694282218386, -0.2930714778977619450 ) ) ;
#76544 = CARTESIAN_POINT ( 'NONE',  ( 1.709910653088747789, 0.6025335139634242498, -1.972566668331069195 ) ) ;
#76543 = CARTESIAN_POINT ( 'NONE',  ( 4.774442650306744085, 8.721933525333202653, -0.7998128361456281477 ) ) ;
#76545 = CARTESIAN_POINT ( 'NONE',  ( -5.458264003855187951, 7.602368174425947700, -1.382272695577278387 ) ) ;
#76546 = CARTESIAN_POINT ( 'NONE',  ( 7.095713291905693332, 9.371694488680407886, 1.599625672291268286 ) ) ;
#76548 = EDGE_CURVE ( 'NONE', #106, #132709, #56091, .T. ) ;
#76547 = CARTESIAN_POINT ( 'NONE',  ( -3.285556943750000514, -3.988541666188710089, -1.896917185911906500 ) ) ;
#76549 = CARTESIAN_POINT ( 'NONE',  ( 0.6823417656249899377, 4.926041667008086655, -1.181850606188754593 ) ) ;
#76550 = CARTESIAN_POINT ( 'NONE',  ( 4.664136352776428573, -1.432711980460563250, 1.658340198327029613 ) ) ;
#76551 = CARTESIAN_POINT ( 'NONE',  ( 3.024064729735044921, -1.777011313454954999, 0.9530116517338580451 ) ) ;
#76552 = CARTESIAN_POINT ( 'NONE',  ( 2.067674361007607597, -1.131582805410412673, 1.452419944642673100 ) ) ;
#76553 = EDGE_CURVE ( 'NONE', #56362, #170226, #126486, .T. ) ;
#76554 = CARTESIAN_POINT ( 'NONE',  ( 7.308008492965924141, 8.484763649003774333, -1.199719254218451159 ) ) ;
#76555 = CARTESIAN_POINT ( 'NONE',  ( 6.071303273277399271, 0.1315155018670917386, -1.820917815106848359 ) ) ;
#76556 = CARTESIAN_POINT ( 'NONE',  ( -6.093499974338126179, 9.196501505781426999, -1.199719254218440723 ) ) ;
#76558 = CARTESIAN_POINT ( 'NONE',  ( -4.793689830883590020, 7.750332681742931662, 1.199719254218452935 ) ) ;
#76557 = CARTESIAN_POINT ( 'NONE',  ( 6.245044592044297183, -1.915350782734099200, 1.204081839623271311 ) ) ;
#76559 = CARTESIAN_POINT ( 'NONE',  ( 1.629656122859889811, -1.982562362509328047, 0.7109879831135539341 ) ) ;
#76560 = CARTESIAN_POINT ( 'NONE',  ( -5.611095471209320174, 7.639640364534566075, 1.599625672291263179 ) ) ;
#76561 = CARTESIAN_POINT ( 'NONE',  ( 6.740374924288304648, 11.01552117831172062, 1.040834085586084257E-14 ) ) ;
#76562 = CARTESIAN_POINT ( 'NONE',  ( 8.122743427918724279, 8.649157885426255632, 0.7216878364870267237 ) ) ;
#76563 = CARTESIAN_POINT ( 'NONE',  ( 8.378074386686966690, 23.21353690233408074, 12.34819523476329195 ) ) ;
#76564 = CARTESIAN_POINT ( 'NONE',  ( -7.901704598666176693, 8.113076874732334076, 0.7998128361456602331 ) ) ;
#76565 = CARTESIAN_POINT ( 'NONE',  ( -0.1000000000000080685, -9.999999999999994671, -10.91954211494235238 ) ) ;
#76566 = CARTESIAN_POINT ( 'NONE',  ( 6.873620692004076105, 10.00267932643801672, -1.082531754730537976 ) ) ;
#76567 = CARTESIAN_POINT ( 'NONE',  ( 4.121712324234096059, 7.667736414601909800, 0.7403736254629582625 ) ) ;
#76568 = CARTESIAN_POINT ( 'NONE',  ( -8.161645285746702783, 12.46574390010577105, 0.7216878364870478180 ) ) ;
#76570 = CARTESIAN_POINT ( 'NONE',  ( 2.760263405638745393, 0.7954514732361592788, -2.074294698012415505 ) ) ;
#76569 = CARTESIAN_POINT ( 'NONE',  ( 2.408575119285644384, -2.115224228095522907, -0.1514441693673748146 ) ) ;
#76571 = CARTESIAN_POINT ( 'NONE',  ( 0.5576012004645107822, -1.866542136390366036, -1.177153700605698461 ) ) ;
#76572 = CARTESIAN_POINT ( 'NONE',  ( -5.367048706163331850, 7.354919138647580290, -1.599625672291271394 ) ) ;
#76573 = CARTESIAN_POINT ( 'NONE',  ( 4.635998460869027227, 7.496083073400806818, -1.199719254218452047 ) ) ;
#76574 = CARTESIAN_POINT ( 'NONE',  ( 4.158614545834369736, -0.6132839004606009947, -1.863630207987923004 ) ) ;
#76575 = CARTESIAN_POINT ( 'NONE',  ( 8.052653171512838881, 11.48218023581863001, -1.199719254218446718 ) ) ;
#76576 = CARTESIAN_POINT ( 'NONE',  ( -4.616994038156231106, 6.938643078242441753, 1.201688966319388374 ) ) ;
#76577 = CARTESIAN_POINT ( 'NONE',  ( -9.540655113774951346, 3.481548657788669843, -7.145788969735948015 ) ) ;
#76578 = CARTESIAN_POINT ( 'NONE',  ( 1.364683531249986537, 1.155208333674754728, -0.7879004041258239610 ) ) ;
#76579 = CARTESIAN_POINT ( 'NONE',  ( -5.316205630334276400, 5.374863788244313767, -0.7216878364870338292 ) ) ;
#76581 = ORIENTED_EDGE ( 'NONE', *, *, #44124, .F. ) ;
#76580 = CARTESIAN_POINT ( 'NONE',  ( -6.561783159334145132, 6.757761228752363181, -0.7216878364870278340 ) ) ;
#76582 = AXIS2_PLACEMENT_3D ( 'NONE', #140719, #109316, #57297 ) ;
#76583 = CARTESIAN_POINT ( 'NONE',  ( 3.181995841446764839, 2.068044944583770306, -0.4684364081647199307 ) ) ;
#76584 = CARTESIAN_POINT ( 'NONE',  ( -4.878955176071358757, 6.785476686873604280, -1.599625672291271394 ) ) ;
#76585 = CARTESIAN_POINT ( 'NONE',  ( 4.522454563201145028, 1.332364063043836033, -1.702191164408660251 ) ) ;
#76586 = CARTESIAN_POINT ( 'NONE',  ( 3.597050949361340511, -0.5310884314010614338, 1.763007376093472800 ) ) ;
#76587 = AXIS2_PLACEMENT_3D ( 'NONE', #179045, #30663, #146565 ) ;
#76588 = CARTESIAN_POINT ( 'NONE',  ( -4.217650912117239415, 7.357101779856191293, 0.8466403022913439047 ) ) ;
#76589 = CARTESIAN_POINT ( 'NONE',  ( -1.364683531250014514, 0.05104166700808546175, -0.7879004041258359514 ) ) ;
#76590 = CARTESIAN_POINT ( 'NONE',  ( 5.665861931341662938, -1.099307624823061547, 1.349167961392354620 ) ) ;
#76591 = CARTESIAN_POINT ( 'NONE',  ( 6.827182134110195477, 7.052946558436035573, 2.509100386683714490 ) ) ;
#76592 = CARTESIAN_POINT ( 'NONE',  ( 4.094199201646931741, 4.839282492418613302, -1.082531754730543083 ) ) ;
#76593 = CARTESIAN_POINT ( 'NONE',  ( 9.444983200488291430, 11.02393056587705367, 7.408221049322018636 ) ) ;
#76594 = CARTESIAN_POINT ( 'NONE',  ( 2.465889518630470789, 2.120156730345585938, -0.4209195040108040797 ) ) ;
#76595 = CARTESIAN_POINT ( 'NONE',  ( 5.624374986212743011, 0.3960386850128463920, -1.976653645673176474 ) ) ;
#76596 = CARTESIAN_POINT ( 'NONE',  ( -7.659993601596713830, 9.959745173328078849, -1.443375672974058777 ) ) ;
#76597 = CARTESIAN_POINT ( 'NONE',  ( 1.903414394802248166, 1.797162532295241366, 1.201017911493490020 ) ) ;
#76598 = CARTESIAN_POINT ( 'NONE',  ( 3.216049615590831579, -0.9687177021495720908, -1.716833007709689607 ) ) ;
#76599 = CARTESIAN_POINT ( 'NONE',  ( 1.249000902703297164E-16, 4.099999999999999645, -2.250000000000000000 ) ) ;
#76600 = CARTESIAN_POINT ( 'NONE',  ( 1.589377644589501148, -0.3404682245478432567, -2.282209529656929803 ) ) ;
#76601 = CARTESIAN_POINT ( 'NONE',  ( 4.950698622930713277, -1.642605121802564350, -1.035792469189389386 ) ) ;
#76603 = EDGE_LOOP ( 'NONE', ( #165740, #3968 ) ) ;
#76602 = CARTESIAN_POINT ( 'NONE',  ( -8.798878505144658746, 10.32807501316600884, -1.082531754730543083 ) ) ;
#76604 = CARTESIAN_POINT ( 'NONE',  ( -5.420227550413282636, 9.545625585449309725, 0.7998128361456291469 ) ) ;
#76605 = CARTESIAN_POINT ( 'NONE',  ( 0.07775346131144375561, -0.005211914751935430370, -2.288974916015192651 ) ) ;
#76607 = ORIENTED_EDGE ( 'NONE', *, *, #72791, .T. ) ;
#76606 = CARTESIAN_POINT ( 'NONE',  ( -6.140917232347002042, 6.129101290685087911, -0.7998128361456362523 ) ) ;
#76608 = CARTESIAN_POINT ( 'NONE',  ( -9.314088342463968218, 9.968783942403868892, 0.7216878364870438212 ) ) ;
#76609 = CARTESIAN_POINT ( 'NONE',  ( 2.134064618640969524, -1.441378300436758630, -1.671108464803609417 ) ) ;
#76610 = CARTESIAN_POINT ( 'NONE',  ( 3.285556943750000514, -0.6635416661887083567, 1.896917185911906500 ) ) ;
#76611 = CARTESIAN_POINT ( 'NONE',  ( 6.209812062937981381, 0.5727486527220859713, -1.876249287704085722 ) ) ;
#76612 =( BOUNDED_SURFACE ( )  B_SPLINE_SURFACE ( 3, 2, ( 
 ( #79438, #64262, #45894 ),
 ( #61056, #127215, #193183 ),
 ( #196395, #43766, #48038 ),
 ( #92523, #195331, #158562 ) ),
 .UNSPECIFIED., .F., .F., .T. ) 
 B_SPLINE_SURFACE_WITH_KNOTS ( ( 4, 4 ),
 ( 3, 3 ),
 ( 0.04893088146668655297, 0.05137248493452929027 ),
 ( 0.000000000000000000, 1.000000000000000000 ),
 .UNSPECIFIED. ) 
 GEOMETRIC_REPRESENTATION_ITEM ( )  RATIONAL_B_SPLINE_SURFACE ( (
 ( 1.000000000000000000, 0.7169884966214681299, 1.000000000000000000),
 ( 1.000000000000000000, 0.7174883642158070840, 1.000000000000000000),
 ( 1.000000000000000000, 0.7180610417773362064, 1.000000000000000000),
 ( 1.000000000000000000, 0.7187540717311200478, 1.000000000000000000) ) ) 
 REPRESENTATION_ITEM ( '' )  SURFACE ( )  );
#76613 = CARTESIAN_POINT ( 'NONE',  ( 0.6823417656249917140, 5.655208333674749177, 1.181850606188765695 ) ) ;
#76614 = CARTESIAN_POINT ( 'NONE',  ( -1.500000000000013101, 3.910416667349482012, -0.8660254037844313801 ) ) ;
#76615 = CARTESIAN_POINT ( 'NONE',  ( 5.285422529909848066, 6.578444217690160301, -1.363614577128515082 ) ) ;
#76617 = CARTESIAN_POINT ( 'NONE',  ( 4.764381983412778688E-15, 12.71875000068279782, -1.499999999999998446 ) ) ;
#76616 = CARTESIAN_POINT ( 'NONE',  ( -1.499999999999997780, 7.240846818246208905, -4.154462424328208670 ) ) ;
#76618 = CARTESIAN_POINT ( 'NONE',  ( 5.595603887632320195, -1.841320590885606068, 0.004091980732826016286 ) ) ;
#76619 = ORIENTED_EDGE ( 'NONE', *, *, #201250, .T. ) ;
#76620 = CARTESIAN_POINT ( 'NONE',  ( 1.360316468749957597, -0.5052083329919204724, 0.7853790794159082322 ) ) ;
#76621 = CARTESIAN_POINT ( 'NONE',  ( -7.705111371268023923, 7.883718109434487253, 1.040834085586084257E-14 ) ) ;
#76622 = CARTESIAN_POINT ( 'NONE',  ( 11.04986227068298277, 13.60939997844336169, -1.056429153205399984 ) ) ;
#76623 = CARTESIAN_POINT ( 'NONE',  ( 11.97929049433705373, 11.37999999999999901, 0.7046979865771804130 ) ) ;
#76624 = CARTESIAN_POINT ( 'NONE',  ( 8.889571721160198337, 12.82189538422087693, -7.992081087592324273 ) ) ;
#76625 = CARTESIAN_POINT ( 'NONE',  ( 3.486418057008484617, 7.219238166485217434, 1.040834085586084257E-14 ) ) ;
#76626 = CARTESIAN_POINT ( 'NONE',  ( 0.3212574623711033639, -0.1015677953285927942, 2.058520922655207031 ) ) ;
#76629 = CARTESIAN_POINT ( 'NONE',  ( 4.265079090171526310, 1.784866007061826298, -0.4516350764028759235 ) ) ;
#76628 = CARTESIAN_POINT ( 'NONE',  ( 2.418200368955259361, 0.7924288909779563239, 1.684046449600750561 ) ) ;
#76627 = CARTESIAN_POINT ( 'NONE',  ( -9.604686356149278126, 4.469082183884762749, 7.193747284969080447 ) ) ;
#76630 = CARTESIAN_POINT ( 'NONE',  ( 7.283754839039659146, 9.520799950344851936, -1.599625672291262513 ) ) ;
#76631 = CARTESIAN_POINT ( 'NONE',  ( -9.549101787676201880, 14.79376669176756387, -7.267872539543604127 ) ) ;
#76632 = CARTESIAN_POINT ( 'NONE',  ( -4.959250327548641479, 9.007818825440551791, -0.7998128361456362523 ) ) ;
#76634 = ORIENTED_EDGE ( 'NONE', *, *, #170328, .T. ) ;
#76633 = CARTESIAN_POINT ( 'NONE',  ( 6.610000000000006537, 2.052567036419289614, 2.306714106643445561 ) ) ;
#76635 = EDGE_CURVE ( 'NONE', #107579, #25034, #83744, .T. ) ;
#76636 = CARTESIAN_POINT ( 'NONE',  ( 4.547634279845023109, -1.704780727694398479, -1.401453192282381188 ) ) ;
#76637 = CARTESIAN_POINT ( 'NONE',  ( 5.764971491839249396, -2.041691765312734663, -0.9750072289948004123 ) ) ;
#76638 = CARTESIAN_POINT ( 'NONE',  ( -6.724481002698138532, 6.947575379343695623, -0.7216878364870278340 ) ) ;
#76639 = CARTESIAN_POINT ( 'NONE',  ( 6.082253981448354274, 0.9392408507493594794, 1.548964021007705139 ) ) ;
#76640 = CARTESIAN_POINT ( 'NONE',  ( 0.1105650446291406575, 1.931126588553159884, 0.5807481968119408977 ) ) ;
#76641 = LINE ( 'NONE', #60389, #99104 ) ;
#76642 = CARTESIAN_POINT ( 'NONE',  ( -0.1099460098627005888, 6.494484681433106310, 3.110387376256865011 ) ) ;
#76643 = CARTESIAN_POINT ( 'NONE',  ( 5.971340724440282521, -1.642497693792897451, -0.9790476769208908969 ) ) ;
#76644 = FILL_AREA_STYLE ('',( #7359 ) ) ;
#76645 = AXIS2_PLACEMENT_3D ( 'NONE', #149419, #34593, #181895 ) ;
#76646 = CARTESIAN_POINT ( 'NONE',  ( 1.041631754505952134, 0.7616270086890539748, -1.708776438048253077 ) ) ;
#76647 = CARTESIAN_POINT ( 'NONE',  ( 2.219935720625454412, 0.9462983093676997637, -1.780669029686342331 ) ) ;
#76649 = CARTESIAN_POINT ( 'NONE',  ( 4.442079272866404693, 0.9008978453017953969, -1.903793715863113523 ) ) ;
#76648 = CARTESIAN_POINT ( 'NONE',  ( -9.667127221743832877, 11.23706883257798772, 1.199719254218462483 ) ) ;
#76650 = CARTESIAN_POINT ( 'NONE',  ( 9.368847842243145152, 10.88907622316056312, 1.199719254218453823 ) ) ;
#76652 = CARTESIAN_POINT ( 'NONE',  ( -8.365544474831901667, 9.718555627847388578, 1.199719254218462483 ) ) ;
#76651 = CARTESIAN_POINT ( 'NONE',  ( -1.500000000000015099, -0.6208333333333116988, -0.8660254037844383745 ) ) ;
#76653 = DIRECTION ( 'NONE',  ( 0.000000000000000000, -1.000000000000000000, -9.023263958591317418E-17 ) ) ;
#76654 = CARTESIAN_POINT ( 'NONE',  ( 3.445573674754712545, -1.864599547292019155, 0.7769016540176328922 ) ) ;
#76655 = CARTESIAN_POINT ( 'NONE',  ( 1.364683531249990311, 3.134375000341423245, 1.214306433183764966E-14 ) ) ;
#76656 = CARTESIAN_POINT ( 'NONE',  ( 3.225950485047770933, 5.851027101609320269, 1.199719254218450271 ) ) ;
#76657 = CARTESIAN_POINT ( 'NONE',  ( 4.815789973571149574, -2.120931333841672650, 0.4164600335647972162 ) ) ;
#76658 = CARTESIAN_POINT ( 'NONE',  ( 5.854088466050551887, 10.05179665369283981, 0.7998128361456341429 ) ) ;
#76659 = ADVANCED_FACE ( 'NONE', ( #21716 ), #88909, .T. ) ;
#76660 = CARTESIAN_POINT ( 'NONE',  ( 1.499999999999990896, 5.275000000000022560, 1.214306433183764966E-14 ) ) ;
#76662 = CARTESIAN_POINT ( 'NONE',  ( -9.486277548414619787, -9.200719317737794611, 0.5196196971346862536 ) ) ;
#76661 = CARTESIAN_POINT ( 'NONE',  ( 6.749980374757213575, 8.968339418673846097, 1.599625672291268286 ) ) ;
#76663 = CARTESIAN_POINT ( 'NONE',  ( 7.985389288324691748, 10.33937347451072775, -1.443375672974058777 ) ) ;
#76665 = CARTESIAN_POINT ( 'NONE',  ( 9.368660915953467949, 13.69988896159187242, -7.498844331761238102 ) ) ;
#76664 = CARTESIAN_POINT ( 'NONE',  ( 2.418641202038225302, 0.9268156738743680290, 1.963535311701142483 ) ) ;
#76667 = CARTESIAN_POINT ( 'NONE',  ( 0.5031362391596030381, -1.832460416942282011, 0.1798594046882526221 ) ) ;
#76666 = CARTESIAN_POINT ( 'NONE',  ( -7.700668062882084719, 8.086460282891644979, -0.7216878364870278340 ) ) ;
#76668 = CARTESIAN_POINT ( 'NONE',  ( -1.201851678989727383E-14, 2.321875000341416584, 1.575800808251672791 ) ) ;
#76669 = CARTESIAN_POINT ( 'NONE',  ( 2.665787806004877414, 1.174844384069907655, 1.849873475113596566 ) ) ;
#76670 = CARTESIAN_POINT ( 'NONE',  ( 6.883263157960350043, 2.968548739964393945, 2.406833999121655854 ) ) ;
#76671 = CARTESIAN_POINT ( 'NONE',  ( 2.501149491322187224, 1.817439291034177451, -1.347377658580677817 ) ) ;
#76672 = CARTESIAN_POINT ( 'NONE',  ( -7.555971681517696936, 7.709721804725773175, 0.7998128361456462443 ) ) ;
#76673 = CARTESIAN_POINT ( 'NONE',  ( 1.364683531249988535, 4.426041667008082214, 0.7879004041258500513 ) ) ;
#76674 = CARTESIAN_POINT ( 'NONE',  ( 6.086061792568233209, 7.019478939793144967, 0.9900148145245997178 ) ) ;
#76675 = MECHANICAL_DESIGN_GEOMETRIC_PRESENTATION_REPRESENTATION (  '', ( #21291 ), #194189 ) ;
#76676 = CARTESIAN_POINT ( 'NONE',  ( 0.7500000000000006661, 12.91666666666666607, -1.299038105676657340 ) ) ;
#76677 = CARTESIAN_POINT ( 'NONE',  ( 5.722950238744198614, 8.730506807626655430, 1.082531754730549967 ) ) ;
#76678 = CARTESIAN_POINT ( 'NONE',  ( 4.165142103487808889, 0.2181862141000940336, -1.756177202920036429 ) ) ;
#76679 = CARTESIAN_POINT ( 'NONE',  ( 9.206149998879153529, 10.69926207256923689, 1.199719254218453823 ) ) ;
#76680 = CARTESIAN_POINT ( 'NONE',  ( 0.5695303461548965052, 0.2060630844733425115, -2.095861547610248454 ) ) ;
#76682 = CARTESIAN_POINT ( 'NONE',  ( 0.7499999999999885647, 0.9833333333333569293, 1.299038105676657340 ) ) ;
#76681 = CARTESIAN_POINT ( 'NONE',  ( 1.364683531249996529, 10.46354166700806765, 0.7879004041258405033 ) ) ;
#76683 = CARTESIAN_POINT ( 'NONE',  ( -5.795184315198522285, 5.725746220678519904, -0.7998128361456362523 ) ) ;
#76684 = CARTESIAN_POINT ( 'NONE',  ( -0.2607081404539076663, 7.167562920730330411, -2.095805658632995616 ) ) ;
#76685 = EDGE_LOOP ( 'NONE', ( #71592, #33114, #1159, #105295, #60180 ) ) ;
#76686 = EDGE_CURVE ( 'NONE', #137303, #112565, #108407, .T. ) ;
#76687 = CARTESIAN_POINT ( 'NONE',  ( 7.913155211870404493, 12.38376484715752213, 0.7998128361456462443 ) ) ;
#76688 = CARTESIAN_POINT ( 'NONE',  ( 3.203821283898714345, -1.868584281295191607, 0.09040415888627445495 ) ) ;
#76689 = CARTESIAN_POINT ( 'NONE',  ( 4.909070852169226562, -1.665950775781706028, 1.228889460859562854 ) ) ;
#76690 = CARTESIAN_POINT ( 'NONE',  ( -7.065207446052822249, 7.415365906582643163, -0.7216878364870338292 ) ) ;
#76691 =( LENGTH_UNIT ( ) NAMED_UNIT ( * ) SI_UNIT ( .MILLI., .METRE. ) );
#76692 = CARTESIAN_POINT ( 'NONE',  ( -1.499999999922353666, 8.635424801869593381, 2.574739023100876878 ) ) ;
#76693 = CARTESIAN_POINT ( 'NONE',  ( 7.828907357248368726, 8.098423103070084395, 0.7998128361456281477 ) ) ;
#76694 = CARTESIAN_POINT ( 'NONE',  ( -5.785778052227864343, 5.972700719662596747, -0.3272196074983695357 ) ) ;
#76695 = CARTESIAN_POINT ( 'NONE',  ( -1.201851678989727383E-14, 5.759375000341417028, -1.575800808251660801 ) ) ;
#76696 = CARTESIAN_POINT ( 'NONE',  ( 4.369553226407375313, -0.3375162941181614751, 1.932460123137308861 ) ) ;
#76697 = CARTESIAN_POINT ( 'NONE',  ( 1.124374798274978104, 0.3960433595797500095, -1.976652716225081097 ) ) ;
#76698 = EDGE_CURVE ( 'NONE', #79244, #138713, #27076, .T. ) ;
#76699 = CARTESIAN_POINT ( 'NONE',  ( -2.810282979782591006, 6.500690253046801814, 0.000000000000000000 ) ) ;
#76700 = CARTESIAN_POINT ( 'NONE',  ( 1.475632603725419489, 1.109822327618605442, 1.505604422130282227 ) ) ;
#76701 = CARTESIAN_POINT ( 'NONE',  ( -1.201851678989727383E-14, 4.446875000341417916, -1.575800808251660134 ) ) ;
#76702 = CARTESIAN_POINT ( 'NONE',  ( 3.392840988816598902, -1.941408766427907384, -0.5327130583171105771 ) ) ;
#76704 = CARTESIAN_POINT ( 'NONE',  ( 2.935286906334752199, -1.732537268552689635, -1.216715599779298884 ) ) ;
#76703 = CARTESIAN_POINT ( 'NONE',  ( -5.992340707560165569, 8.014150130285418783, 1.443375672974064550 ) ) ;
#76705 = CARTESIAN_POINT ( 'NONE',  ( 6.825078400183577365, 2.023440267519378999, 2.448151054272352578 ) ) ;
#76706 = CARTESIAN_POINT ( 'NONE',  ( 5.266107318980479235, -2.060723932065291031, 0.1993833602659672022 ) ) ;
#76707 = B_SPLINE_CURVE_WITH_KNOTS ( 'NONE', 3,
 ( #12836, #32310, #180684, #162318 ),
 .UNSPECIFIED., .F., .F.,
 ( 4, 4 ),
 ( 0.000000000000000000, 0.0002908967400263831236 ),
 .UNSPECIFIED. ) ;
#76708 = CARTESIAN_POINT ( 'NONE',  ( 5.083381250481017410, 4.895309311841474553, 0.7998128361456352531 ) ) ;
#76710 = CARTESIAN_POINT ( 'NONE',  ( 11.92619526248521034, 13.52744613914163985, 1.328859120100916558 ) ) ;
#76709 = CARTESIAN_POINT ( 'NONE',  ( -0.006154234300160406693, -2.090381218474619995, -0.04699178559822854429 ) ) ;
#76712 = VERTEX_POINT ( 'NONE', #143012 ) ;
#76711 = CARTESIAN_POINT ( 'NONE',  ( 5.227504313999177477, -1.733024862908550290, 0.5741523302658231298 ) ) ;
#76713 = CARTESIAN_POINT ( 'NONE',  ( 7.781490099239519509, 11.16582331816642260, 1.199719254218460707 ) ) ;
#76714 = CARTESIAN_POINT ( 'NONE',  ( 0.000000000000000000, 0.000000000000000000, 0.000000000000000000 ) ) ;
#76715 = CARTESIAN_POINT ( 'NONE',  ( 10.25134988613697828, 12.94137091940703499, -7.028098868429560220 ) ) ;
#76716 = CARTESIAN_POINT ( 'NONE',  ( 6.088949818052607377, -0.3178892970779038096, -2.183640257897196513 ) ) ;
#76717 = CARTESIAN_POINT ( 'NONE',  ( -0.6823417656250039265, 12.38020833367473017, -1.181850606188755259 ) ) ;
#76718 = CARTESIAN_POINT ( 'NONE',  ( 6.059226159983991167, -1.612925389857391645, 1.026989893868179404 ) ) ;
#76719 = CARTESIAN_POINT ( 'NONE',  ( -9.321394304595349567, 10.83371376257142416, 1.199719254218462483 ) ) ;
#76720 = CARTESIAN_POINT ( 'NONE',  ( 5.309989718046547402, 9.346738437696316737, 0.7998128361456462443 ) ) ;
#76721 = AXIS2_PLACEMENT_3D ( 'NONE', #83624, #210, #116196 ) ;
#76722 = CARTESIAN_POINT ( 'NONE',  ( 1.360316468750004448, 2.546875000341383810, -3.295974604355933479E-14 ) ) ;
#76723 = CARTESIAN_POINT ( 'NONE',  ( 3.592547517496925913, 5.214391408544949869, -1.443375672974058777 ) ) ;
#76724 = CARTESIAN_POINT ( 'NONE',  ( 3.499976210622149253, 7.235056012367825140, 0.7998128361456321445 ) ) ;
#76725 = ORIENTED_EDGE ( 'NONE', *, *, #205691, .F. ) ;
#76726 = CARTESIAN_POINT ( 'NONE',  ( -7.598418745816086783, 7.829519723065708092, 0.000000000000000000 ) ) ;
#76727 = CARTESIAN_POINT ( 'NONE',  ( 10.99462144896566862, -5.166862915010297819, -0.3541067150203519587 ) ) ;
#76729 = CARTESIAN_POINT ( 'NONE',  ( 5.155843554946782703, 9.237177590738404831, -0.7998128361456481317 ) ) ;
#76728 = CARTESIAN_POINT ( 'NONE',  ( 0.3536970929471299763, -9.200718514870473541, -9.493915151247827922 ) ) ;
#76730 = CARTESIAN_POINT ( 'NONE',  ( 0.1399997263885794929, 4.089933038008564559, -2.554595152914000078 ) ) ;
#76731 = CARTESIAN_POINT ( 'NONE',  ( -6.127922243696855453, 7.211959374810172463, 1.082531754730549967 ) ) ;
#76732 = CARTESIAN_POINT ( 'NONE',  ( 5.034155109375821446, 4.767602470560229122, -0.7998128361456221525 ) ) ;
#76733 = CARTESIAN_POINT ( 'NONE',  ( 2.149204315396076481, 1.716066119659308331, -0.9661483248721688399 ) ) ;
#76734 = CARTESIAN_POINT ( 'NONE',  ( 3.567982607561688280, -0.9913820634350967165, 1.755780237201590488 ) ) ;
#76735 = CARTESIAN_POINT ( 'NONE',  ( -6.669721502918952716, 9.868759955792373972, 1.199719254218452047 ) ) ;
#76736 = CARTESIAN_POINT ( 'NONE',  ( 6.827182134110199918, 2.946470958711099541, 2.641117900019366527 ) ) ;
#76737 = CARTESIAN_POINT ( 'NONE',  ( 3.732539452256115275, 0.3211115598316104935, 2.167677955659273348 ) ) ;
#76738 = CARTESIAN_POINT ( 'NONE',  ( 1.676654808981252520, -1.828468026129226542, -0.6065514213326441695 ) ) ;
#76739 = CARTESIAN_POINT ( 'NONE',  ( -8.941766003412679353, 10.39081407785832845, -1.199719254218446718 ) ) ;
#76740 = CYLINDRICAL_SURFACE ( 'NONE', #27531, 11.99999999999999112 ) ;
#76741 = CARTESIAN_POINT ( 'NONE',  ( 0.1333542156527582345, 4.089120883327095335, -2.600857804679152174 ) ) ;
#76742 = CARTESIAN_POINT ( 'NONE',  ( 3.106226591306694651, 6.638031766584184368, 0.000000000000000000 ) ) ;
#76744 = EDGE_CURVE ( 'NONE', #64456, #72069, #44423, .T. ) ;
#76743 = CARTESIAN_POINT ( 'NONE',  ( 6.611572464958476836, 10.86525164242692298, 0.7998128361456462443 ) ) ;
#76745 = CARTESIAN_POINT ( 'NONE',  ( 6.159481859310094620, 6.080483678816896109, 1.040834085586084257E-14 ) ) ;
#76746 = FACE_OUTER_BOUND ( 'NONE', #211500, .T. ) ;
#76747 = CARTESIAN_POINT ( 'NONE',  ( 4.095971805104276164, 7.792734516014745871, 0.7216878364870257245 ) ) ;
#76748 = VERTEX_POINT ( 'NONE', #124677 ) ;
#76750 = CARTESIAN_POINT ( 'NONE',  ( 3.334638158648925099, 1.275257586908218110, -1.557663628481553264 ) ) ;
#76749 = CARTESIAN_POINT ( 'NONE',  ( 5.829618728418341611, 0.9018330327132916269, -1.605192750430362025 ) ) ;
#76751 = CARTESIAN_POINT ( 'NONE',  ( 4.060169364306280393, 1.944150891614861543, -1.225672094199470985 ) ) ;
#76753 = CARTESIAN_POINT ( 'NONE',  ( 2.641259143913599949, 1.703662207083409763, -0.7491738860408488909 ) ) ;
#76752 = CARTESIAN_POINT ( 'NONE',  ( -0.1288028175206881731, 1.984098898469729200, -2.687169534535143178 ) ) ;
#76754 = CARTESIAN_POINT ( 'NONE',  ( 3.285556943750000514, -0.3135416661887098777, 1.896917185911906500 ) ) ;
#76755 = DIRECTION ( 'NONE',  ( 1.276756478318932585E-15, -1.000000000000000000, 1.665334536937738262E-16 ) ) ;
#76756 = CARTESIAN_POINT ( 'NONE',  ( -8.505042434474312074, 8.816971016508505343, -0.7998128361456291469 ) ) ;
#76757 = CARTESIAN_POINT ( 'NONE',  ( -5.261973015879593873, 8.192700047617899273, 1.082531754730549967 ) ) ;
#76759 = CARTESIAN_POINT ( 'NONE',  ( 3.819104250046548632, -0.1383300533824398659, 1.865606469731183825 ) ) ;
#76758 = CARTESIAN_POINT ( 'NONE',  ( 4.564062515778636531, -1.364536961465147913, 1.584173057036510013 ) ) ;
#76760 = CARTESIAN_POINT ( 'NONE',  ( 7.293923454472091450, 7.611924906413328529, 0.7216878364870317197 ) ) ;
#76761 = ORIENTED_EDGE ( 'NONE', *, *, #9358, .F. ) ;
#76762 = COLOUR_RGB ( '', 0.09019608, 0.27058824, 0.51372549) ;
#76763 = CARTESIAN_POINT ( 'NONE',  ( 2.972921499820865066, 6.538163294370741063, -0.5146418828672996160 ) ) ;
#76764 = FACE_OUTER_BOUND ( 'NONE', #144971, .T. ) ;
#76765 = CARTESIAN_POINT ( 'NONE',  ( 6.041572768212772893, -1.254329016146822351, -1.184272192918204514 ) ) ;
#76766 = CARTESIAN_POINT ( 'NONE',  ( -5.225778143063529946, 8.184159369294361497, 1.199719254218452047 ) ) ;
#76767 = CARTESIAN_POINT ( 'NONE',  ( 1.019655691060247227, -1.568448733338474455, 0.7400992899176340734 ) ) ;
#76768 = CARTESIAN_POINT ( 'NONE',  ( -4.369225125877626681, 14.55265043571744421, 11.13763656838536953 ) ) ;
#76769 = CARTESIAN_POINT ( 'NONE',  ( 7.045261094876550167, -5.790678129197933011, 7.662794434365309826 ) ) ;
#76770 = DIRECTION ( 'NONE',  ( 1.000000000000000000, -0.000000000000000000, -0.000000000000000000 ) ) ;
#76771 = CARTESIAN_POINT ( 'NONE',  ( 5.418865745523654631, -1.577555059383651814, 1.491859142196997334 ) ) ;
#76772 = CARTESIAN_POINT ( 'NONE',  ( 4.283705427790140519, 1.194290084605063251, 1.380960126487425166 ) ) ;
#76773 = CARTESIAN_POINT ( 'NONE',  ( 1.850371385673426294, -1.951817131159512719, -0.1975377159662907445 ) ) ;
#76774 = CARTESIAN_POINT ( 'NONE',  ( 6.509000000000050967, 0.001920477310565076989, 2.100274754360692331 ) ) ;
#76775 =( NAMED_UNIT ( * ) SI_UNIT ( $, .STERADIAN. ) SOLID_ANGLE_UNIT ( ) );
#76776 = CARTESIAN_POINT ( 'NONE',  ( -10.47775378526269918, 11.11846759242831872, -0.7998128361456221525 ) ) ;
#76777 = CARTESIAN_POINT ( 'NONE',  ( 7.401861798056875053, 10.72292363345333399, -1.199719254218441611 ) ) ;
#76778 = CARTESIAN_POINT ( 'NONE',  ( 2.701940546545733568, 1.501232083741442125, 1.497845299259781049 ) ) ;
#76779 = CARTESIAN_POINT ( 'NONE',  ( 6.827182134110222123, -0.006956174471953178659, 2.188967759425272330 ) ) ;
#76780 = CARTESIAN_POINT ( 'NONE',  ( 0.000000000000000000, -13.99999999999999822, 6.249999999999995559 ) ) ;
#76781 = AXIS2_PLACEMENT_3D ( 'NONE', #209008, #126807, #139799 ) ;
#76782 = CARTESIAN_POINT ( 'NONE',  ( -5.357982633755392854, 6.353232995037386033, -1.097174801447881487 ) ) ;
#76783 = CARTESIAN_POINT ( 'NONE',  ( 0.9716355300813659390, -0.3074278181635254348, 2.047203142020392441 ) ) ;
#76785 = CARTESIAN_POINT ( 'NONE',  ( 1.499999999999997113, 14.42708333401612819, -0.8660254037844378194 ) ) ;
#76784 = CARTESIAN_POINT ( 'NONE',  ( -10.96384816988334343, 2.972657967447018823, 3.969100948795338812 ) ) ;
#76787 = VERTEX_POINT ( 'NONE', #57459 ) ;
#76786 = CARTESIAN_POINT ( 'NONE',  ( 3.141495721539554697, 0.05644213937440466927, 2.220748567232306847 ) ) ;
#76788 = CARTESIAN_POINT ( 'NONE',  ( 1.126083094664981799, 0.4549445381971609637, 2.253098081826758303 ) ) ;
#76790 = CARTESIAN_POINT ( 'NONE',  ( 6.526245194314398645, 1.055377990298064450, 1.771961156250308145 ) ) ;
#76789 = CARTESIAN_POINT ( 'NONE',  ( 4.857899112398166075, 4.561970474086296079, 1.040834085586084257E-14 ) ) ;
#76792 = CARTESIAN_POINT ( 'NONE',  ( 1.737500000000001155, -2.683333333333332682, 3.009438278150922130 ) ) ;
#76791 = CARTESIAN_POINT ( 'NONE',  ( 4.065465959251388206, 5.836405933916976707, -1.599625672291269396 ) ) ;
#76793 = ADVANCED_FACE ( 'NONE', ( #59582 ), #142706, .T. ) ;
#76794 = CARTESIAN_POINT ( 'NONE',  ( 0.1333542156527530165, 6.948072531064762636, -2.641009269961028139 ) ) ;
#76795 = CARTESIAN_POINT ( 'NONE',  ( 5.987831981441136264, -1.833028718050220940, -0.1737628300680846560 ) ) ;
#76796 = CARTESIAN_POINT ( 'NONE',  ( 0.000000000000000000, 0.4999999999999998890, 0.000000000000000000 ) ) ;
#76797 = CARTESIAN_POINT ( 'NONE',  ( -0.2104748580754183807, 4.084054299358617079, -2.658391380015924010 ) ) ;
#76798 = CARTESIAN_POINT ( 'NONE',  ( 2.660839013829336075, -1.499436941970986759, -0.8522202921518050589 ) ) ;
#76799 = CARTESIAN_POINT ( 'NONE',  ( 1.569546381206438967, 1.394087592100446971, 1.457234012747665508 ) ) ;
#76800 = CARTESIAN_POINT ( 'NONE',  ( 3.358291665479910648, 0.05479990919179249936, -2.298175070600398939 ) ) ;
#76801 = CARTESIAN_POINT ( 'NONE',  ( 2.776973401877864234, -2.164208356635976216, -0.6592219059844570683 ) ) ;
#76802 = CARTESIAN_POINT ( 'NONE',  ( 4.740906146847382985, 0.3592350385927112200, 2.075039481041524247 ) ) ;
#76803 = CARTESIAN_POINT ( 'NONE',  ( -5.126391479742927970, 8.994890803093138487, 0.7216878364870267237 ) ) ;
#76804 = CARTESIAN_POINT ( 'NONE',  ( 3.233429047156919811, -1.186097956103189910, -1.313638963288694228 ) ) ;
#76805 = EDGE_CURVE ( 'NONE', #187025, #140333, #38771, .T. ) ;
#76807 = CARTESIAN_POINT ( 'NONE',  ( -0.02301423135257947214, -0.1624751001964518382, -2.256290569412158220 ) ) ;
#76806 = CARTESIAN_POINT ( 'NONE',  ( 4.055297343818931033, 6.784911763547157193, 1.082531754730549078 ) ) ;
#76808 = CARTESIAN_POINT ( 'NONE',  ( 4.997927640213790212, -0.6233917918176261619, -1.732523409203725606 ) ) ;
#76809 = CARTESIAN_POINT ( 'NONE',  ( -3.750802052474980108, 7.527686161196117887, 1.040834085586084257E-14 ) ) ;
#76810 = CARTESIAN_POINT ( 'NONE',  ( 6.141480396866128899, 6.267408005873028820, -0.7216878364870257245 ) ) ;
#76811 = CARTESIAN_POINT ( 'NONE',  ( -1.201851678989727383E-14, 3.337500000000019007, -1.732050807568863648 ) ) ;
#76812 = AXIS2_PLACEMENT_3D ( 'NONE', #31125, #694, #130813 ) ;
#76813 = CARTESIAN_POINT ( 'NONE',  ( 4.312563266315373234, 2.003113633248252867, 0.8892094534625747393 ) ) ;
#76814 = CARTESIAN_POINT ( 'NONE',  ( -3.100010679019018500, 6.768429558830820980, 1.040834085586084257E-14 ) ) ;
#76815 = CARTESIAN_POINT ( 'NONE',  ( 0.07580519709491868874, 7.079373232789521353, -2.120991669649995526 ) ) ;
#76816 = CARTESIAN_POINT ( 'NONE',  ( 5.055165704564410944, 1.723227314588217318, -1.147259442322377865 ) ) ;
#76817 = CARTESIAN_POINT ( 'NONE',  ( -11.92619526913699879, 10.19999999999999929, -1.328859060402686199 ) ) ;
#76818 = CARTESIAN_POINT ( 'NONE',  ( -1.364683531249997417, 4.759375000341424133, 1.214306433183764966E-14 ) ) ;
#76819 = CARTESIAN_POINT ( 'NONE',  ( 3.580616652426432012, -1.856930023900615456, -0.5128254122194577658 ) ) ;
#76820 = CARTESIAN_POINT ( 'NONE',  ( -1.364683531250010295, 8.880208333674731946, 0.7879004041258445001 ) ) ;
#76821 = CARTESIAN_POINT ( 'NONE',  ( -4.284013352238274841, 4.100363120473813794, -0.7216878364870207285 ) ) ;
#76822 = CARTESIAN_POINT ( 'NONE',  ( 0.2115809916233695465, 1.842269378952247738, -1.241004044093022340 ) ) ;
#76823 = ORIENTED_EDGE ( 'NONE', *, *, #150960, .F. ) ;
#76825 = DIRECTION ( 'NONE',  ( -0.6483454320283799088, 0.000000000000000000, 0.7613463080411786432 ) ) ;
#76824 = CARTESIAN_POINT ( 'NONE',  ( -2.862179826260718762, 6.353310540697199471, 0.000000000000000000 ) ) ;
#76826 = CARTESIAN_POINT ( 'NONE',  ( 3.734381245560244089, 6.444196322207211836, 1.199719254218462483 ) ) ;
#76827 = CARTESIAN_POINT ( 'NONE',  ( 4.217995187182933314, 7.935095128439808576, 0.7216878364870397133 ) ) ;
#76828 = UNCERTAINTY_MEASURE_WITH_UNIT (LENGTH_MEASURE( 1.000000000000000082E-05 ), #12589, 'distance_accuracy_value', 'NONE');
#76829 = CARTESIAN_POINT ( 'NONE',  ( -2.609770642201835855, 0.3830433331901555993, -0.1872689674646474400 ) ) ;
#76830 = CARTESIAN_POINT ( 'NONE',  ( 9.527355378288246968, 12.67468934319733442, 7.222524825386243741 ) ) ;
#76831 = CARTESIAN_POINT ( 'NONE',  ( 1.574581288703358339, 1.320057194528483135, -1.451483715152704246 ) ) ;
#76832 = CARTESIAN_POINT ( 'NONE',  ( 0.6823417656249899377, 1.405208333674752508, 1.181850606188755259 ) ) ;
#76833 = EDGE_CURVE ( 'NONE', #80409, #120419, #201384, .T. ) ;
#76834 = CARTESIAN_POINT ( 'NONE',  ( 0.000000000000000000, -3.517800438942085606, 3.000000000000000000 ) ) ;
#76835 = CARTESIAN_POINT ( 'NONE',  ( 5.617619635959271385, 0.3843197845415853853, -1.923678648292715732 ) ) ;
#76836 = CARTESIAN_POINT ( 'NONE',  ( -9.917953063596627317, 11.52969898140628047, -1.199719254218441611 ) ) ;
#76837 = EDGE_CURVE ( 'NONE', #165149, #101925, #155466, .T. ) ;
#76838 = CARTESIAN_POINT ( 'NONE',  ( -5.056828107772852299, 7.883087978168217269, -1.082531754730548412 ) ) ;
#76839 = CARTESIAN_POINT ( 'NONE',  ( 0.1634265777989383772, -2.022787333623011108, -1.013812598571243617 ) ) ;
#76841 = ORIENTED_EDGE ( 'NONE', *, *, #98624, .T. ) ;
#76840 = CARTESIAN_POINT ( 'NONE',  ( -0.2106725631050099246, 1.363266585364702577, -2.259529575671606505 ) ) ;
#76842 = CARTESIAN_POINT ( 'NONE',  ( -1.364683531250012516, 4.488541667008090208, -0.7879004041258300672 ) ) ;
#76843 = CARTESIAN_POINT ( 'NONE',  ( 6.854760797074392897, -1.525272977149809694, 1.248552938341955798 ) ) ;
#76844 = CARTESIAN_POINT ( 'NONE',  ( 6.415404398373737216, 0.5482957075174756945, 1.644958459601528755 ) ) ;
#76846 = CARTESIAN_POINT ( 'NONE',  ( 2.648187065138879692, 0.7411268365287645432, 2.062558662443473523 ) ) ;
#76845 = CARTESIAN_POINT ( 'NONE',  ( 0.6801582343749935644, 0.9739583336747514863, 1.178068619123805227 ) ) ;
#76847 = CARTESIAN_POINT ( 'NONE',  ( 4.788248824917088697, -1.092567961935811960, 2.032559802855623321 ) ) ;
#76848 = CARTESIAN_POINT ( 'NONE',  ( 5.536423053809180317, 2.029556968340691547, 0.3564751269278207957 ) ) ;
#76849 = CARTESIAN_POINT ( 'NONE',  ( 1.675622358955121571, -1.039060084690484942, 1.640409814757173734 ) ) ;
#76850 = CARTESIAN_POINT ( 'NONE',  ( -6.697364695026446491, 6.915939687060050467, 1.040834085586084257E-14 ) ) ;
#76851 = CARTESIAN_POINT ( 'NONE',  ( 5.586448450635356444, 5.811331697797319507, -0.7399639515439475623 ) ) ;
#76852 = CARTESIAN_POINT ( 'NONE',  ( 4.763993809689464065, 0.6627061821620899851, -2.014485251161435286 ) ) ;
#76853 = CARTESIAN_POINT ( 'NONE',  ( -1.409462824231155764E-15, 2.018041202054154493, 12.16970660573693586 ) ) ;
#76854 = CARTESIAN_POINT ( 'NONE',  ( 2.567029916978436077, -1.034165006014248211, 1.730866473406714068 ) ) ;
#76855 = CARTESIAN_POINT ( 'NONE',  ( -5.138177029454855216, 7.017625839162543677, 1.443375672974064550 ) ) ;
#76856 = CARTESIAN_POINT ( 'NONE',  ( 5.667066814448853407, -1.992748536412903615, -0.9483587796220711574 ) ) ;
#76857 = CARTESIAN_POINT ( 'NONE',  ( 11.52463353791759992, 12.22000000000000242, -3.346594096177641475 ) ) ;
#76858 = DIRECTION ( 'NONE',  ( -0.000000000000000000, 1.000000000000000000, 0.000000000000000000 ) ) ;
#76859 = CARTESIAN_POINT ( 'NONE',  ( 0.2229205655521030172, -0.09321834626660817358, 1.823428419517532983 ) ) ;
#76860 = CARTESIAN_POINT ( 'NONE',  ( -5.803772275101700906, 8.928762199997411386, -1.199719254218452047 ) ) ;
#76862 = CARTESIAN_POINT ( 'NONE',  ( -4.457598643843001973, 8.422558527783969851, 0.000000000000000000 ) ) ;
#76861 = CARTESIAN_POINT ( 'NONE',  ( -4.948302019123040019, 8.085739352127342627, 1.088677458455259650 ) ) ;
#76863 = CARTESIAN_POINT ( 'NONE',  ( 1.482143263342159623, 8.748906972890436506, -2.523193690251291699 ) ) ;
#76864 = ORIENTED_EDGE ( 'NONE', *, *, #189585, .T. ) ;
#76865 = CARTESIAN_POINT ( 'NONE',  ( 5.577047029790810129, -0.04816181868504652158, -2.060495320025256483 ) ) ;
#76866 = CARTESIAN_POINT ( 'NONE',  ( -0.6801582343750004478, 2.598958333674746157, -1.178068619123848526 ) ) ;
#76867 = CARTESIAN_POINT ( 'NONE',  ( -3.765413976293358278, 5.416068943807445635, 1.599625672291267398 ) ) ;
#76868 = CARTESIAN_POINT ( 'NONE',  ( -5.102699428007002602, 6.712334911283204697, 1.441218774086165721 ) ) ;
#76869 = CARTESIAN_POINT ( 'NONE',  ( 4.863928438619278261, 0.6316314618598058983, -1.918449035972718431 ) ) ;
#76871 = ORIENTED_EDGE ( 'NONE', *, *, #174801, .T. ) ;
#76870 = CARTESIAN_POINT ( 'NONE',  ( 1.499999999999989120, 0.2750000000000182854, 0.000000000000000000 ) ) ;
#76873 = CARTESIAN_POINT ( 'NONE',  ( 9.910647101909615841, 10.66476916175714607, 0.000000000000000000 ) ) ;
#76872 = CARTESIAN_POINT ( 'NONE',  ( -4.034433228518296666, 6.864533312316751790, -1.199719254218450271 ) ) ;
#76874 = CARTESIAN_POINT ( 'NONE',  ( 8.281332899848809603, 8.555976559445431562, 0.7998128361456481317 ) ) ;
#76875 = CARTESIAN_POINT ( 'NONE',  ( 3.784101207196560068, -1.017168810052709205, 1.792309825713923166 ) ) ;
#76876 = CARTESIAN_POINT ( 'NONE',  ( 2.391250195717840477, -0.7743161457766101208, -1.862016636315230844 ) ) ;
#76877 = VERTEX_POINT ( 'NONE', #122555 ) ;
#76878 = CARTESIAN_POINT ( 'NONE',  ( 6.727182134110196721, 6.033756510516266935, 2.783943001041962795 ) ) ;
#76879 = CARTESIAN_POINT ( 'NONE',  ( 4.487912541323413329, 5.194651705420806564, 1.199719254218462483 ) ) ;
#76880 = CIRCLE ( 'NONE', #14711, 9.499999999999991118 ) ;
#76882 = ORIENTED_EDGE ( 'NONE', *, *, #20455, .F. ) ;
#76881 = CARTESIAN_POINT ( 'NONE',  ( -10.12374542407608757, -16.99999999999999645, 4.551898349974279334 ) ) ;
#76883 = CARTESIAN_POINT ( 'NONE',  ( 3.304064382408095302, -1.779354530013575131, 0.9478943420064069869 ) ) ;
#76884 = CARTESIAN_POINT ( 'NONE',  ( 2.484105014303281234, -0.3146448974087300288, -1.813890345909507928 ) ) ;
#76885 = CARTESIAN_POINT ( 'NONE',  ( 1.243279834139981999, 0.4545127484847265031, 2.262342451343732463 ) ) ;
#76886 = CARTESIAN_POINT ( 'NONE',  ( 5.896870467300973750, 5.844380064798101237, 0.7998128361456352531 ) ) ;
#76887 = CARTESIAN_POINT ( 'NONE',  ( 2.231903258980330484, -1.410129017595105561, -1.638413920015222125 ) ) ;
#76888 = CARTESIAN_POINT ( 'NONE',  ( -5.038826645773246682, 9.030381520044109322, 0.7998128361456481317 ) ) ;
#76889 = VERTEX_POINT ( 'NONE', #9763 ) ;
#76890 = DIRECTION ( 'NONE',  ( -0.6507913734559640506, -0.7592566023653004592, 0.000000000000000000 ) ) ;
#76891 = CARTESIAN_POINT ( 'NONE',  ( 1.551402291579254022, 0.5461136009352780540, -1.789155053659279071 ) ) ;
#76892 = CARTESIAN_POINT ( 'NONE',  ( 5.541858398712612654, 0.7996551022716179569, -1.802186847774432943 ) ) ;
#76894 = CARTESIAN_POINT ( 'NONE',  ( 9.232739420781973294, 9.873876867108206667, -0.7216878364870257245 ) ) ;
#76893 = CARTESIAN_POINT ( 'NONE',  ( 1.364683531249988535, 2.863541667008082658, 0.7879004041258500513 ) ) ;
#76896 = CARTESIAN_POINT ( 'NONE',  ( 0.8036966383840878914, 1.806304194667744500, 1.267646993260997723 ) ) ;
#76895 = CARTESIAN_POINT ( 'NONE',  ( -6.247609857798938293, 6.183299677053865295, -0.7998128361456291469 ) ) ;
#76897 = CARTESIAN_POINT ( 'NONE',  ( 6.303194806757332458, -1.751150776259063457, 1.104182018118210262 ) ) ;
#76898 = CARTESIAN_POINT ( 'NONE',  ( 3.818592820543298405, 7.606775390609172405, -0.7998128361456221525 ) ) ;
#76899 = CARTESIAN_POINT ( 'NONE',  ( -6.600121851754250812, 6.594563670001734046, 0.7998128361456341429 ) ) ;
#76900 = CARTESIAN_POINT ( 'NONE',  ( 6.539320575229251808, 2.414832891527439962, 2.584256253838035366 ) ) ;
#76901 = CARTESIAN_POINT ( 'NONE',  ( 4.768415704089838947, -1.288333767974993327, 1.492341041399107393 ) ) ;
#76902 = CARTESIAN_POINT ( 'NONE',  ( 0.0004480315400831600455, -0.9938866557669153723, 1.873244595478529728 ) ) ;
#76903 = CARTESIAN_POINT ( 'NONE',  ( 4.231326342634161186, 0.1110341807785204943, 2.305146914567071548 ) ) ;
#76904 = CARTESIAN_POINT ( 'NONE',  ( 2.870046724737782995, -2.040761436538469198, 0.2982335875671269787 ) ) ;
#76905 = CARTESIAN_POINT ( 'NONE',  ( 6.982085921357777281, 7.248114451113292667, 1.040834085586084257E-14 ) ) ;
#76906 = CARTESIAN_POINT ( 'NONE',  ( 4.044074958626150185, 7.940114228364351767, 0.7998128361456271485 ) ) ;
#76907 = CARTESIAN_POINT ( 'NONE',  ( 5.896870467300973750, 5.844380064798101237, 0.7998128361456352531 ) ) ;
#76908 = CARTESIAN_POINT ( 'NONE',  ( -0.6823417656250212460, 1.613541667008083769, 1.181850606188755259 ) ) ;
#76909 = CARTESIAN_POINT ( 'NONE',  ( 3.390420931869152721, 6.113185632892752075, -1.199719254218452047 ) ) ;
#76910 = CARTESIAN_POINT ( 'NONE',  ( 5.572037945092146671, 8.484166121707415797, -1.082531754730543971 ) ) ;
#76911 = CARTESIAN_POINT ( 'NONE',  ( 5.195835581519938629, -1.531768914234220347, -1.538983792029069209 ) ) ;
#76913 = CARTESIAN_POINT ( 'NONE',  ( 4.405690278861111864, -0.7914791229979671883, -1.662609734262666894 ) ) ;
#76912 = CARTESIAN_POINT ( 'NONE',  ( -4.121315508874269007, 5.831287398485176077, -1.443375672974053447 ) ) ;
#76915 = CARTESIAN_POINT ( 'NONE',  ( 6.720655732516647163, 0.6055996050860124047, 1.780393570709505546 ) ) ;
#76914 = CARTESIAN_POINT ( 'NONE',  ( -3.719872605471121751, 6.605953636083950364, -2.419999999999998597 ) ) ;
#76916 = CARTESIAN_POINT ( 'NONE',  ( 5.073855206572205567, -1.217758175834412260, 1.821886007100224969 ) ) ;
#76917 = CARTESIAN_POINT ( 'NONE',  ( 0.6124999999999914957, 0.2291666673494702211, -1.060881119635965764 ) ) ;
#76918 = CARTESIAN_POINT ( 'NONE',  ( 0.4919812829822337030, 1.677557865031731765, 1.518126404548009178 ) ) ;
#76919 = CARTESIAN_POINT ( 'NONE',  ( -3.975490874141025088, 7.849583646728635955, 0.01022619435145193101 ) ) ;
#76920 = CARTESIAN_POINT ( 'NONE',  ( 5.307274686206796765, 7.744096871513173497, 1.304404211447189876 ) ) ;
#76921 = CIRCLE ( 'NONE', #104624, 0.5000000000000000000 ) ;
#76922 = CARTESIAN_POINT ( 'NONE',  ( -3.621436428181653788, 7.239109909604962922, 0.7216878364870338292 ) ) ;
#76923 = DIRECTION ( 'NONE',  ( 0.000000000000000000, -1.000000000000000000, 0.000000000000000000 ) ) ;
#76924 = CARTESIAN_POINT ( 'NONE',  ( 1.340303658288226396, 0.3404796732740902887, 1.736595688552546424 ) ) ;
#76925 = CARTESIAN_POINT ( 'NONE',  ( 5.180342516426402533, 0.9943292982247069478, 1.750330089345548679 ) ) ;
#76926 = CARTESIAN_POINT ( 'NONE',  ( 6.494519276145969577, 7.535692896047149425, -1.199719254218446718 ) ) ;
#76927 = CARTESIAN_POINT ( 'NONE',  ( 4.102637100452250607, -0.6586339671014628250, -2.000395093806975222 ) ) ;
#76928 = CARTESIAN_POINT ( 'NONE',  ( 2.864735742032016752, -0.1435939464786405995, -1.910298799178041351 ) ) ;
#76929 = CARTESIAN_POINT ( 'NONE',  ( 4.356247428692526569, 3.976710176429713250, 0.7998128361456341429 ) ) ;
#76930 = CARTESIAN_POINT ( 'NONE',  ( 4.141030287458704606, -0.1905934838449650226, -1.960285098343496291 ) ) ;
#76931 = CARTESIAN_POINT ( 'NONE',  ( 5.344012529290226965, -1.284645313656457288, -1.558556736529070674 ) ) ;
#76932 = CARTESIAN_POINT ( 'NONE',  ( 2.061206331123175861, 0.3224310286589862629, -1.842498087946140561 ) ) ;
#76935 = ORIENTED_EDGE ( 'NONE', *, *, #63311, .T. ) ;
#76934 = CARTESIAN_POINT ( 'NONE',  ( 1.177825114000274898, 1.883588471398514264, -0.3297955356276888184 ) ) ;
#76933 = CARTESIAN_POINT ( 'NONE',  ( 5.566962092400322248, -1.562093814453187735, -0.7318214103424671713 ) ) ;
#76937 = CARTESIAN_POINT ( 'NONE',  ( 4.528060117284240071, 5.345453560662148718, 1.082531754730560403 ) ) ;
#76936 = CARTESIAN_POINT ( 'NONE',  ( 1.489210700298746692, -0.3264265768355456010, -2.182489157894373033 ) ) ;
#76938 = EDGE_CURVE ( 'NONE', #102987, #47677, #188516, .T. ) ;
#76939 = CARTESIAN_POINT ( 'NONE',  ( -1.364683531250012516, 1.842708333674749843, 0.7879004041258379498 ) ) ;
#76940 = CARTESIAN_POINT ( 'NONE',  ( 6.232861002365865488, -1.862453515449840724, -0.6167318247369477646 ) ) ;
#76941 = CARTESIAN_POINT ( 'NONE',  ( 7.263417608619159083, 9.497073181520933716, -1.599625672291262513 ) ) ;
#76942 = CARTESIAN_POINT ( 'NONE',  ( 6.719622092096638966, -1.813896567892055112, 0.4569536213836836169 ) ) ;
#76943 = CARTESIAN_POINT ( 'NONE',  ( 1.607015867998833336, -0.9165151389911481150, 1.199999999999999734 ) ) ;
#76944 = CARTESIAN_POINT ( 'NONE',  ( -5.901876940650454095, 5.779944607047298177, -0.7998128361456291469 ) ) ;
#76945 = MECHANICAL_DESIGN_GEOMETRIC_PRESENTATION_REPRESENTATION (  '', ( #21717 ), #201543 ) ;
#76946 = CARTESIAN_POINT ( 'NONE',  ( 6.493979434129337314, -7.868711957284896030, 6.493979434129313333 ) ) ;
#76947 = VECTOR ( 'NONE', #98621, 1000.000000000000000 ) ;
#76948 = CARTESIAN_POINT ( 'NONE',  ( 1.926316106172959230, 1.062450747350886848, 1.776810178100460824 ) ) ;
#76949 = CARTESIAN_POINT ( 'NONE',  ( 1.499999999999987121, 2.795833333333352488, -0.8660254037844262731 ) ) ;
#76950 = CARTESIAN_POINT ( 'NONE',  ( 5.286789834324991055, 8.255339675766103724, -1.199719254218452935 ) ) ;
#76951 = CARTESIAN_POINT ( 'NONE',  ( -6.177711549321182716, 10.35908057418338402, 0.7998128361456481317 ) ) ;
#76952 = CARTESIAN_POINT ( 'NONE',  ( 4.523580528814945545, 5.306540700819438960, 1.199719254218452047 ) ) ;
#76953 = CARTESIAN_POINT ( 'NONE',  ( -0.05793207083453711520, -1.244369569480655136, -1.591280167384064637 ) ) ;
#76954 = CARTESIAN_POINT ( 'NONE',  ( -11.84668730067608600, 10.90000000000000036, -1.400000000000001910 ) ) ;
#76955 = CARTESIAN_POINT ( 'NONE',  ( -0.6823417656250003738, 2.967708333674754062, -1.181850606188749264 ) ) ;
#76957 = CARTESIAN_POINT ( 'NONE',  ( 2.347533153460546806, 5.890539112345938300, 0.000000000000000000 ) ) ;
#76956 = CARTESIAN_POINT ( 'NONE',  ( -1.500000000000008216, 11.74999999999999645, 3.469446951953614189E-15 ) ) ;
#76958 = CARTESIAN_POINT ( 'NONE',  ( 5.975935433960424703, 1.776740614516297390, 0.9528632009266969627 ) ) ;
#76959 = CARTESIAN_POINT ( 'NONE',  ( 4.434732071067119641, -1.534896228733380052, 1.146084025706934684 ) ) ;
#76960 = DIRECTION ( 'NONE',  ( 0.6507913734559640506, -0.7592566023653003482, 0.000000000000000000 ) ) ;
#76961 = CARTESIAN_POINT ( 'NONE',  ( 2.806388347806953121, 1.585463108415147149, -1.513251884624075672 ) ) ;
#76962 = CARTESIAN_POINT ( 'NONE',  ( 0.1399997263886003374, 0.002789056014650820314, -1.999853399661279063 ) ) ;
#76963 = CARTESIAN_POINT ( 'NONE',  ( -1.500000000000001332, 0.4312500006828159926, 0.000000000000000000 ) ) ;
#76964 = CARTESIAN_POINT ( 'NONE',  ( 5.343998949255959197, -1.280338926806196431, -1.553582282148850524 ) ) ;
#76965 = CARTESIAN_POINT ( 'NONE',  ( 1.705181254219298115, 1.662258477346746588, -0.9455041445245655485 ) ) ;
#76966 = CARTESIAN_POINT ( 'NONE',  ( -7.366157530926372488, 7.488271962369228874, -0.7998128361456291469 ) ) ;
#76968 = CARTESIAN_POINT ( 'NONE',  ( 0.1578276607246929530, 1.163290555716024244, 1.646825313395771762 ) ) ;
#76967 = CARTESIAN_POINT ( 'NONE',  ( -4.012850279964973232, 4.744375417122949301, 1.082531754730560403 ) ) ;
#76969 = CARTESIAN_POINT ( 'NONE',  ( 1.364683531249996529, 9.526041667008062319, 0.7879004041258405033 ) ) ;
#76971 = CARTESIAN_POINT ( 'NONE',  ( -7.469616286486262524, 7.679250187180907794, 0.7998128361456341429 ) ) ;
#76970 = CARTESIAN_POINT ( 'NONE',  ( 3.192999258835881093, 1.649592175042478015, 1.284459162532962440 ) ) ;
#76973 = VERTEX_POINT ( 'NONE', #157104 ) ;
#76972 = CARTESIAN_POINT ( 'NONE',  ( 1.570901180570225542, 0.1317378181442031559, -1.719804994506502149 ) ) ;
#76974 = CARTESIAN_POINT ( 'NONE',  ( 6.433838290133602200, -2.056603270127650429, 0.5165238393732355382 ) ) ;
#76975 = CARTESIAN_POINT ( 'NONE',  ( 5.124091990960999432, 8.065525525174782828, -1.199719254218452047 ) ) ;
#76976 = VECTOR ( 'NONE', #39013, 1000.000000000000227 ) ;
#76977 = CARTESIAN_POINT ( 'NONE',  ( -7.503508839934899477, -6.893137084989717778, -8.043940816608035504 ) ) ;
#76978 = CARTESIAN_POINT ( 'NONE',  ( 7.505515594164131166, -6.699677480914246530, 8.042162931143014504 ) ) ;
#76979 = CARTESIAN_POINT ( 'NONE',  ( 11.55950211276791251, 9.799999999999998934, -3.221476510067115662 ) ) ;
#76980 = CARTESIAN_POINT ( 'NONE',  ( 5.819474248763732760, 7.812472595022922128, -1.599625672291262513 ) ) ;
#76981 = ORIENTED_EDGE ( 'NONE', *, *, #151476, .T. ) ;
#76982 = CARTESIAN_POINT ( 'NONE',  ( 1.264911064067342439, 3.884384971023816746, -0.4999999999999986122 ) ) ;
#76983 = CARTESIAN_POINT ( 'NONE',  ( 2.789504176380937395, 1.719411750852325449, -0.5702826837221984801 ) ) ;
#76984 = CARTESIAN_POINT ( 'NONE',  ( -6.501298352952815662, 7.543601818988450169, -1.199719254218446718 ) ) ;
#76985 = ORIENTED_EDGE ( 'NONE', *, *, #19052, .T. ) ;
#76986 = CARTESIAN_POINT ( 'NONE',  ( 3.867100128395839942, 5.534702787927018974, -1.599625672291255185 ) ) ;
#76987 = ORIENTED_EDGE ( 'NONE', *, *, #93999, .F. ) ;
#76988 = CARTESIAN_POINT ( 'NONE',  ( 4.064412189046650248, 7.963840997188264659, 0.7998128361456271485 ) ) ;
#76989 = CARTESIAN_POINT ( 'NONE',  ( 3.809066866439265286, 1.528366121442883196, -0.9720638507800370975 ) ) ;
#76990 = CARTESIAN_POINT ( 'NONE',  ( 6.539320575229250920, 3.702490941164796379, 2.411252750440337156 ) ) ;
#76991 = CARTESIAN_POINT ( 'NONE',  ( -10.99039737178640408, -7.697079954928536694, 0.4645147939555879235 ) ) ;
#76992 = CARTESIAN_POINT ( 'NONE',  ( 4.274728378101444903, 7.249864702071729283, 0.9550516446962635797 ) ) ;
#76993 = CARTESIAN_POINT ( 'NONE',  ( 3.736619961808427259, -1.792986960150410036, -0.4983748678565723678 ) ) ;
#76994 = CARTESIAN_POINT ( 'NONE',  ( 1.265090914671564759, 1.769361140067410521, -0.7345930670351871195 ) ) ;
#76995 = CARTESIAN_POINT ( 'NONE',  ( 1.465546361252961560, 1.799214786004127209, -0.3081908958329632742 ) ) ;
#76996 = DIRECTION ( 'NONE',  ( 0.000000000000000000, 0.000000000000000000, 1.000000000000000000 ) ) ;
#76997 = CARTESIAN_POINT ( 'NONE',  ( 6.966220764712121927, 6.002124920821316323, 2.420000000000000373 ) ) ;
#76998 = CARTESIAN_POINT ( 'NONE',  ( 5.067666882003905471, 7.850148838107081417, 1.122879199148843377 ) ) ;
#76999 = CARTESIAN_POINT ( 'NONE',  ( 5.569000761389712117, 7.517326589397093528, 1.347931912527022158 ) ) ;
#77000 = CARTESIAN_POINT ( 'NONE',  ( -4.355417078319587354, 3.138959145363762637, 0.7750000000000117906 ) ) ;
#77001 = CARTESIAN_POINT ( 'NONE',  ( -3.389175213736311587, 4.977123720824209840, 1.443375672974064550 ) ) ;
#77002 = CARTESIAN_POINT ( 'NONE',  ( 7.944714827928043732, 10.29191993738131927, 1.443375672974076540 ) ) ;
#77003 = CARTESIAN_POINT ( 'NONE',  ( 6.262555971378708897, -0.7055598467285629782, -1.838920630280465041 ) ) ;
#77004 = CARTESIAN_POINT ( 'NONE',  ( -5.091250377131585125, 5.898545847196970726, 1.199719254218450271 ) ) ;
#77005 = DIRECTION ( 'NONE',  ( 0.9885327375000381167, 0.000000000000000000, -0.1510067114093955609 ) ) ;
#77006 = CARTESIAN_POINT ( 'NONE',  ( 0.5332922803617061724, -1.479851573012560761, -1.477019686621689143 ) ) ;
#77007 = CARTESIAN_POINT ( 'NONE',  ( 8.446893396513862839, 9.813462703143045474, -1.199719254218445830 ) ) ;
#77008 = CARTESIAN_POINT ( 'NONE',  ( 5.227533229383872104, -1.829308364520453978, 0.6040709075912870096 ) ) ;
#77009 = CARTESIAN_POINT ( 'NONE',  ( -4.720210035852093533, 8.658662141802762946, -0.7998128361456281477 ) ) ;
#77010 = CARTESIAN_POINT ( 'NONE',  ( 1.061231560844998034, 0.3605832424212577769, -1.789441408372116182 ) ) ;
#77011 = CARTESIAN_POINT ( 'NONE',  ( 1.629795212970772456, -2.077151576879713080, 0.7458654493318407352 ) ) ;
#77012 = DIRECTION ( 'NONE',  ( -5.578564026256490882E-16, -1.000000000000000000, -9.066213480720158442E-32 ) ) ;
#77013 = CARTESIAN_POINT ( 'NONE',  ( 0.9317291061951762376, -1.865162313430932750, 0.4216105838140621342 ) ) ;
#77014 = CARTESIAN_POINT ( 'NONE',  ( 6.807475516257630588, -1.579661688080177262, -1.175915379947721773 ) ) ;
#77015 = CARTESIAN_POINT ( 'NONE',  ( 2.067823894287325714, -1.192992258377950865, 1.532381367046357523 ) ) ;
#77016 = CARTESIAN_POINT ( 'NONE',  ( 1.177110994959302825, -0.9039684864705423983, -1.802142742073430171 ) ) ;
#77018 = CARTESIAN_POINT ( 'NONE',  ( 6.977413160773116019, -0.1420559494431029579, 1.829748798152310174 ) ) ;
#77017 = CARTESIAN_POINT ( 'NONE',  ( -5.281783360975562225, 8.319775133516907673, 1.199719254218452935 ) ) ;
#77019 = CARTESIAN_POINT ( 'NONE',  ( 4.869313445963426190, 5.709895770826003414, 1.199719254218452935 ) ) ;
#77020 = CARTESIAN_POINT ( 'NONE',  ( 1.500000000000065503, 7.750000000000000000, -10.99818166789400919 ) ) ;
#77021 = CARTESIAN_POINT ( 'NONE',  ( 8.224992744984721327, 12.74757530245756243, 1.040834085586084257E-14 ) ) ;
#77022 = CARTESIAN_POINT ( 'NONE',  ( -4.283486466913726254, 7.084819080452935403, -1.199719254218452047 ) ) ;
#77023 = CARTESIAN_POINT ( 'NONE',  ( -6.074935347375019390, 9.245119117649618801, 1.199719254218452047 ) ) ;
#77024 = CARTESIAN_POINT ( 'NONE',  ( 2.015410700679621137, -2.124826835150806392, 0.5361769018528695918 ) ) ;
#77025 = CARTESIAN_POINT ( 'NONE',  ( 4.880572111239557920, 4.796348339308675435, -0.7216878364870197293 ) ) ;
#77026 = CARTESIAN_POINT ( 'NONE',  ( 5.989670002187236442, 10.20997511251894529, -0.7998128361456481317 ) ) ;
#77028 =( BOUNDED_CURVE ( )  B_SPLINE_CURVE ( 2, ( #15628, #193329, #128430, #29778, #213816, #65434, #28705 ),
 .UNSPECIFIED., .F., .T. ) 
 B_SPLINE_CURVE_WITH_KNOTS ( ( 3, 2, 2, 3 ),
 ( 0.2125000000000000222, 0.2166666666666667573, 0.2208333333333334647, 0.2250000000000001998 ),
 .UNSPECIFIED. ) 
 CURVE ( )  GEOMETRIC_REPRESENTATION_ITEM ( )  RATIONAL_B_SPLINE_CURVE ( ( 0.9999999999999991118, 0.8660254037844395958, 1.000000000000000000, 0.8660254037844387076, 1.000000000000000000, 0.8660254037844324904, 1.000000000000006217 ) ) 
 REPRESENTATION_ITEM ( '' )  );
#77027 = DIRECTION ( 'NONE',  ( 0.7592566023653005702, 0.6507913734559639396, 0.000000000000000000 ) ) ;
#77029 = CARTESIAN_POINT ( 'NONE',  ( 2.279681363911123970, 1.122676072794186908, 1.439608767588994365 ) ) ;
#77030 = CARTESIAN_POINT ( 'NONE',  ( -4.810445574750349174, 4.506608013497163334, 0.7998128361456341429 ) ) ;
#77031 = CARTESIAN_POINT ( 'NONE',  ( -3.440018289565379028, 5.036440642624797626, 1.599625672291267398 ) ) ;
#77032 = TOROIDAL_SURFACE ( 'NONE', #153247, 11.92000000000000171, 0.08000000000000000167 ) ;
#77033 = CARTESIAN_POINT ( 'NONE',  ( -5.426384371074921553, 7.636973626576035734, -1.343385757368668498 ) ) ;
#77034 = CARTESIAN_POINT ( 'NONE',  ( 4.255647627037052709E-16, 0.5000000000000004441, 3.475000000000000089 ) ) ;
#77035 = CARTESIAN_POINT ( 'NONE',  ( 10.05353459973327368, 11.68787744023238417, -1.199719254218440723 ) ) ;
#77036 = CIRCLE ( 'NONE', #135808, 0.07999999999999991840 ) ;
#77037 = CARTESIAN_POINT ( 'NONE',  ( 0.6801461905075457670, -1.071176224578209935, 1.601055298966150842 ) ) ;
#77038 = CARTESIAN_POINT ( 'NONE',  ( 5.172687041346638814, 1.355624813549320740, -1.418227474788292364 ) ) ;
#77039 = CARTESIAN_POINT ( 'NONE',  ( 1.499999999999993117, 14.60416666666666963, 0.8660254037844409281 ) ) ;
#77040 = CARTESIAN_POINT ( 'NONE',  ( -7.283754839039664475, 9.520799950344851936, -1.599625672291263179 ) ) ;
#77041 = CARTESIAN_POINT ( 'NONE',  ( 4.852928918687680948, 7.749168607522574526, 1.199719254218462483 ) ) ;
#77042 = CARTESIAN_POINT ( 'NONE',  ( 5.161759341795384870, 1.079763445194487970, 1.907048802792680631 ) ) ;
#77043 = CARTESIAN_POINT ( 'NONE',  ( 5.495132332240461714, 5.305409230568988832, 0.7998128361456341429 ) ) ;
#77044 = CARTESIAN_POINT ( 'NONE',  ( 3.537997267176114846, 1.309675639058418550, 1.603382541711120268 ) ) ;
#77046 = CARTESIAN_POINT ( 'NONE',  ( 0.6823417656249899377, 1.405208333674752508, 1.181850606188755259 ) ) ;
#77045 = FACE_OUTER_BOUND ( 'NONE', #139067, .T. ) ;
#77047 = ORIENTED_EDGE ( 'NONE', *, *, #117837, .T. ) ;
#77048 = CARTESIAN_POINT ( 'NONE',  ( 3.903220922379626145, -1.182460753651290775, -1.971142157236325243 ) ) ;
#77050 = ORIENTED_EDGE ( 'NONE', *, *, #3407, .T. ) ;
#77049 = CARTESIAN_POINT ( 'NONE',  ( 6.453317930424781856, 10.47269531889685545, -0.7216878364870267237 ) ) ;
#77052 = CARTESIAN_POINT ( 'NONE',  ( 1.642778471875001811, -0.3427083328553758301, 2.845375778867859751 ) ) ;
#77051 = CARTESIAN_POINT ( 'NONE',  ( 6.211043768836185031, 6.418841616496599123, 0.7216878364870328300 ) ) ;
#77053 = CARTESIAN_POINT ( 'NONE',  ( -7.624693973552363779, -5.341768514962208059, -7.882977371601961991 ) ) ;
#77054 = CARTESIAN_POINT ( 'NONE',  ( -1.772826578343107640, 3.949999999999974420, 0.4499999999999487188 ) ) ;
#77055 = CARTESIAN_POINT ( 'NONE',  ( 4.277243253991915850, 1.269349932698702110, 1.469746654517690487 ) ) ;
#77056 = ORIENTED_EDGE ( 'NONE', *, *, #137134, .T. ) ;
#77057 = CARTESIAN_POINT ( 'NONE',  ( 8.039621902779343188, 12.32338328664385507, -0.7216878364870328300 ) ) ;
#77058 = ORIENTED_EDGE ( 'NONE', *, *, #39139, .F. ) ;
#77059 = CARTESIAN_POINT ( 'NONE',  ( 5.590081826628392925, 1.144292256163012667, 1.532101299821154949 ) ) ;
#77060 = CARTESIAN_POINT ( 'NONE',  ( 5.930603204692192598, 1.663448300781378508, 0.4554771339976750322 ) ) ;
#77061 = CARTESIAN_POINT ( 'NONE',  ( 5.120327457147888950, 1.987497208294352280, 0.3399611521368098854 ) ) ;
#77062 = CARTESIAN_POINT ( 'NONE',  ( 0.000000000000000000, 6.999999999999999112, 0.000000000000000000 ) ) ;
#77063 = CARTESIAN_POINT ( 'NONE',  ( 1.401302286655212948, 1.802556353783949517, -1.272968949304439379 ) ) ;
#77065 = CARTESIAN_POINT ( 'NONE',  ( -3.933273961740340496, 5.682181936820735579, 1.443375672974065660 ) ) ;
#77064 = CARTESIAN_POINT ( 'NONE',  ( -8.045874094706015001, 11.47427131287732927, -1.199719254218446718 ) ) ;
#77066 = CARTESIAN_POINT ( 'NONE',  ( 3.285556943749998737, -3.142708332855375986, -1.896917185911906500 ) ) ;
#77068 = CARTESIAN_POINT ( 'NONE',  ( 6.919227944281516329, -0.1317407762830881124, 1.740281130587753688 ) ) ;
#77067 = CARTESIAN_POINT ( 'NONE',  ( 2.062552408159121775, -1.911915923569502684, -0.8461947581326088041 ) ) ;
#77069 = CARTESIAN_POINT ( 'NONE',  ( 5.836564609439236939, 0.5826586670559866787, -1.930416874340326938 ) ) ;
#77070 = EDGE_CURVE ( 'NONE', #63977, #80984, #75837, .T. ) ;
#77072 = CARTESIAN_POINT ( 'NONE',  ( 3.205313226950608385, -0.4470181708258395004, 2.248096707283386841 ) ) ;
#77071 = CARTESIAN_POINT ( 'NONE',  ( 5.520104819419390907, 6.469152373191302985, 1.199719254218452935 ) ) ;
#77073 = CARTESIAN_POINT ( 'NONE',  ( 1.271012957286155709, 1.034212954684173180, 1.399518829098946204 ) ) ;
#77074 = AXIS2_PLACEMENT_3D ( 'NONE', #207046, #154048, #90125 ) ;
#77075 = CARTESIAN_POINT ( 'NONE',  ( 3.129257641292593650, 1.918792544363761454, 0.9031103230835100248 ) ) ;
#77076 = CARTESIAN_POINT ( 'NONE',  ( 6.773376349083131132, -7.246166700180801001, 6.661184041420955992 ) ) ;
#77077 = CARTESIAN_POINT ( 'NONE',  ( 1.018380972650875460, 1.732250818821230443, -0.07729615888975129023 ) ) ;
#77078 = CARTESIAN_POINT ( 'NONE',  ( 1.360316468749992236, 1.546875000341396689, -1.040834085586084257E-14 ) ) ;
#77079 = CARTESIAN_POINT ( 'NONE',  ( 1.205250485101029723, -1.463924481597483007, -1.148973905474151014 ) ) ;
#77080 = CARTESIAN_POINT ( 'NONE',  ( 1.504584854702104124, 2.168655969765376224, 0.1073316571278438991 ) ) ;
#77081 = CARTESIAN_POINT ( 'NONE',  ( 2.975796278104340331, -0.8128168404246680634, 1.845627246706407210 ) ) ;
#77082 = CARTESIAN_POINT ( 'NONE',  ( 4.593750000000003553, -1.895863743164180493, -0.7852924748297412938 ) ) ;
#77083 =( BOUNDED_SURFACE ( )  B_SPLINE_SURFACE ( 3, 2, ( 
 ( #19397, #85477, #172885 ),
 ( #7141, #151564, #3131 ),
 ( #119111, #9298, #73212 ),
 ( #189116, #69201, #141485 ) ),
 .UNSPECIFIED., .F., .F., .T. ) 
 B_SPLINE_SURFACE_WITH_KNOTS ( ( 4, 4 ),
 ( 3, 3 ),
 ( 0.005313560486515473899, 0.008339948430246690511 ),
 ( 0.000000000000000000, 1.000000000000000000 ),
 .UNSPECIFIED. ) 
 GEOMETRIC_REPRESENTATION_ITEM ( )  RATIONAL_B_SPLINE_SURFACE ( (
 ( 1.000000000000000000, 0.7184380228464071205, 1.000000000000000000),
 ( 1.000000000000000000, 0.7185467277397563635, 1.000000000000000000),
 ( 1.000000000000000000, 0.7186585579881024088, 1.000000000000000000),
 ( 1.000000000000000000, 0.7187737999613684758, 1.000000000000000000) ) ) 
 REPRESENTATION_ITEM ( '' )  SURFACE ( )  );
#77084 = CARTESIAN_POINT ( 'NONE',  ( -1.500000000000013101, 0.9520833340161557468, 0.8660254037844403729 ) ) ;
#77085 = CARTESIAN_POINT ( 'NONE',  ( 6.217406027492617504, -0.2333201818524588411, 1.912260165615098595 ) ) ;
#77086 = CARTESIAN_POINT ( 'NONE',  ( -0.6823417656250003738, 13.90104166700806232, 1.181850606188754593 ) ) ;
#77087 = CARTESIAN_POINT ( 'NONE',  ( 3.076664410187186505, 1.002321471918452556, 1.982530577833590879 ) ) ;
#77088 = EDGE_LOOP ( 'NONE', ( #49667, #125371, #47953, #15559 ) ) ;
#77089 = CARTESIAN_POINT ( 'NONE',  ( -0.2108831679771168421, 6.948330828014878335, -2.492181822431015270 ) ) ;
#77090 = CARTESIAN_POINT ( 'NONE',  ( 0.7499999999999885647, -1.016666666666644847, 1.299038105676657340 ) ) ;
#77091 = CARTESIAN_POINT ( 'NONE',  ( 8.263858322729371153, 9.599921783727809910, -1.199719254218446718 ) ) ;
#77092 = CARTESIAN_POINT ( 'NONE',  ( -1.364683531250014514, -1.011458332991911568, -0.7879004041258359514 ) ) ;
#77093 = CARTESIAN_POINT ( 'NONE',  ( 5.195737816846159873, -1.386088135442983260, -1.388664821390848347 ) ) ;
#77095 = CARTESIAN_POINT ( 'NONE',  ( -7.212574532790110737, 7.517017831117667193, -0.7216878364870278340 ) ) ;
#77094 = CARTESIAN_POINT ( 'NONE',  ( 2.659370686574860976, 6.254349567645977714, -0.7998128361456291469 ) ) ;
#77096 = DIRECTION ( 'NONE',  ( 0.000000000000000000, -1.000000000000000000, 0.000000000000000000 ) ) ;
#77097 = CARTESIAN_POINT ( 'NONE',  ( 5.782586711780850486, -2.205454299129143703, -0.5038293679325082097 ) ) ;
#77098 = AXIS2_PLACEMENT_3D ( 'NONE', #57269, #74586, #140689 ) ;
#77099 = VECTOR ( 'NONE', #86781, 1000.000000000000000 ) ;
#77100 = CARTESIAN_POINT ( 'NONE',  ( 2.207554788950978786, -1.655329399669298818, -1.230451883716067174 ) ) ;
#77101 = CARTESIAN_POINT ( 'NONE',  ( -6.344325816190970357, 9.489131654609717970, 1.199719254218452047 ) ) ;
#77102 = EDGE_CURVE ( 'NONE', #110637, #26075, #93182, .T. ) ;
#77103 = ORIENTED_EDGE ( 'NONE', *, *, #188457, .T. ) ;
#77104 = CARTESIAN_POINT ( 'NONE',  ( 1.499999999999989120, 1.556250000682817047, 0.000000000000000000 ) ) ;
#77105 = CARTESIAN_POINT ( 'NONE',  ( 3.251090012001829788, -1.527204365403836306, -1.079795099579644591 ) ) ;
#77106 = CARTESIAN_POINT ( 'NONE',  ( 2.162404540820038967, 1.068076967457934012, 1.366050734290222834 ) ) ;
#77107 = CARTESIAN_POINT ( 'NONE',  ( 6.567925981381852907, -1.350348970527824211, 1.726830949945204363 ) ) ;
#77108 = CARTESIAN_POINT ( 'NONE',  ( 1.202499378025536636, -2.206952907257493823, 0.001246274542086866404 ) ) ;
#77109 = CARTESIAN_POINT ( 'NONE',  ( 4.188458007013862172, -2.137797052781073237, -0.3198388112101158143 ) ) ;
#77110 = CARTESIAN_POINT ( 'NONE',  ( 5.261643664715593971, 0.9589319835984220219, 1.688605554185283575 ) ) ;
#77111 = CARTESIAN_POINT ( 'NONE',  ( -4.970620135051034616, 8.062850052469723749, -1.111334424012894617 ) ) ;
#77112 = CARTESIAN_POINT ( 'NONE',  ( 0.1562501595635738816, -1.895867669153105339, 0.7852924748299968671 ) ) ;
#77113 = CARTESIAN_POINT ( 'NONE',  ( -0.06968618116158857567, -1.560424145883563929, -1.276814929289785239 ) ) ;
#77114 = CARTESIAN_POINT ( 'NONE',  ( 0.1410940620840978044, 2.031152781523197337, 0.6094965309384676733 ) ) ;
#77115 = CARTESIAN_POINT ( 'NONE',  ( -5.666381855868691808, 5.575476684793721383, 0.000000000000000000 ) ) ;
#77117 = CARTESIAN_POINT ( 'NONE',  ( 5.924453975591452703, -1.462443569488897754, -1.388487997949397368 ) ) ;
#77116 = COLOUR_RGB ( '', 0.40784314, 0.44705882, 0.49803922) ;
#77118 = CARTESIAN_POINT ( 'NONE',  ( -9.677822722056413696, 10.18521468535430685, 1.040834085586084257E-14 ) ) ;
#77119 = CARTESIAN_POINT ( 'NONE',  ( 6.877010230629674759, 9.046264573866535486, 1.599625672291281386 ) ) ;
#77120 = CARTESIAN_POINT ( 'NONE',  ( 4.913904330310220558, 4.697586238308844919, 0.000000000000000000 ) ) ;
#77121 = CARTESIAN_POINT ( 'NONE',  ( 3.510199737632841543, -0.7410081052188906003, -1.668730646197075673 ) ) ;
#77122 = CARTESIAN_POINT ( 'NONE',  ( 1.729795059504362076, -2.077734391967264838, 0.7439406459070623256 ) ) ;
#77123 = ORIENTED_EDGE ( 'NONE', *, *, #170125, .T. ) ;
#77124 = CARTESIAN_POINT ( 'NONE',  ( -5.289089322662584358, 5.343228095960675716, 0.000000000000000000 ) ) ;
#77125 = UNCERTAINTY_MEASURE_WITH_UNIT (LENGTH_MEASURE( 1.000000000000000082E-05 ), #69234, 'distance_accuracy_value', 'NONE');
#77126 = CARTESIAN_POINT ( 'NONE',  ( 3.285556943750000514, -3.201041666188709112, 1.896917185911906500 ) ) ;
#77127 = CARTESIAN_POINT ( 'NONE',  ( -7.645908563102897126, 11.00764485934031889, 1.199719254218453823 ) ) ;
#77128 = CARTESIAN_POINT ( 'NONE',  ( 0.9319058833903216543, -1.969584188619889487, 0.4467263836498857055 ) ) ;
#77129 = CARTESIAN_POINT ( 'NONE',  ( 1.541811043186253061, -1.995513645039903361, 0.7175487213698438227 ) ) ;
#77131 = CARTESIAN_POINT ( 'NONE',  ( 11.92619526913699524, 10.07219975838508219, 1.328859060402684644 ) ) ;
#77130 = CIRCLE ( 'NONE', #132528, 3.475000000000000089 ) ;
#77132 = ORIENTED_EDGE ( 'NONE', *, *, #88561, .T. ) ;
#77133 = CARTESIAN_POINT ( 'NONE',  ( -5.123001941117347080, 7.070197912760590064, 1.599625672291263179 ) ) ;
#77134 = CARTESIAN_POINT ( 'NONE',  ( 3.045584334709343644, 1.312524258565110680, 1.319513337161677846 ) ) ;
#77135 = CARTESIAN_POINT ( 'NONE',  ( 3.005103603723342953, 6.657704637652544832, -0.7998128361456291469 ) ) ;
#77136 = CARTESIAN_POINT ( 'NONE',  ( 1.288190726105652217, -0.9714702286227733241, 1.931199087792371261 ) ) ;
#77137 = CARTESIAN_POINT ( 'NONE',  ( 6.604150280000163242, -0.1430408514614608939, 1.983920101186954721 ) ) ;
#77138 = ORIENTED_EDGE ( 'NONE', *, *, #107143, .T. ) ;
#77139 = EDGE_LOOP ( 'NONE', ( #35199, #83606, #163598 ) ) ;
#77140 = CARTESIAN_POINT ( 'NONE',  ( -10.47097470845587175, 11.11055866948701443, 1.040834085586084257E-14 ) ) ;
#77141 = CARTESIAN_POINT ( 'NONE',  ( 3.861776535121093090, 1.811678901967550326, -0.2252020330209548171 ) ) ;
#77143 = CARTESIAN_POINT ( 'NONE',  ( -5.830469385422084372, 6.191968629596825480, -0.9632026293319171373 ) ) ;
#77142 = CARTESIAN_POINT ( 'NONE',  ( -5.655686355556086120, 6.627330832017406692, 1.199719254218452935 ) ) ;
#77144 = CARTESIAN_POINT ( 'NONE',  ( 6.272253174914359519, 6.990222103910356921, -0.9563742486745248073 ) ) ;
#77145 = CARTESIAN_POINT ( 'NONE',  ( 6.626327358740755180, 0.3474107405085808953, -1.985797104380654376 ) ) ;
#77146 = CARTESIAN_POINT ( 'NONE',  ( 5.367088761235753402, 1.773375748883701419, -0.4946613714205680967 ) ) ;
#77147 = CARTESIAN_POINT ( 'NONE',  ( -0.02319159430949797526, 7.629137130509074716, -2.410989586153565067 ) ) ;
#77148 = CARTESIAN_POINT ( 'NONE',  ( 4.846439200125199243, 2.301219453760998679, 0.1735292846544200795 ) ) ;
#77149 = CARTESIAN_POINT ( 'NONE',  ( 4.193214648376505593, 8.114110533073061404, 0.000000000000000000 ) ) ;
#77150 = CARTESIAN_POINT ( 'NONE',  ( 6.731704548537910782, -1.406307105171537009, -1.641701734229366716 ) ) ;
#77151 = CARTESIAN_POINT ( 'NONE',  ( 1.804143404396211681, 1.437808690349717589, -1.305647666910898730 ) ) ;
#77152 = CARTESIAN_POINT ( 'NONE',  ( 5.237821733363889010, -2.161759915733433068, -0.7809387408506673900 ) ) ;
#77153 = CARTESIAN_POINT ( 'NONE',  ( -1.458777222063855294, 0.5999999999999998668, 1.713029193092652225 ) ) ;
#77154 = CARTESIAN_POINT ( 'NONE',  ( -5.752402313948099533, 9.933162809573264695, -0.7998128361456362523 ) ) ;
#77155 = CARTESIAN_POINT ( 'NONE',  ( 4.662891624058607576, -1.671085903211678270, -0.8408918736509605196 ) ) ;
#77156 = ORIENTED_EDGE ( 'NONE', *, *, #112217, .F. ) ;
#77159 = CARTESIAN_POINT ( 'NONE',  ( -4.274563570058511175, 8.209017608368725405, 0.000000000000000000 ) ) ;
#77158 = CARTESIAN_POINT ( 'NONE',  ( 1.499999999999989120, 0.8062500006828163812, 0.000000000000000000 ) ) ;
#77157 = CARTESIAN_POINT ( 'NONE',  ( 2.882959773793275726, -1.768624019741386277, -0.7279546805132871556 ) ) ;
#77160 = CARTESIAN_POINT ( 'NONE',  ( 4.002700589841681200, -0.6913439845411989415, -2.095861086919461602 ) ) ;
#77161 = CARTESIAN_POINT ( 'NONE',  ( 6.983263157960368339, 4.695310640067480001, 2.508805386165738227 ) ) ;
#77162 = CARTESIAN_POINT ( 'NONE',  ( -0.2110808730067326444, 6.948329377029001996, -2.392166167428900536 ) ) ;
#77163 = CARTESIAN_POINT ( 'NONE',  ( 4.217995187182915551, 7.935095128439824563, 0.7216878364870257245 ) ) ;
#77164 = CARTESIAN_POINT ( 'NONE',  ( -4.760321331729590710, 8.567808963744235839, 0.7216878364870267237 ) ) ;
#77165 = CARTESIAN_POINT ( 'NONE',  ( 1.844934828179781050, -1.667470251784016089, 1.051280099994149841 ) ) ;
#77166 = CARTESIAN_POINT ( 'NONE',  ( 1.501454852758288494, 1.885366349659310048, -1.330307493247370410 ) ) ;
#77167 = CARTESIAN_POINT ( 'NONE',  ( 2.365611650783586040, -0.4327418640146083462, 1.913375882425945917 ) ) ;
#77168 = CARTESIAN_POINT ( 'NONE',  ( -6.473091995881817162, 6.516638514809040217, 0.7998128361456282587 ) ) ;
#77169 = CARTESIAN_POINT ( 'NONE',  ( 6.192244813941197634, 1.021713635409545073, -1.791695130993501417 ) ) ;
#77170 = CARTESIAN_POINT ( 'NONE',  ( 5.029711800989886683, 4.970344644017389513, 1.040834085586084257E-14 ) ) ;
#77171 = CARTESIAN_POINT ( 'NONE',  ( 4.369470645354133431, 8.319742529546998000, 0.7998128361456271485 ) ) ;
#77172 = EDGE_LOOP ( 'NONE', ( #208295, #61968, #183967, #43965 ) ) ;
#77173 = CARTESIAN_POINT ( 'NONE',  ( -8.448702279610222021, 13.00856975952063088, 1.040834085586084257E-14 ) ) ;
#77174 = CARTESIAN_POINT ( 'NONE',  ( -10.60630588279735242, 5.715763139788331948, 4.896273837757428637 ) ) ;
#77175 = CARTESIAN_POINT ( 'NONE',  ( 10.55910270694468345, 11.21337466772398095, 0.7998128361456462443 ) ) ;
#77176 = CARTESIAN_POINT ( 'NONE',  ( 2.272564004159416395, -1.020438428401538200, -1.916272530736246926 ) ) ;
#77177 = CARTESIAN_POINT ( 'NONE',  ( 3.834746474454188013E-15, 12.31250000000000178, 1.500000000000001554 ) ) ;
#77178 = CARTESIAN_POINT ( 'NONE',  ( -4.386105057119274342, 14.48107186952841374, -11.17860366588836563 ) ) ;
#77179 = CARTESIAN_POINT ( 'NONE',  ( -0.9311234436981514762, -1.821869630441516952, -3.474999999999999645 ) ) ;
#77180 = CARTESIAN_POINT ( 'NONE',  ( 1.932664581101939838, 0.1784410483233467293, 1.861995071071875785 ) ) ;
#77181 = CARTESIAN_POINT ( 'NONE',  ( 0.3509462063632540763, -1.656586674793923075, 1.225593781303188967 ) ) ;
#77183 = CARTESIAN_POINT ( 'NONE',  ( 6.827182134110222123, 7.629137130509070275, 2.410944104600701188 ) ) ;
#77182 = CARTESIAN_POINT ( 'NONE',  ( 0.07755575628181145265, 0.6932613274447991802, -2.271134039238668301 ) ) ;
#77184 = CARTESIAN_POINT ( 'NONE',  ( -1.364683531250000748, -0.2406249996585799189, 0.000000000000000000 ) ) ;
#77185 = CARTESIAN_POINT ( 'NONE',  ( 1.770022778749248182, 1.907080152163560971, -0.1419829583147319274 ) ) ;
#77186 = TOROIDAL_SURFACE ( 'NONE', #115442, 11.18000000000000149, 0.08000000000000000167 ) ;
#77187 = CARTESIAN_POINT ( 'NONE',  ( 4.381574371570028603, 1.156860168461280036, 1.339510341777202074 ) ) ;
#77188 = CARTESIAN_POINT ( 'NONE',  ( 1.576665144504853400, -1.351504567317940664, 1.353124384123285617 ) ) ;
#77189 = VECTOR ( 'NONE', #15870, 1000.000000000000000 ) ;
#77190 = CARTESIAN_POINT ( 'NONE',  ( -4.205000198532790279, 8.057583998263570635, 0.7998128361456341429 ) ) ;
#77192 = CARTESIAN_POINT ( 'NONE',  ( 6.433208386744649232, -1.541796563146474286, -1.136648034191472645 ) ) ;
#77191 = CARTESIAN_POINT ( 'NONE',  ( -3.011287625495571607, 6.360174617139689346, -0.7852620323503290978 ) ) ;
#77193 = CARTESIAN_POINT ( 'NONE',  ( 1.499999999999987121, -0.2458333333333099502, 0.8660254037844524744 ) ) ;
#77194 = CARTESIAN_POINT ( 'NONE',  ( 0.4497787391488928810, 1.533077660697563793, 1.391591089521776681 ) ) ;
#77195 = CARTESIAN_POINT ( 'NONE',  ( -1.201851678989727383E-14, 5.587500000000021672, -1.732050807568863648 ) ) ;
#77196 = SURFACE_SIDE_STYLE ('',( #128187 ) ) ;
#77197 = CARTESIAN_POINT ( 'NONE',  ( 5.541831131927607679, 0.7570117910807551143, -1.710825945835430462 ) ) ;
#77198 = CARTESIAN_POINT ( 'NONE',  ( 1.594096589105632011, -1.816728215151931058, -0.1805768397986490248 ) ) ;
#77200 = CARTESIAN_POINT ( 'NONE',  ( 5.176795123377851304, 7.746134302493202561, 1.185296789734613387 ) ) ;
#77199 = CARTESIAN_POINT ( 'NONE',  ( 5.426482453889071245, 1.317083479513626587, -1.770629405693980640 ) ) ;
#77201 = EDGE_CURVE ( 'NONE', #99096, #21883, #148554, .T. ) ;
#77202 = CARTESIAN_POINT ( 'NONE',  ( 0.6823417656249882723, -0.9072916663252494907, 1.181850606188755259 ) ) ;
#77203 = CARTESIAN_POINT ( 'NONE',  ( 2.770046845359328103, -2.040585247751625086, 0.3002346618998888439 ) ) ;
#77204 = CARTESIAN_POINT ( 'NONE',  ( -6.340409392685171674, 10.54889472477470846, 0.7998128361456481317 ) ) ;
#77205 = CARTESIAN_POINT ( 'NONE',  ( 6.610000000000021636, 3.695490760540712127, 2.514297579034238783 ) ) ;
#77206 = CARTESIAN_POINT ( 'NONE',  ( 1.467639082483200630, 3.323620087475168905, 0.3198401300024580896 ) ) ;
#77207 = SURFACE_SIDE_STYLE ('',( #146517 ) ) ;
#77208 = CARTESIAN_POINT ( 'NONE',  ( 6.668631453075247073, 8.873432343378178544, -1.599625672291281386 ) ) ;
#77209 = ORIENTED_EDGE ( 'NONE', *, *, #80428, .T. ) ;
#77210 = CARTESIAN_POINT ( 'NONE',  ( 5.758279222819879806, -2.070544812512797428, -0.003756845764937844813 ) ) ;
#77211 = CARTESIAN_POINT ( 'NONE',  ( -1.402160292154681736E-14, 0.2593750003414224681, -1.575800808251665908 ) ) ;
#77212 = CARTESIAN_POINT ( 'NONE',  ( 2.231903258980330484, -1.410129017595105561, -1.638413920015222125 ) ) ;
#77213 = CARTESIAN_POINT ( 'NONE',  ( -4.740694425254917910, 8.216228820413899570, 0.6995903363472668612 ) ) ;
#77214 = CARTESIAN_POINT ( 'NONE',  ( 3.475264548829166689, -1.782285498782819610, -0.9499825727283210952 ) ) ;
#77215 = CARTESIAN_POINT ( 'NONE',  ( 6.720655732516654268, 4.688933928088002467, 2.736284108207136079 ) ) ;
#77216 = ADVANCED_FACE ( 'NONE', ( #175489 ), #163387, .T. ) ;
#77218 = CARTESIAN_POINT ( 'NONE',  ( 6.914295153289432783, 10.05013286460426691, -1.082531754730537976 ) ) ;
#77217 = CARTESIAN_POINT ( 'NONE',  ( -3.474999999999998312, -1.720833333333333881, 2.006292185433951047 ) ) ;
#77219 = CARTESIAN_POINT ( 'NONE',  ( -7.456058132872594335, 7.663432341298296535, 0.000000000000000000 ) ) ;
#77220 = CARTESIAN_POINT ( 'NONE',  ( 1.341030165941111241, -1.731997234073547220, -1.032477317303444053 ) ) ;
#77222 = CARTESIAN_POINT ( 'NONE',  ( 6.321842903100938216, 1.263506803105146625, -1.790488031206059150 ) ) ;
#77221 = CARTESIAN_POINT ( 'NONE',  ( -4.055860508782465068, 7.883587693554856557, 1.040834085586084257E-14 ) ) ;
#77223 = CARTESIAN_POINT ( 'NONE',  ( 0.7499999999999920064, 4.264583334016150751, 1.299038105676669330 ) ) ;
#77224 = CARTESIAN_POINT ( 'NONE',  ( 4.377155534175989793, -1.710687068321177007, -0.8549628122409487219 ) ) ;
#77225 = CARTESIAN_POINT ( 'NONE',  ( -3.952365473583647315, 4.569846793057691592, 1.199719254218462483 ) ) ;
#77226 = CARTESIAN_POINT ( 'NONE',  ( 6.927853306458752414, 7.184843067064434763, 0.7216878364870317197 ) ) ;
#77228 = CARTESIAN_POINT ( 'NONE',  ( 3.374625213368151133, -0.3961236654455925765, -1.976952669325626299 ) ) ;
#77227 = CARTESIAN_POINT ( 'NONE',  ( -7.985389288324685531, 12.26011190311341537, -0.7216878364870267237 ) ) ;
#77229 = CARTESIAN_POINT ( 'NONE',  ( -0.6823417656250003738, 13.96354166700806942, 1.181850606188754593 ) ) ;
#77230 = CARTESIAN_POINT ( 'NONE',  ( -6.074935347375019390, 9.245119117649618801, 1.199719254218452047 ) ) ;
#77231 = CARTESIAN_POINT ( 'NONE',  ( 4.928557879857294211, 1.651178231652555617, 0.4983569138605167814 ) ) ;
#77232 = CARTESIAN_POINT ( 'NONE',  ( 6.176621499477501054, 9.363752961769195693, -1.199719254218452047 ) ) ;
#77233 = VECTOR ( 'NONE', #38290, 1000.000000000000000 ) ;
#77234 = CARTESIAN_POINT ( 'NONE',  ( 2.683624340501134853, 5.218313266304903664, -1.199719254218446718 ) ) ;
#77235 = DIRECTION ( 'NONE',  ( 0.000000000000000000, -1.000000000000000000, 0.000000000000000000 ) ) ;
#77236 = CARTESIAN_POINT ( 'NONE',  ( 4.024554299415397551, 1.775361691451295520, 0.5892213400080713592 ) ) ;
#77237 = CARTESIAN_POINT ( 'NONE',  ( -5.249999999999987566, -1.374772708486751593, 1.000000000000000888 ) ) ;
#77238 = CARTESIAN_POINT ( 'NONE',  ( 0.6552395816744536194, 1.723207459482085202, -1.147090658606984892 ) ) ;
#77239 = CARTESIAN_POINT ( 'NONE',  ( 0.09500528524172392741, -5.338246727548283665, 10.99984294789629935 ) ) ;
#77240 = ORIENTED_EDGE ( 'NONE', *, *, #202906, .F. ) ;
#77241 = CARTESIAN_POINT ( 'NONE',  ( 6.586573151046549945, -1.108064789702201569, 1.433474704228101748 ) ) ;
#77242 = CARTESIAN_POINT ( 'NONE',  ( 3.553118775233146120, 6.302999783484076524, -1.199719254218453823 ) ) ;
#77243 = ADVANCED_FACE ( 'NONE', ( #206891 ), #170675, .T. ) ;
#77244 = CARTESIAN_POINT ( 'NONE',  ( 0.05258934297286410597, 0.3095000349466696110, 1.784779062553583984 ) ) ;
#77245 = CARTESIAN_POINT ( 'NONE',  ( 6.170369307550831017, 6.371388078330353366, 0.7216878364870328300 ) ) ;
#77246 = CARTESIAN_POINT ( 'NONE',  ( -9.579764304849156531, -9.999999999999994671, 0.06720017513374074158 ) ) ;
#77247 = CARTESIAN_POINT ( 'NONE',  ( 3.029421956395737858, -1.472182739719897215, -1.623467934892895759 ) ) ;
#77248 = ORIENTED_EDGE ( 'NONE', *, *, #62637, .T. ) ;
#77250 = CARTESIAN_POINT ( 'NONE',  ( 9.589694723567584234, 10.08239868711733855, -0.7998128361456281477 ) ) ;
#77249 = CARTESIAN_POINT ( 'NONE',  ( 0.5198770262540284293, 1.941052373433370448, -0.2841105942011297736 ) ) ;
#77251 = VECTOR ( 'NONE', #6826, 1000.000000000000000 ) ;
#77252 = CARTESIAN_POINT ( 'NONE',  ( 4.710494965788769584, 1.834319554003289721, 0.5521488281355608763 ) ) ;
#77253 = PRESENTATION_LAYER_ASSIGNMENT (  '', '', ( #143015 ) ) ;
#77254 = FACE_OUTER_BOUND ( 'NONE', #86044, .T. ) ;
#77255 = CARTESIAN_POINT ( 'NONE',  ( -5.865985541149716376, 7.193105608424513520, 1.152625159504708119 ) ) ;
#77256 = EDGE_CURVE ( 'NONE', #160913, #149147, #191038, .T. ) ;
#77257 = CARTESIAN_POINT ( 'NONE',  ( -10.48884024596653397, 1.000000000000000888, 5.608780650328914597 ) ) ;
#77258 = CARTESIAN_POINT ( 'NONE',  ( 1.364683531249986537, 1.155208333674754728, -0.7879004041258239610 ) ) ;
#77260 = VERTEX_POINT ( 'NONE', #62772 ) ;
#77259 = CARTESIAN_POINT ( 'NONE',  ( 5.721177635286841756, 6.737423998331861341, -1.082531754730543083 ) ) ;
#77261 = CARTESIAN_POINT ( 'NONE',  ( -7.524412065904404479, 11.72230514362308185, 0.000000000000000000 ) ) ;
#77262 = CARTESIAN_POINT ( 'NONE',  ( 1.446389902895691693, 2.159248346720197276, 0.1057134262518744372 ) ) ;
#77263 = EDGE_CURVE ( 'NONE', #119686, #201094, #210082, .T. ) ;
#77264 = CARTESIAN_POINT ( 'NONE',  ( -2.986538976760251263, 6.706322249520737522, -0.7998128361456481317 ) ) ;
#77265 = CARTESIAN_POINT ( 'NONE',  ( 6.780486220610169035, 9.003929572168926754, -1.443375672974078761 ) ) ;
#77266 = CARTESIAN_POINT ( 'NONE',  ( -4.274898507010545856, 3.881803101134051470, -0.7998128361456221525 ) ) ;
#77267 = CARTESIAN_POINT ( 'NONE',  ( 5.034128509002383289, 0.9373949799435165042, -1.566401400633938179 ) ) ;
#77268 = CIRCLE ( 'NONE', #11555, 0.08000000000000020983 ) ;
#77269 = CARTESIAN_POINT ( 'NONE',  ( 11.70309665408334254, 6.967153772763111874, -4.128557813934621734 ) ) ;
#77270 = CARTESIAN_POINT ( 'NONE',  ( 1.440630571055816489, 0.3805203625029949799, 1.934124978983255527 ) ) ;
#77271 = CARTESIAN_POINT ( 'NONE',  ( 3.638835171272115421, 1.817485770107383436, 0.5952672491930725007 ) ) ;
#77272 = B_SPLINE_CURVE_WITH_KNOTS ( 'NONE', 3,
 ( #5214, #71289, #203419, #104905 ),
 .UNSPECIFIED., .F., .F.,
 ( 4, 4 ),
 ( 3.951020751517320303E-17, 0.0001635767864326787382 ),
 .UNSPECIFIED. ) ;
#77273 = ORIENTED_EDGE ( 'NONE', *, *, #73755, .T. ) ;
#77274 = CARTESIAN_POINT ( 'NONE',  ( 3.859776292547572929, -0.5741801112500494186, 1.883974994742370068 ) ) ;
#77275 = ORIENTED_EDGE ( 'NONE', *, *, #1086, .F. ) ;
#77276 = CARTESIAN_POINT ( 'NONE',  ( 5.478056170419292492, -1.895640208600479326, -0.4214399443674861079 ) ) ;
#77277 = ORIENTED_EDGE ( 'NONE', *, *, #24605, .T. ) ;
#77278 = CARTESIAN_POINT ( 'NONE',  ( -7.598418745816086783, 7.829519723065708092, 0.000000000000000000 ) ) ;
#77280 = CARTESIAN_POINT ( 'NONE',  ( 5.871359616481898414, -1.819694913365289768, -1.088597390283413402 ) ) ;
#77279 = CARTESIAN_POINT ( 'NONE',  ( -6.283277845290492714, 6.295188672452495915, -0.7998128361456362523 ) ) ;
#77281 = CARTESIAN_POINT ( 'NONE',  ( 6.116136693096175136, 9.189224337703940648, -1.082531754730548412 ) ) ;
#77283 = ORIENTED_EDGE ( 'NONE', *, *, #39803, .T. ) ;
#77282 = CARTESIAN_POINT ( 'NONE',  ( 4.441997247558228779, -1.179148908705367482, -1.505365500079666852 ) ) ;
#77284 = CARTESIAN_POINT ( 'NONE',  ( 4.477916600690244664, 7.270601638097409669, -1.256879854437189969 ) ) ;
#77285 = CARTESIAN_POINT ( 'NONE',  ( -2.314109536355652530, 5.457892750589173225, -0.8025987720412944837 ) ) ;
#77286 = LINE ( 'NONE', #209395, #43454 ) ;
#77287 = DIRECTION ( 'NONE',  ( 3.330669073875478989E-16, -3.540251991789410786E-16, -1.000000000000000000 ) ) ;
#77288 = PRODUCT_RELATED_PRODUCT_CATEGORY ( 'part', '', ( #176864 ) ) ;
#77289 = CARTESIAN_POINT ( 'NONE',  ( 5.672526239869847053, 0.8180066501249063649, 1.839585422649665958 ) ) ;
#77290 = DIRECTION ( 'NONE',  ( -0.8271092603132983445, -0.5620411653108593475, 3.452101583626667318E-12 ) ) ;
#77291 = CARTESIAN_POINT ( 'NONE',  ( 6.639283661800273961, -1.628176093627232479, 0.8261057939347238310 ) ) ;
#77292 = CARTESIAN_POINT ( 'NONE',  ( 1.820844063133007396, -1.465591517063178806, 1.462601037713284535 ) ) ;
#77293 = CARTESIAN_POINT ( 'NONE',  ( -9.015808963407680565, 9.620791333504852716, 1.040834085586084257E-14 ) ) ;
#77294 = CARTESIAN_POINT ( 'NONE',  ( -6.348239482750515528, 6.857177101084271698, -0.6483580952693357435 ) ) ;
#77295 = CARTESIAN_POINT ( 'NONE',  ( -3.188928480291426837, 8.980740528189164351, -2.451733079074508659 ) ) ;
#77296 = CARTESIAN_POINT ( 'NONE',  ( 6.280143113937574739, -0.9989825818290422044, 1.581392243879369053 ) ) ;
#77297 = CARTESIAN_POINT ( 'NONE',  ( 6.094553744542824170, 7.069066442510145265, 1.199719254218462483 ) ) ;
#77298 = CARTESIAN_POINT ( 'NONE',  ( -0.08000000000000714873, -6.134628647623513231, 10.99970695577494872 ) ) ;
#77299 = CARTESIAN_POINT ( 'NONE',  ( 5.234856708652227297, 7.200695141551334721, 1.443375672974065660 ) ) ;
#77300 = CARTESIAN_POINT ( 'NONE',  ( -2.428612866367529932E-14, 2.999999999999999112, 2.420000000000000373 ) ) ;
#77301 = CARTESIAN_POINT ( 'NONE',  ( 1.364683531249996529, 11.27604166700806410, 0.7879004041258405033 ) ) ;
#77302 = CARTESIAN_POINT ( 'NONE',  ( -4.355193658487827690, 6.104145239700998538, -1.599625672291256295 ) ) ;
#77304 = CARTESIAN_POINT ( 'NONE',  ( -6.149505192250180663, 9.332117270003974951, -1.199719254218452047 ) ) ;
#77303 = CARTESIAN_POINT ( 'NONE',  ( -11.94980361723156292, 11.00238056585436119, -1.099999926404080064 ) ) ;
#77305 = CARTESIAN_POINT ( 'NONE',  ( 3.885211248783075888, -0.5490618756427265712, -1.644986201639383028 ) ) ;
#77306 = CARTESIAN_POINT ( 'NONE',  ( -3.906720819032141190, 7.709591388846142479, -0.7998128361456281477 ) ) ;
#77307 = CARTESIAN_POINT ( 'NONE',  ( 1.305626334525695986, -1.629615561912756805, -1.276682400165381148 ) ) ;
#77308 = CARTESIAN_POINT ( 'NONE',  ( 2.935286906334752199, -1.732537268552689635, -1.216715599779298884 ) ) ;
#77309 = CARTESIAN_POINT ( 'NONE',  ( 8.535021395002688749, 9.916278701380017324, 1.199719254218462483 ) ) ;
#77310 = CARTESIAN_POINT ( 'NONE',  ( 0.01975730027497306709, 6.477791580114294234, 3.085592232244173339 ) ) ;
#77311 = CARTESIAN_POINT ( 'NONE',  ( 6.912946559606852226, -1.604190412254998810, 1.308348183162249434 ) ) ;
#77312 = CARTESIAN_POINT ( 'NONE',  ( 5.026094266273638311, 6.779731885415203330, 1.422988838494985364 ) ) ;
#77313 = CARTESIAN_POINT ( 'NONE',  ( 3.551873057100274789, 7.087676300018221021, 0.7216878364870298324 ) ) ;
#77315 = CARTESIAN_POINT ( 'NONE',  ( 0.1231139863388103495, 1.664874722635242277, 0.9407772870168448209 ) ) ;
#77314 = CARTESIAN_POINT ( 'NONE',  ( -3.474999999999998312, -2.420833333333334725, 2.006292185433951047 ) ) ;
#77316 = CARTESIAN_POINT ( 'NONE',  ( 4.031398662939575495, -1.579512745870830237, -1.661420017294244156 ) ) ;
#77317 = CARTESIAN_POINT ( 'NONE',  ( 0.1877650043593872553, -0.8638833939697135866, 1.608357707688967242 ) ) ;
#77318 = CARTESIAN_POINT ( 'NONE',  ( 3.709155072767254868, 1.612916391665040416, -1.027221078234448859 ) ) ;
#77319 = CARTESIAN_POINT ( 'NONE',  ( 7.028976294042106332, 7.165170195996068969, 0.000000000000000000 ) ) ;
#77320 = CARTESIAN_POINT ( 'NONE',  ( 7.266807146800403849, 7.580289214129690478, 1.040834085586084257E-14 ) ) ;
#77321 = CARTESIAN_POINT ( 'NONE',  ( -7.621654909176601045, 12.04368116068139472, 0.7998128361456481317 ) ) ;
#77322 = CARTESIAN_POINT ( 'NONE',  ( 2.004154220962415689, -0.8570942286123193199, 1.821751609655430260 ) ) ;
#77323 = CARTESIAN_POINT ( 'NONE',  ( 1.815213341579174688, -1.679845371888911698, -1.013028538569618719 ) ) ;
#77324 = CARTESIAN_POINT ( 'NONE',  ( -7.635213062790267458, 12.05949900656400686, 0.000000000000000000 ) ) ;
#77325 = CARTESIAN_POINT ( 'NONE',  ( -6.413170354464012846, 7.440785820751486312, 1.199719254218450271 ) ) ;
#77326 = CARTESIAN_POINT ( 'NONE',  ( 9.579665964948885559, 7.849261790823902629, 0.07999999999999847511 ) ) ;
#77328 = CARTESIAN_POINT ( 'NONE',  ( 3.449836819150660538, 1.770032027316788437, 0.0008499603425977939660 ) ) ;
#77327 = CARTESIAN_POINT ( 'NONE',  ( 4.910148475136437263, 1.442109633637311372, -1.513870239069979196 ) ) ;
#77329 = CARTESIAN_POINT ( 'NONE',  ( -11.48243876534946217, 13.79999999999998295, 3.199999999999997957 ) ) ;
#77330 = EDGE_CURVE ( 'NONE', #82462, #90832, #109124, .T. ) ;
#77331 = CARTESIAN_POINT ( 'NONE',  ( 6.263675073536269622, 1.173004239817846850, 1.969288764181243989 ) ) ;
#77332 = CARTESIAN_POINT ( 'NONE',  ( 5.033026810027643627, -1.234204449110408053, -1.227257546430237989 ) ) ;
#77333 = CARTESIAN_POINT ( 'NONE',  ( 7.076466111328892694, 10.34329533227067799, -1.199719254218441611 ) ) ;
#77334 = CARTESIAN_POINT ( 'NONE',  ( -0.1104750535120251481, 6.947232870375212421, -2.698533382536407732 ) ) ;
#77335 = CARTESIAN_POINT ( 'NONE',  ( 4.639819690880945480, -0.0003889188416681537710, -1.734034292319245552 ) ) ;
#77336 = CARTESIAN_POINT ( 'NONE',  ( 5.441899255841128102, 1.454089660041712140, 1.612519925251713060 ) ) ;
#77337 = LINE ( 'NONE', #106693, #182976 ) ;
#77338 = CARTESIAN_POINT ( 'NONE',  ( 6.315638730379727228, -1.320822524126588515, -1.523799118890494020 ) ) ;
#77339 = CARTESIAN_POINT ( 'NONE',  ( 5.500000000000004441, -3.262149103155007084E-13, -2.052068128417942283 ) ) ;
#77340 = TOROIDAL_SURFACE ( 'NONE', #198391, 1.052419468952678239, 0.9475805310473219834 ) ;
#77341 = CARTESIAN_POINT ( 'NONE',  ( 11.04986239659823433, 9.990607685143002570, -1.056426191432995765 ) ) ;
#77342 = CARTESIAN_POINT ( 'NONE',  ( 3.364200941815390866, 0.8650686769993837233, 1.721291803412771992 ) ) ;
#77343 = CARTESIAN_POINT ( 'NONE',  ( -1.500000000000008216, 11.03125000068279427, 3.469446951953614189E-15 ) ) ;
#77344 = CARTESIAN_POINT ( 'NONE',  ( 6.468989383178811892, -1.718075365336281246, 1.407709432230166202 ) ) ;
#77345 = ORIENTED_EDGE ( 'NONE', *, *, #70182, .T. ) ;
#77346 = CARTESIAN_POINT ( 'NONE',  ( -0.1411974294642228400, 2.034035580701949897, -2.316051970441324936 ) ) ;
#77347 = CARTESIAN_POINT ( 'NONE',  ( 1.499999999999989120, 2.754166666666688190, 0.8660254037844524744 ) ) ;
#77348 = CARTESIAN_POINT ( 'NONE',  ( 4.852928918687680948, 7.749168607522574526, 1.199719254218462483 ) ) ;
#77349 = CARTESIAN_POINT ( 'NONE',  ( 2.368119171756615238, 0.5893650439614643854, -2.141638343492527685 ) ) ;
#77350 = DIRECTION ( 'NONE',  ( -2.345077562848782505E-16, 0.000000000000000000, -1.000000000000000000 ) ) ;
#77351 = CARTESIAN_POINT ( 'NONE',  ( 7.700668062882064291, 10.00719871149432549, -1.443375672974057666 ) ) ;
#77352 = ADVANCED_FACE ( 'NONE', ( #80092 ), #125436, .T. ) ;
#77353 = DIRECTION ( 'NONE',  ( 0.000000000000000000, -1.000000000000000000, 0.000000000000000000 ) ) ;
#77354 = CARTESIAN_POINT ( 'NONE',  ( 3.230585741806197841, 6.991043475407723307, 0.7998128361456271485 ) ) ;
#77355 = CARTESIAN_POINT ( 'NONE',  ( 0.1939827082095749167, 1.755770691208278889, 0.9913967135185000057 ) ) ;
#77357 = CARTESIAN_POINT ( 'NONE',  ( 5.793442459296725744, -1.866233137118753715, 0.8787832743982221251 ) ) ;
#77356 = CARTESIAN_POINT ( 'NONE',  ( 10.06423010004587759, 10.63602329300870153, 0.000000000000000000 ) ) ;
#77358 = CARTESIAN_POINT ( 'NONE',  ( 11.48243876534946217, 9.719999999999982876, 3.199999999999997957 ) ) ;
#77359 = DIRECTION ( 'NONE',  ( 0.000000000000000000, 1.000000000000000000, 0.000000000000000000 ) ) ;
#77360 = SURFACE_SIDE_STYLE ('',( #159679 ) ) ;
#77361 = CARTESIAN_POINT ( 'NONE',  ( 0.6823417656249899377, 0.8427083336747520637, 1.181850606188755259 ) ) ;
#77362 = CARTESIAN_POINT ( 'NONE',  ( 0.5437790142346760058, 1.764394620056912055, 0.1386062191098563767 ) ) ;
#77363 = CARTESIAN_POINT ( 'NONE',  ( 6.240799290569317925, 1.728800370330787928, -0.1372766232172056844 ) ) ;
#77364 = CARTESIAN_POINT ( 'NONE',  ( 5.601031023413125531, -0.4148525734360584138, 1.690157204064596019 ) ) ;
#77365 = CARTESIAN_POINT ( 'NONE',  ( 2.577988946098773049, -1.175687941515238588, 1.967785589457039741 ) ) ;
#77366 = CARTESIAN_POINT ( 'NONE',  ( 0.6823417656249864960, -0.8239583329919114574, -1.181850606188749264 ) ) ;
#77367 = CARTESIAN_POINT ( 'NONE',  ( 2.431387202150552707, 0.8680758514147070004, -1.623638265414374171 ) ) ;
#77368 = CARTESIAN_POINT ( 'NONE',  ( 8.398386088661320414, 11.88553530582519357, -1.199719254218446718 ) ) ;
#77369 =( LENGTH_UNIT ( ) NAMED_UNIT ( * ) SI_UNIT ( .MILLI., .METRE. ) );
#77370 = CARTESIAN_POINT ( 'NONE',  ( 2.467563089314188662, 1.790814366166630034, -0.3536809140580049471 ) ) ;
#77371 = CARTESIAN_POINT ( 'NONE',  ( -4.256897044566581911, 4.068727428190179296, 1.214306433183764966E-14 ) ) ;
#77372 = CARTESIAN_POINT ( 'NONE',  ( -11.43204722947019825, 12.44407245973826193, -3.649275849833183649 ) ) ;
#77373 = CARTESIAN_POINT ( 'NONE',  ( 4.594815077023072902, -0.4589311638903668111, -2.055181093106945855 ) ) ;
#77374 = CARTESIAN_POINT ( 'NONE',  ( -6.575868197828002693, 7.630599971342813426, 1.199719254218450271 ) ) ;
#77375 = CARTESIAN_POINT ( 'NONE',  ( 8.210650312929315575, 13.38009969560112999, 8.580131456927484024 ) ) ;
#77376 = CARTESIAN_POINT ( 'NONE',  ( 2.031770498437397876, 1.981864486777328294, -0.5989037013024376410 ) ) ;
#77377 = CARTESIAN_POINT ( 'NONE',  ( 5.352771719296971042, 5.139321848801576387, 0.7998128361456341429 ) ) ;
#77378 = CARTESIAN_POINT ( 'NONE',  ( -1.360316468750042862, 0.9010416670080622081, -0.7853790794159041244 ) ) ;
#77379 = CARTESIAN_POINT ( 'NONE',  ( 4.530007735025624704, -2.079396993832134388, 0.4145621898983055109 ) ) ;
#77380 = CARTESIAN_POINT ( 'NONE',  ( 0.06489154195065281738, -1.720053269671377949, -0.8678208687467499072 ) ) ;
#77381 = VERTEX_POINT ( 'NONE', #30293 ) ;
#77382 = CARTESIAN_POINT ( 'NONE',  ( -3.980200614063634568, 6.801261928786307642, 1.199719254218452935 ) ) ;
#77383 = CARTESIAN_POINT ( 'NONE',  ( 7.736899214892750010, 12.17813285068358020, 1.040834085586084257E-14 ) ) ;
#77384 = CARTESIAN_POINT ( 'NONE',  ( 6.685579144870162693, 6.972466221869550118, -0.7216878364870458196 ) ) ;
#77385 = CARTESIAN_POINT ( 'NONE',  ( -3.474999999999998312, -1.327083332377416713, 2.006292185433951047 ) ) ;
#77386 = CARTESIAN_POINT ( 'NONE',  ( -5.066996723205291708, 6.934582148538044777, 1.599625672291267398 ) ) ;
#77387 = CARTESIAN_POINT ( 'NONE',  ( -0.01689291694152022724, -1.444339507245323118, 1.687895485215410885 ) ) ;
#77388 = CARTESIAN_POINT ( 'NONE',  ( 1.624194961551369776, -1.169474557214383870, -1.751182684644275289 ) ) ;
#77389 = CARTESIAN_POINT ( 'NONE',  ( -5.978219388983010418, 5.939287140093762574, -0.7998128361456362523 ) ) ;
#77390 = CARTESIAN_POINT ( 'NONE',  ( 9.185812768458653466, 10.67553530374532045, 1.199719254218453823 ) ) ;
#77391 = CARTESIAN_POINT ( 'NONE',  ( 5.840631046605349042, -1.815184518647503742, -0.4092948386957768747 ) ) ;
#77392 = CARTESIAN_POINT ( 'NONE',  ( 8.274553823041976841, 8.548067636504127265, 1.040834085586084257E-14 ) ) ;
#77393 = CARTESIAN_POINT ( 'NONE',  ( 0.5773502691896192918, -2.500000000000002220, 1.000000000000004441 ) ) ;
#77394 = EDGE_LOOP ( 'NONE', ( #19843, #195250 ) ) ;
#77395 = CARTESIAN_POINT ( 'NONE',  ( -5.646044625448194410, 5.551749915969804938, 0.000000000000000000 ) ) ;
#77396 = CARTESIAN_POINT ( 'NONE',  ( -9.544576954340667996, 11.19805653722800365, 1.082531754730558626 ) ) ;
#77397 = CARTESIAN_POINT ( 'NONE',  ( -0.1225938595818750754, -1.897163925677572305, -0.9476133185889324961 ) ) ;
#77398 = CARTESIAN_POINT ( 'NONE',  ( 0.6685859206620029527, -4.211945764156018512, 0.8419752161881538521 ) ) ;
#77400 = CARTESIAN_POINT ( 'NONE',  ( 2.717183929654675811, -1.705535211757349456, -0.9694657131227711888 ) ) ;
#77399 = CARTESIAN_POINT ( 'NONE',  ( 0.6801582343749831283, 2.755208333674742605, 1.178068619123796568 ) ) ;
#77401 = CARTESIAN_POINT ( 'NONE',  ( 0.8487565004985967443, 0.6285140637429244004, 2.068326486519965979 ) ) ;
#77403 = CARTESIAN_POINT ( 'NONE',  ( -5.816164686850935794, 6.201415483580719368, 0.9813818067917270405 ) ) ;
#77402 = CARTESIAN_POINT ( 'NONE',  ( -5.478376588373717659, 8.549133898814758936, -1.199719254218452047 ) ) ;
#77404 = CARTESIAN_POINT ( 'NONE',  ( -1.364683531250000748, 2.009375000341421913, 1.214306433183764966E-14 ) ) ;
#77405 = CARTESIAN_POINT ( 'NONE',  ( 3.092811855500672280, 0.9656183884470933565, -1.439801824928796048 ) ) ;
#77406 = CARTESIAN_POINT ( 'NONE',  ( 1.956607802488403269, 0.2990611944714368642, -1.714256857270479051 ) ) ;
#77407 = CARTESIAN_POINT ( 'NONE',  ( 7.158341918335438869, 7.453746447587225710, -0.7216878364870257245 ) ) ;
#77408 = CARTESIAN_POINT ( 'NONE',  ( -11.19364298753552411, 5.612864353363596237, -3.868560769348357464 ) ) ;
#77409 = EDGE_CURVE ( 'NONE', #53793, #209728, #214309, .T. ) ;
#77410 = CARTESIAN_POINT ( 'NONE',  ( 2.407577179044288584, 0.4389615990625857500, 1.967586618684707522 ) ) ;
#77411 = CARTESIAN_POINT ( 'NONE',  ( 6.825078400183552496, 6.035069422732725286, 2.639236294420511442 ) ) ;
#77413 = COLOUR_RGB ( '', 0.31764706, 0.68627451, 0.89019608) ;
#77412 = CARTESIAN_POINT ( 'NONE',  ( -3.447516199624892419, 7.244129009529488350, 0.7998128361456352531 ) ) ;
#77414 = CARTESIAN_POINT ( 'NONE',  ( 1.727351915365995083, -1.857048012799527248, 0.6622322079550806428 ) ) ;
#77415 = AXIS2_PLACEMENT_3D ( 'NONE', #37145, #169286, #53398 ) ;
#77417 = CARTESIAN_POINT ( 'NONE',  ( -6.780486220610195680, 7.083191143566240910, -0.7216878364870338292 ) ) ;
#77416 = CARTESIAN_POINT ( 'NONE',  ( 5.238497809344139000, 1.134185964801931679, -1.539638564045166857 ) ) ;
#77418 = CARTESIAN_POINT ( 'NONE',  ( -6.089020385868867180, 7.236850217336030511, -1.082531754730549967 ) ) ;
#77419 = CARTESIAN_POINT ( 'NONE',  ( 7.225569521440261767, 7.394528961293920233, -0.7998128361456341429 ) ) ;
#77420 = CARTESIAN_POINT ( 'NONE',  ( -6.903036488013351679, 8.082572653217566128, -1.199719254218452047 ) ) ;
#77421 = CARTESIAN_POINT ( 'NONE',  ( 1.014326189163064607, -2.019862491587170350, 0.002270882547714125031 ) ) ;
#77422 = CARTESIAN_POINT ( 'NONE',  ( -0.4500000000000382583, 3.999999999999934275, 0.9353126743250876896 ) ) ;
#77423 = CARTESIAN_POINT ( 'NONE',  ( 5.544061457994609476, 0.9416624597364110505, -2.106895457712253616 ) ) ;
#77424 = CARTESIAN_POINT ( 'NONE',  ( 6.057081135787192316, 1.604708697955498087, -1.128374156723031430 ) ) ;
#77425 = CARTESIAN_POINT ( 'NONE',  ( 3.432423435979839343, -1.172226468724973936, 1.572839002276872566 ) ) ;
#77426 = CARTESIAN_POINT ( 'NONE',  ( 8.718056468787178659, 10.12981962079525289, 1.199719254218462483 ) ) ;
#77427 = CARTESIAN_POINT ( 'NONE',  ( 0.2467204944939948852, 1.994070950632735428, -0.2986300710981006357 ) ) ;
#77428 = ORIENTED_EDGE ( 'NONE', *, *, #23742, .F. ) ;
#77429 = CARTESIAN_POINT ( 'NONE',  ( 1.182980447155062453, 1.727502145113229970, -1.224025170244628757 ) ) ;
#77431 = CARTESIAN_POINT ( 'NONE',  ( -6.645467848992654858, 10.90479625713344625, 0.7998128361456481317 ) ) ;
#77430 = CARTESIAN_POINT ( 'NONE',  ( -2.950870989268691957, 6.594433254122103349, -0.7998128361456281477 ) ) ;
#77432 = CARTESIAN_POINT ( 'NONE',  ( 2.044624030687072214, -1.478315374303545093, -1.097237131862264903 ) ) ;
#77433 = EDGE_LOOP ( 'NONE', ( #115908, #154526, #62329, #65730 ) ) ;
#77434 = CARTESIAN_POINT ( 'NONE',  ( 11.95224097337929337, 7.720691929998547920, -1.091235320809971210 ) ) ;
#77435 = CARTESIAN_POINT ( 'NONE',  ( 3.252298345715322281, 0.9499829135306799843, -1.895951488860507128 ) ) ;
#77436 = CARTESIAN_POINT ( 'NONE',  ( 1.499999999999987121, 4.077083334016147198, -0.8660254037844323793 ) ) ;
#77437 = CARTESIAN_POINT ( 'NONE',  ( 6.642605195691581699, 9.837124264027149678, 1.199719254218462483 ) ) ;
#77438 = CARTESIAN_POINT ( 'NONE',  ( -1.162044386198238935E-15, 2.625000000682799151, 1.224999999999985656 ) ) ;
#77439 = CARTESIAN_POINT ( 'NONE',  ( 2.671226777604285729, 0.1043416919609811144, -2.058284026376159925 ) ) ;
#77441 = FACE_OUTER_BOUND ( 'NONE', #109097, .T. ) ;
#77440 = CARTESIAN_POINT ( 'NONE',  ( -7.178152263431422320, 10.46192917639026554, 1.199719254218453823 ) ) ;
#77442 = CARTESIAN_POINT ( 'NONE',  ( 0.6823417656249899377, 4.426041667008086655, -1.181850606188754593 ) ) ;
#77443 = CARTESIAN_POINT ( 'NONE',  ( -0.02244404828160086532, 2.859736408857795009, -2.677210243787793598 ) ) ;
#77444 = CARTESIAN_POINT ( 'NONE',  ( -5.346851039111044201, 6.199209027673978412, 7.500000000000000000 ) ) ;
#77445 = CARTESIAN_POINT ( 'NONE',  ( 0.2763675079364875664, 1.274320874971252460, 1.801605125401319007 ) ) ;
#77446 = CARTESIAN_POINT ( 'NONE',  ( 2.653932422735814978, 0.6056841677779849498, -2.179737047031413244 ) ) ;
#77447 = CARTESIAN_POINT ( 'NONE',  ( -9.707274797704657843, 11.38787068781932987, 1.082531754730558626 ) ) ;
#77448 = CARTESIAN_POINT ( 'NONE',  ( 3.023486134662889402, -0.3489238238089559241, 1.777470660238470224 ) ) ;
#77449 = EDGE_CURVE ( 'NONE', #52465, #121123, #34241, .T. ) ;
#77450 = CARTESIAN_POINT ( 'NONE',  ( 3.520622370129117940, 0.2863239327370070697, 1.894091974173327531 ) ) ;
#77451 = CARTESIAN_POINT ( 'NONE',  ( 3.736834853878097107, -1.994506513866915576, -0.5549897870569252545 ) ) ;
#77452 = CARTESIAN_POINT ( 'NONE',  ( -1.201851678989727383E-14, 2.884375000341418804, 1.575800808251672791 ) ) ;
#77453 = CARTESIAN_POINT ( 'NONE',  ( 1.780087957478289074, -1.056366978776434484, 1.664393130878606852 ) ) ;
#77454 = CARTESIAN_POINT ( 'NONE',  ( 6.305299685587768543, 1.603216850002240124, 1.067941234924398852 ) ) ;
#77455 = CARTESIAN_POINT ( 'NONE',  ( 3.221420234344949840, -1.803205065257794004, 0.4975683872451354683 ) ) ;
#77457 = CARTESIAN_POINT ( 'NONE',  ( 4.648548116941726427, 8.423941524322412278, -0.4686463081053967583 ) ) ;
#77456 = CARTESIAN_POINT ( 'NONE',  ( 2.614278096488438674, -2.282406316997650286, 0.3399710349294912115 ) ) ;
#77458 = CARTESIAN_POINT ( 'NONE',  ( 2.506119797010537997, 1.860588423725167306, 0.04906839929019050223 ) ) ;
#77459 = CARTESIAN_POINT ( 'NONE',  ( -1.364683531249997417, 3.009375000341422801, 1.214306433183764966E-14 ) ) ;
#77460 = CARTESIAN_POINT ( 'NONE',  ( 6.496538660071067284, 2.039668932145132008, 0.3065683105917779705 ) ) ;
#77461 = CARTESIAN_POINT ( 'NONE',  ( -4.761938266897808525, 6.578680616179308771, 1.599625672291267398 ) ) ;
#77462 = CARTESIAN_POINT ( 'NONE',  ( 6.205881626753210867, 8.263281202677319470, 1.599625672291281386 ) ) ;
#77463 = CARTESIAN_POINT ( 'NONE',  ( -1.378881877344243723, 4.087185210397143109, 0.5904953584335904671 ) ) ;
#77464 = CARTESIAN_POINT ( 'NONE',  ( 0.08283480907551789285, -2.043431366640800384, -0.5094137356045270737 ) ) ;
#77465 = CARTESIAN_POINT ( 'NONE',  ( -1.364683531250012516, 3.592708333674750509, 0.7879004041258379498 ) ) ;
#77466 = CARTESIAN_POINT ( 'NONE',  ( 5.800121417639972243, -2.161773191644947634, -0.006422599366645573467 ) ) ;
#77467 = CARTESIAN_POINT ( 'NONE',  ( 6.604167511870285168, -0.8622997358492515696, 1.824817093501039267 ) ) ;
#77468 = CARTESIAN_POINT ( 'NONE',  ( -1.364683531250014514, -0.4697916663252449943, 0.7879004041258379498 ) ) ;
#77469 = CARTESIAN_POINT ( 'NONE',  ( -4.500943810056945438, 5.313817868896925312, 1.082531754730560403 ) ) ;
#77470 = EDGE_CURVE ( 'NONE', #152468, #174627, #97437, .T. ) ;
#77473 = CARTESIAN_POINT ( 'NONE',  ( 4.365362273920238678, 7.076377838673507448, 1.082531754730558626 ) ) ;
#77472 = CARTESIAN_POINT ( 'NONE',  ( -1.642778471875000035, -0.5177083328553738761, -2.845375778867859751 ) ) ;
#77471 = CARTESIAN_POINT ( 'NONE',  ( 5.525830126021535449, 8.604496359403894346, -1.199719254218452047 ) ) ;
#77474 = CARTESIAN_POINT ( 'NONE',  ( -0.2104748580754201293, 5.720428293583295520, -2.697747842008205943 ) ) ;
#77475 = CARTESIAN_POINT ( 'NONE',  ( 4.926970384345759513, -1.727065721694167832, 1.040790168839386798 ) ) ;
#77476 = CARTESIAN_POINT ( 'NONE',  ( -8.701635661872465732, 9.046329781806354831, 1.040834085586084257E-14 ) ) ;
#77478 = CARTESIAN_POINT ( 'NONE',  ( -5.926322542504864899, 8.967774495347393682, -1.082531754730549967 ) ) ;
#77477 = CARTESIAN_POINT ( 'NONE',  ( -7.849807752632384172, 12.10193344480572897, 0.000000000000000000 ) ) ;
#77479 = DIRECTION ( 'NONE',  ( -3.330669073875478989E-16, 3.330669073875478989E-16, 1.000000000000000000 ) ) ;
#77481 = CARTESIAN_POINT ( 'NONE',  ( 1.364683531250000748, 9.755208333674737275, -0.7879004041258355073 ) ) ;
#77480 = CARTESIAN_POINT ( 'NONE',  ( 6.385629968321593353, 1.486944277142748572, 1.569300510047972219 ) ) ;
#77482 = DIRECTION ( 'NONE',  ( -0.000000000000000000, 1.000000000000000000, -0.000000000000000000 ) ) ;
#77483 = CARTESIAN_POINT ( 'NONE',  ( -9.215791728987058562, 11.77484298861683598, -1.599625672291263179 ) ) ;
#77485 = CARTESIAN_POINT ( 'NONE',  ( 0.4037314067151754893, -1.025472807287574506, -1.617813098647686632 ) ) ;
#77484 = CARTESIAN_POINT ( 'NONE',  ( -7.009202228140764213, 7.279750142360097875, -0.7216878364870267237 ) ) ;
#77486 = CARTESIAN_POINT ( 'NONE',  ( 0.6823417656249882723, 0.4885416670080827695, -1.181850606188749264 ) ) ;
#77487 = CARTESIAN_POINT ( 'NONE',  ( 11.97929049433705373, 11.37999999999999901, 0.7046979865771783036 ) ) ;
#77488 = CARTESIAN_POINT ( 'NONE',  ( 2.050978400279603875, -1.384275906022333968, -1.028850351009907849 ) ) ;
#77489 = CARTESIAN_POINT ( 'NONE',  ( 3.923105346307896202, 5.670318552149568703, -1.599625672291269396 ) ) ;
#77490 = CARTESIAN_POINT ( 'NONE',  ( 4.857564175446106525, 8.889184981320973122, 0.7998128361456331437 ) ) ;
#77491 = CARTESIAN_POINT ( 'NONE',  ( 4.177814833343409084, 3.976464848429826393, 1.040551764647542070E-14 ) ) ;
#77492 = CARTESIAN_POINT ( 'NONE',  ( 1.317257508235271102, -1.728110672573167639, 0.3808341387830004865 ) ) ;
#77493 = CARTESIAN_POINT ( 'NONE',  ( 1.682290626080079621, 1.036857497476886936, 1.725414394560653042 ) ) ;
#77494 = DIRECTION ( 'NONE',  ( 0.000000000000000000, 1.000000000000000000, 0.000000000000000000 ) ) ;
#77495 = CARTESIAN_POINT ( 'NONE',  ( 4.102700518754747172, -0.6894086160392081108, -2.096397988278507096 ) ) ;
#77496 = CARTESIAN_POINT ( 'NONE',  ( 5.735278773323231327, -0.04571225511484919291, -2.170743740471086980 ) ) ;
#77497 = ORIENTED_EDGE ( 'NONE', *, *, #60250, .F. ) ;
#77498 = CARTESIAN_POINT ( 'NONE',  ( -1.402160292154681736E-14, -0.9124999999999769962, -1.732050807568870754 ) ) ;
#77499 = CARTESIAN_POINT ( 'NONE',  ( 9.042925270190638187, 9.652427024751663254, 0.7216878364870458196 ) ) ;
#77501 = CARTESIAN_POINT ( 'NONE',  ( 3.023064714212614135, -1.777003028299545484, 0.9530295004822467719 ) ) ;
#77500 = CARTESIAN_POINT ( 'NONE',  ( 2.842561206135377994, 1.176089095116246153, -1.764248410475676820 ) ) ;
#77503 = VERTEX_POINT ( 'NONE', #161366 ) ;
#77502 = CARTESIAN_POINT ( 'NONE',  ( 3.164119808340008611, 1.811767227632065325, -0.004774541488360150264 ) ) ;
#77504 = CARTESIAN_POINT ( 'NONE',  ( 5.525830126021535449, 8.604496359403894346, -1.199719254218452047 ) ) ;
#77505 = EDGE_LOOP ( 'NONE', ( #171097, #162671, #166585, #149003 ) ) ;
#77506 = CARTESIAN_POINT ( 'NONE',  ( 0.7252172114964609007, -1.777616610744123804, 0.5828384007960025759 ) ) ;
#77507 = CARTESIAN_POINT ( 'NONE',  ( 5.148345644887269756, 7.029489223833707001, -1.599625672291256295 ) ) ;
#77508 = CARTESIAN_POINT ( 'NONE',  ( 6.516225534515442952, -0.8655890497146904172, -1.607451055071248636 ) ) ;
#77510 = CARTESIAN_POINT ( 'NONE',  ( 1.094790513324794601, 1.691201413147478183, 0.8998118624304138891 ) ) ;
#77509 = CARTESIAN_POINT ( 'NONE',  ( -5.088387723830502196, 4.830873854090670605, -0.7998128361456221525 ) ) ;
#77511 = CARTESIAN_POINT ( 'NONE',  ( -9.348561386899501002, 3.999985931113709814, -7.001914024221969512 ) ) ;
#77512 = EDGE_CURVE ( 'NONE', #167635, #131570, #208356, .T. ) ;
#77513 = CARTESIAN_POINT ( 'NONE',  ( 1.364683531249988757, 1.196875000341421469, 0.000000000000000000 ) ) ;
#77514 = CARTESIAN_POINT ( 'NONE',  ( 6.092610039548504552, 6.029531113932129038, 0.3159152987922431710 ) ) ;
#77515 = CARTESIAN_POINT ( 'NONE',  ( -8.833300774503376473, 10.26427131079744193, 1.199719254218462483 ) ) ;
#77516 = CARTESIAN_POINT ( 'NONE',  ( 5.120075222393803749, -1.153228217640640985, -1.828211184805514700 ) ) ;
#77517 = ADVANCED_FACE ( 'NONE', ( #111605 ), #44820, .T. ) ;
#77518 = CARTESIAN_POINT ( 'NONE',  ( -4.177320726786319049, 6.927272377009067839, -1.082531754730551743 ) ) ;
#77519 = CARTESIAN_POINT ( 'NONE',  ( -7.611976899429754084, 7.845337568948314022, 0.7998128361456341429 ) ) ;
#77520 = CARTESIAN_POINT ( 'NONE',  ( 3.234745892528373634, 1.342314639517484087, -1.641720766639112039 ) ) ;
#77522 = CARTESIAN_POINT ( 'NONE',  ( -10.47476534206535170, 5.237283261923990629, -5.169982392003922733 ) ) ;
#77521 = DIRECTION ( 'NONE',  ( -0.9999655912483514930, 0.000000000000000000, 0.008295560218253852924 ) ) ;
#77523 = CARTESIAN_POINT ( 'NONE',  ( 4.059811131046401123, 1.956822991617146457, -0.2382644796226577599 ) ) ;
#77524 = CARTESIAN_POINT ( 'NONE',  ( 6.416268857797894576, -1.911816439625917852, 0.05404522429636184067 ) ) ;
#77525 = EDGE_LOOP ( 'NONE', ( #45701, #119190, #167210, #64552 ) ) ;
#77526 = CARTESIAN_POINT ( 'NONE',  ( 5.542236361656130761, 0.8606211682868989410, 1.934736125387125361 ) ) ;
#77527 = CARTESIAN_POINT ( 'NONE',  ( 0.8716356842100521085, -0.3054578492302991721, 2.047597563663336118 ) ) ;
#77528 = CARTESIAN_POINT ( 'NONE',  ( 2.273291157499750526, 1.194718917728957885, 1.530869066462538619 ) ) ;
#77529 = VERTEX_POINT ( 'NONE', #16133 ) ;
#77530 = CARTESIAN_POINT ( 'NONE',  ( -2.810282979782591006, 6.500690253046801814, 0.000000000000000000 ) ) ;
#77531 = CARTESIAN_POINT ( 'NONE',  ( 7.212011367826596242, 7.378711115411311638, 0.000000000000000000 ) ) ;
#77533 = CARTESIAN_POINT ( 'NONE',  ( 6.307567778855705853, 8.381915046796901692, -1.599625672291262513 ) ) ;
#77532 = CARTESIAN_POINT ( 'NONE',  ( 3.187526948619547884, -0.8467841439671991433, 1.911654264539459191 ) ) ;
#77534 = CARTESIAN_POINT ( 'NONE',  ( 7.014364370223726830, 9.276787413384745662, -1.599625672291269396 ) ) ;
#77536 = VERTEX_POINT ( 'NONE', #65939 ) ;
#77535 = CARTESIAN_POINT ( 'NONE',  ( 0.1350377444619410283, -0.09094779274463302143, 1.809295058508665566 ) ) ;
#77537 = CARTESIAN_POINT ( 'NONE',  ( 5.777994779145079640, 1.311685685134782231, 1.774619457157788904 ) ) ;
#77538 = CARTESIAN_POINT ( 'NONE',  ( -1.154700538379266339, -2.500000000000002220, 2.602085213965210642E-15 ) ) ;
#77539 = CARTESIAN_POINT ( 'NONE',  ( 3.030518406005321186, 1.227118389542979804, -1.833929004854919276 ) ) ;
#77540 = CARTESIAN_POINT ( 'NONE',  ( 9.108380270282433244, 9.520865158284665952, 1.040834085586084257E-14 ) ) ;
#77541 = LINE ( 'NONE', #174013, #54692 ) ;
#77542 = CARTESIAN_POINT ( 'NONE',  ( 2.191926089937683564, 1.177725938178806997, 1.506473034612793915 ) ) ;
#77543 = CARTESIAN_POINT ( 'NONE',  ( 7.899597058256738968, 12.36794700127490820, 1.040834085586084257E-14 ) ) ;
#77544 = CARTESIAN_POINT ( 'NONE',  ( 5.846161131210033446, -0.9342735719010831774, 1.847668428805064655 ) ) ;
#77546 = CARTESIAN_POINT ( 'NONE',  ( 3.133815226704575796, -1.450665623810345473, -1.602838778681405785 ) ) ;
#77545 = CARTESIAN_POINT ( 'NONE',  ( 0.000000000000000000, 3.956598013261175772, 0.000000000000000000 ) ) ;
#77547 = CARTESIAN_POINT ( 'NONE',  ( 4.880524338131243312, -0.2681524694418158661, -2.175044001020635331 ) ) ;
#77548 = ORIENTED_EDGE ( 'NONE', *, *, #110539, .T. ) ;
#77549 = CARTESIAN_POINT ( 'NONE',  ( -0.02948999725180654480, 0.001137248348246934970, -1.926291057026579434 ) ) ;
#77550 = CARTESIAN_POINT ( 'NONE',  ( -2.679285714285713826, -0.4970443252110337551, -0.5000000000000004441 ) ) ;
#77551 = CARTESIAN_POINT ( 'NONE',  ( -0.9045775026450960654, 15.44695887967888304, 11.95520906865927380 ) ) ;
#77552 = CARTESIAN_POINT ( 'NONE',  ( 3.400062661977048428, 7.188766548940353829, -1.734723475976807094E-15 ) ) ;
#77553 = CARTESIAN_POINT ( 'NONE',  ( -0.6823417656250039265, 15.38020833367473372, -1.181850606188755259 ) ) ;
#77554 = FACE_OUTER_BOUND ( 'NONE', #149723, .T. ) ;
#77556 = CARTESIAN_POINT ( 'NONE',  ( 0.8267963299631932994, 0.8146243292815741333, -1.844710905833810255 ) ) ;
#77555 = AXIS2_PLACEMENT_3D ( 'NONE', #40081, #88841, #159153 ) ;
#77557 = CARTESIAN_POINT ( 'NONE',  ( -9.653042183249972652, 10.36423008998754192, -0.7216878364870267237 ) ) ;
#77558 = CARTESIAN_POINT ( 'NONE',  ( 4.712340909201580885, 7.655425606447271214, -1.199719254218452047 ) ) ;
#77559 = CARTESIAN_POINT ( 'NONE',  ( 6.104363016364067640, 2.067617457866403718, 0.1074407263862015016 ) ) ;
#77560 = CARTESIAN_POINT ( 'NONE',  ( 4.055238279289786973, -1.602352113334176043, -1.069235405101864878 ) ) ;
#77561 = CARTESIAN_POINT ( 'NONE',  ( 6.573823534745116604, -0.9041686956474543901, 1.912245183953432237 ) ) ;
#77562 = CIRCLE ( 'NONE', #191649, 0.08000000000000020983 ) ;
#77563 = CARTESIAN_POINT ( 'NONE',  ( -8.611400122974211868, 13.19838391011195888, 1.040834085586084257E-14 ) ) ;
#77564 = CARTESIAN_POINT ( 'NONE',  ( 3.988069740714122791, 7.804498464141805592, 0.7998128361456321445 ) ) ;
#77565 = CARTESIAN_POINT ( 'NONE',  ( 1.500000000000001332, 13.12499999999999822, 0.000000000000000000 ) ) ;
#77566 = CARTESIAN_POINT ( 'NONE',  ( 3.678522182247864869, 1.252989934047860965, -1.519404455180313640 ) ) ;
#77567 = CARTESIAN_POINT ( 'NONE',  ( 0.5334774086375413393, -1.552487152004313087, -1.546944964277228607 ) ) ;
#77568 = CARTESIAN_POINT ( 'NONE',  ( 3.633261591126951018, -1.686358373764598406, 0.7000054678709469735 ) ) ;
#77569 = CARTESIAN_POINT ( 'NONE',  ( 6.916067756746836714, 8.201738816693689316, -1.082531754730548412 ) ) ;
#77570 = CARTESIAN_POINT ( 'NONE',  ( 4.541618270453549044, 5.361271406026338227, -1.082531754730548412 ) ) ;
#77571 = CARTESIAN_POINT ( 'NONE',  ( -7.117104292530948229, 7.267986194233038155, -0.7998128361456362523 ) ) ;
#77572 = CARTESIAN_POINT ( 'NONE',  ( 6.229045230835819069, 6.231917288922055320, -0.7998128361456481317 ) ) ;
#77573 = ORIENTED_EDGE ( 'NONE', *, *, #184656, .T. ) ;
#77575 = CARTESIAN_POINT ( 'NONE',  ( 4.658451966079163675, 2.008086622728368464, 0.1439865329972197516 ) ) ;
#77574 = CARTESIAN_POINT ( 'NONE',  ( 1.223879446662301307, 1.774596971308094018, 0.4907264878865265634 ) ) ;
#77576 = CARTESIAN_POINT ( 'NONE',  ( 1.159977488309314797, -0.5597072352675269702, -2.229110579909891143 ) ) ;
#77577 = CARTESIAN_POINT ( 'NONE',  ( 5.330891710049517229, -1.845885424482188286, -0.6645199359083459045 ) ) ;
#77578 = CARTESIAN_POINT ( 'NONE',  ( -5.392392409933270514, 7.314210449720692786, 1.599625672291269396 ) ) ;
#77579 = CARTESIAN_POINT ( 'NONE',  ( 6.760415694340460783E-18, 5.633679745283718603E-18, 0.4330127018937082184 ) ) ;
#77580 = CARTESIAN_POINT ( 'NONE',  ( -2.462777459176719308, 6.024990802348131780, -0.7998128361456281477 ) ) ;
#77581 = CARTESIAN_POINT ( 'NONE',  ( 0.3794556558127279988, -0.1030994254981997954, 2.067933115924729837 ) ) ;
#77582 = CARTESIAN_POINT ( 'NONE',  ( -3.949167883330528372, 7.829389307186077396, 1.214306433183764966E-14 ) ) ;
#77584 = CARTESIAN_POINT ( 'NONE',  ( 6.578955313817166584, -0.09182192948648319752, -1.767577901409943086 ) ) ;
#77583 = CARTESIAN_POINT ( 'NONE',  ( 1.364907732811880159, 0.1502005422731657047, -2.085395908040136526 ) ) ;
#77585 = CARTESIAN_POINT ( 'NONE',  ( -0.007473969438217894709, 8.279395425053857949, -1.999986034896452880 ) ) ;
#77586 = CARTESIAN_POINT ( 'NONE',  ( -0.1102773484823885153, 6.947233595868168798, -2.798541112319170576 ) ) ;
#77587 = CARTESIAN_POINT ( 'NONE',  ( 1.592878374036447164, -0.5866614404700842833, 1.638733785964431755 ) ) ;
#77588 = CARTESIAN_POINT ( 'NONE',  ( 4.690231075323689325, 7.559354456931247412, 1.199719254218462483 ) ) ;
#77589 = CARTESIAN_POINT ( 'NONE',  ( -0.6311622855796790166, 3.199999999999973532, -0.4000000000000444311 ) ) ;
#77590 = CARTESIAN_POINT ( 'NONE',  ( 2.103723633838894713, -1.724574586359624906, 0.04069764719066489012 ) ) ;
#77591 = CARTESIAN_POINT ( 'NONE',  ( 1.839652601550560096, 0.8350199954420146620, -2.026445374841173930 ) ) ;
#77592 = CARTESIAN_POINT ( 'NONE',  ( 0.08792998612136559977, -0.4660014661636499578, 1.670295066556278352 ) ) ;
#77593 = CARTESIAN_POINT ( 'NONE',  ( 4.055453297694236348, -1.834216022232620702, -1.226887332174103173 ) ) ;
#77594 = PLANE ( 'NONE',  #140058 ) ;
#77595 = CARTESIAN_POINT ( 'NONE',  ( 2.272564004159416395, -1.020438428401538200, -1.916272530736246926 ) ) ;
#77596 = CARTESIAN_POINT ( 'NONE',  ( 1.611646134362737959, -1.812087876328593916, 0.2219229778191167957 ) ) ;
#77597 = CARTESIAN_POINT ( 'NONE',  ( 2.958335891534333850, -1.257395014299323988, 1.703445231074371291 ) ) ;
#77598 = CARTESIAN_POINT ( 'NONE',  ( 6.539320575229274901, 7.053161517996441532, 2.494893549996656912 ) ) ;
#77599 = ORIENTED_EDGE ( 'NONE', *, *, #90947, .T. ) ;
#77601 = CARTESIAN_POINT ( 'NONE',  ( 1.364683531249988757, 0.9468750003414211358, 0.000000000000000000 ) ) ;
#77600 = CARTESIAN_POINT ( 'NONE',  ( 3.825942575589100780, 1.225831451615842393, -1.936910307245596652 ) ) ;
#77602 = CARTESIAN_POINT ( 'NONE',  ( 4.383363735919856730, 4.008345868194933104, -0.7998128361456211532 ) ) ;
#77603 = CARTESIAN_POINT ( 'NONE',  ( 3.680148631105580215, 6.380924938676771241, -1.199719254218446718 ) ) ;
#77604 = CARTESIAN_POINT ( 'NONE',  ( 5.848318881832833327, 1.097015000334870649, -1.931420017644119635 ) ) ;
#77605 = CARTESIAN_POINT ( 'NONE',  ( -7.727784370109414880, 8.118095974656867497, 0.7216878364870578100 ) ) ;
#77606 = CARTESIAN_POINT ( 'NONE',  ( 3.714570900464269076, 7.277490450609545469, 0.7216878364870298324 ) ) ;
#77607 = CARTESIAN_POINT ( 'NONE',  ( -6.195713011320795438, 8.251417818006149929, -1.443375672974058777 ) ) ;
#77608 =( BOUNDED_CURVE ( )  B_SPLINE_CURVE ( 2, ( #197975, #136209, #34413, #166560, #131963, #214189, #52803, #181719, #18149 ),
 .UNSPECIFIED., .F., .T. ) 
 B_SPLINE_CURVE_WITH_KNOTS ( ( 3, 2, 2, 2, 3 ),
 ( 0.4531250000000001665, 0.4583333333333333148, 0.4687500000000000000, 0.4791666666666666852, 0.4843749999999998335 ),
 .UNSPECIFIED. ) 
 CURVE ( )  GEOMETRIC_REPRESENTATION_ITEM ( )  RATIONAL_B_SPLINE_CURVE ( ( 0.9330127018922194093, 0.9330127018922215187, 1.000000000000000000, 0.8660254037844387076, 1.000000000000000000, 0.8660254037844387076, 1.000000000000000000, 0.9330127018922215187, 0.9330127018922194093 ) ) 
 REPRESENTATION_ITEM ( '' )  );
#77609 = CARTESIAN_POINT ( 'NONE',  ( 0.02191186323000256231, -9.962467934940974601, 10.91967397018795438 ) ) ;
#77610 = CIRCLE ( 'NONE', #184740, 0.8300000000000008482 ) ;
#77611 = VERTEX_POINT ( 'NONE', #198098 ) ;
#77612 = CARTESIAN_POINT ( 'NONE',  ( 4.113907844847329187, 0.1017495355152969322, 2.013985960686740295 ) ) ;
#77614 = CARTESIAN_POINT ( 'NONE',  ( 2.289955638094377299, -1.343889277006144356, -1.564782475634781900 ) ) ;
#77613 = CARTESIAN_POINT ( 'NONE',  ( 5.124091990960999432, 8.065525525174782828, -1.199719254218452047 ) ) ;
#77615 = PLANE ( 'NONE',  #57527 ) ;
#77616 = CARTESIAN_POINT ( 'NONE',  ( 3.567203813726958828, 6.215469311773181182, 1.082531754730549078 ) ) ;
#77617 = CARTESIAN_POINT ( 'NONE',  ( -3.285556943749998737, -3.580208332855374653, 1.896917185911908499 ) ) ;
#77618 = CARTESIAN_POINT ( 'NONE',  ( 0.6823417656249899377, 4.676041667008086655, -1.181850606188754593 ) ) ;
#77619 = CARTESIAN_POINT ( 'NONE',  ( 4.734432829848630675, 0.3728853646711489112, 2.159338447334692823 ) ) ;
#77620 = CARTESIAN_POINT ( 'NONE',  ( 2.584611472894111195, -0.6298744119781033435, 1.915600275669691488 ) ) ;
#77621 = CARTESIAN_POINT ( 'NONE',  ( 2.120424178990498731, 0.001545453418709194504, 1.841430844159386293 ) ) ;
#77622 = CIRCLE ( 'NONE', #63863, 0.07999999999999998779 ) ;
#77623 = CARTESIAN_POINT ( 'NONE',  ( 6.120616281565444794, 9.228137197546649517, -1.199719254218440723 ) ) ;
#77624 = CARTESIAN_POINT ( 'NONE',  ( 6.739283625173963621, -1.628968703954777553, 0.8242606506234579911 ) ) ;
#77625 = CARTESIAN_POINT ( 'NONE',  ( 0.2824055751470951892, 1.906470811695348599, -1.284064767653005257 ) ) ;
#77626 = CARTESIAN_POINT ( 'NONE',  ( -6.028571859570855729, 10.18508426947466816, 0.000000000000000000 ) ) ;
#77628 = CARTESIAN_POINT ( 'NONE',  ( -3.806807270387036368, 7.663301925418665839, 0.000000000000000000 ) ) ;
#77627 = CARTESIAN_POINT ( 'NONE',  ( 5.260715670973223901, -1.642634774727338653, 1.556112085687613611 ) ) ;
#77629 = CARTESIAN_POINT ( 'NONE',  ( 1.770285920821415449, 1.083698108115097591, 1.805711900068427411 ) ) ;
#77630 = CARTESIAN_POINT ( 'NONE',  ( -5.966470118465691641, 9.118576350588734059, -1.199719254218452047 ) ) ;
#77631 = CARTESIAN_POINT ( 'NONE',  ( 8.209625708274705502, 9.536650400197368427, 1.199719254218462483 ) ) ;
#77632 = CARTESIAN_POINT ( 'NONE',  ( 6.495764994278795612, 9.632124022417032805, 1.082531754730549078 ) ) ;
#77633 = CARTESIAN_POINT ( 'NONE',  ( 0.000000000000000000, 0.000000000000000000, 0.000000000000000000 ) ) ;
#77634 = CARTESIAN_POINT ( 'NONE',  ( -7.552055258011950656, 8.769484874890757453, 1.199719254218462483 ) ) ;
#77635 = UNCERTAINTY_MEASURE_WITH_UNIT (LENGTH_MEASURE( 1.000000000000000082E-05 ), #87687, 'distance_accuracy_value', 'NONE');
#77636 = CARTESIAN_POINT ( 'NONE',  ( 6.412643469139427843, 10.42524178073059993, -0.7216878364870267237 ) ) ;
#77637 = CARTESIAN_POINT ( 'NONE',  ( 4.015052158831055706, 7.807088067957844046, 0.2846288760043579336 ) ) ;
#77638 = CARTESIAN_POINT ( 'NONE',  ( -10.00555417720528872, 10.77549408293541866, 0.7216878364870438212 ) ) ;
#77640 = CARTESIAN_POINT ( 'NONE',  ( 2.356001076229676805, -1.649452400593539148, -1.488157709660995920 ) ) ;
#77639 = CARTESIAN_POINT ( 'NONE',  ( 1.705496241919310707, 1.842552997918958768, -1.049655202612943095 ) ) ;
#77641 = CARTESIAN_POINT ( 'NONE',  ( 0.5927436934281338221, -2.190715567557582677, -0.2661302102612560505 ) ) ;
#77642 = CARTESIAN_POINT ( 'NONE',  ( -5.074494633264801990, 9.142270515442742607, 0.7998128361456291469 ) ) ;
#77643 = CARTESIAN_POINT ( 'NONE',  ( 5.066996723205273057, 6.934582148538044777, 1.599625672291267398 ) ) ;
#77644 = CARTESIAN_POINT ( 'NONE',  ( 4.721123852359588646, -1.751549048416237486, -0.8839179009662299080 ) ) ;
#77645 = CARTESIAN_POINT ( 'NONE',  ( 7.553864141108259211, 11.96459193126834464, 1.040834085586084257E-14 ) ) ;
#77646 = CARTESIAN_POINT ( 'NONE',  ( -4.728240158028945928, 6.838416746360681309, 1.235430216343525567 ) ) ;
#77647 = CARTESIAN_POINT ( 'NONE',  ( 4.695201269034174452, 4.372156323494968966, 1.214306433183764966E-14 ) ) ;
#77648 = CARTESIAN_POINT ( 'NONE',  ( -1.402160292154681736E-14, 0.1968750003414221628, -1.575800808251665908 ) ) ;
#77649 = CARTESIAN_POINT ( 'NONE',  ( -3.526529353330350336, 7.128384988945109413, -0.7216878364870458196 ) ) ;
#77651 = ORIENTED_EDGE ( 'NONE', *, *, #34941, .F. ) ;
#77650 = CARTESIAN_POINT ( 'NONE',  ( -5.422898255786186006, 9.270539031818461950, -0.7216878364870207285 ) ) ;
#77652 = CARTESIAN_POINT ( 'NONE',  ( 3.445663904809421307, -1.957918079443463855, 0.8150281543025169606 ) ) ;
#77653 = CARTESIAN_POINT ( 'NONE',  ( -3.772911886352873445, 7.623757310712140800, 0.7998128361456352531 ) ) ;
#77654 = CARTESIAN_POINT ( 'NONE',  ( 4.786082296487640164, -1.021991182799499409, 1.904868704497929333 ) ) ;
#77655 = CARTESIAN_POINT ( 'NONE',  ( 3.913478945735289205, -0.9499487412085620974, -1.577145280185827447 ) ) ;
#77656 = CARTESIAN_POINT ( 'NONE',  ( -4.595282798756362475, 6.958845989550745514, 1.192800718855389297 ) ) ;
#77657 = CARTESIAN_POINT ( 'NONE',  ( -1.364683531250014514, 0.09270833367475767028, 0.7879004041258379498 ) ) ;
#77658 = CARTESIAN_POINT ( 'NONE',  ( 5.314300430047540935, 1.610136290765556977, 0.6609758457527656894 ) ) ;
#77660 = EDGE_CURVE ( 'NONE', #14615, #160452, #17202, .T. ) ;
#77659 = CARTESIAN_POINT ( 'NONE',  ( 1.466069532605751007E-15, 14.48154074412737558, 12.00000000000000178 ) ) ;
#77661 = CARTESIAN_POINT ( 'NONE',  ( 4.365362273920250225, 5.155639410070820716, 1.082531754730560403 ) ) ;
#77662 = CARTESIAN_POINT ( 'NONE',  ( -6.462464340777758665, 6.712165690604718016, -0.3031571887801186027 ) ) ;
#77663 = CARTESIAN_POINT ( 'NONE',  ( 3.520547545725543515, 1.372905562624787024, -1.669742455111824286 ) ) ;
#77664 = ADVANCED_FACE ( 'NONE', ( #183986 ), #119056, .T. ) ;
#77665 = CARTESIAN_POINT ( 'NONE',  ( 5.589220178194088895, 1.203167956798111060, -1.617571559180859486 ) ) ;
#77666 = CARTESIAN_POINT ( 'NONE',  ( -8.636180661780668899, 10.13826086257468795, -1.082531754730543083 ) ) ;
#77667 = CARTESIAN_POINT ( 'NONE',  ( 2.817419395390472037, -0.2130390993498078311, 2.151187356804876050 ) ) ;
#77668 = CARTESIAN_POINT ( 'NONE',  ( 3.585193993258027678, 1.783571249345828003, -0.8399556444593555549 ) ) ;
#77669 = CARTESIAN_POINT ( 'NONE',  ( 0.1170720436180875679, -0.1011795954627830590, 2.189343785608413917 ) ) ;
#77670 = CARTESIAN_POINT ( 'NONE',  ( 4.335450565170337001, 0.8274041267214229389, -1.757107282799404091 ) ) ;
#77673 = ORIENTED_EDGE ( 'NONE', *, *, #67235, .F. ) ;
#77672 = FILL_AREA_STYLE ('',( #164261 ) ) ;
#77671 = CARTESIAN_POINT ( 'NONE',  ( -9.151390499099978371, 9.778969791812544443, 0.7216878364870438212 ) ) ;
#77674 = CARTESIAN_POINT ( 'NONE',  ( -5.257529707049291900, 9.355811434857983500, 0.7998128361456291469 ) ) ;
#77675 = DIRECTION ( 'NONE',  ( 1.000000000000000000, 0.000000000000000000, 0.000000000000000000 ) ) ;
#77677 = ORIENTED_EDGE ( 'NONE', *, *, #192214, .F. ) ;
#77676 = CARTESIAN_POINT ( 'NONE',  ( -4.411198876399886615, 6.239761003923544713, -1.599625672291271394 ) ) ;
#77678 = CARTESIAN_POINT ( 'NONE',  ( -9.137832345486311070, 9.763151945929928743, 1.040834085586084257E-14 ) ) ;
#77679 = CARTESIAN_POINT ( 'NONE',  ( 2.046200460737709559, 0.8445575735530999051, -2.038961412367201298 ) ) ;
#77680 = CARTESIAN_POINT ( 'NONE',  ( 1.642778471875000035, -1.626041666188710044, -2.845375778867859751 ) ) ;
#77681 = CARTESIAN_POINT ( 'NONE',  ( 6.438335799692933570, -1.052282694883142078, 1.655480336553965648 ) ) ;
#77682 = CARTESIAN_POINT ( 'NONE',  ( -1.500000000000008216, 9.000000000000001776, 3.469446951953614189E-15 ) ) ;
#77683 = CARTESIAN_POINT ( 'NONE',  ( 1.499999999999989120, 4.827083334016149863, -0.8660254037844323793 ) ) ;
#77684 = CARTESIAN_POINT ( 'NONE',  ( 6.021928883684827483, 6.074059740061504620, -0.5497475987105825412 ) ) ;
#77686 = CARTESIAN_POINT ( 'NONE',  ( 5.936183876523434932, 1.091049494364674466, -1.918236432931222257 ) ) ;
#77685 = DIRECTION ( 'NONE',  ( -1.000000000000000000, 5.578564026256490882E-16, 2.058387550816952846E-48 ) ) ;
#77687 = CARTESIAN_POINT ( 'NONE',  ( 5.068220161613846031, -1.734768455660203434, -0.6171159064975312303 ) ) ;
#77688 = EDGE_LOOP ( 'NONE', ( #206357, #8990, #141053, #65733 ) ) ;
#77689 = CARTESIAN_POINT ( 'NONE',  ( -0.6801582343750213200, -1.067708332991926135, 1.178068619123832983 ) ) ;
#77690 = CARTESIAN_POINT ( 'NONE',  ( -7.263417608619167076, 9.497073181520933716, -1.599625672291263179 ) ) ;
#77691 = DIRECTION ( 'NONE',  ( -0.000000000000000000, -1.000000000000000000, -0.000000000000000000 ) ) ;
#77692 = CARTESIAN_POINT ( 'NONE',  ( 11.96209379583854293, 11.32792940594236519, 0.9572398070798464609 ) ) ;
#77693 = PLANE ( 'NONE',  #18427 ) ;
#77694 = CARTESIAN_POINT ( 'NONE',  ( 4.904298879841284098, 6.744767997946721216, 1.599625672291267398 ) ) ;
#77695 = CARTESIAN_POINT ( 'NONE',  ( 6.151650338133601181, 0.6026783403972060249, -1.970659962842249424 ) ) ;
#77698 = CARTESIAN_POINT ( 'NONE',  ( 3.702549152423353807, 1.581054339307564449, 0.9433870219286569769 ) ) ;
#77697 = CARTESIAN_POINT ( 'NONE',  ( 2.013881029938934919, 1.856366682828480608, -0.1327402387825328822 ) ) ;
#77696 = CARTESIAN_POINT ( 'NONE',  ( -9.569358774149648639, 4.446947634372959257, 7.167287524840459945 ) ) ;
#77699 = CARTESIAN_POINT ( 'NONE',  ( 7.630541526392844887, 7.796719957080126662, 0.7998128361456341429 ) ) ;
#77700 = CARTESIAN_POINT ( 'NONE',  ( -4.911987184702322651, 4.724253982773818805, 0.4179318588051501027 ) ) ;
#77701 =( BOUNDED_SURFACE ( )  B_SPLINE_SURFACE ( 3, 2, ( 
 ( #140156, #206180, #190990 ),
 ( #5822, #138006, #57809 ),
 ( #142299, #43720, #58877 ),
 ( #173724, #123970, #72974 ),
 ( #91403, #157463, #9058 ),
 ( #75133, #125033, #42655 ) ),
 .UNSPECIFIED., .F., .F., .T. ) 
 B_SPLINE_SURFACE_WITH_KNOTS ( ( 4, 2, 4 ),
 ( 3, 3 ),
 ( 0.000000000000000000, 0.0003831416164015014384, 0.0007662832328030028768 ),
 ( 0.000000000000000000, 1.000000000000000000 ),
 .UNSPECIFIED. ) 
 GEOMETRIC_REPRESENTATION_ITEM ( )  RATIONAL_B_SPLINE_SURFACE ( (
 ( 1.000000000000000000, 0.7071067811865475727, 1.000000000000000000),
 ( 1.000000000000000000, 0.6829713513656885393, 1.000000000000000000),
 ( 1.000000000000000000, 0.6534833722367636710, 1.000000000000000000),
 ( 1.000000000000000000, 0.6054027484667212633, 1.000000000000000000),
 ( 1.000000000000000000, 0.5875453974411548597, 1.000000000000000000),
 ( 1.000000000000000000, 0.5879095031487528988, 1.000000000000000000) ) ) 
 REPRESENTATION_ITEM ( '' )  SURFACE ( )  );
#77702 = CARTESIAN_POINT ( 'NONE',  ( -6.282224075085783177, 8.422623735723785643, 1.599625672291269396 ) ) ;
#77704 = ORIENTED_EDGE ( 'NONE', *, *, #213278, .T. ) ;
#77703 = CARTESIAN_POINT ( 'NONE',  ( 0.000000000000000000, 14.48154074412737025, -11.92000000000000171 ) ) ;
#77705 = CARTESIAN_POINT ( 'NONE',  ( 3.791807063958370971, 1.597966631936774684, 1.522356218736670153 ) ) ;
#77706 = CARTESIAN_POINT ( 'NONE',  ( 6.151720675889260193, 0.6653518678880927517, -2.162357237652327679 ) ) ;
#77707 = CARTESIAN_POINT ( 'NONE',  ( -6.127922243696855453, 7.211959374810172463, 1.082531754730549967 ) ) ;
#77708 = CARTESIAN_POINT ( 'NONE',  ( 6.345981700719151242, -1.190820116993321243, -1.365292378351635083 ) ) ;
#77709 = CARTESIAN_POINT ( 'NONE',  ( -0.1531117392989979065, -1.803405091603600185, -0.9023890051431044945 ) ) ;
#77710 = CARTESIAN_POINT ( 'NONE',  ( 3.877268743828266029, 6.506935386899531437, 1.082531754730558626 ) ) ;
#77711 = CARTESIAN_POINT ( 'NONE',  ( 6.262560305340551636, -1.321439916381482060, 1.324322166508178356 ) ) ;
#77712 = CARTESIAN_POINT ( 'NONE',  ( 5.813130153884224605, 1.560705751063670377, -1.104717755519408984 ) ) ;
#77713 = VECTOR ( 'NONE', #39211, 1000.000000000000000 ) ;
#77714 = CARTESIAN_POINT ( 'NONE',  ( 0.8482696660519238874, 0.5391449902514727777, 1.791282564952957124 ) ) ;
#77715 = CARTESIAN_POINT ( 'NONE',  ( 0.9718890779336667451, -0.9023411006064323558, 1.803417998987096427 ) ) ;
#77717 = CARTESIAN_POINT ( 'NONE',  ( 4.354198888085320185, 2.105621147513780045, -0.05115374888297812700 ) ) ;
#77716 = CARTESIAN_POINT ( 'NONE',  ( -7.980945979938748103, 12.46285407657057220, 0.000000000000000000 ) ) ;
#77718 = B_SPLINE_CURVE_WITH_KNOTS ( 'NONE', 3,
 ( #971, #82242, #50819, #49753, #201306, #148333 ),
 .UNSPECIFIED., .F., .F.,
 ( 4, 2, 4 ),
 ( 0.000000000000000000, 0.0003258677429877278493, 0.0006517354859754556987 ),
 .UNSPECIFIED. ) ;
#77719 = CARTESIAN_POINT ( 'NONE',  ( 7.235247531187115833, 11.59287255302699648, -0.7998128361456291469 ) ) ;
#77721 = CARTESIAN_POINT ( 'NONE',  ( -9.854078719034067291, 10.39084668182823634, 0.7998128361456462443 ) ) ;
#77720 = CARTESIAN_POINT ( 'NONE',  ( 1.499999999999987121, -0.7458333333333122539, 0.8660254037844524744 ) ) ;
#77722 = CARTESIAN_POINT ( 'NONE',  ( 0.000000000000000000, 13.49999999999999822, 0.000000000000000000 ) ) ;
#77723 = CARTESIAN_POINT ( 'NONE',  ( 3.551039915000217206, 0.3004019028194653829, 1.997212655505080203 ) ) ;
#77724 = CARTESIAN_POINT ( 'NONE',  ( -1.364683531249997417, 3.259375000341423245, 1.214306433183764966E-14 ) ) ;
#77725 = CARTESIAN_POINT ( 'NONE',  ( 8.920901888111986366, 12.39117405523060889, 1.082531754730546636 ) ) ;
#77726 = EDGE_CURVE ( 'NONE', #96829, #108458, #186530, .T. ) ;
#77727 = CARTESIAN_POINT ( 'NONE',  ( 3.058072297120766336, 2.151488047868503894, -0.2085137855245971505 ) ) ;
#77728 = CARTESIAN_POINT ( 'NONE',  ( -1.499999999999993339, 10.64264068711930733, 1.232676135170975238E-14 ) ) ;
#77729 = CARTESIAN_POINT ( 'NONE',  ( -0.7500000000000215383, 4.691666666666684193, 1.299038105676671107 ) ) ;
#77731 = CARTESIAN_POINT ( 'NONE',  ( -9.491602870538727643, -9.241975548351229364, 0.4178506376739494765 ) ) ;
#77730 = CARTESIAN_POINT ( 'NONE',  ( 8.005163354226054295, 8.304055099544019214, 0.000000000000000000 ) ) ;
#77732 = CARTESIAN_POINT ( 'NONE',  ( 9.544576953896278582, 10.23768732240824164, 0.000000000000000000 ) ) ;
#77734 = CARTESIAN_POINT ( 'NONE',  ( 7.986935577548707421, 15.27020226968796734, -8.898074972344000244 ) ) ;
#77733 = CARTESIAN_POINT ( 'NONE',  ( 0.9597157272863182653, 1.774996621215488624, 1.250093255441329543 ) ) ;
#77735 = CIRCLE ( 'NONE', #209136, 0.4800000000000000933 ) ;
#77736 = CARTESIAN_POINT ( 'NONE',  ( -5.097502569058207200, 8.890910730635814829, -0.7216878364870207285 ) ) ;
#77737 = CARTESIAN_POINT ( 'NONE',  ( -1.364683531249997417, 2.509375000341422357, 1.214306433183764966E-14 ) ) ;
#77738 = CARTESIAN_POINT ( 'NONE',  ( 2.349409277133751139, 0.5813161652389825518, -2.113004480973964760 ) ) ;
#77739 = CARTESIAN_POINT ( 'NONE',  ( 6.983263157960360346, 2.057644363497754814, 2.260506123227977948 ) ) ;
#77740 = CARTESIAN_POINT ( 'NONE',  ( 2.342968712349004168, 0.4955985968413346709, 2.207426715909040826 ) ) ;
#77741 = CARTESIAN_POINT ( 'NONE',  ( -8.016948904382338981, 8.247528564734524892, -0.7998128361456291469 ) ) ;
#77742 = CARTESIAN_POINT ( 'NONE',  ( -1.364683531250010295, 5.342708333674750953, 0.7879004041258379498 ) ) ;
#77743 = CARTESIAN_POINT ( 'NONE',  ( 5.417061852544872380, 7.532864896096530316, 1.248242807326222392 ) ) ;
#77744 = CARTESIAN_POINT ( 'NONE',  ( -0.7500000000000006661, 12.45833333333333570, -1.299038105676657340 ) ) ;
#77745 = CARTESIAN_POINT ( 'NONE',  ( 5.234856708652215751, 9.121433570154021453, 0.7216878364870317197 ) ) ;
#77746 = EDGE_CURVE ( 'NONE', #29424, #76787, #104483, .T. ) ;
#77747 = CARTESIAN_POINT ( 'NONE',  ( 3.936565515923634795, 0.2574710272360211105, 1.750749954138763442 ) ) ;
#77748 = CARTESIAN_POINT ( 'NONE',  ( 9.772729797352075920, 10.29593960653257234, -0.7998128361456281477 ) ) ;
#77749 = CARTESIAN_POINT ( 'NONE',  ( 0.7980485993467776318, -0.7579980429349441051, 1.964993406121709807 ) ) ;
#77751 = CARTESIAN_POINT ( 'NONE',  ( 1.499999999999989120, 0.5250000000000185629, 0.000000000000000000 ) ) ;
#77750 = CARTESIAN_POINT ( 'NONE',  ( 0.6823417656249934904, 9.192708333674733723, 1.181850606188764807 ) ) ;
#77752 = CARTESIAN_POINT ( 'NONE',  ( -4.878955176071358757, 6.785476686873604280, -1.599625672291271394 ) ) ;
#77753 = CARTESIAN_POINT ( 'NONE',  ( 6.222279831957800766, 1.994873610751911164, 0.2930524845206964879 ) ) ;
#77754 = ORIENTED_EDGE ( 'NONE', *, *, #94349, .F. ) ;
#77755 = CARTESIAN_POINT ( 'NONE',  ( 8.401248741962376698, 12.95320729893149370, 0.7998128361456462443 ) ) ;
#77756 = CARTESIAN_POINT ( 'NONE',  ( 3.151090109352538082, -1.528452604574185525, -1.078222621661927061 ) ) ;
#77757 = CARTESIAN_POINT ( 'NONE',  ( 4.926661076633905623, -1.356332079400805135, 1.564123780295342492 ) ) ;
#77758 = CARTESIAN_POINT ( 'NONE',  ( -7.390603132780803719, 7.794994207765291172, -0.7216878364870338292 ) ) ;
#77759 = CARTESIAN_POINT ( 'NONE',  ( 0.000000000000000000, 0.4330127018922214077, 6.500000000000000000 ) ) ;
#77760 = CARTESIAN_POINT ( 'NONE',  ( 7.564559641420864899, 10.91273778404466199, -1.199719254218446718 ) ) ;
#77761 = CARTESIAN_POINT ( 'NONE',  ( -8.455481356417053007, 13.01647868246193518, 0.7998128361456341429 ) ) ;
#77762 = CARTESIAN_POINT ( 'NONE',  ( 5.072905659164107739, 4.910989440906482706, -0.2235617647182771561 ) ) ;
#77763 = EDGE_CURVE ( 'NONE', #160452, #160219, #13529, .T. ) ;
#77764 = CARTESIAN_POINT ( 'NONE',  ( 1.364683531249990311, 5.196875000341417916, 1.214306433183764966E-14 ) ) ;
#77765 = VECTOR ( 'NONE', #61582, 1000.000000000000114 ) ;
#77766 = CARTESIAN_POINT ( 'NONE',  ( 4.351973852746993110, -0.7528527933186466292, 1.811862133468461922 ) ) ;
#77767 = EDGE_CURVE ( 'NONE', #164652, #23582, #68078, .T. ) ;
#77768 = CARTESIAN_POINT ( 'NONE',  ( 0.8431247865267020858, -1.122328847578180078, 1.674629589540656216 ) ) ;
#77769 = CARTESIAN_POINT ( 'NONE',  ( -4.767627293860968507, 5.591261926706423857, -1.199719254218453823 ) ) ;
#77771 = CARTESIAN_POINT ( 'NONE',  ( 7.834948825496932834, -5.907420853759296264, 7.720982897393586342 ) ) ;
#77770 = CARTESIAN_POINT ( 'NONE',  ( 7.411503528164766763, 11.79850454950093841, 1.040834085586084257E-14 ) ) ;
#77772 = CARTESIAN_POINT ( 'NONE',  ( 1.229531971273215341, -1.182229855178434930, -1.449605969065965949 ) ) ;
#77773 = CARTESIAN_POINT ( 'NONE',  ( -1.364683531250012516, 3.738541667008087099, -0.7879004041258300672 ) ) ;
#77774 = CARTESIAN_POINT ( 'NONE',  ( 2.777592571122803555, 0.2913108041502753820, -1.991885045997557224 ) ) ;
#77776 = CARTESIAN_POINT ( 'NONE',  ( 2.320046401798322222, 0.9952771033397389555, -1.868693074688542843 ) ) ;
#77775 = CARTESIAN_POINT ( 'NONE',  ( -4.921246572080546500, 8.685278734161874681, 1.214306433183764966E-14 ) ) ;
#77777 = DIRECTION ( 'NONE',  ( 0.000000000000000000, -1.000000000000000000, 0.000000000000000000 ) ) ;
#77778 = CARTESIAN_POINT ( 'NONE',  ( 3.473154722801426786, 1.870513717286937494, 0.8877811045280564750 ) ) ;
#77779 = CARTESIAN_POINT ( 'NONE',  ( 7.614839552730775729, 8.913009562054615031, 1.199719254218452047 ) ) ;
#77781 = CARTESIAN_POINT ( 'NONE',  ( 3.999819011231439347, 4.625209253646830554, 1.199719254218464037 ) ) ;
#77780 = CARTESIAN_POINT ( 'NONE',  ( 0.2223640086436579066, 2.001884549173582606, 0.6031067468692548061 ) ) ;
#77783 = ORIENTED_EDGE ( 'NONE', *, *, #46115, .T. ) ;
#77782 = CARTESIAN_POINT ( 'NONE',  ( 5.649374308873757577, -1.440485763676568443, -1.121356984487072328 ) ) ;
#77784 = CARTESIAN_POINT ( 'NONE',  ( 9.426996880203592610, 9.892584536526015881, -0.7998128361456281477 ) ) ;
#77785 = CARTESIAN_POINT ( 'NONE',  ( 3.741371894207385917, 7.428709027653158437, -2.448389769268734195 ) ) ;
#77786 = CARTESIAN_POINT ( 'NONE',  ( 9.709990956404908502, 13.29774486163194958, 8.129890332494706939 ) ) ;
#77787 = CARTESIAN_POINT ( 'NONE',  ( -10.33392256004288079, 4.765625372279607141, 5.445010993851796322 ) ) ;
#77788 = CARTESIAN_POINT ( 'NONE',  ( -0.6823417656250003738, 11.46354166700806765, 1.181850606188754593 ) ) ;
#77789 = CARTESIAN_POINT ( 'NONE',  ( 5.127564033545165323, -0.2766344828325461580, 1.892035409188079997 ) ) ;
#77790 = CARTESIAN_POINT ( 'NONE',  ( -7.645908563102897126, 11.00764485934031889, 1.199719254218453823 ) ) ;
#77791 = CARTESIAN_POINT ( 'NONE',  ( 6.993308306550549247, 7.053281200597435685, 1.040834085586084257E-14 ) ) ;
#77792 = B_SPLINE_CURVE_WITH_KNOTS ( 'NONE', 3,
 ( #35067, #34013, #84899, #83824, #2550, #70754 ),
 .UNSPECIFIED., .F., .F.,
 ( 4, 2, 4 ),
 ( 0.000000000000000000, 0.0003778774010236168076, 0.0007557548020472336153 ),
 .UNSPECIFIED. ) ;
#77793 = CARTESIAN_POINT ( 'NONE',  ( -4.957638175832625493E-14, 2.359375000341373152, -1.570758158831806250 ) ) ;
#77794 = CARTESIAN_POINT ( 'NONE',  ( 3.511198595814926993, 6.079853547550633230, 1.082531754730558626 ) ) ;
#77795 = CARTESIAN_POINT ( 'NONE',  ( 9.499668754385638181, -7.473374494045003757, 0.07933194154488365513 ) ) ;
#77796 = CARTESIAN_POINT ( 'NONE',  ( 4.334856428067313416, 6.080418470877079429, -1.599625672291256295 ) ) ;
#77797 = ORIENTED_EDGE ( 'NONE', *, *, #78667, .F. ) ;
#77798 = CARTESIAN_POINT ( 'NONE',  ( -6.912678218121246942, 9.158153569265168770, 1.599625672291269396 ) ) ;
#77799 = CARTESIAN_POINT ( 'NONE',  ( 1.467871227757891193E-11, -3.138498625356828775, -3.379301813585260383 ) ) ;
#77800 = CARTESIAN_POINT ( 'NONE',  ( 6.587282531393223728, 8.778525268082516320, 1.599625672291268286 ) ) ;
#77801 = FILL_AREA_STYLE_COLOUR ( '', #143836 ) ;
#77802 = CARTESIAN_POINT ( 'NONE',  ( -5.425839481171796486, 7.540841100536294306, 1.248335065278019629 ) ) ;
#77803 = CARTESIAN_POINT ( 'NONE',  ( -4.609409038966229666, 8.321468278861834378, -0.7216878364870267237 ) ) ;
#77804 = CARTESIAN_POINT ( 'NONE',  ( 2.984766373302843778, 6.633977868828633717, -0.7998128361456291469 ) ) ;
#77805 = CARTESIAN_POINT ( 'NONE',  ( 2.606253914610905387, 1.968914028630329272, 0.05319026939461755227 ) ) ;
#77806 = CARTESIAN_POINT ( 'NONE',  ( 3.005482631727268039, -1.942536929278560365, 0.5405117225928540714 ) ) ;
#77807 = CARTESIAN_POINT ( 'NONE',  ( -6.320072162264675164, 10.52516795595079557, 0.7998128361456481317 ) ) ;
#77808 = CARTESIAN_POINT ( 'NONE',  ( 6.150558962454855561, 7.204682206732687000, 1.199719254218452047 ) ) ;
#77809 = CARTESIAN_POINT ( 'NONE',  ( 6.827182134110222123, 7.629137130509067610, 2.789055895399249252 ) ) ;
#77810 = CARTESIAN_POINT ( 'NONE',  ( 3.556733441538503016, -1.932615445784117369, -1.033156731641969195 ) ) ;
#77811 = DIRECTION ( 'NONE',  ( 0.000000000000000000, 0.000000000000000000, 1.000000000000000000 ) ) ;
#77812 = CARTESIAN_POINT ( 'NONE',  ( 2.344641424807081709, 0.4199494819796690814, 1.879913682802894614 ) ) ;
#77813 = CARTESIAN_POINT ( 'NONE',  ( -8.809047120577080392, 11.30030761213851953, 1.599625672291269396 ) ) ;
#77814 = CARTESIAN_POINT ( 'NONE',  ( 0.1331565106231363538, 2.033293680964400885, -2.362282156872722805 ) ) ;
#77815 = CARTESIAN_POINT ( 'NONE',  ( -10.10707714348148301, 4.359868340440408829, -5.857196085253971063 ) ) ;
#77816 = CARTESIAN_POINT ( 'NONE',  ( 7.741869408603235136, 8.990934717247309749, 1.199719254218462483 ) ) ;
#77817 = CARTESIAN_POINT ( 'NONE',  ( 6.796715079152391148, 6.823922435299587974, 0.7998128361456341429 ) ) ;
#77818 = DIRECTION ( 'NONE',  ( 0.000000000000000000, 0.000000000000000000, -1.000000000000000000 ) ) ;
#77819 = CARTESIAN_POINT ( 'NONE',  ( 4.529832720741620022, 7.338536369956936589, -1.082531754730548412 ) ) ;
#77820 = VERTEX_POINT ( 'NONE', #149363 ) ;
#77822 = CARTESIAN_POINT ( 'NONE',  ( 1.242838715397933225, 1.940741670474394498, 0.5346661475282618037 ) ) ;
#77821 = CARTESIAN_POINT ( 'NONE',  ( 6.022987620897008121, -1.731432113864934674, 0.6267441317700100933 ) ) ;
#77823 = CARTESIAN_POINT ( 'NONE',  ( 4.640180047935675844, 0.006009439367033602396, -2.298542322207643984 ) ) ;
#77825 = CARTESIAN_POINT ( 'NONE',  ( 2.043593076603223757, 1.278923709890807503, 1.352104710524345554 ) ) ;
#77824 = CARTESIAN_POINT ( 'NONE',  ( -0.02919842301645457147, 6.946858002156226064, -2.668856405631584217 ) ) ;
#77826 = CARTESIAN_POINT ( 'NONE',  ( -3.285556943749998737, -2.180208332855376518, 1.896917185911908499 ) ) ;
#77827 = CARTESIAN_POINT ( 'NONE',  ( -0.1290005225502641184, 1.996213967822700663, -2.587563282167547385 ) ) ;
#77828 = CARTESIAN_POINT ( 'NONE',  ( 5.133030909251353968, 1.769313487831367659, 0.7262901588861517821 ) ) ;
#77829 = CARTESIAN_POINT ( 'NONE',  ( -6.184490626128011925, 10.36698949712469364, -0.7998128361456291469 ) ) ;
#77830 = CARTESIAN_POINT ( 'NONE',  ( -6.292392690518223475, 6.513748691792265788, -0.7216878364870338292 ) ) ;
#77832 = CARTESIAN_POINT ( 'NONE',  ( 3.502682687546424312, 1.475339254275360279, -1.149998991230333223 ) ) ;
#77831 = CARTESIAN_POINT ( 'NONE',  ( 4.458587642939345841, -1.868375113230103857, -0.9383987773294580892 ) ) ;
#77833 = CARTESIAN_POINT ( 'NONE',  ( 6.995644074971448134, 7.263932296995902149, -0.7216878364870257245 ) ) ;
#77834 = VERTEX_POINT ( 'NONE', #37747 ) ;
#77835 = CARTESIAN_POINT ( 'NONE',  ( 0.000000000000000000, -0.5000000000000004441, 0.000000000000000000 ) ) ;
#77836 = DIRECTION ( 'NONE',  ( -5.578564026256491869E-16, -1.000000000000000000, -9.066213480720160632E-32 ) ) ;
#77837 = CARTESIAN_POINT ( 'NONE',  ( 6.270102258788001315, 0.8933021238881621029, 1.475393591635131507 ) ) ;
#77838 = CARTESIAN_POINT ( 'NONE',  ( -6.586563698140583512, 6.578745824119123675, 1.040834085586084257E-14 ) ) ;
#77839 = CARTESIAN_POINT ( 'NONE',  ( 1.300929835083320274, 1.165380355416269609, -1.284392162598305021 ) ) ;
#77840 = CARTESIAN_POINT ( 'NONE',  ( -11.84668730067608600, 10.90000000000000036, -1.400000000000001910 ) ) ;
#77841 = EDGE_CURVE ( 'NONE', #137780, #55379, #18275, .T. ) ;
#77842 = CARTESIAN_POINT ( 'NONE',  ( 6.051681997923831879, 1.638823605779341053, 1.424080724270002873 ) ) ;
#77843 = CARTESIAN_POINT ( 'NONE',  ( 4.406759617291758246, 1.409692282476209924, -1.160130723419292353 ) ) ;
#77844 = CARTESIAN_POINT ( 'NONE',  ( 1.832786370036399326, -1.861117592713131819, -0.6203919267877274768 ) ) ;
#77845 = CARTESIAN_POINT ( 'NONE',  ( 0.6150561885070615631, 0.1604698007556179251, 2.111222410368835067 ) ) ;
#77846 = DIRECTION ( 'NONE',  ( -1.000000000000000000, 0.000000000000000000, 0.000000000000000000 ) ) ;
#77847 = CARTESIAN_POINT ( 'NONE',  ( 0.000000000000000000, 15.51887838114830132, 0.000000000000000000 ) ) ;
#77848 = CARTESIAN_POINT ( 'NONE',  ( 8.450809820019639318, 8.753699632978056755, -0.7998128361456291469 ) ) ;
#77849 = CARTESIAN_POINT ( 'NONE',  ( 2.842561206135377994, 1.176089095116246153, -1.764248410475676820 ) ) ;
#77850 = CARTESIAN_POINT ( 'NONE',  ( -3.795919822146283540, 6.412028311603867436, -1.082531754730549967 ) ) ;
#77851 = AXIS2_PLACEMENT_3D ( 'NONE', #177489, #46425, #32298 ) ;
#77852 = DIRECTION ( 'NONE',  ( -0.000000000000000000, -1.000000000000000000, -0.000000000000000000 ) ) ;
#77853 = CARTESIAN_POINT ( 'NONE',  ( -4.654334680973787108, 6.904393480334801048, -1.215188995478516221 ) ) ;
#77854 = CARTESIAN_POINT ( 'NONE',  ( 0.2333690889706682703, 0.003390530909083006028, -2.053566628440507635 ) ) ;
#77856 = CARTESIAN_POINT ( 'NONE',  ( -0.7500000000000179856, 13.82291666734946567, 1.299038105676658228 ) ) ;
#77855 = CARTESIAN_POINT ( 'NONE',  ( -10.84254087577866521, 4.919568073182916557, 5.035408296252067650 ) ) ;
#77859 = ORIENTED_EDGE ( 'NONE', *, *, #108140, .T. ) ;
#77858 = CARTESIAN_POINT ( 'NONE',  ( 3.545754021904829134, -2.051903114543842666, 0.8512574589945339776 ) ) ;
#77857 = AXIS2_PLACEMENT_3D ( 'NONE', #1065, #35716, #84471 ) ;
#77860 = CARTESIAN_POINT ( 'NONE',  ( 0.5108563537194388271, -2.180326652049785707, 0.7283127579034570642 ) ) ;
#77862 = CARTESIAN_POINT ( 'NONE',  ( 5.014538805069497229, 0.7844730879308317029, 1.907755517398136647 ) ) ;
#77861 = CARTESIAN_POINT ( 'NONE',  ( 2.900554798319789906, 5.471398800426671372, 1.199719254218452047 ) ) ;
#77864 = CARTESIAN_POINT ( 'NONE',  ( 1.737499999999999378, -2.566666666666668650, -3.009438278150925683 ) ) ;
#77863 = CARTESIAN_POINT ( 'NONE',  ( 3.867818961648523235, 7.734482231890414283, 1.040834085586084257E-14 ) ) ;
#77865 = FACE_OUTER_BOUND ( 'NONE', #162813, .T. ) ;
#77866 = CARTESIAN_POINT ( 'NONE',  ( 5.144037045698616417, 0.5398437887287730330, 1.760322748975438500 ) ) ;
#77867 = CARTESIAN_POINT ( 'NONE',  ( -3.331659036430328236, 7.719744385808867015, -2.450696915730449454 ) ) ;
#77868 = ADVANCED_FACE ( 'NONE', ( #69148 ), #201282, .T. ) ;
#77869 = CARTESIAN_POINT ( 'NONE',  ( 4.355193658487811703, 6.104145239700998538, -1.599625672291255185 ) ) ;
#77870 = CARTESIAN_POINT ( 'NONE',  ( 2.871755265489631448, 0.9208624611983186048, 1.458155879698035395 ) ) ;
#77871 = CARTESIAN_POINT ( 'NONE',  ( 1.007046422456716384, -0.04465021774549028655, 2.016188868504041665 ) ) ;
#77872 =( BOUNDED_SURFACE ( )  B_SPLINE_SURFACE ( 3, 2, ( 
 ( #133866, #1658, #199873 ),
 ( #42758, #38458, #41687 ),
 ( #191089, #90421, #104535 ),
 ( #186828, #154344, #190034 ),
 ( #106713, #24315, #156490 ),
 ( #6990, #137034, #105621 ),
 ( #170581, #89359, #26468 ),
 ( #39521, #107798, #9155 ) ),
 .UNSPECIFIED., .F., .F., .T. ) 
 B_SPLINE_SURFACE_WITH_KNOTS ( ( 4, 2, 2, 4 ),
 ( 3, 3 ),
 ( 0.000000000000000000, 0.0005109843281227146802, 0.0007664764921840720203, 0.001021968656245429360 ),
 ( 0.000000000000000000, 1.000000000000000000 ),
 .UNSPECIFIED. ) 
 GEOMETRIC_REPRESENTATION_ITEM ( )  RATIONAL_B_SPLINE_SURFACE ( (
 ( 1.000000000000000000, 0.7045118851637611757, 1.000000000000000000),
 ( 1.000000000000000000, 0.6478559580220908387, 1.000000000000000000),
 ( 1.000000000000000000, 0.5832506164448501007, 1.000000000000000000),
 ( 1.000000000000000000, 0.4879709628489244944, 1.000000000000000000),
 ( 1.000000000000000000, 0.4561823831825844722, 1.000000000000000000),
 ( 1.000000000000000000, 0.4039565156456113582, 1.000000000000000000),
 ( 1.000000000000000000, 0.3848936348730044310, 1.000000000000000000),
 ( 1.000000000000000000, 0.3826834323650832315, 1.000000000000000000) ) ) 
 REPRESENTATION_ITEM ( '' )  SURFACE ( )  );
#77873 = CARTESIAN_POINT ( 'NONE',  ( 2.848558797923263164, 0.3346648989216906012, -2.274091979294257992 ) ) ;
#77874 = CARTESIAN_POINT ( 'NONE',  ( -1.201851678989727383E-14, 4.259375000341417028, -1.575800808251660134 ) ) ;
#77875 = CARTESIAN_POINT ( 'NONE',  ( 2.636292518416444075, 1.068738387235500298, -1.994089298797457666 ) ) ;
#77876 = CARTESIAN_POINT ( 'NONE',  ( 5.145193760806440864, -1.806914327231067929, 1.081695767794567775 ) ) ;
#77877 = CARTESIAN_POINT ( 'NONE',  ( -6.238160076063538284, 9.331584951165851294, 1.082531754730549967 ) ) ;
#77878 = CARTESIAN_POINT ( 'NONE',  ( 3.444378845967084324, 0.4270997545614327318, 1.717301222563255791 ) ) ;
#77879 = CARTESIAN_POINT ( 'NONE',  ( 5.799137018343234473, 7.788745826199009237, -1.599625672291262513 ) ) ;
#77881 = CARTESIAN_POINT ( 'NONE',  ( 5.987847201643853978, -2.280908734910926938, -0.2287418647285797413 ) ) ;
#77880 = CARTESIAN_POINT ( 'NONE',  ( 5.031484404002891431, 5.042689024191078673, 0.7216878364870328300 ) ) ;
#77882 = CARTESIAN_POINT ( 'NONE',  ( 4.083814069670049562, -1.821384084514931612, -0.2681248149544179227 ) ) ;
#77883 = CARTESIAN_POINT ( 'NONE',  ( -5.220052836461385404, 6.048815383081766583, -1.199719254218446718 ) ) ;
#77884 = CARTESIAN_POINT ( 'NONE',  ( 4.473827502385202770, 8.163289819517311585, 1.040834085586084257E-14 ) ) ;
#77885 = CARTESIAN_POINT ( 'NONE',  ( 1.499999999999987121, 3.045833333333353377, -0.8660254037844262731 ) ) ;
#77886 = EDGE_CURVE ( 'NONE', #9659, #211508, #88339, .T. ) ;
#77887 = CARTESIAN_POINT ( 'NONE',  ( 4.136819237485493517, -1.907179771870757046, 1.079280405373375773 ) ) ;
#77888 = CARTESIAN_POINT ( 'NONE',  ( -2.950870989268691957, 6.594433254122103349, -0.7998128361456281477 ) ) ;
#77889 = CARTESIAN_POINT ( 'NONE',  ( 0.4599077567407924838, 8.047644787141630118, -1.947158400785528487 ) ) ;
#77890 = DIRECTION ( 'NONE',  ( 0.000000000000000000, 1.000000000000000000, 0.000000000000000000 ) ) ;
#77891 = CARTESIAN_POINT ( 'NONE',  ( 0.6823417656249899377, 4.176041667008085767, -1.181850606188754593 ) ) ;
#77892 = CARTESIAN_POINT ( 'NONE',  ( 3.545458749278436184, -1.459459766114965973, -1.257631776117454914 ) ) ;
#77893 = CARTESIAN_POINT ( 'NONE',  ( -1.364683531250000748, 8.359375000341396245, 0.000000000000000000 ) ) ;
#77894 = CARTESIAN_POINT ( 'NONE',  ( -3.280709984826970516, 6.771319382366015383, 0.7216878364870317197 ) ) ;
#77895 = CARTESIAN_POINT ( 'NONE',  ( 6.504144398916748671, -0.9053081408615070158, 1.915699539216948688 ) ) ;
#77896 = ORIENTED_EDGE ( 'NONE', *, *, #41175, .T. ) ;
#77898 = CARTESIAN_POINT ( 'NONE',  ( -3.456965981804629884, 6.976951378839947537, 1.040834085586084257E-14 ) ) ;
#77897 = CARTESIAN_POINT ( 'NONE',  ( -3.363831509966363598, 5.978201624052440266, -1.082531754730548412 ) ) ;
#77899 = CARTESIAN_POINT ( 'NONE',  ( 3.948449050077836642, 5.629609863222681199, 1.599625672291267398 ) ) ;
#77900 = CARTESIAN_POINT ( 'NONE',  ( 4.908649743871434268, 4.822872567462811233, -0.4817574433751614094 ) ) ;
#77901 = FACE_OUTER_BOUND ( 'NONE', #29764, .T. ) ;
#77903 = EDGE_CURVE ( 'NONE', #35911, #105939, #63189, .T. ) ;
#77902 = CARTESIAN_POINT ( 'NONE',  ( 0.5023040531197673353, 1.956348610274569744, 0.1481081594910879096 ) ) ;
#77904 = CARTESIAN_POINT ( 'NONE',  ( -1.364683531250000748, 0.8218750003414210248, 0.000000000000000000 ) ) ;
#77905 = CARTESIAN_POINT ( 'NONE',  ( 6.825078400183575589, -0.005632053428735600553, 2.144262460745151255 ) ) ;
#77906 = EDGE_CURVE ( 'NONE', #141010, #101381, #156850, .T. ) ;
#77907 = CARTESIAN_POINT ( 'NONE',  ( 5.318788500806308051, -1.422220495204097546, 1.351624447685224162 ) ) ;
#77908 = CARTESIAN_POINT ( 'NONE',  ( -8.299562589859897699, 12.83457345481192036, -0.7998128361456281477 ) ) ;
#77909 = CARTESIAN_POINT ( 'NONE',  ( -6.209271164934474285, 6.346497235286081562, 1.040834085586084257E-14 ) ) ;
#77910 = VECTOR ( 'NONE', #83868, 1000.000000000000000 ) ;
#77911 = CARTESIAN_POINT ( 'NONE',  ( 5.348557406608104969, 0.6236849695623291057, 2.069784783864880851 ) ) ;
#77913 = EDGE_LOOP ( 'NONE', ( #58613, #144797, #49793, #162481 ) ) ;
#77912 = CARTESIAN_POINT ( 'NONE',  ( -0.2104748580754426390, 2.865278511227668634, -2.591885361450113834 ) ) ;
#77914 = CARTESIAN_POINT ( 'NONE',  ( 1.364683531249990311, 4.884375000341417916, 1.214306433183764966E-14 ) ) ;
#77915 = CARTESIAN_POINT ( 'NONE',  ( 0.4736314445139556684, 1.071599637473351629, 1.532994764490814177 ) ) ;
#77916 = CARTESIAN_POINT ( 'NONE',  ( 5.958250847983307175, 1.314789979124462382, 1.130330842948763514 ) ) ;
#77918 = CARTESIAN_POINT ( 'NONE',  ( 3.157961424266928052, 0.9873743524775533409, 1.956624655947765357 ) ) ;
#77917 = CARTESIAN_POINT ( 'NONE',  ( -1.360316468750006669, 0.1614583336747227316, 0.7853790794158981292 ) ) ;
#77919 = CARTESIAN_POINT ( 'NONE',  ( 2.872455039471259575, 1.233635154574242554, 1.949979759383664524 ) ) ;
#77920 = CARTESIAN_POINT ( 'NONE',  ( 6.046181036401986120, 2.058226046012123334, 0.1054989004632029409 ) ) ;
#77921 = CARTESIAN_POINT ( 'NONE',  ( 1.253738886202176106, 0.7867099759248905588, 1.775636482627058088 ) ) ;
#77922 = CARTESIAN_POINT ( 'NONE',  ( -7.009202228140764213, 7.279750142360097875, -0.7216878364870267237 ) ) ;
#77923 = MECHANICAL_DESIGN_GEOMETRIC_PRESENTATION_REPRESENTATION (  '', ( #71085 ), #88290 ) ;
#77924 = CARTESIAN_POINT ( 'NONE',  ( -0.1796516426514560283, -8.073984524010633379, -9.498564853506501038 ) ) ;
#77925 = CARTESIAN_POINT ( 'NONE',  ( -9.367496997601305608, 14.48154074412967596, 7.499999999995371702 ) ) ;
#77926 = CARTESIAN_POINT ( 'NONE',  ( 4.746395313581045272, 1.087821826000658909, -1.820160695957805608 ) ) ;
#77927 = CARTESIAN_POINT ( 'NONE',  ( 3.248783280693067424E-12, 2.974000657016963256, 11.66643802584408185 ) ) ;
#77928 = CARTESIAN_POINT ( 'NONE',  ( 2.356092462967720458, 0.09613450340887133572, -2.014232768679749430 ) ) ;
#77929 = CARTESIAN_POINT ( 'NONE',  ( -4.704316113817535339, 8.432193199521691440, 0.7216878364870458196 ) ) ;
#77930 = CARTESIAN_POINT ( 'NONE',  ( 5.561621765989873900, 0.4355406452380207738, -2.163202247768724718 ) ) ;
#77931 = CARTESIAN_POINT ( 'NONE',  ( -4.676113526401191933, 5.272618711636657629, 1.141756068723397854 ) ) ;
#77932 = CARTESIAN_POINT ( 'NONE',  ( -10.23127510237379667, 3.700502905159952949, 5.878152162067748598 ) ) ;
#77933 = CARTESIAN_POINT ( 'NONE',  ( 0.4338677482375961070, 0.9413943332680120291, -1.564114433284753636 ) ) ;
#77934 = CYLINDRICAL_SURFACE ( 'NONE', #92615, 0.07999999999999993228 ) ;
#77936 = CARTESIAN_POINT ( 'NONE',  ( -5.607897038807837298, 5.667647723685407257, 0.4330508580119977746 ) ) ;
#77935 = CARTESIAN_POINT ( 'NONE',  ( -4.762965077474956566, 8.286028185285090331, 0.8196324637163689975 ) ) ;
#77937 = CARTESIAN_POINT ( 'NONE',  ( -4.969177613625957335, 8.005234357488689056, 1.071350258858670967 ) ) ;
#77938 = ORIENTED_EDGE ( 'NONE', *, *, #180702, .T. ) ;
#77939 = CARTESIAN_POINT ( 'NONE',  ( 4.118082307656718122, -1.057753326809774963, -1.768578378466668877 ) ) ;
#77940 = DIRECTION ( 'NONE',  ( 0.9446243521954068578, 0.000000000000000000, 0.3281536732072456997 ) ) ;
#77941 = CARTESIAN_POINT ( 'NONE',  ( -0.07933194154488883154, -7.473374494045017968, 9.499668754385636404 ) ) ;
#77942 = CARTESIAN_POINT ( 'NONE',  ( -5.742041750587549842, 6.657802449562273850, 1.199719254218450271 ) ) ;
#77943 = CARTESIAN_POINT ( 'NONE',  ( -3.169574050544739841, 6.919863168935977527, -0.7998128361456481317 ) ) ;
#77944 = CARTESIAN_POINT ( 'NONE',  ( 4.248697963213067474, 1.981114831247460017, 0.3918398546494082368 ) ) ;
#77945 = CARTESIAN_POINT ( 'NONE',  ( -0.7500000000000006661, 0.8583333333333567072, -1.299038105676652011 ) ) ;
#77947 = CARTESIAN_POINT ( 'NONE',  ( 9.246297574839980271, 10.85006392781057905, 1.082531754730549967 ) ) ;
#77946 = CARTESIAN_POINT ( 'NONE',  ( -3.494969737272722643, 7.299491470118629088, -0.7998128361456481317 ) ) ;
#77948 = CARTESIAN_POINT ( 'NONE',  ( 7.091078035147269532, 8.231678114882006625, 1.199719254218462483 ) ) ;
#77949 = CARTESIAN_POINT ( 'NONE',  ( 2.975518139630950021, 1.957357868463033501, -0.6452315760040390202 ) ) ;
#77950 = CARTESIAN_POINT ( 'NONE',  ( 2.953750172290267706, -1.864168560446223033, -0.7691209412190866956 ) ) ;
#77951 = VERTEX_POINT ( 'NONE', #23616 ) ;
#77952 = CARTESIAN_POINT ( 'NONE',  ( 1.899436509991839772, 3.291494839451058585, -0.4074537448169834319 ) ) ;
#77953 = CARTESIAN_POINT ( 'NONE',  ( 5.192936529234042808, 6.017179691316550283, -1.199719254218452047 ) ) ;
#77955 = VERTEX_POINT ( 'NONE', #76642 ) ;
#77954 = CARTESIAN_POINT ( 'NONE',  ( -0.07021666366558332317, 7.008523639392694626, -2.000250312771549854 ) ) ;
#77956 = CARTESIAN_POINT ( 'NONE',  ( 2.882185300971401798, -0.2004049647258976941, 2.006138917898095730 ) ) ;
#77957 = CARTESIAN_POINT ( 'NONE',  ( 2.923586578878138109, 1.022379729796508041, -1.530975008504284141 ) ) ;
#77958 = CARTESIAN_POINT ( 'NONE',  ( 1.102667438898880192, -2.307868968971817036, 0.004735511273680144059 ) ) ;
#77959 = CARTESIAN_POINT ( 'NONE',  ( 3.901714345682657292, 7.774026846596938434, 0.7998128361456271485 ) ) ;
#77960 = CARTESIAN_POINT ( 'NONE',  ( 2.319794969891198821, -2.097318901067245722, 0.5227781780692899449 ) ) ;
#77961 = CARTESIAN_POINT ( 'NONE',  ( -7.074657228232555717, 7.148188275893099686, 1.040834085586084257E-14 ) ) ;
#77962 = CARTESIAN_POINT ( 'NONE',  ( 2.636409100479879086, 0.1147267580069409321, -2.295643959171574711 ) ) ;
#77963 = EDGE_LOOP ( 'NONE', ( #132293, #81324, #46938, #202483 ) ) ;
#77964 = DIRECTION ( 'NONE',  ( -0.000000000000000000, -1.000000000000000000, -0.000000000000000000 ) ) ;
#77965 = CARTESIAN_POINT ( 'NONE',  ( 1.481098450213329976, 1.729700800547562478, -0.7128637423776186255 ) ) ;
#77966 = CARTESIAN_POINT ( 'NONE',  ( 5.278184311449350297, -1.095828550124495981, 1.638662057970756925 ) ) ;
#77968 = CARTESIAN_POINT ( 'NONE',  ( 8.012505595552012139, 11.33137838057728786, -1.082531754730543083 ) ) ;
#77967 = CARTESIAN_POINT ( 'NONE',  ( 1.364683531249988535, 3.655208333674750509, -0.7879004041258239610 ) ) ;
#77970 = CARTESIAN_POINT ( 'NONE',  ( 0.1884680354247054990, -1.036234488384666586, 1.948478269905975946 ) ) ;
#77969 = CARTESIAN_POINT ( 'NONE',  ( -6.201965203247477909, 9.323044272842313518, 1.199719254218452047 ) ) ;
#77971 = CARTESIAN_POINT ( 'NONE',  ( 6.812946544903684121, -1.603000239855886466, 1.309962327488790157 ) ) ;
#77972 = CARTESIAN_POINT ( 'NONE',  ( 6.657217119509961201, 7.725507046638470321, -1.199719254218446718 ) ) ;
#77973 = CARTESIAN_POINT ( 'NONE',  ( -5.087333953625788219, 6.958308917361963886, 1.599625672291267398 ) ) ;
#77974 = CARTESIAN_POINT ( 'NONE',  ( 11.48243876534946217, 12.22000000000000064, -3.200000000000001510 ) ) ;
#77975 = CARTESIAN_POINT ( 'NONE',  ( 4.487161871577921346, 1.761403164857084702, -0.8856326919300193667 ) ) ;
#77976 = CARTESIAN_POINT ( 'NONE',  ( 0.01804983835817890528, -0.5593552815991027494, 2.045460531183339814 ) ) ;
#77977 = CARTESIAN_POINT ( 'NONE',  ( -0.7500000000000006661, 0.8895833340161543035, -1.299038105676652011 ) ) ;
#77978 = CARTESIAN_POINT ( 'NONE',  ( 4.653107873243750525, -1.855428480829583338, 1.371977642438865885 ) ) ;
#77979 = CARTESIAN_POINT ( 'NONE',  ( 1.709910653088747789, 0.6025335139634242498, -1.972566668331069195 ) ) ;
#77980 = CARTESIAN_POINT ( 'NONE',  ( 7.673551755654734130, 9.015193805427763607, -1.082531754730537976 ) ) ;
#77981 = EDGE_CURVE ( 'NONE', #89251, #22085, #101210, .T. ) ;
#77982 = CARTESIAN_POINT ( 'NONE',  ( 5.285699784481295183, 7.260012063351913625, 1.599625672291268286 ) ) ;
#77983 = CARTESIAN_POINT ( 'NONE',  ( 3.736153849017632922, 6.516540702899320081, -1.199719254218453823 ) ) ;
#77984 = CARTESIAN_POINT ( 'NONE',  ( 0.6823417656249899377, 2.155208333674753174, 1.181850606188767472 ) ) ;
#77985 = CARTESIAN_POINT ( 'NONE',  ( 5.401997860402196316, 5.267028690082820930, 0.000000000000000000 ) ) ;
#77986 = CARTESIAN_POINT ( 'NONE',  ( 6.466876083594112146, 6.647036307055676829, -0.7216878364870257245 ) ) ;
#77987 = CARTESIAN_POINT ( 'NONE',  ( 4.703694880604158968, -1.675542544088706620, -1.380765677988102791 ) ) ;
#77988 = LINE ( 'NONE', #190657, #68547 ) ;
#77990 = CARTESIAN_POINT ( 'NONE',  ( 4.370544011308346910, -0.004580445953385886559, -1.841430844414258861 ) ) ;
#77989 = CARTESIAN_POINT ( 'NONE',  ( -4.772106882330247046, 4.669805572247793357, -0.7216878364870207285 ) ) ;
#77992 = CARTESIAN_POINT ( 'NONE',  ( 6.720655732516649827, 7.053635520514346169, 2.324416633011537225 ) ) ;
#77991 = CARTESIAN_POINT ( 'NONE',  ( 1.530808498934191324E-16, 6.161115872820241535, -1.249999999999999778 ) ) ;
#77993 = CARTESIAN_POINT ( 'NONE',  ( 5.249643141573060667, 2.189086832579402842, -0.1069518675670885766 ) ) ;
#77994 = DIRECTION ( 'NONE',  ( 0.000000000000000000, 0.000000000000000000, 1.000000000000000000 ) ) ;
#77995 = CARTESIAN_POINT ( 'NONE',  ( 5.840765815766128632, 0.4347934677991367458, 2.220198762108383850 ) ) ;
#77996 = CARTESIAN_POINT ( 'NONE',  ( -4.201979666139121328, 7.560802217138083314, -0.9697280773930611053 ) ) ;
#77997 = CARTESIAN_POINT ( 'NONE',  ( -2.973958751752119767, 6.684155243576896943, 0.05118324351628460861 ) ) ;
#77998 = CARTESIAN_POINT ( 'NONE',  ( 5.126881573038487794, 7.911131357477594328, 1.221340741751137493 ) ) ;
#77999 = CARTESIAN_POINT ( 'NONE',  ( -5.614485009390564940, 5.722856397143323726, 0.000000000000000000 ) ) ;
#78000 = CARTESIAN_POINT ( 'NONE',  ( -6.734029298721184276, -7.783114986501010080, -6.778728372092619914 ) ) ;
#78001 = CARTESIAN_POINT ( 'NONE',  ( 0.3909914118310651165, 1.306912223127455919, 1.193654972778479539 ) ) ;
#78002 = CARTESIAN_POINT ( 'NONE',  ( 5.303390062791992321, 1.774253655011595709, -0.9511161165304935494 ) ) ;
#78003 = CARTESIAN_POINT ( 'NONE',  ( 7.006866460164219212, 7.069099046480051385, -0.7998128361456281477 ) ) ;
#78004 = CARTESIAN_POINT ( 'NONE',  ( 3.891714145839750838, 1.523869777361567479, 1.453819373739003051 ) ) ;
#78005 = CARTESIAN_POINT ( 'NONE',  ( 2.179167455442470480, 1.482148263166820801, 1.213602503745815353 ) ) ;
#78006 = DIRECTION ( 'NONE',  ( 0.6507913734559640506, -0.7592566023653003482, 0.000000000000000000 ) ) ;
#78007 = CARTESIAN_POINT ( 'NONE',  ( 3.473067387030086994, 1.779531822584624834, 0.8443681024216052045 ) ) ;
#78008 = CARTESIAN_POINT ( 'NONE',  ( 5.994400513263062891, -1.076938050528394308, 1.708516719617196422 ) ) ;
#78009 = CARTESIAN_POINT ( 'NONE',  ( 1.217418975555501826, -1.825842229346545498, 0.4062821374252246764 ) ) ;
#78012 = ORIENTED_EDGE ( 'NONE', *, *, #178677, .F. ) ;
#78011 = CARTESIAN_POINT ( 'NONE',  ( 1.793074957647671663, -0.09724762972821224261, -1.910064080951429100 ) ) ;
#78010 = CARTESIAN_POINT ( 'NONE',  ( 5.549328304323321248, -1.363462989569711681, -1.056374310239334591 ) ) ;
#78014 = CARTESIAN_POINT ( 'NONE',  ( 4.867013957625893283, 4.780530493426062399, 1.040834085586084257E-14 ) ) ;
#78013 = CARTESIAN_POINT ( 'NONE',  ( 1.348561525465460820, 2.204488851003219896, 0.1053889787279923829 ) ) ;
#78015 = CARTESIAN_POINT ( 'NONE',  ( -0.6823417656250003738, 2.530208333674753618, -1.181850606188749264 ) ) ;
#78016 = CARTESIAN_POINT ( 'NONE',  ( 9.237182729612253951, 9.671134694169463586, 0.7998128361456462443 ) ) ;
#78017 = CARTESIAN_POINT ( 'NONE',  ( 11.49966000274960898, 12.35767154435270498, -3.429881629453144232 ) ) ;
#78018 = CARTESIAN_POINT ( 'NONE',  ( -1.123270288250318494, 3.235197346350006331, -0.7749999999993562039 ) ) ;
#78019 = CARTESIAN_POINT ( 'NONE',  ( -0.4000000000000243916, 3.000000000000566214, -2.023857702507757317 ) ) ;
#78020 = CARTESIAN_POINT ( 'NONE',  ( 7.137427454243371550, -7.616807780282499607, 7.137427454242994074 ) ) ;
#78021 = CARTESIAN_POINT ( 'NONE',  ( 1.522023487246677798, 2.040062638832959241, -0.3519594530456415793 ) ) ;
#78023 = CARTESIAN_POINT ( 'NONE',  ( 0.7499999999999885647, 1.816666666666688634, -1.299038105676652899 ) ) ;
#78022 = VECTOR ( 'NONE', #70635, 1000.000000000000000 ) ;
#78024 = CARTESIAN_POINT ( 'NONE',  ( 4.313465427442102929, 8.184126765324453601, 0.7998128361456462443 ) ) ;
#78025 = CARTESIAN_POINT ( 'NONE',  ( -5.526920175865215334, 9.599823971818089774, 0.7998128361456481317 ) ) ;
#78026 = CARTESIAN_POINT ( 'NONE',  ( 2.878073747850912412, 6.579779482459851003, -0.7998128361456362523 ) ) ;
#78027 = CARTESIAN_POINT ( 'NONE',  ( 6.516280388114966904, -2.120036885061008292, 0.05137064186952475936 ) ) ;
#78028 = DIRECTION ( 'NONE',  ( -0.000000000000000000, -1.000000000000000000, -0.000000000000000000 ) ) ;
#78029 = ADVANCED_FACE ( 'NONE', ( #26824 ), #174181, .T. ) ;
#78030 = CARTESIAN_POINT ( 'NONE',  ( -0.6823417656250212460, 2.801041667008084879, 1.181850606188767472 ) ) ;
#78032 = CARTESIAN_POINT ( 'NONE',  ( 2.171277156482887882, 5.684907115872006145, -0.7998128361456291469 ) ) ;
#78031 = CARTESIAN_POINT ( 'NONE',  ( -0.4626273691814333788, 3.108307088186319955, -0.4053073865230780726 ) ) ;
#78033 = CARTESIAN_POINT ( 'NONE',  ( 4.763045971468515383, -2.015604388477490350, -0.05228862439247972116 ) ) ;
#78034 = CARTESIAN_POINT ( 'NONE',  ( 4.276519664212295346, -0.4255873229474533281, -1.867665486979957157 ) ) ;
#78035 = CARTESIAN_POINT ( 'NONE',  ( 0.000000000000000000, 4.000000000000003553, -11.49999999999998934 ) ) ;
#78036 = CARTESIAN_POINT ( 'NONE',  ( 2.577880719133851084, -1.123996537731044354, 1.881222605751430521 ) ) ;
#78037 = CARTESIAN_POINT ( 'NONE',  ( -1.981527703613581659, 3.480048614628247439, 0.4617793045967767407 ) ) ;
#78038 = CARTESIAN_POINT ( 'NONE',  ( -1.500000000000001332, 0.6812500006828161592, 0.000000000000000000 ) ) ;
#78039 = CARTESIAN_POINT ( 'NONE',  ( 5.062748685862976217, 0.5883423404384033883, 1.925289297555386359 ) ) ;
#78040 = CARTESIAN_POINT ( 'NONE',  ( -6.368579470117215813, 8.453095353268645695, 1.599625672291283607 ) ) ;
#78041 = EDGE_CURVE ( 'NONE', #111689, #184764, #208508, .T. ) ;
#78043 = CARTESIAN_POINT ( 'NONE',  ( 6.292584676692968948, 1.568786179414104032, -1.421969346915842092 ) ) ;
#78042 = DIRECTION ( 'NONE',  ( 0.000000000000000000, 0.000000000000000000, -1.000000000000000000 ) ) ;
#78044 = CARTESIAN_POINT ( 'NONE',  ( -0.6823417656250039265, 9.130208333674726617, -1.181850606188755259 ) ) ;
#78046 = CARTESIAN_POINT ( 'NONE',  ( -5.447343857640614573, 9.577261277214532242, -0.7998128361456362523 ) ) ;
#78045 = CARTESIAN_POINT ( 'NONE',  ( 3.632441420962172263, 0.3087965321501208726, 2.067699918487746036 ) ) ;
#78048 = ORIENTED_EDGE ( 'NONE', *, *, #208749, .F. ) ;
#78047 = CARTESIAN_POINT ( 'NONE',  ( 1.975234724782324980, 1.651647476387863467, -0.4968862749653804589 ) ) ;
#78049 = CARTESIAN_POINT ( 'NONE',  ( 4.922192346260839457, -2.110166376318895587, 0.2103620946037400852 ) ) ;
#78050 = CARTESIAN_POINT ( 'NONE',  ( 5.286789834324991055, 8.255339675766103724, -1.199719254218452935 ) ) ;
#78051 = CARTESIAN_POINT ( 'NONE',  ( 10.95308175811721085, 12.29999999999998295, 1.799999999999999600 ) ) ;
#78052 = CARTESIAN_POINT ( 'NONE',  ( -6.158835246850665884E-15, 0.8125000000000031086, 1.224999999999960565 ) ) ;
#78053 = CARTESIAN_POINT ( 'NONE',  ( 6.808607288253659462, -8.010031549403118234, -6.625366561259649956 ) ) ;
#78054 = CARTESIAN_POINT ( 'NONE',  ( 5.147291874682557555, 9.156924287104992288, 0.7998128361456462443 ) ) ;
#78055 = ORIENTED_EDGE ( 'NONE', *, *, #147413, .F. ) ;
#78056 = CARTESIAN_POINT ( 'NONE',  ( 0.000000000000000000, 0.7999999999999951594, 0.000000000000000000 ) ) ;
#78057 = VERTEX_POINT ( 'NONE', #6287 ) ;
#78058 = CARTESIAN_POINT ( 'NONE',  ( 1.945701609745503324, -1.183853311710543199, -1.371160031100856935 ) ) ;
#78060 = CARTESIAN_POINT ( 'NONE',  ( -7.230575994789712801, 7.330093503543126054, 0.7998128361456341429 ) ) ;
#78059 = CIRCLE ( 'NONE', #19130, 11.92000000000000171 ) ;
#78061 = CARTESIAN_POINT ( 'NONE',  ( 3.408985558832261731, 6.064568021024562938, 1.199719254218462483 ) ) ;
#78062 = ORIENTED_EDGE ( 'NONE', *, *, #111366, .T. ) ;
#78063 = CARTESIAN_POINT ( 'NONE',  ( 6.008198349511364000, 7.038594824965278995, 1.199719254218453823 ) ) ;
#78064 = CARTESIAN_POINT ( 'NONE',  ( 2.279683508022036342, 1.776238746767303978, -0.3545518163566608871 ) ) ;
#78065 = CARTESIAN_POINT ( 'NONE',  ( 6.539320575229274901, 7.629137130509072051, 2.496737603865983424 ) ) ;
#78066 = CARTESIAN_POINT ( 'NONE',  ( 4.124567353486244592, 7.428622122647839277, 0.6979301818166357974 ) ) ;
#78067 = CARTESIAN_POINT ( 'NONE',  ( 4.299146511743386689, -1.619905129461503224, 0.9160139579608633786 ) ) ;
#78068 = CARTESIAN_POINT ( 'NONE',  ( 1.054133004535224849, -1.214278006866207571, 1.481595424536867656 ) ) ;
#78069 = CARTESIAN_POINT ( 'NONE',  ( 0.9557436305893592943, 1.823730570757615022, -0.08488363409227267509 ) ) ;
#78070 = PLANE ( 'NONE',  #121818 ) ;
#78071 = CARTESIAN_POINT ( 'NONE',  ( 4.217276354152451390, 3.814577256132954730, 1.214306433183764966E-14 ) ) ;
#78072 = EDGE_CURVE ( 'NONE', #157226, #27240, #125579, .T. ) ;
#78073 = AXIS2_PLACEMENT_3D ( 'NONE', #111443, #75680, #45323 ) ;
#78074 = CARTESIAN_POINT ( 'NONE',  ( 4.702859892337409420, 8.240897811179339172, 0.6291740908887258898 ) ) ;
#78075 = DIRECTION ( 'NONE',  ( 0.000000000000000000, 0.000000000000000000, -1.000000000000000000 ) ) ;
#78076 = CARTESIAN_POINT ( 'NONE',  ( 8.758204044748010730, 9.320252261735261001, 0.7216878364870438212 ) ) ;
#78077 = CARTESIAN_POINT ( 'NONE',  ( 5.453942691717160507, -0.7125396638749655898, 1.836196350841996949 ) ) ;
#78078 = CARTESIAN_POINT ( 'NONE',  ( -5.576481253922474401, 5.400316305864651056, -0.7998128361456221525 ) ) ;
#78079 = CARTESIAN_POINT ( 'NONE',  ( -11.97929049433705551, 9.799999999999998934, -0.7046979865771820783 ) ) ;
#78080 = CIRCLE ( 'NONE', #105796, 10.25000000000000000 ) ;
#78081 = CARTESIAN_POINT ( 'NONE',  ( 0.3750906047784249853, 1.949931092985623726, -0.7544815049443721611 ) ) ;
#78082 = CARTESIAN_POINT ( 'NONE',  ( 8.471147050440139381, 8.777426401801974976, -0.7998128361456281477 ) ) ;
#78083 = CARTESIAN_POINT ( 'NONE',  ( 5.754890659886483739, -1.518548266084504439, 1.185242666505934572 ) ) ;
#78084 = CARTESIAN_POINT ( 'NONE',  ( -5.045605722580076780, 9.038290442985410067, -0.7998128361456231517 ) ) ;
#78085 = CARTESIAN_POINT ( 'NONE',  ( 1.781981981289095796, -0.9795585948506604357, 1.540336029244721461 ) ) ;
#78086 = CARTESIAN_POINT ( 'NONE',  ( 2.614145488985010424, -2.182733025630137824, 0.3247920039054427721 ) ) ;
#78087 = LINE ( 'NONE', #81292, #117433 ) ;
#78088 = CARTESIAN_POINT ( 'NONE',  ( 0.1406777020166137260, 1.830675540527426648, 0.5531436448603862521 ) ) ;
#78089 = CARTESIAN_POINT ( 'NONE',  ( 0.8187300819318241718, -1.428952508342665517, 1.355707701654704112 ) ) ;
#78090 = CARTESIAN_POINT ( 'NONE',  ( 2.823698466604074309, 1.076742338344888639, -1.616048498441272407 ) ) ;
#78091 = CARTESIAN_POINT ( 'NONE',  ( 0.3860920070548681804, -0.1017387759476989784, 2.013677428805898728 ) ) ;
#78093 = CARTESIAN_POINT ( 'NONE',  ( 5.928513603989616243, -1.181800583780348468, 1.437463819671711995 ) ) ;
#78092 = CARTESIAN_POINT ( 'NONE',  ( -6.306477729012051725, 7.386587434382707151, 1.199719254218452047 ) ) ;
#78094 = CARTESIAN_POINT ( 'NONE',  ( 6.222266154028957885, 6.224008365980749247, 0.7998128361456352531 ) ) ;
#78095 = CARTESIAN_POINT ( 'NONE',  ( -11.48767021851168124, 13.83004227463830738, -3.470194894594655910 ) ) ;
#78096 = CARTESIAN_POINT ( 'NONE',  ( 1.419999999999989049, 6.200000000000045475, -2.579999999999995630 ) ) ;
#78097 = CARTESIAN_POINT ( 'NONE',  ( -6.091691091241777656, 6.001394449403842479, 0.7998128361456341429 ) ) ;
#78098 = CARTESIAN_POINT ( 'NONE',  ( -5.912237504011027767, 9.055304967058290799, 1.199719254218454489 ) ) ;
#78099 = CARTESIAN_POINT ( 'NONE',  ( 1.417800074541092137, -1.221294057239637576, -1.819523406426680090 ) ) ;
#78100 = CARTESIAN_POINT ( 'NONE',  ( 4.704316114261903436, 4.590716342834741504, 1.214306433183764966E-14 ) ) ;
#78101 = DIRECTION ( 'NONE',  ( 0.000000000000000000, 1.000000000000000000, 0.000000000000000000 ) ) ;
#78102 = DIRECTION ( 'NONE',  ( -1.000000000000000000, 0.000000000000000000, 0.000000000000000000 ) ) ;
#78103 = CARTESIAN_POINT ( 'NONE',  ( 3.105874302609371362, -1.823586186413633126, 0.09019715141062728536 ) ) ;
#78104 = CARTESIAN_POINT ( 'NONE',  ( 0.4644214298828999166, 7.369507887686750358, 4.459343850248959740 ) ) ;
#78105 = CARTESIAN_POINT ( 'NONE',  ( -4.939248034080176097, 4.656877549381960080, 1.214306433183764966E-14 ) ) ;
#78106 = CARTESIAN_POINT ( 'NONE',  ( -5.058680321808019187, 7.974527835229765493, -1.188367278328520849 ) ) ;
#78107 = FACE_OUTER_BOUND ( 'NONE', #41746, .T. ) ;
#78108 = CARTESIAN_POINT ( 'NONE',  ( 9.511208455186636712, 11.05516360492796935, 1.199719254218453823 ) ) ;
#78109 = CARTESIAN_POINT ( 'NONE',  ( 1.102032671262738850, -1.926676517669764443, -0.0008590682252854196007 ) ) ;
#78110 = CARTESIAN_POINT ( 'NONE',  ( 5.840667439708360220, -1.913134005453724251, -0.4332900713753874977 ) ) ;
#78111 = CARTESIAN_POINT ( 'NONE',  ( -7.877450944739929461, 9.149113176073413456, 1.199719254218462483 ) ) ;
#78112 = CARTESIAN_POINT ( 'NONE',  ( 5.066996723205273057, 6.934582148538044777, 1.599625672291267398 ) ) ;
#78113 = CARTESIAN_POINT ( 'NONE',  ( 4.810206850810132551, 1.511280187219691928, -1.587364365194674498 ) ) ;
#78114 = CARTESIAN_POINT ( 'NONE',  ( 5.508690485854129903, 5.321227076451600091, 1.040834085586084257E-14 ) ) ;
#78115 = CARTESIAN_POINT ( 'NONE',  ( 4.557524383921963462, 1.659614545607337677, 1.237363147772299721 ) ) ;
#78117 = CARTESIAN_POINT ( 'NONE',  ( 1.364683531249986537, 1.176041667008082658, 0.7879004041258500513 ) ) ;
#78116 =( NAMED_UNIT ( * ) PLANE_ANGLE_UNIT ( ) SI_UNIT ( $, .RADIAN. ) );
#78118 = ORIENTED_EDGE ( 'NONE', *, *, #75556, .T. ) ;
#78119 = CARTESIAN_POINT ( 'NONE',  ( 4.149308075173010479, 1.083998706471595463, 2.027078093135482817 ) ) ;
#78121 = ORIENTED_EDGE ( 'NONE', *, *, #81005, .F. ) ;
#78120 = CARTESIAN_POINT ( 'NONE',  ( 6.887178846062110615, 9.058127958537705027, -1.443375672974057666 ) ) ;
#78123 = CARTESIAN_POINT ( 'NONE',  ( -3.606105671554928893, 7.150947683548683820, 0.7216878364870122908 ) ) ;
#78122 = CARTESIAN_POINT ( 'NONE',  ( 5.234856708652227297, 7.200695141551334721, 1.443375672974065660 ) ) ;
#78124 = CARTESIAN_POINT ( 'NONE',  ( 6.620655732516649294, 2.985444497229528427, 2.280274006979409407 ) ) ;
#78125 = DIRECTION ( 'NONE',  ( 0.000000000000000000, 0.000000000000000000, -1.000000000000000000 ) ) ;
#78126 = CARTESIAN_POINT ( 'NONE',  ( 4.013568362537369261, -0.9994162096361800529, -1.664904219174968114 ) ) ;
#78127 = ORIENTED_EDGE ( 'NONE', *, *, #168064, .T. ) ;
#78128 = CARTESIAN_POINT ( 'NONE',  ( 9.531018800282598846, 12.14260790512831889, 1.443375672974076540 ) ) ;
#78129 = EDGE_CURVE ( 'NONE', #55552, #182455, #142698, .T. ) ;
#78130 = ORIENTED_EDGE ( 'NONE', *, *, #137433, .T. ) ;
#78131 = CARTESIAN_POINT ( 'NONE',  ( 4.886922752366290368, -1.802716094696995786, -0.6387714794457154399 ) ) ;
#78132 = CARTESIAN_POINT ( 'NONE',  ( 0.2331713839410758105, 2.878356536703096324, -2.442089366404568640 ) ) ;
#78133 = CARTESIAN_POINT ( 'NONE',  ( 5.825168945638790063, -0.03770542841243298970, 1.724543776939557960 ) ) ;
#78134 = CARTESIAN_POINT ( 'NONE',  ( 4.452361426671761713, -1.313546101436880109, 1.530156479064001207 ) ) ;
#78135 = CARTESIAN_POINT ( 'NONE',  ( 11.48806469435255551, 12.26910227127549646, 3.468902948106700190 ) ) ;
#78136 = CARTESIAN_POINT ( 'NONE',  ( 1.928631425534212074, 1.268998755960360603, -1.805353087401928569 ) ) ;
#78137 = CARTESIAN_POINT ( 'NONE',  ( -9.829825065107822724, 11.42688298316931572, 1.199719254218462483 ) ) ;
#78139 = CARTESIAN_POINT ( 'NONE',  ( 0.3382653665467276749, 0.2958422019357190291, 1.744775138515190616 ) ) ;
#78138 = CARTESIAN_POINT ( 'NONE',  ( 1.324293675337850695, 2.015212547500934814, 0.5562262626958893730 ) ) ;
#78140 = CARTESIAN_POINT ( 'NONE',  ( 5.291638762709002464, 1.525045427759319727, -1.319226660814104335 ) ) ;
#78142 = CARTESIAN_POINT ( 'NONE',  ( 2.836170770286027043, 2.275064633363361732, 0.2797384389828549978 ) ) ;
#78141 = CARTESIAN_POINT ( 'NONE',  ( 5.357406976055401948, 6.279338222599979424, 1.199719254218452935 ) ) ;
#78143 = CARTESIAN_POINT ( 'NONE',  ( 0.5677837317836741393, -1.637140195495973671, -0.5907660828440349787 ) ) ;
#78144 = CARTESIAN_POINT ( 'NONE',  ( 6.770610912236886492, -7.154544010627095219, 6.663994888585879295 ) ) ;
#78145 = CARTESIAN_POINT ( 'NONE',  ( 1.299655142190193402, -1.570548766235444038, 0.7348691985549455907 ) ) ;
#78146 = CARTESIAN_POINT ( 'NONE',  ( 0.6801582343749970061, 0.8385416670080649837, -1.178068619123841643 ) ) ;
#78147 = LINE ( 'NONE', #62962, #135880 ) ;
#78148 = CARTESIAN_POINT ( 'NONE',  ( 1.065148145857688577, 1.644283457976392748, -1.417989991454001730 ) ) ;
#78149 = CARTESIAN_POINT ( 'NONE',  ( 2.378138974734815392, -2.011451771401792321, -0.1435188914247695346 ) ) ;
#78150 = CARTESIAN_POINT ( 'NONE',  ( 3.656250000000002665, -1.895863743164003523, 0.7852924748301777225 ) ) ;
#78151 = CARTESIAN_POINT ( 'NONE',  ( 1.499999999999987121, 1.827083334016151861, -0.8660254037844253849 ) ) ;
#78152 = CARTESIAN_POINT ( 'NONE',  ( 6.692047312239829182, -0.8199282357786542574, 1.741332009981966022 ) ) ;
#78153 = CARTESIAN_POINT ( 'NONE',  ( -1.364683531250000748, 12.35937500034139980, 0.000000000000000000 ) ) ;
#78154 = CARTESIAN_POINT ( 'NONE',  ( 3.322728300399055534, -0.9034660432867666069, -2.029577789741637162 ) ) ;
#78155 = ORIENTED_EDGE ( 'NONE', *, *, #68743, .F. ) ;
#78156 = CARTESIAN_POINT ( 'NONE',  ( -9.578284150245952588, -9.932867526282002757, 0.1622940087187730029 ) ) ;
#78157 = CARTESIAN_POINT ( 'NONE',  ( -0.7500000000000249800, -1.058333333333314030, 1.299038105676659116 ) ) ;
#78158 = CARTESIAN_POINT ( 'NONE',  ( 8.239604668803105270, 10.63595808506888396, -1.599625672291268286 ) ) ;
#78159 = FILL_AREA_STYLE ('',( #147443 ) ) ;
#78160 = CARTESIAN_POINT ( 'NONE',  ( 4.880260771415650289, -0.2196809260722985546, -1.726461634439285797 ) ) ;
#78162 = EDGE_CURVE ( 'NONE', #65102, #41277, #117020, .T. ) ;
#78161 = CARTESIAN_POINT ( 'NONE',  ( 5.055110333045015558, 1.632132345252810035, -1.088295032039228172 ) ) ;
#78164 = CARTESIAN_POINT ( 'NONE',  ( -7.049876689426121779, 7.327203680526343632, -0.7216878364870278340 ) ) ;
#78163 = CARTESIAN_POINT ( 'NONE',  ( 2.510230996824538430, 6.080353262937265413, 0.000000000000000000 ) ) ;
#78165 = DIRECTION ( 'NONE',  ( 0.000000000000000000, 1.000000000000000000, 0.000000000000000000 ) ) ;
#78166 = CARTESIAN_POINT ( 'NONE',  ( 4.376441990627045087, -1.307286168679543614, 1.846302370218126265 ) ) ;
#78167 = VECTOR ( 'NONE', #166138, 1000.000000000000000 ) ;
#78168 = CARTESIAN_POINT ( 'NONE',  ( 2.383324636069758640, -0.002395321609373335381, 2.062851379284504461 ) ) ;
#78169 = CARTESIAN_POINT ( 'NONE',  ( -6.368579470117215813, 8.453095353268645695, 1.599625672291283607 ) ) ;
#78170 = VECTOR ( 'NONE', #179365, 1000.000000000000000 ) ;
#78171 = ORIENTED_EDGE ( 'NONE', *, *, #157556, .T. ) ;
#78172 = CARTESIAN_POINT ( 'NONE',  ( 0.7499999999999885647, 1.347916667349485786, -1.299038105676652899 ) ) ;
#78173 = CARTESIAN_POINT ( 'NONE',  ( 3.163207368312019430, 0.2779861718534247794, -1.849665920529340646 ) ) ;
#78174 = CARTESIAN_POINT ( 'NONE',  ( 2.531537987306311965, -1.440582175967281886, 0.9650062983845784093 ) ) ;
#78175 = CARTESIAN_POINT ( 'NONE',  ( 6.532779862045914321, -1.958661757936002612, 0.9833580883553474372 ) ) ;
#78176 = CARTESIAN_POINT ( 'NONE',  ( 0.9036964725192305758, 1.805054822729842190, 1.269220749904229839 ) ) ;
#78177 = CARTESIAN_POINT ( 'NONE',  ( 4.504844740329728481, 1.672958716126593082, -1.369014088531981255 ) ) ;
#78178 = CARTESIAN_POINT ( 'NONE',  ( 4.400292492776470610, 1.500370014523371154, -1.232902440404326727 ) ) ;
#78179 = CARTESIAN_POINT ( 'NONE',  ( -4.433153041544240835, 4.274359424664112339, 0.7216878364870317197 ) ) ;
#78181 = UNCERTAINTY_MEASURE_WITH_UNIT (LENGTH_MEASURE( 1.000000000000000082E-05 ), #23589, 'distance_accuracy_value', 'NONE');
#78180 = DIRECTION ( 'NONE',  ( -0.6292706268317891372, -0.7771862570881751253, 0.000000000000000000 ) ) ;
#78182 =( LENGTH_UNIT ( ) NAMED_UNIT ( * ) SI_UNIT ( .MILLI., .METRE. ) );
#78183 = CARTESIAN_POINT ( 'NONE',  ( -11.33772463945036968, 19.00000000000000000, -3.680000000000002824 ) ) ;
#78185 = EDGE_CURVE ( 'NONE', #130351, #119003, #91865, .T. ) ;
#78184 =( LENGTH_UNIT ( ) NAMED_UNIT ( * ) SI_UNIT ( .MILLI., .METRE. ) );
#78186 = CARTESIAN_POINT ( 'NONE',  ( -3.189213936345670852, 2.817530495244580102, -2.450448857954567572 ) ) ;
#78187 = CARTESIAN_POINT ( 'NONE',  ( 5.432267593368638181, -1.591316862017605471, -1.238322901282742805 ) ) ;
#78188 = CARTESIAN_POINT ( 'NONE',  ( -9.154780037725563702, 11.70366268214508487, 1.599625672291281386 ) ) ;
#78189 = CARTESIAN_POINT ( 'NONE',  ( 8.229962938695207342, 9.560377169021284871, 1.199719254218462483 ) ) ;
#78190 = CARTESIAN_POINT ( 'NONE',  ( 0.000000000000000000, 0.000000000000000000, 0.000000000000000000 ) ) ;
#78191 = CARTESIAN_POINT ( 'NONE',  ( 2.877373901574116211, 1.733520850877915187, -0.5729475677913041798 ) ) ;
#78192 = CARTESIAN_POINT ( 'NONE',  ( 2.134064618640969524, -1.441378300436758630, -1.671108464803609417 ) ) ;
#78193 = VERTEX_POINT ( 'NONE', #59331 ) ;
#78194 = CARTESIAN_POINT ( 'NONE',  ( -5.600926855776901192, 5.707038551260711579, -0.7216878364870338292 ) ) ;
#78195 = CARTESIAN_POINT ( 'NONE',  ( -8.667740277838301921, 9.006785167099828016, -0.7998128361456291469 ) ) ;
#78196 = CARTESIAN_POINT ( 'NONE',  ( 0.5627676185161786249, 0.5905471060306236586, 1.931493850173772397 ) ) ;
#78197 = CARTESIAN_POINT ( 'NONE',  ( 1.172698094321134477, 0.8626872041959359194, 1.937259058979395654 ) ) ;
#78198 = DIRECTION ( 'NONE',  ( 0.000000000000000000, 0.000000000000000000, -1.000000000000000000 ) ) ;
#78199 = VERTEX_POINT ( 'NONE', #158973 ) ;
#78200 = CARTESIAN_POINT ( 'NONE',  ( -3.949167883330528372, 7.829389307186077396, 1.214306433183764966E-14 ) ) ;
#78201 = CARTESIAN_POINT ( 'NONE',  ( 2.272090887488043887, -0.8719313595505603365, -1.644003247725301264 ) ) ;
#78202 = CARTESIAN_POINT ( 'NONE',  ( 3.493197133815315603, 7.227147089426516402, -0.7998128361456291469 ) ) ;
#78203 = CARTESIAN_POINT ( 'NONE',  ( 0.2511322555047851290, -1.735185354305257110, 1.289038484408123963 ) ) ;
#78204 = CARTESIAN_POINT ( 'NONE',  ( 6.170546107226446253, 1.392543322632183722, 1.458558933167881211 ) ) ;
#78205 = EDGE_LOOP ( 'NONE', ( #187012, #126050, #163494, #202659 ) ) ;
#78206 = ORIENTED_EDGE ( 'NONE', *, *, #142525, .F. ) ;
#78207 = CARTESIAN_POINT ( 'NONE',  ( -8.435144125996554720, 12.99275191363802229, 0.7998128361456341429 ) ) ;
#78208 = CARTESIAN_POINT ( 'NONE',  ( 3.492628380820805400, -0.3572889717703279788, -1.790209119249221548 ) ) ;
#78209 = CIRCLE ( 'NONE', #109360, 1.500000000000000222 ) ;
#78211 = CARTESIAN_POINT ( 'NONE',  ( -5.176859992674639699, 6.655076503622660233, -1.423794717725470171 ) ) ;
#78210 = CARTESIAN_POINT ( 'NONE',  ( -5.815521545619021460, 5.749472989502435460, -0.7998128361456362523 ) ) ;
#78212 = CARTESIAN_POINT ( 'NONE',  ( 5.602183562003149042, 7.492195738860313092, 1.335281325244306982 ) ) ;
#78213 = B_SPLINE_CURVE_WITH_KNOTS ( 'NONE', 3,
 ( #174505, #200808, #185640, #102268 ),
 .UNSPECIFIED., .F., .F.,
 ( 4, 4 ),
 ( 0.000000000000000000, 0.0007699926951938504535 ),
 .UNSPECIFIED. ) ;
#78214 = CARTESIAN_POINT ( 'NONE',  ( 6.643907658006512840, -0.09612306880287316280, -2.013924184692199137 ) ) ;
#78215 = CARTESIAN_POINT ( 'NONE',  ( 6.298766309436587996, 1.533505995929709487, 1.018591839899836371 ) ) ;
#78216 = CARTESIAN_POINT ( 'NONE',  ( 0.07700591528349547132, 1.369316849116916091, -2.165014180211277228 ) ) ;
#78217 = CARTESIAN_POINT ( 'NONE',  ( 4.354349988907435964, 2.307223249097400064, -0.05412331456603951957 ) ) ;
#78218 = CARTESIAN_POINT ( 'NONE',  ( 5.448397627845284141, 7.449826213943242514, 1.599625672291268286 ) ) ;
#78219 = CARTESIAN_POINT ( 'NONE',  ( 5.852838158510675015, -1.708014377640250991, 1.324763891615586386 ) ) ;
#78220 = CARTESIAN_POINT ( 'NONE',  ( 5.445571254183207088, 9.504916896522420444, -0.7998128361456281477 ) ) ;
#78221 = CARTESIAN_POINT ( 'NONE',  ( 2.577597507962032353, -0.9963960007246205342, 1.666827093504752222 ) ) ;
#78222 = ORIENTED_EDGE ( 'NONE', *, *, #126323, .F. ) ;
#78223 = CARTESIAN_POINT ( 'NONE',  ( 4.833568131691490244, -1.505864581002622105, 1.736428821378619647 ) ) ;
#78224 = CARTESIAN_POINT ( 'NONE',  ( 0.07536363704235826688, -0.001874865094115066300, -2.144269471569634877 ) ) ;
#78225 = CARTESIAN_POINT ( 'NONE',  ( -3.923105346307911745, 5.670318552149568703, -1.599625672291283607 ) ) ;
#78226 = CARTESIAN_POINT ( 'NONE',  ( 4.908994958506140982, 1.627828031611065152, 0.9215782234750914403 ) ) ;
#78227 = ORIENTED_EDGE ( 'NONE', *, *, #155474, .T. ) ;
#78230 = CARTESIAN_POINT ( 'NONE',  ( -6.473091995881817162, 6.516638514809040217, 0.7998128361456281477 ) ) ;
#78229 = CARTESIAN_POINT ( 'NONE',  ( 0.7499999999999867883, 0.09791666734948467621, -1.299038105676652899 ) ) ;
#78228 = CARTESIAN_POINT ( 'NONE',  ( 2.004032382285144021, -0.8144628449315849394, 1.730399521388835460 ) ) ;
#78231 = CARTESIAN_POINT ( 'NONE',  ( 4.160898416275903067, -1.636102012888400292, 1.481223685352812680 ) ) ;
#78232 = CARTESIAN_POINT ( 'NONE',  ( -4.157718419935214627, 7.512196061762048238, 0.8120497619437796466 ) ) ;
#78233 = CARTESIAN_POINT ( 'NONE',  ( 3.673896439178918172, 6.269667698141953238, 1.082531754730558626 ) ) ;
#78234 = CARTESIAN_POINT ( 'NONE',  ( 5.194182247366861738, 9.073980031987776584, 0.7216878364870317197 ) ) ;
#78235 = AXIS2_PLACEMENT_3D ( 'NONE', #150309, #1875, #164412 ) ;
#78236 = CARTESIAN_POINT ( 'NONE',  ( -6.766928066552171828, 7.067373297165212342, 0.7216878364870317197 ) ) ;
#78237 = CARTESIAN_POINT ( 'NONE',  ( 1.546097919708361079, 1.968910558940571320, 0.1009371868440200049 ) ) ;
#78238 = CARTESIAN_POINT ( 'NONE',  ( 1.659631924955577098, -1.980043282969433882, -1.184870857304116898 ) ) ;
#78239 = CARTESIAN_POINT ( 'NONE',  ( 2.453501617077270769, 1.514643136537169310, 1.246875331876770243 ) ) ;
#78240 = CARTESIAN_POINT ( 'NONE',  ( -4.437261413422502798, 8.398831758960053406, 0.000000000000000000 ) ) ;
#78241 = CARTESIAN_POINT ( 'NONE',  ( 5.049704294756152123, 1.524832160660544611, 1.389060530156678297 ) ) ;
#78242 = CARTESIAN_POINT ( 'NONE',  ( 4.202664430556254160, 5.926194473780837413, 1.443375672974062551 ) ) ;
#78243 = CARTESIAN_POINT ( 'NONE',  ( 5.041653019435334393, 6.975290837464928728, -1.599625672291269396 ) ) ;
#78244 = ORIENTED_EDGE ( 'NONE', *, *, #85559, .F. ) ;
#78245 = CARTESIAN_POINT ( 'NONE',  ( -1.115562610750309283E-14, 10.06250000000000000, 1.500000000000001554 ) ) ;
#78246 = DIRECTION ( 'NONE',  ( 1.000000000000000000, 0.000000000000000000, 0.000000000000000000 ) ) ;
#78247 = CARTESIAN_POINT ( 'NONE',  ( 9.103410076571945453, 12.70806329172093818, 1.199719254218450271 ) ) ;
#78248 = CARTESIAN_POINT ( 'NONE',  ( 1.850661656762859542, -2.160338676232275823, -0.2159047328044171599 ) ) ;
#78249 = CARTESIAN_POINT ( 'NONE',  ( 6.527324610336439292, 6.579909898339485252, 0.7998128361456332547 ) ) ;
#78250 = DIRECTION ( 'NONE',  ( 0.000000000000000000, 0.000000000000000000, 1.000000000000000000 ) ) ;
#78251 = CARTESIAN_POINT ( 'NONE',  ( -10.45358220256320436, 1.000000000000000888, 5.892590188894342162 ) ) ;
#78252 = CARTESIAN_POINT ( 'NONE',  ( 2.706148147531197701, -0.7121320899835179574, -1.729884524348634933 ) ) ;
#78253 = CARTESIAN_POINT ( 'NONE',  ( 6.415313282229532454, -0.2716245656670859820, 2.144420208805633887 ) ) ;
#78255 = CARTESIAN_POINT ( 'NONE',  ( 6.827182134110209688, 6.038954451951505042, 2.405852596708078384 ) ) ;
#78254 = CARTESIAN_POINT ( 'NONE',  ( 6.670655732516623360, 7.629137130509072051, 2.773739711112707784 ) ) ;
#78256 = CARTESIAN_POINT ( 'NONE',  ( -1.364683531250000748, -0.7406249996585803075, 0.000000000000000000 ) ) ;
#78257 = CARTESIAN_POINT ( 'NONE',  ( 2.648957786072099641, 0.2360777847093403214, 1.897596177352772306 ) ) ;
#78258 = CARTESIAN_POINT ( 'NONE',  ( 4.522157790900214636, 1.087963700580677484, -1.395837783952274647 ) ) ;
#78259 = CARTESIAN_POINT ( 'NONE',  ( 1.559083858985313542, -1.614856622157490929, 1.023943737511850083 ) ) ;
#78260 = CARTESIAN_POINT ( 'NONE',  ( -6.240830780992103755, 6.175390754112560110, 1.040834085586084257E-14 ) ) ;
#78262 = CARTESIAN_POINT ( 'NONE',  ( 5.237857731762096236, 1.913213232725724966, -0.09853679971996709419 ) ) ;
#78261 = CARTESIAN_POINT ( 'NONE',  ( 7.548736457555743407, -7.034525084975653542, -7.548736457552916335 ) ) ;
#78263 = CARTESIAN_POINT ( 'NONE',  ( 1.499999999999987566, -0.2249999999999821587, 0.000000000000000000 ) ) ;
#78264 = CARTESIAN_POINT ( 'NONE',  ( 6.672316266636414639, -0.9270569987065898632, -1.737699753229291710 ) ) ;
#78265 = CARTESIAN_POINT ( 'NONE',  ( 1.499999999999990896, 5.525000000000022560, 1.214306433183764966E-14 ) ) ;
#78266 = CARTESIAN_POINT ( 'NONE',  ( 5.418772907935071714, 1.728844841293469159, 0.7149302089985640762 ) ) ;
#78267 = CARTESIAN_POINT ( 'NONE',  ( 1.277666653898035021, 1.085793613588705853, 1.467558327050644484 ) ) ;
#78269 = CARTESIAN_POINT ( 'NONE',  ( 4.625518323863472503, 8.335144253906971556, 0.3473850511846506839 ) ) ;
#78268 = CARTESIAN_POINT ( 'NONE',  ( 4.951907052881864502, 0.6945806438464275923, -2.094803410698709900 ) ) ;
#78270 = CARTESIAN_POINT ( 'NONE',  ( 1.364683531249986537, -0.6364583329919177856, 0.7879004041258500513 ) ) ;
#78271 = CARTESIAN_POINT ( 'NONE',  ( 2.453648911872767346, 1.593012163857405961, 1.310297011819524293 ) ) ;
#78272 = CARTESIAN_POINT ( 'NONE',  ( -7.167456763118792651, 11.51378332361394818, 0.000000000000000000 ) ) ;
#78273 = CARTESIAN_POINT ( 'NONE',  ( -6.661184041420952440, -7.473374494058216300, 6.773376349083140013 ) ) ;
#78274 = CARTESIAN_POINT ( 'NONE',  ( 1.495015925693002234, 3.364811783656424637, 0.1395187543289240772 ) ) ;
#78275 = CARTESIAN_POINT ( 'NONE',  ( -1.734723475976807094E-15, -9.911192131523236526, -10.91970695577494332 ) ) ;
#78276 = CARTESIAN_POINT ( 'NONE',  ( 7.126746022638799971, 8.343567110280638133, 1.199719254218452047 ) ) ;
#78277 = VERTEX_POINT ( 'NONE', #10568 ) ;
#78278 = CARTESIAN_POINT ( 'NONE',  ( 5.230950013807261101, -1.948248037745937022, -0.7008574099531189594 ) ) ;
#78279 = CARTESIAN_POINT ( 'NONE',  ( -0.6823417656250246877, 0.6135416670080897639, 1.181850606188755259 ) ) ;
#78280 = CARTESIAN_POINT ( 'NONE',  ( 2.671339989782473001, 0.1089736159370843782, -2.158987078831893669 ) ) ;
#78281 = CARTESIAN_POINT ( 'NONE',  ( -4.624779211906307808, 8.357533986720639518, 0.2900094174717957607 ) ) ;
#78282 = CARTESIAN_POINT ( 'NONE',  ( 3.317061382196756281, 1.590690956008104395, -1.244364558649863728 ) ) ;
#78283 = CARTESIAN_POINT ( 'NONE',  ( 6.720655732516647163, -0.004400176169771369272, 2.173773060281408931 ) ) ;
#78284 = PRODUCT_DEFINITION_SHAPE ( 'NONE', 'NONE',  #214423 ) ;
#78286 = CARTESIAN_POINT ( 'NONE',  ( 8.270110514656037637, 8.750809809961280550, 0.7216878364870458196 ) ) ;
#78285 = CARTESIAN_POINT ( 'NONE',  ( -1.737499999999997824, -2.041666666666667407, 3.009438278150925683 ) ) ;
#78287 = CARTESIAN_POINT ( 'NONE',  ( -4.136646265500970365, 5.919449624541475607, -1.443375672974066548 ) ) ;
#78288 = CARTESIAN_POINT ( 'NONE',  ( 1.710173085450257924, 1.157096902994741772, -1.651345047625000007 ) ) ;
#78289 = CARTESIAN_POINT ( 'NONE',  ( 6.216381822182692751, 2.044192415450503120, 0.7905562269360305594 ) ) ;
#78291 = COLOUR_RGB ( '', 0.40784314, 0.44705882, 0.49803922) ;
#78290 = CARTESIAN_POINT ( 'NONE',  ( 1.499999999999989120, 4.327083334016148086, -0.8660254037844323793 ) ) ;
#78292 = CARTESIAN_POINT ( 'NONE',  ( 4.851772015791367743, -1.356534033432246211, -1.348250844427544282 ) ) ;
#78293 = CARTESIAN_POINT ( 'NONE',  ( -3.066115294984855133, 6.728884944124295053, 0.7998128361456341429 ) ) ;
#78294 = ADVANCED_FACE ( 'NONE', ( #72361 ), #192801, .T. ) ;
#78295 = CARTESIAN_POINT ( 'NONE',  ( 6.656690234185433042, 7.828855363713562276, -1.082531754730543971 ) ) ;
#78297 = CARTESIAN_POINT ( 'NONE',  ( 2.864861414439429321, -0.1511590275467006306, -2.010826137130202529 ) ) ;
#78296 = CARTESIAN_POINT ( 'NONE',  ( -9.205623113554631587, 11.76297960394566466, 1.443375672974076540 ) ) ;
#78298 = CARTESIAN_POINT ( 'NONE',  ( -1.402160292154681736E-14, 13.23437500034139980, 1.575800808251682339 ) ) ;
#78299 = CARTESIAN_POINT ( 'NONE',  ( -4.248501033035892327, 6.049946853332221153, -1.599625672291271394 ) ) ;
#78300 = CARTESIAN_POINT ( 'NONE',  ( 4.770341545797544214, -1.125046721222152213, 1.307389476665332895 ) ) ;
#78301 = CARTESIAN_POINT ( 'NONE',  ( 5.501576472095266901, 9.640532660744973725, -0.7998128361456481317 ) ) ;
#78302 = CARTESIAN_POINT ( 'NONE',  ( 10.56143847536557878, 11.42402576412244386, 0.000000000000000000 ) ) ;
#78303 = CARTESIAN_POINT ( 'NONE',  ( 1.500000000000005329, 4.754166666666690411, 0.8660254037844431485 ) ) ;
#78304 =( BOUNDED_CURVE ( )  B_SPLINE_CURVE ( 2, ( #160509, #192991, #77115, #80321, #96603 ),
 .UNSPECIFIED., .F., .T. ) 
 B_SPLINE_CURVE_WITH_KNOTS ( ( 3, 2, 3 ),
 ( 0.2225013972065820467, 0.2250000000000000056, 0.2278796248419688031 ),
 .UNSPECIFIED. ) 
 CURVE ( )  GEOMETRIC_REPRESENTATION_ITEM ( )  RATIONAL_B_SPLINE_CURVE ( ( 0.9437486473799283626, 0.9598300839578506327, 1.000000000000000000, 0.9537044109453918228, 0.9394041646864383921 ) ) 
 REPRESENTATION_ITEM ( '' )  );
#78305 = CARTESIAN_POINT ( 'NONE',  ( 11.97929049433705373, 9.719999999999998863, -0.7046979865771834106 ) ) ;
#78306 = CARTESIAN_POINT ( 'NONE',  ( 0.5849358142855851650, 1.980036476162419845, 0.6043757699017646701 ) ) ;
#78307 = CARTESIAN_POINT ( 'NONE',  ( 0.03952929641551738982, -5.422159130394859972, 11.00000000000004974 ) ) ;
#78308 = ORIENTED_EDGE ( 'NONE', *, *, #28350, .T. ) ;
#78309 = CARTESIAN_POINT ( 'NONE',  ( 5.338451399618321602, 1.074232541698511900, -1.458426962581545361 ) ) ;
#78310 = CARTESIAN_POINT ( 'NONE',  ( 6.150558962454855561, 7.204682206732687000, 1.199719254218452047 ) ) ;
#78311 = CARTESIAN_POINT ( 'NONE',  ( -1.872228381520320672, 3.299999999999962519, 0.3999999999999628852 ) ) ;
#78312 = CARTESIAN_POINT ( 'NONE',  ( 5.865820270629499511, 0.5193939906856791522, -1.735422816724658146 ) ) ;
#78313 = CARTESIAN_POINT ( 'NONE',  ( 5.356880090730872013, 6.382686539675070492, 1.082531754730549078 ) ) ;
#78314 = CARTESIAN_POINT ( 'NONE',  ( 9.980677382359758099, 11.54895643263491145, -6.667707585166605888 ) ) ;
#78315 = CARTESIAN_POINT ( 'NONE',  ( 2.818527994553555516, 2.063739945100159900, 0.7375456357434084786 ) ) ;
#78316 = VERTEX_POINT ( 'NONE', #163493 ) ;
#78317 = EDGE_CURVE ( 'NONE', #98551, #97523, #51874, .T. ) ;
#78319 = CARTESIAN_POINT ( 'NONE',  ( 7.242026607993941489, 11.60078147596829901, 0.7998128361456462443 ) ) ;
#78318 = CARTESIAN_POINT ( 'NONE',  ( 0.3792546940144908563, -0.1001052471676349837, 1.959448305358338693 ) ) ;
#78320 = CARTESIAN_POINT ( 'NONE',  ( 5.378507874412199463, -0.4701315380702688618, -1.856876755957288516 ) ) ;
#78321 = DIRECTION ( 'NONE',  ( 0.7592566023653005702, -0.6507913734559639396, 0.000000000000000000 ) ) ;
#78322 = CARTESIAN_POINT ( 'NONE',  ( -6.501436840734760914, 6.757938919538193367, -0.04654198066046839888 ) ) ;
#78323 = ADVANCED_FACE ( 'NONE', ( #149364 ), #22624, .T. ) ;
#78324 = AXIS2_PLACEMENT_3D ( 'NONE', #198763, #183597, #118669 ) ;
#78325 = FILL_AREA_STYLE_COLOUR ( '', #184839 ) ;
#78326 = CARTESIAN_POINT ( 'NONE',  ( -1.402160292154681736E-14, -0.5531249996585814177, -1.575800808251665908 ) ) ;
#78328 = ORIENTED_EDGE ( 'NONE', *, *, #6305, .F. ) ;
#78327 = CARTESIAN_POINT ( 'NONE',  ( 4.690757960648221037, 7.456006139856155457, 1.082531754730558626 ) ) ;
#78329 = CARTESIAN_POINT ( 'NONE',  ( -8.514157279702027736, 10.95626946445095307, -1.443375672974059665 ) ) ;
#78330 = CARTESIAN_POINT ( 'NONE',  ( 1.797963993548271411, -0.7283430984801853025, 2.035426966748521860 ) ) ;
#78331 = CARTESIAN_POINT ( 'NONE',  ( -5.320648938720212051, 5.172121614787156929, 0.000000000000000000 ) ) ;
#78332 = CARTESIAN_POINT ( 'NONE',  ( 5.885648082108177803, 9.880690172519326353, 0.7216878364870317197 ) ) ;
#78333 = CARTESIAN_POINT ( 'NONE',  ( 2.045663570152244315, 0.7015605659913305425, -1.685594894050304493 ) ) ;
#78334 = CARTESIAN_POINT ( 'NONE',  ( -3.195971524519394702, 4.751719416737803847, -1.599625672291262513 ) ) ;
#78335 = CARTESIAN_POINT ( 'NONE',  ( 4.155160913615768337, -1.517764731708035386, -1.014145119915064841 ) ) ;
#78336 = CARTESIAN_POINT ( 'NONE',  ( 8.726851280726220850, 11.84099526508991218, 8.258125689521147450 ) ) ;
#78337 = ORIENTED_EDGE ( 'NONE', *, *, #10652, .F. ) ;
#78338 = CARTESIAN_POINT ( 'NONE',  ( 4.000420421810535032, 1.959860935258441517, 0.1952677912114946512 ) ) ;
#78339 = VERTEX_POINT ( 'NONE', #119058 ) ;
#78340 = CARTESIAN_POINT ( 'NONE',  ( 5.882362869737407074, -0.2893225776206589384, -1.920288418758001159 ) ) ;
#78341 = ORIENTED_EDGE ( 'NONE', *, *, #72882, .T. ) ;
#78342 = CARTESIAN_POINT ( 'NONE',  ( -4.762657100150483380, 8.778460060142702304, 0.000000000000000000 ) ) ;
#78344 = CARTESIAN_POINT ( 'NONE',  ( 5.906510592826289319, -2.110524776404258507, -0.2060971850248518311 ) ) ;
#78343 = CARTESIAN_POINT ( 'NONE',  ( -4.827585214917754719, 7.789877296449459365, -1.199719254218453823 ) ) ;
#78345 = CARTESIAN_POINT ( 'NONE',  ( 6.577113915960825175, 8.766661883411348555, -1.443375672974078761 ) ) ;
#78346 = CARTESIAN_POINT ( 'NONE',  ( 3.721269560815092525, 1.641568950759502377, 0.9805937191851579193 ) ) ;
#78347 = CARTESIAN_POINT ( 'NONE',  ( 5.302928268938337020, 6.565392180301311775, -1.356678214699511775 ) ) ;
#78348 = CARTESIAN_POINT ( 'NONE',  ( 0.000000000000000000, 9.719999999999998863, 0.000000000000000000 ) ) ;
#78349 = CARTESIAN_POINT ( 'NONE',  ( 0.1127427399064059588, -0.9454589178800475446, -1.991880357201977425 ) ) ;
#78350 = CARTESIAN_POINT ( 'NONE',  ( 5.602202738069384402, -0.9032165795441854383, 1.799149290095316767 ) ) ;
#78351 = CARTESIAN_POINT ( 'NONE',  ( 0.08676667164121812381, -9.915770458193639669, 9.499603944220597285 ) ) ;
#78352 = CARTESIAN_POINT ( 'NONE',  ( 5.813091150998386247, 1.612263477354998864, 0.8566026058636074803 ) ) ;
#78353 = CARTESIAN_POINT ( 'NONE',  ( 0.8892259839063383353, 0.1505779921940515187, 2.064926437897919964 ) ) ;
#78354 = CARTESIAN_POINT ( 'NONE',  ( -8.242994207428740339, 9.679543332497402730, 1.082531754730558626 ) ) ;
#78355 = AXIS2_PLACEMENT_3D ( 'NONE', #211494, #13306, #79379 ) ;
#78356 =( BOUNDED_CURVE ( )  B_SPLINE_CURVE ( 3, ( #155970, #123558, #205764, #41168 ),
 .UNSPECIFIED., .F., .T. ) 
 B_SPLINE_CURVE_WITH_KNOTS ( ( 4, 4 ),
 ( 4.845169979278624695, 4.852380668139161912 ),
 .UNSPECIFIED. ) 
 CURVE ( )  GEOMETRIC_REPRESENTATION_ITEM ( )  RATIONAL_B_SPLINE_CURVE ( ( 1.000000000000000000, 0.9999956671685397147, 0.9999956671685397147, 1.000000000000000000 ) ) 
 REPRESENTATION_ITEM ( '' )  );
#78357 = CARTESIAN_POINT ( 'NONE',  ( -6.444026653998019327, 6.794751805161505231, -0.4079633569072909638 ) ) ;
#78358 = CARTESIAN_POINT ( 'NONE',  ( -1.225000000000038058, 2.083333334016205907, 0.7072540797572697269 ) ) ;
#78359 = CARTESIAN_POINT ( 'NONE',  ( -1.642778471874998480, -2.851041666188706802, 2.845375778867863303 ) ) ;
#78360 = CARTESIAN_POINT ( 'NONE',  ( 6.124532705071213279, 8.168374127381657246, -1.599625672291262513 ) ) ;
#78361 = CARTESIAN_POINT ( 'NONE',  ( -3.086452525405351643, 6.752611712948207057, 0.7998128361456341429 ) ) ;
#78362 = CIRCLE ( 'NONE', #130404, 11.09999999999999964 ) ;
#78363 = CARTESIAN_POINT ( 'NONE',  ( 3.623053363349855172, 5.249981562040033189, 1.599625672291267398 ) ) ;
#78364 = CARTESIAN_POINT ( 'NONE',  ( 1.364683531249997417, 11.29687500034139802, 2.602085213965210642E-15 ) ) ;
#78365 = CARTESIAN_POINT ( 'NONE',  ( -4.273844736805832767, 6.009238164405336313, 1.599625672291267398 ) ) ;
#78367 = CARTESIAN_POINT ( 'NONE',  ( -7.781453819600577582, 8.043060642480948985, 0.000000000000000000 ) ) ;
#78366 = CARTESIAN_POINT ( 'NONE',  ( -11.95359438121989371, 11.10421899708699733, -1.059536798430483984 ) ) ;
#78368 = CARTESIAN_POINT ( 'NONE',  ( 3.639074924717408788, 0.6284830325712500443, 1.616442243290783232 ) ) ;
#78369 = CARTESIAN_POINT ( 'NONE',  ( -4.497554271431319250, 6.270232621468402989, -1.599625672291256295 ) ) ;
#78370 = CARTESIAN_POINT ( 'NONE',  ( 1.252880909328604186, -0.4992908342843911940, -2.009044966204868388 ) ) ;
#78371 = CARTESIAN_POINT ( 'NONE',  ( 2.548581339128490608, -1.457745987184940306, 1.535692819318078550 ) ) ;
#78372 = CARTESIAN_POINT ( 'NONE',  ( 5.691725559638619814, 5.534767995866836543, 1.040834085586084257E-14 ) ) ;
#78373 = CARTESIAN_POINT ( 'NONE',  ( 7.456094412511537151, 10.78619501698377370, 1.199719254218460707 ) ) ;
#78374 = CARTESIAN_POINT ( 'NONE',  ( 0.3782569160206556425, 3.049340702855431129, 0.4285286083245459787 ) ) ;
#78375 = CARTESIAN_POINT ( 'NONE',  ( 0.7253723109368491739, 0.1984653623241394993, -1.959446941136263831 ) ) ;
#78376 = CARTESIAN_POINT ( 'NONE',  ( 4.972575192752072937, 6.823350471033509557, 1.425105271486303282 ) ) ;
#78377 = CARTESIAN_POINT ( 'NONE',  ( 3.714570900464269076, 7.277490450609545469, 0.7216878364870298324 ) ) ;
#78379 = CARTESIAN_POINT ( 'NONE',  ( 0.000000000000000000, 0.000000000000000000, -0.5000000000000004441 ) ) ;
#78378 = CARTESIAN_POINT ( 'NONE',  ( -3.475000000000000533, -1.429166666666668251, -2.006292185433948827 ) ) ;
#78380 = CARTESIAN_POINT ( 'NONE',  ( 2.519810532312277473, -1.321113963755312870, -1.873090484924363697 ) ) ;
#78381 = CARTESIAN_POINT ( 'NONE',  ( 0.9436603434208358232, 0.7422609627109194586, -1.668170528445270140 ) ) ;
#78382 = CARTESIAN_POINT ( 'NONE',  ( 3.234525475359388391, 1.209690070866603406, -1.481213593849866950 ) ) ;
#78383 = MECHANICAL_DESIGN_GEOMETRIC_PRESENTATION_REPRESENTATION (  '', ( #47337 ), #185664 ) ;
#78384 = CARTESIAN_POINT ( 'NONE',  ( 6.692885107001518286, 7.837396042037102717, -1.199719254218452047 ) ) ;
#78385 = CARTESIAN_POINT ( 'NONE',  ( 5.273758565591489145, 9.096542726591325234, -0.7216878364870267237 ) ) ;
#78386 = CARTESIAN_POINT ( 'NONE',  ( -8.507905087775398556, 9.884643009614800135, 1.199719254218462483 ) ) ;
#78387 = CARTESIAN_POINT ( 'NONE',  ( 2.092043371607322566, 1.241737408274107501, 1.584530653180368009 ) ) ;
#78388 = CARTESIAN_POINT ( 'NONE',  ( 1.780054392102415672, -1.085390340960286082, -1.633940563308281968 ) ) ;
#78389 = CARTESIAN_POINT ( 'NONE',  ( -8.971744963941075568, 11.49012176272984931, 1.599625672291269396 ) ) ;
#78390 = CARTESIAN_POINT ( 'NONE',  ( -8.227100285394159940, 8.492705175914988303, 0.7998128361456602331 ) ) ;
#78391 = CARTESIAN_POINT ( 'NONE',  ( -7.552496594302674282, -5.254973434576990954, -7.962224162659105708 ) ) ;
#78393 = CARTESIAN_POINT ( 'NONE',  ( 3.537761123354207893, 0.7962651652904990662, -1.580685414113996545 ) ) ;
#78392 = CARTESIAN_POINT ( 'NONE',  ( 4.857415893618338032, 2.067970888898474247, -0.3061586078061846461 ) ) ;
#78394 = CARTESIAN_POINT ( 'NONE',  ( 1.050790385995002740, 15.00000000000000355, 12.64745918785790302 ) ) ;
#78396 = CARTESIAN_POINT ( 'NONE',  ( 6.703114550498504798, -0.5130225571751775293, 2.242675272849779411 ) ) ;
#78395 = CARTESIAN_POINT ( 'NONE',  ( 1.499999999998266054, 8.673756432004708472, -2.614717076620979963 ) ) ;
#78397 = CARTESIAN_POINT ( 'NONE',  ( 4.488070181461626618, -0.3849740463353290010, -1.697036094149968255 ) ) ;
#78398 = CARTESIAN_POINT ( 'NONE',  ( 8.055515824813896941, 12.54985222892493368, 0.7998128361456462443 ) ) ;
#78399 = CARTESIAN_POINT ( 'NONE',  ( -7.221001870987141302, -6.414086731524416329, 6.604641253243925370 ) ) ;
#78400 = CARTESIAN_POINT ( 'NONE',  ( 4.622224120573574346, 0.3796314994632241646, -1.691551752166654543 ) ) ;
#78401 = CARTESIAN_POINT ( 'NONE',  ( 4.281792510435393773, -2.078899500905183828, 0.6263114880437108400 ) ) ;
#78402 = CARTESIAN_POINT ( 'NONE',  ( 4.695201269034174452, 4.372156323494968966, 1.214306433183764966E-14 ) ) ;
#78403 = CARTESIAN_POINT ( 'NONE',  ( 0.1283146926199127957, 2.112135570198115708, 0.1490006669643220705 ) ) ;
#78404 = CARTESIAN_POINT ( 'NONE',  ( 6.281249999999699796, 0.7852924748228357066, 1.895863743163936022 ) ) ;
#78405 = CARTESIAN_POINT ( 'NONE',  ( 1.499999999999991118, 5.285416667349480235, 0.8660254037844524744 ) ) ;
#78406 = CARTESIAN_POINT ( 'NONE',  ( 3.627879330711426320, -1.146429500678107116, -1.547990911671823566 ) ) ;
#78407 = CARTESIAN_POINT ( 'NONE',  ( 0.7500000000000006661, 9.864583334016129967, 1.299038105676657340 ) ) ;
#78408 = CARTESIAN_POINT ( 'NONE',  ( 0.3818600843802121836, 0.2116341679995105141, -2.211193375792892546 ) ) ;
#78409 = ORIENTED_EDGE ( 'NONE', *, *, #81748, .F. ) ;
#78410 = CARTESIAN_POINT ( 'NONE',  ( 6.983263157960404754, 7.052265632007776119, 2.644342174942279744 ) ) ;
#78411 = CARTESIAN_POINT ( 'NONE',  ( -1.201851678989727383E-14, 3.087500000000026112, -1.732050807568863648 ) ) ;
#78412 = CARTESIAN_POINT ( 'NONE',  ( 5.473741331615251227, 7.409117525016355010, -1.599625672291262513 ) ) ;
#78413 = CARTESIAN_POINT ( 'NONE',  ( 2.245073739244434208, 2.155446677131687139, 0.5364521487482876161 ) ) ;
#78415 = EDGE_CURVE ( 'NONE', #14287, #169596, #42502, .T. ) ;
#78414 = DIRECTION ( 'NONE',  ( 0.000000000000000000, 1.000000000000000000, 0.000000000000000000 ) ) ;
#78416 = CARTESIAN_POINT ( 'NONE',  ( 6.480434237652121787, 9.543961796360731498, 1.082531754730558626 ) ) ;
#78417 = CARTESIAN_POINT ( 'NONE',  ( 1.836970198721030181E-16, 13.49999999999999822, 1.500000000000000222 ) ) ;
#78418 = CARTESIAN_POINT ( 'NONE',  ( 3.217027588192558074, 6.975225629525113824, -1.734723475976807094E-15 ) ) ;
#78419 = CARTESIAN_POINT ( 'NONE',  ( 0.5631252389872200004, -1.117830369828230808, 1.678006741548984770 ) ) ;
#78421 = CARTESIAN_POINT ( 'NONE',  ( 6.057095868330090838, 1.688466812627244185, -1.184547966247089912 ) ) ;
#78420 = CARTESIAN_POINT ( 'NONE',  ( 9.077347539549325717, 10.54899253668443393, -1.199719254218446718 ) ) ;
#78422 = CARTESIAN_POINT ( 'NONE',  ( -1.499999999999997780, 5.400000000000022560, 1.214306433183764966E-14 ) ) ;
#78423 = CARTESIAN_POINT ( 'NONE',  ( -3.228813138348844536, 6.918699094715619502, 0.7998128361456341429 ) ) ;
#78424 = CARTESIAN_POINT ( 'NONE',  ( 0.7499999999999920064, 5.014583334016150751, 1.299038105676669330 ) ) ;
#78425 = CARTESIAN_POINT ( 'NONE',  ( 0.6823417656249882723, 1.676041667008083769, -1.181850606188749264 ) ) ;
#78426 = CARTESIAN_POINT ( 'NONE',  ( 0.4030913312595973408, -0.4806107285681981423, 1.703151836983556988 ) ) ;
#78427 = CARTESIAN_POINT ( 'NONE',  ( 6.311143239517568837, 0.9901597221020401740, -1.423469027432751943 ) ) ;
#78428 = CARTESIAN_POINT ( 'NONE',  ( 5.161534370633450663, 0.8641669074914829496, 1.510678848428636201 ) ) ;
#78429 = CARTESIAN_POINT ( 'NONE',  ( 3.527152830493656577, -2.117552691746289018, 0.8784855890422419433 ) ) ;
#78430 = CARTESIAN_POINT ( 'NONE',  ( 1.364683531249986537, -0.8447916663252468261, -0.7879004041258309554 ) ) ;
#78431 = CARTESIAN_POINT ( 'NONE',  ( 1.376629057770164311, 1.701771572936720212, -0.7031625657484343872 ) ) ;
#78432 = CARTESIAN_POINT ( 'NONE',  ( -0.3000000000000352940, 3.999999999999973799, 0.9782388782688533624 ) ) ;
#78433 = CARTESIAN_POINT ( 'NONE',  ( 2.010518257881420023, 1.354885872097401078, -1.223726681998098087 ) ) ;
#78434 = CARTESIAN_POINT ( 'NONE',  ( 2.901017702322743919, -0.9963018188003970321, -1.753030416019534021 ) ) ;
#78435 = CARTESIAN_POINT ( 'NONE',  ( -2.277406616971334508, 5.600798786534425311, 1.040834085586084257E-14 ) ) ;
#78436 = CARTESIAN_POINT ( 'NONE',  ( 1.394752248596371702, 1.789971953256053627, -1.264032476404143512 ) ) ;
#78437 = CARTESIAN_POINT ( 'NONE',  ( 8.779421058653776200, 13.51919467333984493, -7.714288002668382660 ) ) ;
#78438 = CARTESIAN_POINT ( 'NONE',  ( 4.067482540003349634, 0.2598354432931935243, -2.089805856947650309 ) ) ;
#78439 = CARTESIAN_POINT ( 'NONE',  ( -6.307567778855718288, 8.381915046796901692, -1.599625672291263179 ) ) ;
#78440 = CARTESIAN_POINT ( 'NONE',  ( 8.110954823418250470, 13.89836686726292037, 9.741300253657557917 ) ) ;
#78441 = CARTESIAN_POINT ( 'NONE',  ( 1.135311898753359472, -0.04898221611688948623, -2.069941200615910581 ) ) ;
#78442 = CARTESIAN_POINT ( 'NONE',  ( 5.529027716274630855, 5.344953845275508542, 1.040834085586084257E-14 ) ) ;
#78443 = CARTESIAN_POINT ( 'NONE',  ( 1.360316468749955598, -0.7239583329918893861, 0.7853790794158480582 ) ) ;
#78444 = CARTESIAN_POINT ( 'NONE',  ( 4.617906949270495609, -0.5647423089508787353, 2.043846993246847710 ) ) ;
#78446 = AXIS2_PLACEMENT_3D ( 'NONE', #121565, #155051, #187537 ) ;
#78445 = CONTEXT_DEPENDENT_SHAPE_REPRESENTATION ( #21529, #175094 ) ;
#78447 = CARTESIAN_POINT ( 'NONE',  ( 6.481070005604858686, -0.09514881109910081070, -1.823337098959529001 ) ) ;
#78448 = ORIENTED_EDGE ( 'NONE', *, *, #135735, .T. ) ;
#78449 = CARTESIAN_POINT ( 'NONE',  ( -5.224688093219839402, 7.188831756880171397, -1.599625672291271394 ) ) ;
#78450 = CARTESIAN_POINT ( 'NONE',  ( 8.211434591371064684, 12.73175745657494851, -0.7998128361456352531 ) ) ;
#78451 = CARTESIAN_POINT ( 'NONE',  ( 7.322812364712459221, 7.715904978352238430, 0.000000000000000000 ) ) ;
#78452 = CARTESIAN_POINT ( 'NONE',  ( 1.737500000000001155, -0.5395833323774169576, 3.009438278150922130 ) ) ;
#78453 = CARTESIAN_POINT ( 'NONE',  ( -5.042743069279040036, 7.970618449879118828, 1.199719254218464037 ) ) ;
#78454 = CARTESIAN_POINT ( 'NONE',  ( 6.521762860236213655, -0.4636855090699961712, 2.076960040381255812 ) ) ;
#78455 = CARTESIAN_POINT ( 'NONE',  ( 0.8859290024384089968, 1.414438444053778055, 1.560449103131421156 ) ) ;
#78456 = CARTESIAN_POINT ( 'NONE',  ( -4.132202957115018727, 8.042930226601317401, 0.000000000000000000 ) ) ;
#78457 = CARTESIAN_POINT ( 'NONE',  ( 7.404724451357931336, 11.79059562655963056, 0.7998128361456462443 ) ) ;
#78458 = CARTESIAN_POINT ( 'NONE',  ( 5.612096381091351560, 1.858897858770152789, -0.08933831184920922042 ) ) ;
#78459 = CARTESIAN_POINT ( 'NONE',  ( 8.776205506747620788, 9.133327934160710981, -0.7998128361456221525 ) ) ;
#78460 = CARTESIAN_POINT ( 'NONE',  ( -0.4153311931459070516, 3.919822700377107783, -0.4999999999999988343 ) ) ;
#78461 = CARTESIAN_POINT ( 'NONE',  ( -4.442231607132987925, 5.211633625523774960, -1.199719254218453823 ) ) ;
#78462 = CARTESIAN_POINT ( 'NONE',  ( -3.277320446201389181, 4.846626492033466072, 1.599625672291267398 ) ) ;
#78463 = DIRECTION ( 'NONE',  ( -0.000000000000000000, 1.000000000000000000, -0.000000000000000000 ) ) ;
#78465 = CARTESIAN_POINT ( 'NONE',  ( 2.348037267531626338, -0.8415878996531295231, 1.772339229757218471 ) ) ;
#78464 = CARTESIAN_POINT ( 'NONE',  ( -7.528855374290365887, 7.678086112960552434, -0.7998128361456291469 ) ) ;
#78466 = CARTESIAN_POINT ( 'NONE',  ( 0.7608789386071808103, -1.564954856162886765, 1.491513986042219297 ) ) ;
#78468 = CARTESIAN_POINT ( 'NONE',  ( -6.016097364521681534, 6.072308155256833651, 0.6301904134648171896 ) ) ;
#78467 = CARTESIAN_POINT ( 'NONE',  ( -4.111865726694519552, 8.019203457777400956, 0.000000000000000000 ) ) ;
#78469 = CARTESIAN_POINT ( 'NONE',  ( 0.6823417656249882723, -0.1572916663252488245, 1.181850606188755259 ) ) ;
#78470 = CARTESIAN_POINT ( 'NONE',  ( 2.793977985172685141, -1.619072854944574313, 0.6208489642184951141 ) ) ;
#78471 = CARTESIAN_POINT ( 'NONE',  ( 2.255425419672125287, 0.7431408456733903378, 1.573829366573131328 ) ) ;
#78472 = CARTESIAN_POINT ( 'NONE',  ( 6.141480397310468575, 10.10888486359680982, 1.040834085586084257E-14 ) ) ;
#78473 = CARTESIAN_POINT ( 'NONE',  ( -12.76914910123260682, 7.416938840849524262, -2.145643146812736823 ) ) ;
#78474 = AXIS2_PLACEMENT_3D ( 'NONE', #116055, #203618, #51005 ) ;
#78475 = CARTESIAN_POINT ( 'NONE',  ( 0.8431247865267020858, -1.122328847578180078, 1.674629589540656216 ) ) ;
#78476 = CARTESIAN_POINT ( 'NONE',  ( 6.925078400183593885, 7.051837472187183486, 2.742497896504832333 ) ) ;
#78477 = CARTESIAN_POINT ( 'NONE',  ( -3.474632506852224356, 7.275764701294714420, -0.7998128361456481317 ) ) ;
#78478 = CARTESIAN_POINT ( 'NONE',  ( 1.674623549722221716, -1.871433754200592992, -0.6201854899473575600 ) ) ;
#78479 = AXIS2_PLACEMENT_3D ( 'NONE', #138108, #68798, #17914 ) ;
#78480 = EDGE_CURVE ( 'NONE', #81487, #74349, #207084, .T. ) ;
#78482 = CARTESIAN_POINT ( 'NONE',  ( -6.631346530859867805, 6.909194838857525944, 0.000000000000000000 ) ) ;
#78481 = CARTESIAN_POINT ( 'NONE',  ( 6.029550621839829816, -0.2273517531893587407, 1.898748578088353733 ) ) ;
#78483 = CARTESIAN_POINT ( 'NONE',  ( -6.739811759324831897, 7.996106819701333634, -1.082531754730549967 ) ) ;
#78484 = CARTESIAN_POINT ( 'NONE',  ( 7.212011367826596242, 7.378711115411311638, 0.000000000000000000 ) ) ;
#78485 = CARTESIAN_POINT ( 'NONE',  ( -5.433785704026946384, 9.561443431331920095, 0.000000000000000000 ) ) ;
#78486 = CARTESIAN_POINT ( 'NONE',  ( 1.401042149647635071, -0.2984598639739938220, -1.997379878556293731 ) ) ;
#78487 = CARTESIAN_POINT ( 'NONE',  ( -10.75000000000000000, 0.000000000000000000, 0.000000000000000000 ) ) ;
#78488 = CARTESIAN_POINT ( 'NONE',  ( 4.788248824917088697, -1.092567961935811960, 2.032559802855623321 ) ) ;
#78489 = CARTESIAN_POINT ( 'NONE',  ( 6.162552467866693640, -0.7048080804108979303, -1.831077584432870609 ) ) ;
#78490 = CARTESIAN_POINT ( 'NONE',  ( 3.485159065011545376, 0.04355839926390054490, 1.961427607708134957 ) ) ;
#78491 = CARTESIAN_POINT ( 'NONE',  ( 7.801827329660018684, 11.18955008699033726, 1.199719254218460707 ) ) ;
#78492 = CARTESIAN_POINT ( 'NONE',  ( -9.608184375605320682, 15.11803084963731258, 7.189074558345553534 ) ) ;
#78493 = VERTEX_POINT ( 'NONE', #188252 ) ;
#78494 = CARTESIAN_POINT ( 'NONE',  ( 1.710321574826153324, 1.214426542090217609, -1.734289745093554380 ) ) ;
#78496 = CARTESIAN_POINT ( 'NONE',  ( -7.802881099864745984, 9.062115023719057305, -1.199719254218446718 ) ) ;
#78495 = CARTESIAN_POINT ( 'NONE',  ( -4.298098390732130625, 4.973201863064262263, 1.199719254218462483 ) ) ;
#78497 = CARTESIAN_POINT ( 'NONE',  ( 1.306327274835542784, 1.622920506532832929, 0.8694138843568788300 ) ) ;
#78498 = ORIENTED_EDGE ( 'NONE', *, *, #27529, .T. ) ;
#78499 = CARTESIAN_POINT ( 'NONE',  ( 11.83030212645851620, 7.766851926455670352, -1.746998778190154589 ) ) ;
#78500 = CARTESIAN_POINT ( 'NONE',  ( 3.305043459179863419, -0.4174351347619070229, -2.078937965663613774 ) ) ;
#78501 = CARTESIAN_POINT ( 'NONE',  ( 0.7499999999999902300, 3.847916667349481123, -1.299038105676658228 ) ) ;
#78502 = CARTESIAN_POINT ( 'NONE',  ( 8.106885785967500979, 11.54545161934907682, 1.199719254218460707 ) ) ;
#78503 = CARTESIAN_POINT ( 'NONE',  ( -1.853343808665687931, 2.488708180678084414, -2.484983702926222726 ) ) ;
#78504 = CARTESIAN_POINT ( 'NONE',  ( 3.444654265643578128, 0.4973230594479564060, 1.999757164544394561 ) ) ;
#78506 = CARTESIAN_POINT ( 'NONE',  ( 0.1339853816830008371, 0.3136495386693045062, 1.814181566856580607 ) ) ;
#78505 = CARTESIAN_POINT ( 'NONE',  ( -9.040589502214116280, 9.441775928871617651, 0.7998128361456462443 ) ) ;
#78507 = CARTESIAN_POINT ( 'NONE',  ( 1.364683531249988535, 3.613541667008086211, 0.7879004041258500513 ) ) ;
#78508 = CARTESIAN_POINT ( 'NONE',  ( -0.9311234436981514762, -2.871869630441517884, -3.474999999999999645 ) ) ;
#78509 = CARTESIAN_POINT ( 'NONE',  ( 1.500343415223059917, 4.450747917682662980, -0.07855322731631581012 ) ) ;
#78510 = PRESENTATION_LAYER_ASSIGNMENT (  '', '', ( #164942 ) ) ;
#78511 = CARTESIAN_POINT ( 'NONE',  ( 0.4697016844467936103, 0.2121168557088908557, -2.196667960996725011 ) ) ;
#78512 = CARTESIAN_POINT ( 'NONE',  ( 2.267197333419627370, -2.067742563539621603, -0.9185262150545376869 ) ) ;
#78513 = CARTESIAN_POINT ( 'NONE',  ( -9.666600336863641729, 10.38004793587015584, 1.040834085586084257E-14 ) ) ;
#78514 = CARTESIAN_POINT ( 'NONE',  ( 2.214858347191206445, 1.452946758456060250, -1.081763258146416939 ) ) ;
#78515 = CARTESIAN_POINT ( 'NONE',  ( 2.799894175352398484, -0.9483327596419667271, -1.664474063330185105 ) ) ;
#78516 = CARTESIAN_POINT ( 'NONE',  ( 4.686024408448190570, -1.271122505372159539, -1.634150330299996012 ) ) ;
#78517 = CARTESIAN_POINT ( 'NONE',  ( 1.364683531249988535, 3.217708333674748289, -0.7879004041258239610 ) ) ;
#78518 = CARTESIAN_POINT ( 'NONE',  ( 1.516417288619626769, 1.325465413702779482, -1.459542524610158098 ) ) ;
#78519 = CARTESIAN_POINT ( 'NONE',  ( 0.2527871956496882122, -1.549381263408876830, 1.144551880545265465 ) ) ;
#78520 = CARTESIAN_POINT ( 'NONE',  ( 3.080767038946086611, -0.1360980058115155988, -1.865751385159146070 ) ) ;
#78522 = CARTESIAN_POINT ( 'NONE',  ( 4.701115458738250652, 8.361069499448168685, -0.6471830670988186762 ) ) ;
#78521 = CARTESIAN_POINT ( 'NONE',  ( 1.577271561783103460, -2.192461267746559361, -0.7203256085408450415 ) ) ;
#78523 = CARTESIAN_POINT ( 'NONE',  ( 2.717075380476912994, -1.617705633067820559, -0.9199624106535415624 ) ) ;
#78524 = CARTESIAN_POINT ( 'NONE',  ( -0.6823417656249969321, 3.217708333674754062, -1.181850606188749264 ) ) ;
#78525 = CARTESIAN_POINT ( 'NONE',  ( 6.004357462130720080, 2.060136995665005522, 0.1050117271170700056 ) ) ;
#78526 = CARTESIAN_POINT ( 'NONE',  ( -3.927058049452637700, 7.733318157670055371, -0.7998128361456281477 ) ) ;
#78527 = CARTESIAN_POINT ( 'NONE',  ( 7.772902139336337335, 7.962807338847539107, 0.7998128361456341429 ) ) ;
#78528 = CARTESIAN_POINT ( 'NONE',  ( -1.466385641617019342, 3.464586277566083172, -0.3259940066991236507 ) ) ;
#78529 = CARTESIAN_POINT ( 'NONE',  ( 5.965875410913440646, 2.075401660611264631, -0.3564754433343624296 ) ) ;
#78530 = CARTESIAN_POINT ( 'NONE',  ( 1.364683531249990311, 3.946875000341417028, 1.214306433183764966E-14 ) ) ;
#78531 = CARTESIAN_POINT ( 'NONE',  ( 5.835289683280778128, -1.956920075724715602, 0.9183947573421016308 ) ) ;
#78532 = CARTESIAN_POINT ( 'NONE',  ( 6.094400524283400067, -1.078572965507901715, 1.707356775630589851 ) ) ;
#78533 = CARTESIAN_POINT ( 'NONE',  ( 0.6823417656249882723, -0.9072916663252494907, 1.181850606188755259 ) ) ;
#78534 =( GEOMETRIC_REPRESENTATION_CONTEXT ( 3 ) GLOBAL_UNCERTAINTY_ASSIGNED_CONTEXT ( ( #118229 ) ) GLOBAL_UNIT_ASSIGNED_CONTEXT ( ( #53637, #69855, #100254 ) ) REPRESENTATION_CONTEXT ( 'NONE', 'WORKASPACE' ) );
#78535 = CARTESIAN_POINT ( 'NONE',  ( -3.280709984826970516, 6.771319382366015383, 0.7216878364870317197 ) ) ;
#78538 = CARTESIAN_POINT ( 'NONE',  ( 5.395781948558860286, 6.357795697149212444, -1.082531754730542195 ) ) ;
#78537 = CARTESIAN_POINT ( 'NONE',  ( 6.825078400183545391, 0.005516643811322509937, 1.755566376062764222 ) ) ;
#78536 = CARTESIAN_POINT ( 'NONE',  ( 6.984385409695311964, 8.177479728513226576, 1.199719254218452935 ) ) ;
#78539 = CARTESIAN_POINT ( 'NONE',  ( -4.305596300791617814, 7.180890229968955651, 1.199719254218452935 ) ) ;
#78540 = CARTESIAN_POINT ( 'NONE',  ( 4.223842396274177347, 0.8578445224393380641, -1.825075645057252505 ) ) ;
#78541 = CARTESIAN_POINT ( 'NONE',  ( -8.199983978166823562, 8.461069484149769337, -0.7998128361456291469 ) ) ;
#78543 = CARTESIAN_POINT ( 'NONE',  ( -5.261973015435229328, 9.153069261400824885, 0.000000000000000000 ) ) ;
#78542 = CARTESIAN_POINT ( 'NONE',  ( -9.842856333841300653, 10.58567993234409421, 0.7216878364870438212 ) ) ;
#78544 = CARTESIAN_POINT ( 'NONE',  ( -1.364683531250010295, 5.530208333674751842, 0.7879004041258379498 ) ) ;
#78546 = CARTESIAN_POINT ( 'NONE',  ( -0.6823417656250003738, 9.151041667008065872, 1.181850606188754593 ) ) ;
#78545 = CARTESIAN_POINT ( 'NONE',  ( 5.629794960336353071, -1.368038101806166029, -1.673757646710342550 ) ) ;
#78547 = DIRECTION ( 'NONE',  ( -3.330669073875478989E-16, 3.540251991789410786E-16, 1.000000000000000000 ) ) ;
#78548 = CARTESIAN_POINT ( 'NONE',  ( -11.88508768177337771, 7.945503028788528432, -1.311673572704820767 ) ) ;
#78549 = ADVANCED_FACE ( 'NONE', ( #201283 ), #137396, .T. ) ;
#78551 = CARTESIAN_POINT ( 'NONE',  ( 6.398064575937244314, -0.9530261711272209890, -1.777004751544956962 ) ) ;
#78550 = CARTESIAN_POINT ( 'NONE',  ( -6.033015167956805591, 8.061603667414825480, -1.443375672974058777 ) ) ;
#78552 = CARTESIAN_POINT ( 'NONE',  ( 0.6823417656249882723, -0.8447916663252494907, 1.181850606188755259 ) ) ;
#78553 = CARTESIAN_POINT ( 'NONE',  ( 1.593959923740532414, -1.716304196509855329, -0.1716357895808154899 ) ) ;
#78554 = CARTESIAN_POINT ( 'NONE',  ( 3.061108821635398769, 6.793320401875094561, -0.7998128361456362523 ) ) ;
#78555 = CARTESIAN_POINT ( 'NONE',  ( 5.071631979963703962, 8.074598522336444262, 1.199719254218451159 ) ) ;
#78556 = CARTESIAN_POINT ( 'NONE',  ( -11.95485367524497811, 9.001114148948307303, 0.3044536461800395610 ) ) ;
#78557 = CARTESIAN_POINT ( 'NONE',  ( 0.1804953903597758258, -0.1286114524143982807, -1.740565225867502397 ) ) ;
#78558 = CARTESIAN_POINT ( 'NONE',  ( 0.8385398129025347647, 1.197303422201956957, -1.618206657969661011 ) ) ;
#78559 = FILL_AREA_STYLE ('',( #43954 ) ) ;
#78560 = CARTESIAN_POINT ( 'NONE',  ( 3.434799832723956836, 2.152550277175222515, 0.4854691814954179563 ) ) ;
#78561 = CARTESIAN_POINT ( 'NONE',  ( 5.067309307786254102, 1.885564733447910646, 1.076134493607887155 ) ) ;
#78562 = VERTEX_POINT ( 'NONE', #53998 ) ;
#78563 = CARTESIAN_POINT ( 'NONE',  ( 1.499999999999985123, -0.7041666666666481778, -0.8660254037844323793 ) ) ;
#78564 = CARTESIAN_POINT ( 'NONE',  ( 9.531018800282605952, 11.18223869082697597, 1.082531754730548412 ) ) ;
#78566 = CARTESIAN_POINT ( 'NONE',  ( 3.181267708840180397, 1.591331833097202608, 1.238305487465785726 ) ) ;
#78565 = CARTESIAN_POINT ( 'NONE',  ( 3.580828998445852562, -1.422877522674294681, 1.572404880189558485 ) ) ;
#78568 = ORIENTED_EDGE ( 'NONE', *, *, #196068, .F. ) ;
#78567 = CARTESIAN_POINT ( 'NONE',  ( 3.111360644411143017, 1.430921235420354654, 1.110905701166440940 ) ) ;
#78569 = CARTESIAN_POINT ( 'NONE',  ( 5.688527969385528849, 8.794310509995222347, -1.199719254218452047 ) ) ;
#78570 = VERTEX_POINT ( 'NONE', #120137 ) ;
#78571 = CARTESIAN_POINT ( 'NONE',  ( 0.2329894512427649056, -1.712236961970284410, 0.7538099095961706686 ) ) ;
#78572 = CARTESIAN_POINT ( 'NONE',  ( 5.612185521052973414, 8.634967976948757951, -1.199719254218440723 ) ) ;
#78574 = CARTESIAN_POINT ( 'NONE',  ( 1.270553553854154361, -0.2845990055821822629, -1.894349495789057647 ) ) ;
#78573 = CARTESIAN_POINT ( 'NONE',  ( -3.253066792275140173, 5.882662793374543675, 1.199719254218462483 ) ) ;
#78575 = CARTESIAN_POINT ( 'NONE',  ( -2.677589438261867016, 0.4530478092824221648, -0.1093532045961659316 ) ) ;
#78576 = LINE ( 'NONE', #176100, #183667 ) ;
#78577 = CARTESIAN_POINT ( 'NONE',  ( 1.364683531249986537, 1.967708333674750731, -0.7879004041258239610 ) ) ;
#78578 = DIRECTION ( 'NONE',  ( -0.4999999999999978906, 0.000000000000000000, 0.8660254037844399289 ) ) ;
#78579 = CARTESIAN_POINT ( 'NONE',  ( -9.158696461231359720, 10.64389961198009615, 1.199719254218462483 ) ) ;
#78580 = CARTESIAN_POINT ( 'NONE',  ( 5.102478102407745908, -0.7247817745383768884, -2.036717088958202471 ) ) ;
#78581 = CARTESIAN_POINT ( 'NONE',  ( -4.285785955695645910, 7.053815144069948140, 1.082531754730549967 ) ) ;
#78582 = CARTESIAN_POINT ( 'NONE',  ( -6.454563648557663846, 9.688018802362710957, -1.199719254218452047 ) ) ;
#78583 = CARTESIAN_POINT ( 'NONE',  ( 2.760144723603759065, 0.7592700852765141839, -1.980205354017528840 ) ) ;
#78585 = CARTESIAN_POINT ( 'NONE',  ( -11.77618483200234500, 4.711409542047888976, 4.977076041189349098 ) ) ;
#78584 = DIRECTION ( 'NONE',  ( -5.578564026256490882E-16, -1.000000000000000000, -9.066213480720158442E-32 ) ) ;
#78586 = CARTESIAN_POINT ( 'NONE',  ( 4.833256578820930294, -1.803536663746601709, 0.7962986557112069486 ) ) ;
#78587 = CARTESIAN_POINT ( 'NONE',  ( 6.504189997394580480, -0.8109953713257547214, 1.730197269205424160 ) ) ;
#78588 = ORIENTED_EDGE ( 'NONE', *, *, #204577, .T. ) ;
#78589 = CIRCLE ( 'NONE', #189306, 0.5000000000000008882 ) ;
#78590 = CARTESIAN_POINT ( 'NONE',  ( 5.630101985619759830, 2.115003628044552553, 0.1013798475145138156 ) ) ;
#78591 = CARTESIAN_POINT ( 'NONE',  ( 1.713667314260276076, -1.036161614632699957, 1.380621972511351547 ) ) ;
#78592 = CARTESIAN_POINT ( 'NONE',  ( 6.707475516188797116, -1.580950341439198992, -1.174378316608926331 ) ) ;
#78593 = CARTESIAN_POINT ( 'NONE',  ( 2.906119529042447969, 1.406244311732379293, -1.339499261486200465 ) ) ;
#78594 = ORIENTED_EDGE ( 'NONE', *, *, #24813, .T. ) ;
#78595 = CARTESIAN_POINT ( 'NONE',  ( 2.280056242076713424, 5.600610285695403867, 0.4779128307904490502 ) ) ;
#78596 = CARTESIAN_POINT ( 'NONE',  ( 6.068156270568149324, 9.237210194708310951, 1.199719254218452047 ) ) ;
#78598 = CARTESIAN_POINT ( 'NONE',  ( 5.144429221381498607, 8.089252293998699272, -1.199719254218452047 ) ) ;
#78597 = CARTESIAN_POINT ( 'NONE',  ( 2.291069257668688408, 1.616616537889125516, 1.325633359429157831 ) ) ;
#78599 = CARTESIAN_POINT ( 'NONE',  ( 6.502017186205484300, 9.743381262951846367, -1.199719254218452047 ) ) ;
#78601 = VERTEX_POINT ( 'NONE', #172023 ) ;
#78600 = CARTESIAN_POINT ( 'NONE',  ( 0.3635249777022043771, 0.5700983740567664437, -1.719507965497588220 ) ) ;
#78602 = CARTESIAN_POINT ( 'NONE',  ( 4.653060005753134831, -1.773635849817876586, 1.313014255023836618 ) ) ;
#78603 = CARTESIAN_POINT ( 'NONE',  ( -0.3811408430856468854, -6.893136995914816545, -10.99374989157286819 ) ) ;
#78604 = CARTESIAN_POINT ( 'NONE',  ( 3.171135245091468491, -2.038329301889611589, -0.8460836234857532778 ) ) ;
#78605 = CARTESIAN_POINT ( 'NONE',  ( -11.78331023100045627, 12.22000000000000064, -1.800000000000001155 ) ) ;
#78606 = CARTESIAN_POINT ( 'NONE',  ( 1.383307607624170155, 0.1396965592646744470, -1.907218110473147155 ) ) ;
#78607 = CARTESIAN_POINT ( 'NONE',  ( 8.666686507633574621, 11.13422023037111330, 1.599625672291281386 ) ) ;
#78608 = CARTESIAN_POINT ( 'NONE',  ( 4.000488093070094564, 2.060113009926473726, 0.2059288336104248551 ) ) ;
#78610 = CARTESIAN_POINT ( 'NONE',  ( 2.588937169860201504, -0.3686131662095324946, -2.129881858774537395 ) ) ;
#78609 = CARTESIAN_POINT ( 'NONE',  ( 5.908535366263007127, 4.807949608181236734, 2.500000000000011102 ) ) ;
#78611 = CARTESIAN_POINT ( 'NONE',  ( 5.038714576072483631, -1.879839391954684746, 1.126354835186346603 ) ) ;
#78612 = CARTESIAN_POINT ( 'NONE',  ( 8.536830278099042602, 13.11138575775759563, -0.7998128361456352531 ) ) ;
#78613 = CARTESIAN_POINT ( 'NONE',  ( -0.5021762176675858003, 7.740673110510177146, 1.993154341637425331 ) ) ;
#78614 = CARTESIAN_POINT ( 'NONE',  ( 6.900173834712277632, 7.014900660111269559, -0.7998128361456341429 ) ) ;
#78615 = CARTESIAN_POINT ( 'NONE',  ( 0.000000000000000000, -2.384374999522042238, -3.793834371823813445 ) ) ;
#78616 = CARTESIAN_POINT ( 'NONE',  ( -4.411198876399886615, 6.239761003923544713, -1.599625672291271394 ) ) ;
#78617 = CARTESIAN_POINT ( 'NONE',  ( 0.1939827082095749167, 1.755770691208278889, 0.9913967135185000057 ) ) ;
#78618 = CARTESIAN_POINT ( 'NONE',  ( -9.381879110976678149, 11.00824238663667565, 1.082531754730558626 ) ) ;
#78620 = CARTESIAN_POINT ( 'NONE',  ( 5.737035277238070385, 6.722237907313067140, -1.199719254218452047 ) ) ;
#78619 = AXIS2_PLACEMENT_3D ( 'NONE', #84690, #203744, #167017 ) ;
#78621 = CARTESIAN_POINT ( 'NONE',  ( 4.241125740018336643, -0.1978421677554068614, -2.060750949040678570 ) ) ;
#78622 = CARTESIAN_POINT ( 'NONE',  ( 3.756402471274498112, 0.6942424141608801724, 1.797233106274237713 ) ) ;
#78623 = CARTESIAN_POINT ( 'NONE',  ( 0.4918148228068714989, -2.006445053647107013, 0.2004575690456936732 ) ) ;
#78624 = CARTESIAN_POINT ( 'NONE',  ( 6.471319392424407901, 6.444294134116939077, 0.7998128361456341429 ) ) ;
#78625 = CARTESIAN_POINT ( 'NONE',  ( 9.406792723036287995, 4.446947629225665111, 7.380298948578114526 ) ) ;
#78626 = CARTESIAN_POINT ( 'NONE',  ( 3.520317136570957128, 0.8812775084000439296, 1.761307543597267822 ) ) ;
#78627 = CARTESIAN_POINT ( 'NONE',  ( 0.6740948890744530297, -1.214310170130480593, 1.824057261183717582 ) ) ;
#78628 = CARTESIAN_POINT ( 'NONE',  ( 4.600122369450095228, -1.825375079466069694, -0.04201004182294298950 ) ) ;
#78629 = CARTESIAN_POINT ( 'NONE',  ( 5.546694241766559230, 9.485244025454063532, 0.000000000000000000 ) ) ;
#78630 = CARTESIAN_POINT ( 'NONE',  ( 3.999292125906911188, 4.728557570721922509, 1.082531754730560403 ) ) ;
#78631 = CARTESIAN_POINT ( 'NONE',  ( -7.795011973214244883, 8.058878488363559356, 0.7998128361456341429 ) ) ;
#78632 = CARTESIAN_POINT ( 'NONE',  ( 3.555981428534177091, 7.370671776590375757, 0.7998128361456271485 ) ) ;
#78633 = EDGE_LOOP ( 'NONE', ( #42923, #2362, #70188, #210250 ) ) ;
#78635 = CARTESIAN_POINT ( 'NONE',  ( 4.922139854824453487, -2.003099925734778797, 0.2017396019941309904 ) ) ;
#78634 = CARTESIAN_POINT ( 'NONE',  ( 1.434833617064284805, -1.334073193498284793, -1.269287082821937362 ) ) ;
#78636 = CARTESIAN_POINT ( 'NONE',  ( 0.3866022076702098076, -0.1098403002397010941, 2.295889243394435564 ) ) ;
#78637 = CARTESIAN_POINT ( 'NONE',  ( 5.172687041346638814, 1.355624813549320740, -1.418227474788292364 ) ) ;
#78638 = CARTESIAN_POINT ( 'NONE',  ( -5.585069213825653023, 8.603332285183535433, -1.199719254218440723 ) ) ;
#78639 = CARTESIAN_POINT ( 'NONE',  ( -4.761938266897808525, 6.578680616179308771, 1.599625672291267398 ) ) ;
#78640 = CARTESIAN_POINT ( 'NONE',  ( -10.20634067979475823, 1.972237431424362253, -5.892633538919750613 ) ) ;
#78641 = CARTESIAN_POINT ( 'NONE',  ( -4.716257332707368910, 6.595662536282280719, -1.599625672291271394 ) ) ;
#78643 = CARTESIAN_POINT ( 'NONE',  ( 0.4087956859853311142, 1.625333209436867321, 0.9259686016569528277 ) ) ;
#78642 = CARTESIAN_POINT ( 'NONE',  ( 1.400065306692158229, -0.7557916345088554477, -1.949536834912476646 ) ) ;
#78644 = CARTESIAN_POINT ( 'NONE',  ( -7.874499448206171870, -5.294771359305316061, 7.680942717881079851 ) ) ;
#78645 = CARTESIAN_POINT ( 'NONE',  ( -0.2102771530458459603, 6.947233595868168798, -2.798738817348767949 ) ) ;
#78646 = CARTESIAN_POINT ( 'NONE',  ( 0.4150587399484934603, -0.9287321991380654840, -1.471733822881353015 ) ) ;
#78647 = CARTESIAN_POINT ( 'NONE',  ( 5.612185521052973414, 8.634967976948757951, -1.199719254218440723 ) ) ;
#78649 = CARTESIAN_POINT ( 'NONE',  ( 0.3282377607281126708, 1.738835450998185372, -1.225000000000013634 ) ) ;
#78648 = CARTESIAN_POINT ( 'NONE',  ( 0.000000000000000000, -2.000000000000001776, 0.000000000000000000 ) ) ;
#78650 = CARTESIAN_POINT ( 'NONE',  ( 2.191662871657253486, -0.7386692205221119245, 1.558845181661876467 ) ) ;
#78651 = CARTESIAN_POINT ( 'NONE',  ( 1.365048776756357940, 0.1565470504056795942, -2.186014887712848243 ) ) ;
#78652 = CARTESIAN_POINT ( 'NONE',  ( 4.160898416275903067, -1.636102012888400292, 1.481223685352812680 ) ) ;
#78653 = CARTESIAN_POINT ( 'NONE',  ( -10.80887392267048241, 4.296486016114100082, -4.677321330754881323 ) ) ;
#78654 = CARTESIAN_POINT ( 'NONE',  ( 1.042111193480334430, 1.456518763772189695, 1.610191069602670000 ) ) ;
#78655 = CARTESIAN_POINT ( 'NONE',  ( 0.4162703231485806454, 1.261427835099769634, -1.320066674804179385 ) ) ;
#78656 = CARTESIAN_POINT ( 'NONE',  ( 2.923186261301851996, -1.865062457072470536, 1.002408848433397726 ) ) ;
#78657 = CARTESIAN_POINT ( 'NONE',  ( 6.639320575229252341, 2.457876053485750223, 2.280608551775892501 ) ) ;
#78658 = EDGE_CURVE ( 'NONE', #180856, #178226, #66884, .T. ) ;
#78659 = ORIENTED_EDGE ( 'NONE', *, *, #210003, .F. ) ;
#78661 = CARTESIAN_POINT ( 'NONE',  ( -1.402160292154681736E-14, -0.2406249996585799189, -1.575800808251665908 ) ) ;
#78660 = CARTESIAN_POINT ( 'NONE',  ( 3.404133285375851248, -0.9304739769722850662, -2.095221664589861810 ) ) ;
#78662 = CARTESIAN_POINT ( 'NONE',  ( -11.81905481421901705, 12.34264344382733469, -1.592167362352180593 ) ) ;
#78663 = CARTESIAN_POINT ( 'NONE',  ( 4.029797971759831121, 5.724516938518342535, -1.599625672291255185 ) ) ;
#78664 = AXIS2_PLACEMENT_3D ( 'NONE', #29281, #74836, #160345 ) ;
#78665 = CARTESIAN_POINT ( 'NONE',  ( 5.953820247260992460, -1.607154219335062528, -1.533616513404257198 ) ) ;
#78666 = CARTESIAN_POINT ( 'NONE',  ( -7.551528373131759508, 7.912463978182924684, 1.040834085586084257E-14 ) ) ;
#78667 = EDGE_CURVE ( 'NONE', #120459, #175232, #166062, .T. ) ;
#78668 = CARTESIAN_POINT ( 'NONE',  ( 5.829642864196171281, 5.903597551091405826, 0.7216878364870317197 ) ) ;
#78669 = CARTESIAN_POINT ( 'NONE',  ( -7.551528372687420720, 8.872833191965849409, 1.082531754730558626 ) ) ;
#78670 = CARTESIAN_POINT ( 'NONE',  ( 3.607878275012302627, 7.223292064240769861, 0.7216878364870257245 ) ) ;
#78671 = VERTEX_POINT ( 'NONE', #56429 ) ;
#78672 = CARTESIAN_POINT ( 'NONE',  ( 3.797500137148449362, 1.423962148579031917, -1.427936706820939872 ) ) ;
#78674 = CARTESIAN_POINT ( 'NONE',  ( 2.026308614600486280, 1.056755808076353276, 1.771133502622779243 ) ) ;
#78673 = CARTESIAN_POINT ( 'NONE',  ( 5.880485940025228508, 7.883652901494672349, 1.599625672291267398 ) ) ;
#78675 = FACE_BOUND ( 'NONE', #118382, .T. ) ;
#78676 = CARTESIAN_POINT ( 'NONE',  ( 4.380693030546913391, 7.164540064729805202, 1.082531754730549078 ) ) ;
#78677 = CARTESIAN_POINT ( 'NONE',  ( 0.000000000000000000, -9.919999999999998153, 0.000000000000000000 ) ) ;
#78678 = CARTESIAN_POINT ( 'NONE',  ( -1.364683531249997417, 5.259375000341425022, 1.214306433183764966E-14 ) ) ;
#78679 = CARTESIAN_POINT ( 'NONE',  ( 5.208995777154565410, -0.3238732214236837992, 2.167259527466679270 ) ) ;
#78680 = CARTESIAN_POINT ( 'NONE',  ( 1.916638904718031000, -1.319229391439219246, -1.525043083973671498 ) ) ;
#78681 = CARTESIAN_POINT ( 'NONE',  ( 2.647807870277216757, 0.6224553824519338807, 1.732961026760751366 ) ) ;
#78682 = MECHANICAL_DESIGN_GEOMETRIC_PRESENTATION_REPRESENTATION (  '', ( #106271 ), #40516 ) ;
#78683 = EDGE_CURVE ( 'NONE', #84713, #149901, #47165, .T. ) ;
#78684 = CARTESIAN_POINT ( 'NONE',  ( 7.969495366734495434, 8.192166104145387706, 1.040834085586084257E-14 ) ) ;
#78685 = CARTESIAN_POINT ( 'NONE',  ( 5.754876975610782708, -1.437719105923901841, 1.124948175183659638 ) ) ;
#78686 = CARTESIAN_POINT ( 'NONE',  ( 5.818982467333652764, 0.9914020171761170896, -1.755767668913270407 ) ) ;
#78687 = CARTESIAN_POINT ( 'NONE',  ( -8.040148788103921973, 9.338927326664741457, 1.199719254218462483 ) ) ;
#78689 = CARTESIAN_POINT ( 'NONE',  ( -7.279802135894939852, 7.457800344824362604, -0.7998128361456362523 ) ) ;
#78688 = CARTESIAN_POINT ( 'NONE',  ( 5.893528310750998145, 1.708867279757080748, 1.482922863094847443 ) ) ;
#78690 = CARTESIAN_POINT ( 'NONE',  ( 0.4871192430246041316, -0.2598372338927424918, -2.089908867234680834 ) ) ;
#78691 = CARTESIAN_POINT ( 'NONE',  ( -5.915100157312088491, 10.12297696016459092, -0.7998128361456362523 ) ) ;
#78692 = CARTESIAN_POINT ( 'NONE',  ( 8.911787042884274257, 9.291506392986812912, 0.7998128361456462443 ) ) ;
#78693 = DIRECTION ( 'NONE',  ( -0.6841135908824225176, 0.4746712721541597735, -0.5537831508465286268 ) ) ;
#78694 = CARTESIAN_POINT ( 'NONE',  ( -5.879432169820529630, 10.01108796476595764, -0.7998128361456221525 ) ) ;
#78695 = CARTESIAN_POINT ( 'NONE',  ( 3.619250341049045527, 3.172667246362654847, -2.499999999999995115 ) ) ;
#78696 = CARTESIAN_POINT ( 'NONE',  ( 8.080296363620359301, 8.529359967086321603, 1.040834085586084257E-14 ) ) ;
#78697 = CARTESIAN_POINT ( 'NONE',  ( 4.007117460063951420, 7.817974094756804604, -0.2064290434495383852 ) ) ;
#78698 = CARTESIAN_POINT ( 'NONE',  ( -8.175203439360366531, 12.48156174598837787, 1.040834085586084257E-14 ) ) ;
#78700 = CARTESIAN_POINT ( 'NONE',  ( 3.129344976949835822, 2.009775620968552445, 0.9465212012665072949 ) ) ;
#78699 = CARTESIAN_POINT ( 'NONE',  ( 1.933984528066152953, -2.055706711753771287, 0.5200354980386610038 ) ) ;
#78701 = CARTESIAN_POINT ( 'NONE',  ( 3.243620375240426235, 6.419334294643912031, -0.9047145305212719313 ) ) ;
#78702 = CARTESIAN_POINT ( 'NONE',  ( -6.798487682609798632, 6.896266815991691779, 0.7998128361456341429 ) ) ;
#78703 = CARTESIAN_POINT ( 'NONE',  ( 5.774883364416965037, 8.824782127540085952, -1.199719254218440723 ) ) ;
#78704 = CARTESIAN_POINT ( 'NONE',  ( 3.824618516750320385, -1.319357783791510697, 1.452116237791359010 ) ) ;
#78705 = CARTESIAN_POINT ( 'NONE',  ( 4.635998460869027227, 7.496083073400806818, -1.199719254218452047 ) ) ;
#78706 = CARTESIAN_POINT ( 'NONE',  ( -4.068573627943592008, 7.549288226164498461, -0.4708643921484123585 ) ) ;
#78707 = CARTESIAN_POINT ( 'NONE',  ( 5.169736645512481132, 4.925780929386339935, 0.7998128361456341429 ) ) ;
#78708 = CARTESIAN_POINT ( 'NONE',  ( -5.153507786970276783, 6.145418851954329575, -1.082531754730549967 ) ) ;
#78710 = VERTEX_POINT ( 'NONE', #42330 ) ;
#78709 = CARTESIAN_POINT ( 'NONE',  ( -5.734735788900501952, 9.634349487118505806, 0.000000000000000000 ) ) ;
#78711 = CARTESIAN_POINT ( 'NONE',  ( 2.092179824929023102, 1.308410154019133076, 1.668721082780571408 ) ) ;
#78712 = CARTESIAN_POINT ( 'NONE',  ( -5.255720823952942489, 6.160704378480398979, -1.199719254218453823 ) ) ;
#78713 = CARTESIAN_POINT ( 'NONE',  ( 4.803692121107413726, -0.5798474923815257753, 2.082409481564663434 ) ) ;
#78714 = CARTESIAN_POINT ( 'NONE',  ( 3.087279721815265443, -0.7436087841871074078, 1.684586988852328160 ) ) ;
#78715 = UNCERTAINTY_MEASURE_WITH_UNIT (LENGTH_MEASURE( 1.000000000000000082E-05 ), #194570, 'distance_accuracy_value', 'NONE');
#78716 = CARTESIAN_POINT ( 'NONE',  ( -5.443780329924999606, 6.294985656096041993, 1.034245658874383578 ) ) ;
#78717 = EDGE_CURVE ( 'NONE', #120384, #122713, #212463, .T. ) ;
#78718 = CARTESIAN_POINT ( 'NONE',  ( -0.6823417656250003738, -0.4697916663252491021, -1.181850606188749264 ) ) ;
#78719 = CARTESIAN_POINT ( 'NONE',  ( 5.964775352603689740, 0.1210227373375266924, -1.736196924002187947 ) ) ;
#78720 = CARTESIAN_POINT ( 'NONE',  ( 3.877268743828258479, 7.467304601200877023, 0.7216878364870298324 ) ) ;
#78721 = CYLINDRICAL_SURFACE ( 'NONE', #167099, 0.08000000000000020983 ) ;
#78722 = CARTESIAN_POINT ( 'NONE',  ( 3.502937704049163159, 1.705309618848281472, -1.328393843302433153 ) ) ;
#78723 = CARTESIAN_POINT ( 'NONE',  ( 6.169296033003512925, -0.7230314695168098549, -1.882185070641306801 ) ) ;
#78724 = CARTESIAN_POINT ( 'NONE',  ( -8.093854517234044366, 11.42628545587295186, 1.082531754730549967 ) ) ;
#78725 = CARTESIAN_POINT ( 'NONE',  ( 2.430746436576446179, 2.096607243605509208, 0.5259719050795114148 ) ) ;
#78726 = CARTESIAN_POINT ( 'NONE',  ( 3.813711686511447763, -1.942732367404787830, 0.3338136033803756342 ) ) ;
#78727 = EDGE_CURVE ( 'NONE', #29327, #101924, #85878, .T. ) ;
#78728 = CARTESIAN_POINT ( 'NONE',  ( 0.1698123575781598782, 1.266975945507025081, 1.788028528876134393 ) ) ;
#78729 = CARTESIAN_POINT ( 'NONE',  ( 4.546391927783274056, -1.557747286768229600, 1.159548114344757019 ) ) ;
#78732 = VERTEX_POINT ( 'NONE', #162466 ) ;
#78731 = CARTESIAN_POINT ( 'NONE',  ( 0.000000000000000000, -1.500000000000001332, 2.000000000000000000 ) ) ;
#78730 = CARTESIAN_POINT ( 'NONE',  ( -9.449669878600623463, 11.08733161553131197, -1.082531754730537976 ) ) ;
#78734 = EDGE_CURVE ( 'NONE', #138616, #204013, #124713, .T. ) ;
#78733 = CARTESIAN_POINT ( 'NONE',  ( -7.279802135894939852, 7.457800344824362604, -0.7998128361456362523 ) ) ;
#78735 = DIRECTION ( 'NONE',  ( 0.000000000000000000, 1.000000000000000000, 0.000000000000000000 ) ) ;
#78737 = EDGE_LOOP ( 'NONE', ( #59741, #211394, #18489, #124124 ) ) ;
#78736 = CARTESIAN_POINT ( 'NONE',  ( -5.842637852846353397, 5.781108681267656202, 0.7998128361456281477 ) ) ;
#78738 = CARTESIAN_POINT ( 'NONE',  ( -8.975134502122321223, 9.573337795338607847, 1.040834085586084257E-14 ) ) ;
#78739 = CARTESIAN_POINT ( 'NONE',  ( 1.712255133470397261, -2.190042126362458319, 0.2705847154940849153 ) ) ;
#78740 = CARTESIAN_POINT ( 'NONE',  ( 1.001543065824772753E-15, -1.071874999522043792, 3.793834371823811669 ) ) ;
#78741 = CARTESIAN_POINT ( 'NONE',  ( 6.912952593004609625, -1.518390278170888008, 1.241885805282373134 ) ) ;
#78742 = CARTESIAN_POINT ( 'NONE',  ( 0.6823417656249899377, 4.988541667008086655, -1.181850606188754593 ) ) ;
#78743 = CARTESIAN_POINT ( 'NONE',  ( -1.001543065824772872E-14, 4.493750000682820378, 1.732050807568877637 ) ) ;
#78744 = CARTESIAN_POINT ( 'NONE',  ( 5.440174215215161979, 6.465126095745926449, -1.288585324421805511 ) ) ;
#78746 = CARTESIAN_POINT ( 'NONE',  ( -6.227272627378437342, 6.159572908229946187, -0.7998128361456291469 ) ) ;
#78745 = CARTESIAN_POINT ( 'NONE',  ( 5.031484404002879884, 6.963427452793765404, 1.443375672974065660 ) ) ;
#78747 = CARTESIAN_POINT ( 'NONE',  ( 5.191278274421009975, -0.6593680717656666967, 1.719199333795925710 ) ) ;
#78748 = ORIENTED_EDGE ( 'NONE', *, *, #169097, .T. ) ;
#78749 = CARTESIAN_POINT ( 'NONE',  ( -0.6801582343750125492, -0.6510416663252707181, -1.178068619123848526 ) ) ;
#78750 = CARTESIAN_POINT ( 'NONE',  ( -7.212047647465563038, 10.50147379109678880, -1.199719254218446718 ) ) ;
#78751 = CARTESIAN_POINT ( 'NONE',  ( 5.783468009189684622, 0.1541500780414573890, -2.115021274163720211 ) ) ;
#78752 = CARTESIAN_POINT ( 'NONE',  ( -2.474351396550309445, -0.3224749582910480528, -0.3303680917369637426 ) ) ;
#78753 = CARTESIAN_POINT ( 'NONE',  ( 4.286349120214771879, 8.152491073559232859, -0.7998128361456221525 ) ) ;
#78754 = B_SPLINE_CURVE_WITH_KNOTS ( 'NONE', 3,
 ( #31449, #177701, #163584, #94336, #113831, #130088 ),
 .UNSPECIFIED., .F., .F.,
 ( 4, 2, 4 ),
 ( 0.001105973075985389100, 0.001142139074170185750, 0.001178305072354982400 ),
 .UNSPECIFIED. ) ;
#78755 = CARTESIAN_POINT ( 'NONE',  ( 6.520785525839065677, 1.921145329286999326, 0.7461220883302563944 ) ) ;
#78758 = CARTESIAN_POINT ( 'NONE',  ( 3.403688466941825475, -0.7492148395099357261, -1.682118234477212537 ) ) ;
#78757 = CARTESIAN_POINT ( 'NONE',  ( 1.556854020514925496, 1.524047875013130104, -1.067797667942985917 ) ) ;
#78756 = SURFACE_SIDE_STYLE ('',( #12680 ) ) ;
#78759 = CARTESIAN_POINT ( 'NONE',  ( 9.271078113646423091, 9.710679308875986848, 1.040834085586084257E-14 ) ) ;
#78760 = FILL_AREA_STYLE ('',( #12684 ) ) ;
#78761 = CARTESIAN_POINT ( 'NONE',  ( -5.108390017298964914, 9.181815130149269422, 0.000000000000000000 ) ) ;
#78762 = CARTESIAN_POINT ( 'NONE',  ( 6.610000000000026077, 2.442988107647511065, 2.382821027452782570 ) ) ;
#78763 = AXIS2_PLACEMENT_3D ( 'NONE', #138690, #76858, #191663 ) ;
#78764 = CARTESIAN_POINT ( 'NONE',  ( 3.352369063006555905, 2.207063162671081713, 4.936380160885933677E-05 ) ) ;
#78765 = CARTESIAN_POINT ( 'NONE',  ( 6.345044588916532113, -1.916324442970654962, 1.202328811479462578 ) ) ;
#78766 = CARTESIAN_POINT ( 'NONE',  ( -7.104109303880803417, 8.350844278358124484, 1.082531754730549967 ) ) ;
#78767 = CARTESIAN_POINT ( 'NONE',  ( 5.467019156909919353, -1.422831870918849217, 1.121200454338074692 ) ) ;
#78768 = CARTESIAN_POINT ( 'NONE',  ( 6.051949806467664672, 0.9910487912591151582, 1.639330874965704732 ) ) ;
#78769 = CARTESIAN_POINT ( 'NONE',  ( 3.469446951953614189E-15, 6.120000000000021423, 1.214306433183764966E-14 ) ) ;
#78770 = CARTESIAN_POINT ( 'NONE',  ( 6.737182200980119440, -1.669782060861616291, 0.8434366901180423426 ) ) ;
#78771 = DIRECTION ( 'NONE',  ( 0.000000000000000000, 1.000000000000000000, 0.000000000000000000 ) ) ;
#78772 = CARTESIAN_POINT ( 'NONE',  ( 6.438360790777991838, 1.751285973423050368, 0.2548140705225035441 ) ) ;
#78774 = CIRCLE ( 'NONE', #75389, 2.000000000000000000 ) ;
#78773 = AXIS2_PLACEMENT_3D ( 'NONE', #84161, #67875, #102548 ) ;
#78775 = CARTESIAN_POINT ( 'NONE',  ( 1.657435761918718331, 1.928256795251210631, -0.5899901959932273288 ) ) ;
#78777 = CARTESIAN_POINT ( 'NONE',  ( 2.807361190694975139, 1.779531611039061767, 1.126096823879179754 ) ) ;
#78776 = CARTESIAN_POINT ( 'NONE',  ( -8.371269781434001800, 11.85389961405997816, -1.199719254218446718 ) ) ;
#78778 = CARTESIAN_POINT ( 'NONE',  ( 7.560643217915098191, 11.97250085420964716, -0.7998128361456291469 ) ) ;
#78780 = CARTESIAN_POINT ( 'NONE',  ( -7.492852449846775897, 11.89341162479659531, 0.000000000000000000 ) ) ;
#78779 = CARTESIAN_POINT ( 'NONE',  ( 1.499999999999985123, -0.9541666666666493990, -0.8660254037844323793 ) ) ;
#78781 = CARTESIAN_POINT ( 'NONE',  ( -11.80247861663003484, 11.29999999999997939, 1.695431928471866190 ) ) ;
#78782 = CARTESIAN_POINT ( 'NONE',  ( 2.988540512386147707, -1.199814222051265311, 1.624667845120256748 ) ) ;
#78783 = CARTESIAN_POINT ( 'NONE',  ( 0.6823417656249899377, 3.092708333674754062, 1.181850606188765695 ) ) ;
#78784 = CARTESIAN_POINT ( 'NONE',  ( 10.41229878561526512, 11.25002945941372623, -0.7216878364870257245 ) ) ;
#78785 = CARTESIAN_POINT ( 'NONE',  ( 3.567792053227138105, 2.109782723108716063, -0.4697668898906853796 ) ) ;
#78786 = CARTESIAN_POINT ( 'NONE',  ( 1.445103857048098739, 8.688264192037886247, -2.625611233228243968 ) ) ;
#78787 = CARTESIAN_POINT ( 'NONE',  ( 6.424584688029230328, 8.588711117491191871, 1.599625672291268286 ) ) ;
#78788 = CARTESIAN_POINT ( 'NONE',  ( 9.531018800282609504, 10.22186947652563305, 0.7216878364870458196 ) ) ;
#78790 = CARTESIAN_POINT ( 'NONE',  ( 9.278968692716386357, 13.84997945651597639, -7.537346677959899210 ) ) ;
#78789 = CARTESIAN_POINT ( 'NONE',  ( 0.3093308919281665959, -1.743438469055924145, 1.293836907758689758 ) ) ;
#78791 = CARTESIAN_POINT ( 'NONE',  ( -6.941411460516810017, 8.161030127766803588, 1.082531754730549967 ) ) ;
#78792 = CARTESIAN_POINT ( 'NONE',  ( -0.6823417656250246877, 0.5510416670080897639, 1.181850606188755259 ) ) ;
#78793 = CARTESIAN_POINT ( 'NONE',  ( 2.050558489324630251, -1.691691439650149897, 1.393213601605561180 ) ) ;
#78794 = CARTESIAN_POINT ( 'NONE',  ( 6.883263157960364254, 2.431740398616466070, 2.435552827938294751 ) ) ;
#78795 = CARTESIAN_POINT ( 'NONE',  ( 2.923041840916926315, 2.129999922893408559, 0.7632657742467786610 ) ) ;
#78796 = CARTESIAN_POINT ( 'NONE',  ( -7.320512876374914768, 10.62801655815766999, 1.199719254218453823 ) ) ;
#78797 = CARTESIAN_POINT ( 'NONE',  ( -3.375617059678305054, 5.921675088724528635, 1.082531754730560403 ) ) ;
#78798 = CARTESIAN_POINT ( 'NONE',  ( -0.6823417656250003738, 3.030208333674754062, -1.181850606188749264 ) ) ;
#78799 = CARTESIAN_POINT ( 'NONE',  ( 5.916355900263067014, 7.140870225795406867, 1.119544393390920600 ) ) ;
#78800 = CARTESIAN_POINT ( 'NONE',  ( 1.500000000000001332, 12.62499999999999645, 0.000000000000000000 ) ) ;
#78801 = CARTESIAN_POINT ( 'NONE',  ( 6.048345925472178308, 9.110135108809304327, 1.082531754730549967 ) ) ;
#78802 = CARTESIAN_POINT ( 'NONE',  ( 3.883871017828253613, -0.8741022562178245581, 1.538735937109585672 ) ) ;
#78803 = AXIS2_PLACEMENT_3D ( 'NONE', #18823, #23896, #184526 ) ;
#78804 = CARTESIAN_POINT ( 'NONE',  ( 9.585778300061798873, 11.14216175728232550, -1.199719254218440723 ) ) ;
#78805 = CARTESIAN_POINT ( 'NONE',  ( 0.3410288278610376089, 0.3603064943271740428, 2.074735154451929020 ) ) ;
#78806 = CARTESIAN_POINT ( 'NONE',  ( -0.6823417656250039265, 9.817708333674735499, -1.181850606188755259 ) ) ;
#78807 = CARTESIAN_POINT ( 'NONE',  ( -4.125423880308188629, 8.035021303660014880, -0.7998128361456481317 ) ) ;
#78808 = CARTESIAN_POINT ( 'NONE',  ( 6.327749939939701918, 0.7691082200134462532, -1.864175038933602924 ) ) ;
#78809 = EDGE_LOOP ( 'NONE', ( #96308, #119340, #4390, #170228 ) ) ;
#78810 = AXIS2_PLACEMENT_3D ( 'NONE', #207538, #26655, #143663 ) ;
#78811 = CARTESIAN_POINT ( 'NONE',  ( 8.778014389843965759, 12.32843499053828928, 1.199719254218450271 ) ) ;
#78812 = CARTESIAN_POINT ( 'NONE',  ( 3.836663719693265584, 0.2738035037005565053, 1.850374562403465983 ) ) ;
#78813 = CARTESIAN_POINT ( 'NONE',  ( 2.887621454190898884, -1.933326653459125355, 0.7409182656877840722 ) ) ;
#78814 = CARTESIAN_POINT ( 'NONE',  ( -6.631346530415505036, 7.869564052640446228, 1.082531754730549078 ) ) ;
#78815 = SURFACE_SIDE_STYLE ('',( #194706 ) ) ;
#78816 = CARTESIAN_POINT ( 'NONE',  ( -1.554911173149791992, 8.692115300649543741, 2.503913477513654673 ) ) ;
#78817 = CARTESIAN_POINT ( 'NONE',  ( -4.000897611406796450, 7.681767652865702622, 0.01012816533798947816 ) ) ;
#78818 = CARTESIAN_POINT ( 'NONE',  ( 6.174726448494309849, -2.051094451480539149, -0.6828207641706719455 ) ) ;
#78819 = CARTESIAN_POINT ( 'NONE',  ( -0.6823417656249969321, 5.030208333674755394, -1.181850606188749264 ) ) ;
#78820 = CARTESIAN_POINT ( 'NONE',  ( 3.314850587115983238, -1.487306837207631238, 1.279512770686676681 ) ) ;
#78821 = EDGE_CURVE ( 'NONE', #99737, #127411, #150332, .T. ) ;
#78822 = CARTESIAN_POINT ( 'NONE',  ( 0.6673420201736456336, -0.6766069248959758475, -1.899328980164962655 ) ) ;
#78823 = CARTESIAN_POINT ( 'NONE',  ( -5.157951095356222204, 4.982307464195829816, 0.000000000000000000 ) ) ;
#78825 = CARTESIAN_POINT ( 'NONE',  ( -11.94105721237523099, 13.52740390989733221, -1.187919463087249827 ) ) ;
#78824 = CARTESIAN_POINT ( 'NONE',  ( 7.248805684800777804, 11.60869039890961218, 1.040834085586084257E-14 ) ) ;
#78826 = CARTESIAN_POINT ( 'NONE',  ( 0.7021627906659900775, -0.6242572379067250488, -1.763460184394528341 ) ) ;
#78827 = CARTESIAN_POINT ( 'NONE',  ( -0.6823417656250212460, 3.551041667008085323, 1.181850606188767472 ) ) ;
#78828 = CARTESIAN_POINT ( 'NONE',  ( 2.795184176893855899, -0.1524655061851394322, -2.007514041822997086 ) ) ;
#78830 = CARTESIAN_POINT ( 'NONE',  ( 2.249754300142119856, 2.075745305004289332, -0.4162820868813913999 ) ) ;
#78829 = CARTESIAN_POINT ( 'NONE',  ( -6.236387472606158333, 7.338502141871059870, -1.082531754730544860 ) ) ;
#78831 = CARTESIAN_POINT ( 'NONE',  ( 7.873842894595653341, 14.32264345063075694, -9.058338245841589753 ) ) ;
#78832 = CARTESIAN_POINT ( 'NONE',  ( 4.000488093070094564, 2.060113009926473726, 0.2059288336104248551 ) ) ;
#78833 = CARTESIAN_POINT ( 'NONE',  ( 6.373214726875630731, 9.593111727067046957, 1.199719254218452047 ) ) ;
#78835 = CARTESIAN_POINT ( 'NONE',  ( 3.623053363349855172, 5.249981562040033189, 1.599625672291267398 ) ) ;
#78834 = CARTESIAN_POINT ( 'NONE',  ( -0.07645973585807680495, -1.289725328510348934, -1.646077999003342729 ) ) ;
#78837 = EDGE_LOOP ( 'NONE', ( #28212, #4227, #60892, #64086 ) ) ;
#78836 = CARTESIAN_POINT ( 'NONE',  ( 4.946237996787820279, 1.820793779319082706, 0.1331645236858983172 ) ) ;
#78838 = CARTESIAN_POINT ( 'NONE',  ( 7.832860060393120882, 10.16142270859057462, 1.599625672291281386 ) ) ;
#78839 = AXIS2_PLACEMENT_3D ( 'NONE', #140736, #206748, #42149 ) ;
#78840 = CARTESIAN_POINT ( 'NONE',  ( 3.733524485140474969, 7.410126666105378845, -2.499999999999779288 ) ) ;
#78841 = CARTESIAN_POINT ( 'NONE',  ( 9.742269887272128059, 13.15996534559037912, -8.088430353861673083 ) ) ;
#78842 = CARTESIAN_POINT ( 'NONE',  ( 6.704147062870869256, -2.206433763861126884, 0.04732420095975712476 ) ) ;
#78843 = CARTESIAN_POINT ( 'NONE',  ( -8.012344526598182026E-15, 11.10937500034139802, -1.575800808251669460 ) ) ;
#78844 = CARTESIAN_POINT ( 'NONE',  ( 5.567032834676129305, -1.504811603839781631, 1.179860560037985895 ) ) ;
#78845 = CARTESIAN_POINT ( 'NONE',  ( -8.784793466650835825, 12.33634391347959713, 1.199719254218462483 ) ) ;
#78846 = CARTESIAN_POINT ( 'NONE',  ( 6.765682348419287173, 7.852049813699357728, 1.199719254218462483 ) ) ;
#78847 = CARTESIAN_POINT ( 'NONE',  ( 0.6801582343749917881, 1.005208333674747934, 1.178068619123807004 ) ) ;
#78848 = CARTESIAN_POINT ( 'NONE',  ( 4.663641652976547647, 4.543262804668490418, 1.214306433183764966E-14 ) ) ;
#78849 = CARTESIAN_POINT ( 'NONE',  ( 3.011882680530176604, 6.665613560593854459, 0.7998128361456341429 ) ) ;
#78850 = VERTEX_POINT ( 'NONE', #96416 ) ;
#78851 = CARTESIAN_POINT ( 'NONE',  ( -2.449742653233059286, 3.300000000000011369, 0.3999999999999750422 ) ) ;
#78852 = EDGE_CURVE ( 'NONE', #194558, #71109, #8382, .T. ) ;
#78853 = CARTESIAN_POINT ( 'NONE',  ( 4.569519670753737550, 1.814867081516871261, -0.4525428206468632975 ) ) ;
#78854 = CARTESIAN_POINT ( 'NONE',  ( 0.07700591528354748527, 7.629137130509112907, -2.510791685687420838 ) ) ;
#78855 = CARTESIAN_POINT ( 'NONE',  ( 5.668190738965027897, 8.770583741171307679, -1.199719254218452047 ) ) ;
#78856 = CARTESIAN_POINT ( 'NONE',  ( -0.4169036860910396713, 3.145283463680773828, -0.4342470185719663478 ) ) ;
#78857 = CARTESIAN_POINT ( 'NONE',  ( -5.488562097922137895, 7.488332829134150437, 1.250156803814896245 ) ) ;
#78858 =( BOUNDED_SURFACE ( )  B_SPLINE_SURFACE ( 3, 2, ( 
 ( #166825, #33616, #153769 ),
 ( #133286, #120273, #168944 ),
 ( #186247, #20546, #152697 ),
 ( #170002, #84494, #87694 ) ),
 .UNSPECIFIED., .F., .F., .T. ) 
 B_SPLINE_SURFACE_WITH_KNOTS ( ( 4, 4 ),
 ( 3, 3 ),
 ( 0.01133669335851669041, 0.01377857026255017818 ),
 ( 0.000000000000000000, 1.000000000000000000 ),
 .UNSPECIFIED. ) 
 GEOMETRIC_REPRESENTATION_ITEM ( )  RATIONAL_B_SPLINE_SURFACE ( (
 ( 1.000000000000000000, 0.7169883299103952945, 1.000000000000000000),
 ( 1.000000000000000000, 0.7174882367753899759, 1.000000000000000000),
 ( 1.000000000000000000, 0.7180609655871071917, 1.000000000000000000),
 ( 1.000000000000000000, 0.7187540731122940008, 1.000000000000000000) ) ) 
 REPRESENTATION_ITEM ( '' )  SURFACE ( )  );
#78859 = CARTESIAN_POINT ( 'NONE',  ( -7.212574532790110737, 7.517017831117667193, -0.7216878364870278340 ) ) ;
#78860 = CARTESIAN_POINT ( 'NONE',  ( 4.172158584703322681, 5.890604320285754980, -1.599625672291256295 ) ) ;
#78861 = CARTESIAN_POINT ( 'NONE',  ( 1.481237898015239418, -0.05359582033081673746, 1.968903824098491073 ) ) ;
#78862 = CARTESIAN_POINT ( 'NONE',  ( 3.023064714212614135, -1.777003028299545484, 0.9530295004822467719 ) ) ;
#78863 = CARTESIAN_POINT ( 'NONE',  ( -6.645467848992654858, 10.90479625713344625, 0.7998128361456481317 ) ) ;
#78864 = CARTESIAN_POINT ( 'NONE',  ( 5.041653019435334393, 6.975290837464928728, -1.599625672291269396 ) ) ;
#78865 = CARTESIAN_POINT ( 'NONE',  ( 6.775479680898270907, -7.217880409000325237, 6.775479680898254919 ) ) ;
#78866 = CARTESIAN_POINT ( 'NONE',  ( 3.837968455498752096, 2.180838135830205804, 0.2153102754597763235 ) ) ;
#78867 = CARTESIAN_POINT ( 'NONE',  ( -5.584636475198561989, 5.818617271341436137, -0.4844363064898093429 ) ) ;
#78868 = CARTESIAN_POINT ( 'NONE',  ( 1.957912498325198536, 1.921386756000037055, -0.1395382256239047214 ) ) ;
#78869 = CARTESIAN_POINT ( 'NONE',  ( -9.110189153378817295, 12.71597221466224603, 1.199719254218462483 ) ) ;
#78870 = CARTESIAN_POINT ( 'NONE',  ( 0.1331565106231329398, 0.7299000548664087429, -2.029785554894456556 ) ) ;
#78871 = CARTESIAN_POINT ( 'NONE',  ( 4.095971805104288599, 5.871996087412059140, 1.443375672974058777 ) ) ;
#78872 = CARTESIAN_POINT ( 'NONE',  ( 7.904567251967224095, 9.180748867838630645, 1.199719254218462483 ) ) ;
#78873 = CARTESIAN_POINT ( 'NONE',  ( 4.788000803920411386, 8.737751371215816576, 1.040834085586084257E-14 ) ) ;
#78874 = CARTESIAN_POINT ( 'NONE',  ( -2.456316247939677400, 8.205176026796131339, -2.499999999999995115 ) ) ;
#78875 = CARTESIAN_POINT ( 'NONE',  ( 5.153507786970260796, 7.105788066255672497, -1.443375672974078761 ) ) ;
#78876 = ORIENTED_EDGE ( 'NONE', *, *, #149964, .T. ) ;
#78878 = CARTESIAN_POINT ( 'NONE',  ( 1.752591402120354358, 1.991486659738419984, 0.2933061901304565011 ) ) ;
#78877 = CARTESIAN_POINT ( 'NONE',  ( 5.196754805642953556, 1.508532920973480795, 1.055450849767838317 ) ) ;
#78879 = CARTESIAN_POINT ( 'NONE',  ( 3.831692444270826226, -1.546495240224911250, 1.700404426133800939 ) ) ;
#78881 = CARTESIAN_POINT ( 'NONE',  ( 1.797469275952040979, -1.343413903288761313, -1.288013994602929646 ) ) ;
#78880 = CARTESIAN_POINT ( 'NONE',  ( -0.1288028175207089898, 5.718623287604398087, -2.868046808693432315 ) ) ;
#78882 = CARTESIAN_POINT ( 'NONE',  ( 1.001543065824772753E-15, -1.771874999522040861, 3.793834371823811669 ) ) ;
#78883 = DIRECTION ( 'NONE',  ( 1.000000000000000000, -0.000000000000000000, -0.000000000000000000 ) ) ;
#78884 = CARTESIAN_POINT ( 'NONE',  ( 5.783449990912790106, 0.1341079605299954347, -1.907733270042926810 ) ) ;
#78885 = CARTESIAN_POINT ( 'NONE',  ( -7.914208982075130905, 10.25632978388623684, -1.599625672291263179 ) ) ;
#78886 = CARTESIAN_POINT ( 'NONE',  ( -5.478903473698255588, 7.485416367438324059, -1.443375672974066548 ) ) ;
#78888 = CARTESIAN_POINT ( 'NONE',  ( 3.590566789841375339, -0.3639703897368729568, -1.834726254853453087 ) ) ;
#78887 = CARTESIAN_POINT ( 'NONE',  ( 4.370703248089922610, -0.001752428395085294443, -2.090933975693793911 ) ) ;
#78889 = CARTESIAN_POINT ( 'NONE',  ( 5.802526556968819804, 9.713438716531550554, -0.7216878364870267237 ) ) ;
#78890 = ADVANCED_FACE ( 'NONE', ( #80127 ), #15113, .T. ) ;
#78891 = LINE ( 'NONE', #189459, #112438 ) ;
#78892 = CARTESIAN_POINT ( 'NONE',  ( -1.500000000000001332, -1.099999999999982991, -2.579999999999989413 ) ) ;
#78893 = CARTESIAN_POINT ( 'NONE',  ( 4.723137274085514647, -0.08022016869785492110, 1.723147214940720762 ) ) ;
#78894 = CARTESIAN_POINT ( 'NONE',  ( -6.684333426737305572, 7.757142738403693727, -1.199719254218446718 ) ) ;
#78895 = CARTESIAN_POINT ( 'NONE',  ( 0.7560338623246564138, 1.671613681001963281, -0.4610611789691662632 ) ) ;
#78896 = FACE_OUTER_BOUND ( 'NONE', #162639, .T. ) ;
#78897 = CARTESIAN_POINT ( 'NONE',  ( 1.904329973710225055, 3.286760881231386211, 0.4119279214152646862 ) ) ;
#78898 = AXIS2_PLACEMENT_3D ( 'NONE', #176678, #44563, #78102 ) ;
#78899 =( NAMED_UNIT ( * ) PLANE_ANGLE_UNIT ( ) SI_UNIT ( $, .RADIAN. ) );
#78900 = CARTESIAN_POINT ( 'NONE',  ( 5.629782814718605977, 2.094415894289668678, -0.5717063696269225614 ) ) ;
#78901 = CARTESIAN_POINT ( 'NONE',  ( 4.934128534657983067, 0.9357288403324083292, -1.567518238613223813 ) ) ;
#78902 = CARTESIAN_POINT ( 'NONE',  ( 1.182386158793121256, 1.172985831986381955, -1.572276950389992933 ) ) ;
#78903 = CARTESIAN_POINT ( 'NONE',  ( 0.3338148283143215767, 0.6594671527525318711, -2.011992694175788188 ) ) ;
#78904 = CARTESIAN_POINT ( 'NONE',  ( -0.6823417656249969321, 4.280208333674755394, -1.181850606188749264 ) ) ;
#78905 = CARTESIAN_POINT ( 'NONE',  ( 10.61081979358357863, -7.079050064870602732, -0.4638907948587486230 ) ) ;
#78906 = CARTESIAN_POINT ( 'NONE',  ( 7.507464373665139412, 9.781794407407920389, 1.599625672291281386 ) ) ;
#78907 = CARTESIAN_POINT ( 'NONE',  ( 2.227333921462580246, 1.895369558270381338, 0.9509248740046101211 ) ) ;
#78908 = CARTESIAN_POINT ( 'NONE',  ( -2.819732761962332024, 6.233512622357263666, -0.7216878364870267237 ) ) ;
#78909 = CARTESIAN_POINT ( 'NONE',  ( -4.948362878863562742, 5.835806782504650236, 1.082531754730558626 ) ) ;
#78911 = AXIS2_PLACEMENT_3D ( 'NONE', #88931, #7640, #126831 ) ;
#78910 = CIRCLE ( 'NONE', #13226, 1.249999999999998890 ) ;
#78912 = CARTESIAN_POINT ( 'NONE',  ( 0.8485890540621650047, -2.054197865963180547, -0.2570499307305574299 ) ) ;
#78914 = CARTESIAN_POINT ( 'NONE',  ( -1.500000000000008216, 14.28125000068279604, 3.469446951953614189E-15 ) ) ;
#78913 = CARTESIAN_POINT ( 'NONE',  ( 6.883263157960404222, 4.689511904294953126, 2.716359706997414136 ) ) ;
#78916 = ORIENTED_EDGE ( 'NONE', *, *, #27372, .F. ) ;
#78915 = CARTESIAN_POINT ( 'NONE',  ( 2.139591745018020408, 0.003451857093505344976, 2.221473417793240923 ) ) ;
#78917 = CARTESIAN_POINT ( 'NONE',  ( 1.108484992968819416, -0.04990477548066223068, 2.298298319747505758 ) ) ;
#78919 = CARTESIAN_POINT ( 'NONE',  ( 5.489153638472886954, 0.1464082308396240373, 2.057405090433866324 ) ) ;
#78918 = CARTESIAN_POINT ( 'NONE',  ( 2.361091307074211887, 5.906356958228550447, 0.7998128361456462443 ) ) ;
#78921 = CARTESIAN_POINT ( 'NONE',  ( -3.475000000000000533, -1.779166666666666785, -2.006292185433948827 ) ) ;
#78920 = CARTESIAN_POINT ( 'NONE',  ( 4.505052181490820651, 8.477920988373101707, -0.7998128361456381397 ) ) ;
#78922 = CARTESIAN_POINT ( 'NONE',  ( 5.956828388357757298, 8.042995434541133193, 1.599625672291269396 ) ) ;
#78923 = CARTESIAN_POINT ( 'NONE',  ( 0.000000000000000000, 13.20000000000000284, -1.540450515248283025 ) ) ;
#78924 = CARTESIAN_POINT ( 'NONE',  ( 5.407694413872749628, -0.8332299576223768378, -1.642021276980778932 ) ) ;
#78925 = EDGE_CURVE ( 'NONE', #119756, #93109, #103916, .T. ) ;
#78926 = CARTESIAN_POINT ( 'NONE',  ( 4.216749469050096621, 4.878294787768598262, -1.199719254218452047 ) ) ;
#78927 =( NAMED_UNIT ( * ) SI_UNIT ( $, .STERADIAN. ) SOLID_ANGLE_UNIT ( ) );
#78928 = CARTESIAN_POINT ( 'NONE',  ( 1.641173577361688896, -1.245895879902914727, -1.192971367628747448 ) ) ;
#78929 = CARTESIAN_POINT ( 'NONE',  ( 1.604704241733472037, 1.883313803065278513, 0.7212895827233902768 ) ) ;
#78930 = CARTESIAN_POINT ( 'NONE',  ( 1.706133075696044221, 2.146806223983906747, 0.8221538945956968769 ) ) ;
#78931 = CARTESIAN_POINT ( 'NONE',  ( 1.364683531249990311, 4.196875000341417028, 1.214306433183764966E-14 ) ) ;
#78932 = CARTESIAN_POINT ( 'NONE',  ( 2.267197333419627370, -2.067742563539621603, -0.9185262150545376869 ) ) ;
#78933 = CARTESIAN_POINT ( 'NONE',  ( 4.283879487498391647, 1.375451533845202245, 1.594966088981208729 ) ) ;
#78934 = CARTESIAN_POINT ( 'NONE',  ( -7.431277594066152403, 8.802816960232885179, -1.082531754730549967 ) ) ;
#78935 = CARTESIAN_POINT ( 'NONE',  ( 3.620126565017945275, 1.124893713931356842, -1.366185836280229715 ) ) ;
#78936 = CARTESIAN_POINT ( 'NONE',  ( 4.476163270806094552, 8.373940915915776273, 0.7998128361456462443 ) ) ;
#78938 = CARTESIAN_POINT ( 'NONE',  ( 0.02392203315931124008, -1.416205114373503715, -1.803417470570017000 ) ) ;
#78937 = CARTESIAN_POINT ( 'NONE',  ( 3.377389663135653031, 6.954388683717978026, -0.7216878364870338292 ) ) ;
#78939 = CARTESIAN_POINT ( 'NONE',  ( 4.699059028873219468, -0.4882365319774860102, 1.775153104902137624 ) ) ;
#78940 = CARTESIAN_POINT ( 'NONE',  ( -5.057354993097396445, 5.859001232490445688, -1.199719254218446718 ) ) ;
#78941 = CARTESIAN_POINT ( 'NONE',  ( 0.7499999999999902300, 3.816666666666690411, -1.299038105676658228 ) ) ;
#78942 = CARTESIAN_POINT ( 'NONE',  ( 4.611385148785618782, -2.149487334021232599, 0.4259423572047504880 ) ) ;
#78943 = CARTESIAN_POINT ( 'NONE',  ( -3.411848212133334446, 7.132240014130862171, 0.7998128361456341429 ) ) ;
#78944 = CARTESIAN_POINT ( 'NONE',  ( 8.881784197001254049E-17, 3.599999999999999201, -1.600000000000005196 ) ) ;
#78945 = ADVANCED_FACE ( 'NONE', ( #130037 ), #111290, .T. ) ;
#78946 = CARTESIAN_POINT ( 'NONE',  ( 0.4645846211130746917, -7.563986176625375535, 10.12536109763334302 ) ) ;
#78947 = MECHANICAL_DESIGN_GEOMETRIC_PRESENTATION_REPRESENTATION (  '', ( #61646 ), #9688 ) ;
#78948 =( BOUNDED_SURFACE ( )  B_SPLINE_SURFACE ( 3, 2, ( 
 ( #195212, #164837, #147536 ),
 ( #46848, #213557, #112962 ),
 ( #178974, #65179, #96672 ),
 ( #48969, #131333, #144374 ),
 ( #60939, #162722, #176826 ),
 ( #14294, #197327, #193059 ) ),
 .UNSPECIFIED., .F., .F., .F. ) 
 B_SPLINE_SURFACE_WITH_KNOTS ( ( 4, 2, 4 ),
 ( 3, 3 ),
 ( 0.000000000000000000, 0.0003831416164015018179, 0.0007662832328030036357 ),
 ( 0.000000000000000000, 1.000000000000000000 ),
 .UNSPECIFIED. ) 
 GEOMETRIC_REPRESENTATION_ITEM ( )  RATIONAL_B_SPLINE_SURFACE ( (
 ( 1.000000000000000000, 0.7071067811865475727, 1.000000000000000000),
 ( 1.000000000000000000, 0.6829713513653348222, 1.000000000000000000),
 ( 1.000000000000000000, 0.6534833722372194176, 1.000000000000000000),
 ( 1.000000000000000000, 0.6054027484662655167, 1.000000000000000000),
 ( 1.000000000000000000, 0.5875453974414869274, 1.000000000000000000),
 ( 1.000000000000000000, 0.5879095031487528988, 1.000000000000000000) ) ) 
 REPRESENTATION_ITEM ( '' )  SURFACE ( )  );
#78949 = CARTESIAN_POINT ( 'NONE',  ( -1.364683531250010295, 4.280208333674753618, 0.7879004041258379498 ) ) ;
#78950 = CARTESIAN_POINT ( 'NONE',  ( 2.842313889931574522, 1.911971217405187495, 0.2356370756458354143 ) ) ;
#78951 = CARTESIAN_POINT ( 'NONE',  ( -1.364683531250014514, 9.088541667008060543, -0.7879004041258335089 ) ) ;
#78952 = CARTESIAN_POINT ( 'NONE',  ( -4.785665035943912571, 4.685623418130398399, 1.214306433183764966E-14 ) ) ;
#78953 = CARTESIAN_POINT ( 'NONE',  ( 0.2291713999985908190, 1.525799623841477493, -1.614749986458098974 ) ) ;
#78954 = CARTESIAN_POINT ( 'NONE',  ( -4.489158259900630554, 8.251452046610447510, 0.000000000000000000 ) ) ;
#78955 = EDGE_LOOP ( 'NONE', ( #41673, #64165, #157704, #192936 ) ) ;
#78957 = CARTESIAN_POINT ( 'NONE',  ( 4.234574664202256145, 7.152588777595761727, 1.178691574056603075 ) ) ;
#78956 = CARTESIAN_POINT ( 'NONE',  ( -4.177320726786319049, 6.927272377009067839, -1.082531754730551743 ) ) ;
#78958 = CARTESIAN_POINT ( 'NONE',  ( 5.366329872910639232, 5.155139694684188534, 1.040834085586084257E-14 ) ) ;
#78959 = CARTESIAN_POINT ( 'NONE',  ( 4.204437033569277560, 7.919277282557212416, 0.000000000000000000 ) ) ;
#78960 = CARTESIAN_POINT ( 'NONE',  ( 0.7500000000000006661, 11.19791666734946212, -1.299038105676657340 ) ) ;
#78961 = CARTESIAN_POINT ( 'NONE',  ( 0.08113548435146850091, 6.430127061359857343, -3.206836081813071004 ) ) ;
#78962 = CARTESIAN_POINT ( 'NONE',  ( -1.364683531250012516, 3.551041667008086211, -0.7879004041258300672 ) ) ;
#78963 = CARTESIAN_POINT ( 'NONE',  ( 2.700428686635591546, 1.471443353139300081, 0.9291617766199999906 ) ) ;
#78964 = DIRECTION ( 'NONE',  ( 0.000000000000000000, 0.000000000000000000, 1.000000000000000000 ) ) ;
#78966 = CARTESIAN_POINT ( 'NONE',  ( 0.4671467121175365000, 1.705069321186868159, 0.9702857188121426502 ) ) ;
#78965 = PRESENTATION_LAYER_ASSIGNMENT (  '', '', ( #175935 ) ) ;
#78967 = CARTESIAN_POINT ( 'NONE',  ( 0.6823417656249882723, -0.2614583329919109578, -1.181850606188749264 ) ) ;
#78968 = CARTESIAN_POINT ( 'NONE',  ( -4.270528892807586629, 7.372556535914950082, -0.9884938994864488349 ) ) ;
#78969 = CARTESIAN_POINT ( 'NONE',  ( 6.262596564776618635, -1.532251275270900326, 1.525113613579494709 ) ) ;
#78970 = CARTESIAN_POINT ( 'NONE',  ( -8.448702279610222021, 13.00856975952063088, 1.040834085586084257E-14 ) ) ;
#78971 = CARTESIAN_POINT ( 'NONE',  ( -5.382223794500835545, 8.262716279350872384, -1.082531754730543971 ) ) ;
#78972 = CARTESIAN_POINT ( 'NONE',  ( 5.313408243115379292, -0.3210861823062813314, 2.137610926513198617 ) ) ;
#78974 = ORIENTED_EDGE ( 'NONE', *, *, #45594, .T. ) ;
#78973 = CARTESIAN_POINT ( 'NONE',  ( -0.2104748580754183529, 0.2283854016844401591, -2.137091067173245929 ) ) ;
#78975 = CARTESIAN_POINT ( 'NONE',  ( -1.364683531250010295, 5.030208333674757171, 0.7879004041258379498 ) ) ;
#78976 = CARTESIAN_POINT ( 'NONE',  ( 6.573508854753547404, 1.887220770608761589, -0.5698601248695351895 ) ) ;
#78977 = CARTESIAN_POINT ( 'NONE',  ( 6.186827581914116081, -0.9662774195124073096, -1.439361474112188954 ) ) ;
#78978 = ADVANCED_FACE ( 'NONE', ( #168343 ), #53521, .T. ) ;
#78980 = CARTESIAN_POINT ( 'NONE',  ( 2.982162443640325566, -2.159563097825706990, -0.3721831821169723775 ) ) ;
#78979 = CARTESIAN_POINT ( 'NONE',  ( 1.360316468749955598, -0.005208332991877948244, 0.7853790794158660438 ) ) ;
#78981 = CARTESIAN_POINT ( 'NONE',  ( 3.452467797911736636, 2.307758715189492271, 0.002325993833134780940 ) ) ;
#78982 = CARTESIAN_POINT ( 'NONE',  ( 6.169226111886771946, 0.1559856310293654957, -2.054958193847939096 ) ) ;
#78983 = CARTESIAN_POINT ( 'NONE',  ( 1.517416608934060385, -1.078585517578967368, -1.614684294522166663 ) ) ;
#78984 = CARTESIAN_POINT ( 'NONE',  ( -6.087247782411500552, 7.164505836643929371, 1.082531754730549967 ) ) ;
#78986 = EDGE_CURVE ( 'NONE', #159016, #86684, #2970, .T. ) ;
#78985 = CARTESIAN_POINT ( 'NONE',  ( 2.200495758195375906, 5.718995484536574025, -0.2758893754505519214 ) ) ;
#78987 = SURFACE_STYLE_USAGE ( .BOTH. , #27030 ) ;
#78988 = CARTESIAN_POINT ( 'NONE',  ( 4.535463010148616192, -0.1012041512906610846, 2.118281909017679432 ) ) ;
#78989 = CYLINDRICAL_SURFACE ( 'NONE', #171146, 10.75000000000000000 ) ;
#78990 = CARTESIAN_POINT ( 'NONE',  ( 2.233046271152541618, 2.016033844848092560, 0.04667593304989729741 ) ) ;
#78991 = CARTESIAN_POINT ( 'NONE',  ( -6.033015167956810920, 7.101234453113482559, -1.082531754730543083 ) ) ;
#78992 = CARTESIAN_POINT ( 'NONE',  ( 5.157340341976529352, -1.861842412690998039, -1.184373046124863160 ) ) ;
#78993 = CARTESIAN_POINT ( 'NONE',  ( -4.663391507278085157, 5.284333467198953471, 1.153445959906941320 ) ) ;
#78994 = DIRECTION ( 'NONE',  ( 3.330669073875478989E-16, -3.540251991789410786E-16, -1.000000000000000000 ) ) ;
#78995 = DIRECTION ( 'NONE',  ( 0.000000000000000000, 0.000000000000000000, 1.000000000000000000 ) ) ;
#78996 = CARTESIAN_POINT ( 'NONE',  ( -5.901542003698421190, 10.10715911428198055, 0.000000000000000000 ) ) ;
#78998 = FACE_OUTER_BOUND ( 'NONE', #79199, .T. ) ;
#78997 = CARTESIAN_POINT ( 'NONE',  ( -4.618765760061220860, 8.456409177651165621, 0.3783674834792974950 ) ) ;
#78999 = CARTESIAN_POINT ( 'NONE',  ( -10.83017591827266557, 4.360326817186668258, 4.636531744782178777 ) ) ;
#79000 = ORIENTED_EDGE ( 'NONE', *, *, #81687, .T. ) ;
#79001 = CARTESIAN_POINT ( 'NONE',  ( 4.944241404475337553, 2.055231674695843669, 0.1536075889326995458 ) ) ;
#79002 = CARTESIAN_POINT ( 'NONE',  ( 4.037162115432598064, 7.757183989314783368, -0.4293979441572001177 ) ) ;
#79003 = CARTESIAN_POINT ( 'NONE',  ( -5.091250377131585125, 5.898545847196970726, 1.199719254218450271 ) ) ;
#79004 = CARTESIAN_POINT ( 'NONE',  ( 6.966220764712143243, 6.002124920821316323, -2.500000000000000444 ) ) ;
#79005 = CARTESIAN_POINT ( 'NONE',  ( 3.703775025860293724, 1.464345522003915878, 1.391222453660536873 ) ) ;
#79006 = CARTESIAN_POINT ( 'NONE',  ( 1.499999999999989120, 1.025000000000019007, 0.000000000000000000 ) ) ;
#79007 = AXIS2_PLACEMENT_3D ( 'NONE', #15898, #198907, #148070 ) ;
#79009 = CARTESIAN_POINT ( 'NONE',  ( 8.920901888111997025, 10.47043562662792304, 1.082531754730549967 ) ) ;
#79008 = CARTESIAN_POINT ( 'NONE',  ( -4.736594563127865420, 6.619389305106191834, -1.599625672291271394 ) ) ;
#79010 = CARTESIAN_POINT ( 'NONE',  ( 5.849453209292126310, 8.911780279894442103, 1.199719254218462483 ) ) ;
#79011 = CARTESIAN_POINT ( 'NONE',  ( 2.571226905367568261, 0.1023410288747768487, -2.058482174549924437 ) ) ;
#79012 = CARTESIAN_POINT ( 'NONE',  ( 2.672500184003968382, 1.427937546361924381, 1.423961308954827754 ) ) ;
#79013 = ORIENTED_EDGE ( 'NONE', *, *, #173301, .F. ) ;
#79014 = DIRECTION ( 'NONE',  ( 0.1774649537764392826, 0.000000000000000000, 0.9841271209458288816 ) ) ;
#79015 = CARTESIAN_POINT ( 'NONE',  ( 6.654354466208897811, 6.657835053532175529, 0.7998128361456341429 ) ) ;
#79017 = EDGE_LOOP ( 'NONE', ( #142319, #116679, #164190, #18899, #20228 ) ) ;
#79016 = CARTESIAN_POINT ( 'NONE',  ( -0.1471985351163795641, 7.029189141431414711, -1.995741298138918207 ) ) ;
#79018 = CARTESIAN_POINT ( 'NONE',  ( 3.216172551982798833, -1.646586737935524125, -1.163091166099708529 ) ) ;
#79019 = CARTESIAN_POINT ( 'NONE',  ( 2.782953997937851920, 1.302219384484751830, 1.301801165952347628 ) ) ;
#79020 = CARTESIAN_POINT ( 'NONE',  ( 6.164705905600972535, -1.563586322211576674, 1.557672334054376773 ) ) ;
#79021 = CARTESIAN_POINT ( 'NONE',  ( 3.549202351727371862, 7.362762853649070571, -0.7998128361456362523 ) ) ;
#79022 = CARTESIAN_POINT ( 'NONE',  ( 2.249508738127777630, -1.734628566516350778, -1.289557925820798090 ) ) ;
#79023 =( GEOMETRIC_REPRESENTATION_CONTEXT ( 3 ) GLOBAL_UNCERTAINTY_ASSIGNED_CONTEXT ( ( #179421 ) ) GLOBAL_UNIT_ASSIGNED_CONTEXT ( ( #83581, #133444, #117217 ) ) REPRESENTATION_CONTEXT ( 'NONE', 'WORKASPACE' ) );
#79024 = CARTESIAN_POINT ( 'NONE',  ( -3.118012141462980669, 6.581505231774690046, 0.7216878364870317197 ) ) ;
#79025 = CARTESIAN_POINT ( 'NONE',  ( 4.171193994350897327, 1.889596262492127199, -0.9554925290978563135 ) ) ;
#79026 = ORIENTED_EDGE ( 'NONE', *, *, #152781, .F. ) ;
#79027 = CARTESIAN_POINT ( 'NONE',  ( 3.600749563572586798, 3.160087278257122989, -2.499999999999995115 ) ) ;
#79028 = CARTESIAN_POINT ( 'NONE',  ( 1.059204734455133412, 0.3686402435371800013, -1.833797362824276078 ) ) ;
#79029 = CARTESIAN_POINT ( 'NONE',  ( 5.664905584638975533, -1.781982755157806908, -0.8436340872482649411 ) ) ;
#79031 = CARTESIAN_POINT ( 'NONE',  ( 9.381879110532285182, 10.04787317181692075, 0.000000000000000000 ) ) ;
#79030 = CARTESIAN_POINT ( 'NONE',  ( -1.364683531250012516, 3.738541667008087099, -0.7879004041258300672 ) ) ;
#79033 = CARTESIAN_POINT ( 'NONE',  ( 0.9442952520863318044, 0.8911936224933308948, -2.019119535841918278 ) ) ;
#79032 = CARTESIAN_POINT ( 'NONE',  ( -7.400052914960538963, 7.527816577075747695, 1.040834085586084257E-14 ) ) ;
#79034 = B_SPLINE_CURVE_WITH_KNOTS ( 'NONE', 3,
 ( #46399, #15987, #196895, #97287, #34387, #31214, #179593 ),
 .UNSPECIFIED., .F., .F.,
 ( 4, 3, 4 ),
 ( 2.452946696045431814E-07, 0.0004046562657335614943, 0.0006364688305826464486 ),
 .UNSPECIFIED. ) ;
#79035 = CARTESIAN_POINT ( 'NONE',  ( 5.986797818411375260, 1.994257276370488219, 0.5558945855626205024 ) ) ;
#79036 = CARTESIAN_POINT ( 'NONE',  ( 6.844168616800228477, 6.879284895888727824, -0.7998128361456281477 ) ) ;
#79037 = CARTESIAN_POINT ( 'NONE',  ( -6.144869935491728441, 8.192100896205577243, -1.599625672291263179 ) ) ;
#79038 = CARTESIAN_POINT ( 'NONE',  ( 6.639320575229257670, 2.957073754255258535, 2.555924021811271096 ) ) ;
#79039 = CARTESIAN_POINT ( 'NONE',  ( 4.891463287051191600, 1.460324016362057886, 1.324601213698357149 ) ) ;
#79040 = CARTESIAN_POINT ( 'NONE',  ( 6.398695825915057256, -1.981597308308700844, -0.3899587018172407382 ) ) ;
#79041 = CARTESIAN_POINT ( 'NONE',  ( 1.499999999999987121, 0.5770833340161539704, -0.8660254037844253849 ) ) ;
#79042 = CARTESIAN_POINT ( 'NONE',  ( 4.705897867575262516, -0.6186405800616563422, 2.223174812903663256 ) ) ;
#79043 = CARTESIAN_POINT ( 'NONE',  ( 2.325117943063298664, -1.883989625962046555, -0.8399396378151212650 ) ) ;
#79044 = CARTESIAN_POINT ( 'NONE',  ( 6.805829924380108586, 8.963220883242035697, 1.443375672974076540 ) ) ;
#79045 = CARTESIAN_POINT ( 'NONE',  ( 4.179656494762836516, 8.098292687190454586, -0.7998128361456362523 ) ) ;
#79046 = CARTESIAN_POINT ( 'NONE',  ( 3.576318658954677598, 7.394398545414291313, 0.7998128361456281477 ) ) ;
#79047 = CARTESIAN_POINT ( 'NONE',  ( -1.364683531250012516, 1.842708333674749843, 0.7879004041258379498 ) ) ;
#79048 = CARTESIAN_POINT ( 'NONE',  ( 4.309512724297349884, 6.121127159803966933, 1.599625672291261402 ) ) ;
#79049 = CARTESIAN_POINT ( 'NONE',  ( 4.785665035499516051, 8.527100274817353665, -0.7216878364870207285 ) ) ;
#79050 = CARTESIAN_POINT ( 'NONE',  ( 3.965408508876398841, 1.860285638359628235, 1.119340054616506874 ) ) ;
#79052 = CARTESIAN_POINT ( 'NONE',  ( 3.667381569930192597, 1.025862638139760419, 1.528780434079744843 ) ) ;
#79051 = CARTESIAN_POINT ( 'NONE',  ( -4.446711195602264688, 4.290177271065136466, -0.7216878364870207285 ) ) ;
#79054 = CARTESIAN_POINT ( 'NONE',  ( 6.620655732516627090, 3.711369741872071693, 2.240970959566997323 ) ) ;
#79053 = CARTESIAN_POINT ( 'NONE',  ( 1.364683531249988535, 5.155208333674749177, -0.7879004041258300672 ) ) ;
#79055 = CARTESIAN_POINT ( 'NONE',  ( 4.950807510372833065, -1.851323926424643274, -1.172527737679923465 ) ) ;
#79056 = CARTESIAN_POINT ( 'NONE',  ( 6.104402428500737443, -0.8075561382203682026, -2.113670588390024196 ) ) ;
#79057 = EDGE_LOOP ( 'NONE', ( #185327, #164167, #97790, #178788 ) ) ;
#79058 = CARTESIAN_POINT ( 'NONE',  ( -4.351531800032816477, 7.393666969396889499, -1.175081553336376317 ) ) ;
#79059 = CARTESIAN_POINT ( 'NONE',  ( 5.184698244283005408, 7.856242361780820360, 1.254847465626233616 ) ) ;
#79060 = CARTESIAN_POINT ( 'NONE',  ( -5.519577934094894722, 7.532869904567736974, 1.443375672974058777 ) ) ;
#79061 = CARTESIAN_POINT ( 'NONE',  ( -2.981281212289682792, 6.492261378021210838, -0.0003813922843012157449 ) ) ;
#79062 = CARTESIAN_POINT ( 'NONE',  ( 1.146904862891504173, -1.391901254704702273, -1.093021760518765539 ) ) ;
#79064 = CARTESIAN_POINT ( 'NONE',  ( 5.690095194620785612, 1.200872180055783112, 1.615535318972769474 ) ) ;
#79063 = VECTOR ( 'NONE', #145015, 1000.000000000000000 ) ;
#79065 = CARTESIAN_POINT ( 'NONE',  ( 6.819914962873951936, 7.915321197229798322, -1.199719254218446718 ) ) ;
#79066 = CARTESIAN_POINT ( 'NONE',  ( 4.085071245346539648, -0.2040513417298230325, -2.096037468315871788 ) ) ;
#79067 = CARTESIAN_POINT ( 'NONE',  ( 1.722145930190256191, 1.895023070986867619, 0.2790570245742740041 ) ) ;
#79068 = CARTESIAN_POINT ( 'NONE',  ( 5.169736645512481132, 4.925780929386339935, 0.7998128361456341429 ) ) ;
#79069 = CARTESIAN_POINT ( 'NONE',  ( 2.664455434096600683, -0.7511504341344789060, -1.820894044046962534 ) ) ;
#79070 = CARTESIAN_POINT ( 'NONE',  ( 5.765880396963712684, 0.5824918586248282182, -1.933996001582516611 ) ) ;
#79071 = CARTESIAN_POINT ( 'NONE',  ( 1.762360912074714125, -1.325010844092512796, 1.320751239342173200 ) ) ;
#79072 = CARTESIAN_POINT ( 'NONE',  ( 2.523818479427087702, 1.924573107942130656, -0.3798230296482503210 ) ) ;
#79075 = ORIENTED_EDGE ( 'NONE', *, *, #42883, .T. ) ;
#79074 = CARTESIAN_POINT ( 'NONE',  ( 1.230557176020010912, 1.282188879665364656, -1.419081615486268433 ) ) ;
#79073 = CARTESIAN_POINT ( 'NONE',  ( 4.916472993244619616, 1.186103633638861288, -1.252587755385982771 ) ) ;
#79077 = CARTESIAN_POINT ( 'NONE',  ( 6.493992391265805075, 6.678671999339316656, 1.040834085586084257E-14 ) ) ;
#79076 = CARTESIAN_POINT ( 'NONE',  ( 1.331021600797330118, 2.127646391749141941, 0.5858054460900484761 ) ) ;
#79078 = CARTESIAN_POINT ( 'NONE',  ( 0.6823417656249899377, 1.905208333674752952, 1.181850606188755259 ) ) ;
#79079 = CARTESIAN_POINT ( 'NONE',  ( 7.944187942603509356, 11.35563746875774882, 1.199719254218460707 ) ) ;
#79080 = CARTESIAN_POINT ( 'NONE',  ( 11.92619526913700057, 10.89999999999998259, 1.328859060402682868 ) ) ;
#79081 = DIRECTION ( 'NONE',  ( 0.000000000000000000, 0.000000000000000000, 1.000000000000000000 ) ) ;
#79082 = CARTESIAN_POINT ( 'NONE',  ( -5.607971574822836480, 5.595440440058774278, -0.3944387069941719393 ) ) ;
#79083 = CARTESIAN_POINT ( 'NONE',  ( 6.174686067066744499, 1.394736081427111252, -1.530067588329916628 ) ) ;
#79084 = VECTOR ( 'NONE', #211849, 1000.000000000000000 ) ;
#79085 = CARTESIAN_POINT ( 'NONE',  ( 1.363825363374836286, -0.5049007678423790280, 2.007717453658082629 ) ) ;
#79086 = CARTESIAN_POINT ( 'NONE',  ( -1.500000000000013101, 1.879166666666692187, -0.8660254037844313801 ) ) ;
#79087 = CARTESIAN_POINT ( 'NONE',  ( 4.788000803920411386, 8.737751371215816576, 1.040834085586084257E-14 ) ) ;
#79088 = CARTESIAN_POINT ( 'NONE',  ( -6.039267359883488950, 9.133230122250985517, 1.199719254218452047 ) ) ;
#79089 = CARTESIAN_POINT ( 'NONE',  ( 4.016958651398847557, 7.908478536599129249, -0.7998128361456362523 ) ) ;
#79090 = CARTESIAN_POINT ( 'NONE',  ( 4.916704032076687270, -0.7149955815140829340, -1.996424279390257572 ) ) ;
#79091 = CARTESIAN_POINT ( 'NONE',  ( 4.760848217054122422, 5.583353003765119560, -1.199719254218452047 ) ) ;
#79092 = CARTESIAN_POINT ( 'NONE',  ( -1.201851678989727383E-14, 2.071875000341422801, 1.575800808251672791 ) ) ;
#79093 = CARTESIAN_POINT ( 'NONE',  ( 1.499999999999989120, 3.254166666666690855, 0.8660254037844524744 ) ) ;
#79095 = CARTESIAN_POINT ( 'NONE',  ( 4.844340958784499662, 4.546152628203684820, 0.7998128361456341429 ) ) ;
#79094 = CARTESIAN_POINT ( 'NONE',  ( -1.115562610750309283E-14, 11.81249999999999822, 1.500000000000001554 ) ) ;
#79096 = CARTESIAN_POINT ( 'NONE',  ( 3.866564406427867251, -0.5879305547937460075, 1.928456347981069241 ) ) ;
#79097 = CARTESIAN_POINT ( 'NONE',  ( 3.626117945992116898, 1.907004414510531598, 0.1821707851048308124 ) ) ;
#79098 = CYLINDRICAL_SURFACE ( 'NONE', #75889, 1.250000000000000000 ) ;
#79099 = CARTESIAN_POINT ( 'NONE',  ( 2.085717061910817183, -0.9337068281064246911, 1.982830571388309204 ) ) ;
#79100 = CARTESIAN_POINT ( 'NONE',  ( -11.04536101718726293, 10.90000000000000036, -1.100000000000002087 ) ) ;
#79101 = CARTESIAN_POINT ( 'NONE',  ( -1.500000000000001332, 0.1812500006828157706, 0.000000000000000000 ) ) ;
#79102 = CARTESIAN_POINT ( 'NONE',  ( 5.414319639144633101, -2.013376227731620283, 0.004290823026709827959 ) ) ;
#79103 = CARTESIAN_POINT ( 'NONE',  ( -6.181627972826976958, 9.299317504018391745, 1.199719254218452047 ) ) ;
#79105 = CARTESIAN_POINT ( 'NONE',  ( 5.396159345875370938, -0.9528639288615829983, -1.890782970011774422 ) ) ;
#79104 = CARTESIAN_POINT ( 'NONE',  ( -2.657034918598338180, 6.043698471765932112, -0.7216878364870267237 ) ) ;
#79106 = CARTESIAN_POINT ( 'NONE',  ( 0.6823417656249969321, 8.588541667008065872, -1.181850606188757036 ) ) ;
#79108 = CARTESIAN_POINT ( 'NONE',  ( -7.957709816578236506, 8.248692638954882028, 0.7998128361456341429 ) ) ;
#79107 = CARTESIAN_POINT ( 'NONE',  ( 3.368770691598612643, 0.04892471221396628434, -2.090337739860036681 ) ) ;
#79110 = ORIENTED_EDGE ( 'NONE', *, *, #76805, .T. ) ;
#79109 = CARTESIAN_POINT ( 'NONE',  ( 2.150978262527812213, -1.382985381756835608, -1.030390371524889659 ) ) ;
#79111 = CARTESIAN_POINT ( 'NONE',  ( 5.572555445586866441, 0.8612648569810870125, 1.938019255899057658 ) ) ;
#79112 = CARTESIAN_POINT ( 'NONE',  ( 5.880485940025228508, 7.883652901494672349, 1.599625672291267398 ) ) ;
#79113 = EDGE_CURVE ( 'NONE', #23033, #139477, #152097, .T. ) ;
#79114 = CARTESIAN_POINT ( 'NONE',  ( -7.806764249273705047, -6.480061791515693947, -7.750016138724921788 ) ) ;
#79115 = DIRECTION ( 'NONE',  ( 1.000000000000000000, 0.000000000000000000, 0.000000000000000000 ) ) ;
#79116 = CIRCLE ( 'NONE', #186408, 0.08000000000000015432 ) ;
#79117 = DIRECTION ( 'NONE',  ( -0.000000000000000000, 1.000000000000000000, -0.000000000000000000 ) ) ;
#79118 = CARTESIAN_POINT ( 'NONE',  ( 6.063521013809720195, 8.097193820909906137, 1.599625672291281386 ) ) ;
#79119 = EDGE_LOOP ( 'NONE', ( #137193, #210067, #130624, #30627, #136521, #190684 ) ) ;
#79120 = CARTESIAN_POINT ( 'NONE',  ( -1.500000000000035971, 6.999999999999999112, -9.886859966642587594 ) ) ;
#79122 = CARTESIAN_POINT ( 'NONE',  ( 1.664434086620687703, 0.5685959063129341073, 1.719966406682835958 ) ) ;
#79121 = CARTESIAN_POINT ( 'NONE',  ( 4.206772801990143584, 8.129928378955675328, 0.7998128361456271485 ) ) ;
#79123 = CARTESIAN_POINT ( 'NONE',  ( -6.398558430645608475, 9.552403038140164782, -1.199719254218440723 ) ) ;
#79124 = VERTEX_POINT ( 'NONE', #208028 ) ;
#79125 = CARTESIAN_POINT ( 'NONE',  ( 2.693266070609028784, 6.293894182352508970, 0.000000000000000000 ) ) ;
#79126 = ORIENTED_EDGE ( 'NONE', *, *, #26279, .T. ) ;
#79127 = CARTESIAN_POINT ( 'NONE',  ( 4.525389411911321602, 8.501647757197021704, -0.7998128361456381397 ) ) ;
#79128 = CARTESIAN_POINT ( 'NONE',  ( -1.813763795902466613, 3.949999999999988187, -0.4000000000000339950 ) ) ;
#79129 = CARTESIAN_POINT ( 'NONE',  ( 0.7500000000000006661, 9.114583334016129967, 1.299038105676657340 ) ) ;
#79130 = CARTESIAN_POINT ( 'NONE',  ( 4.301718403444327876, 7.219878030919558043, 0.9872997725082887088 ) ) ;
#79131 = VERTEX_POINT ( 'NONE', #36192 ) ;
#79132 = EDGE_CURVE ( 'NONE', #142570, #105749, #78213, .T. ) ;
#79133 = CARTESIAN_POINT ( 'NONE',  ( 3.508111033888267283, 1.861241883637313688, 0.002260837353922766878 ) ) ;
#79134 = EDGE_CURVE ( 'NONE', #48021, #23152, #69745, .T. ) ;
#79135 = CARTESIAN_POINT ( 'NONE',  ( 1.352997864604365885, 0.1391545085356447886, -1.910588907247000368 ) ) ;
#79136 = CARTESIAN_POINT ( 'NONE',  ( 0.3404811318320751234, 0.3065618842239411501, 1.799498403862239915 ) ) ;
#79137 = CARTESIAN_POINT ( 'NONE',  ( 1.378881877344245277, 3.612814789602863730, 0.5904953584335879135 ) ) ;
#79138 = CARTESIAN_POINT ( 'NONE',  ( -0.7497020852614554309, -3.031334926134804153, 3.474999999999997424 ) ) ;
#79139 = CARTESIAN_POINT ( 'NONE',  ( 1.224999999999979661, 1.437500000682781387, -2.602085213965210642E-14 ) ) ;
#79140 = FACE_OUTER_BOUND ( 'NONE', #139697, .T. ) ;
#79141 = CARTESIAN_POINT ( 'NONE',  ( 8.934460041725669655, 9.525884258209195821, 1.040834085586084257E-14 ) ) ;
#79142 = CARTESIAN_POINT ( 'NONE',  ( 5.664895447484411761, 1.493751497301420761, -1.283663174101207005 ) ) ;
#79143 = CARTESIAN_POINT ( 'NONE',  ( -5.413783410558481002, 5.210502155273325720, -0.7998128361456221525 ) ) ;
#79144 = CARTESIAN_POINT ( 'NONE',  ( -9.581975256308806976, -7.217880409008731846, -3.245988297567687842E-13 ) ) ;
#79145 = CARTESIAN_POINT ( 'NONE',  ( 0.5860218096905758234, -2.075098906900944673, -0.2538066186672620628 ) ) ;
#79146 = CARTESIAN_POINT ( 'NONE',  ( -15.75000000000000000, 10.89999999999998259, 3.599999999999999201 ) ) ;
#79147 = CARTESIAN_POINT ( 'NONE',  ( 5.913098435216375570, 1.699041482274340265, 0.9079036414736068039 ) ) ;
#79148 = CARTESIAN_POINT ( 'NONE',  ( -7.718669524881690336, 7.899535955317097624, 0.7998128361456462443 ) ) ;
#79149 = CARTESIAN_POINT ( 'NONE',  ( 1.026062881544724137, 1.091098483296793820, -1.463488004260153907 ) ) ;
#79150 = CARTESIAN_POINT ( 'NONE',  ( 2.666872310945223923, -1.521158656661812714, 1.599105504226288499 ) ) ;
#79151 = CARTESIAN_POINT ( 'NONE',  ( -6.316846275044603942, 6.877910198612338100, 0.7063612664817873199 ) ) ;
#79152 = CARTESIAN_POINT ( 'NONE',  ( 0.2813230411330031044, 0.1852680230450229892, -1.903361379684164412 ) ) ;
#79153 =( BOUNDED_CURVE ( )  B_SPLINE_CURVE ( 3, ( #92891, #10532, #76605, #98213 ),
 .UNSPECIFIED., .F., .T. ) 
 B_SPLINE_CURVE_WITH_KNOTS ( ( 4, 4 ),
 ( 0.000000000000000000, 0.4999999999999957812 ),
 .UNSPECIFIED. ) 
 CURVE ( )  GEOMETRIC_REPRESENTATION_ITEM ( )  RATIONAL_B_SPLINE_CURVE ( ( 1.000000000000000222, 0.3333333333333390325, 0.3333333333333334259, 0.9999999999999945599 ) ) 
 REPRESENTATION_ITEM ( '' )  );
#79154 = EDGE_LOOP ( 'NONE', ( #209645, #149612, #67883, #10560 ) ) ;
#79155 = ORIENTED_EDGE ( 'NONE', *, *, #138823, .T. ) ;
#79156 = CARTESIAN_POINT ( 'NONE',  ( 0.5550503504515170716, 1.639475800691666985, -1.091118944626153331 ) ) ;
#79157 = CARTESIAN_POINT ( 'NONE',  ( 1.839301188190944902, 0.7414227542083090539, -1.795152619562689233 ) ) ;
#79158 = ORIENTED_EDGE ( 'NONE', *, *, #87756, .F. ) ;
#79159 = CARTESIAN_POINT ( 'NONE',  ( 0.4739822347885510601, 1.752760637641921360, 0.9961516927870717186 ) ) ;
#79161 = CARTESIAN_POINT ( 'NONE',  ( 5.014427361338555933, 0.7098351839037967403, 1.720451000603514524 ) ) ;
#79160 = CARTESIAN_POINT ( 'NONE',  ( -4.457598643843001973, 8.422558527783969851, 0.000000000000000000 ) ) ;
#79162 = CARTESIAN_POINT ( 'NONE',  ( 5.845500506147374153, 6.848780674373954547, 1.199719254218453823 ) ) ;
#79163 = FILL_AREA_STYLE ('',( #33608 ) ) ;
#79164 = CARTESIAN_POINT ( 'NONE',  ( 6.509000000000034092, 7.052765612591089806, 2.598154238703707541 ) ) ;
#79165 = CARTESIAN_POINT ( 'NONE',  ( -5.576481253922474401, 5.400316305864651056, -0.7998128361456221525 ) ) ;
#79166 = CARTESIAN_POINT ( 'NONE',  ( -6.505933609711270549, 8.683618192786854095, -1.599625672291271394 ) ) ;
#79167 = CARTESIAN_POINT ( 'NONE',  ( 1.435386855117400717, -1.590506285900999295, -1.507976327226906443 ) ) ;
#79168 = CARTESIAN_POINT ( 'NONE',  ( 3.551873057100283226, 6.127307085716883428, 1.082531754730558626 ) ) ;
#79169 = VECTOR ( 'NONE', #83592, 1000.000000000000000 ) ;
#79170 = CARTESIAN_POINT ( 'NONE',  ( 8.011942431032855083, 8.311964022485323511, 0.7998128361456291469 ) ) ;
#79171 = DIRECTION ( 'NONE',  ( 0.000000000000000000, 8.546850786086437571E-32, 1.000000000000000000 ) ) ;
#79172 = CARTESIAN_POINT ( 'NONE',  ( 1.840199252755945425, 1.805614550920462635, 0.2691313018618191055 ) ) ;
#79173 = CARTESIAN_POINT ( 'NONE',  ( -4.081167932913447594, 4.720116328942494555, -1.199719254218452047 ) ) ;
#79174 = CARTESIAN_POINT ( 'NONE',  ( -4.277761160311629673, 4.949475094240346706, 1.199719254218462483 ) ) ;
#79175 = CARTESIAN_POINT ( 'NONE',  ( -6.161504026110072196, 7.065710439381887475, -1.087211863304170523 ) ) ;
#79176 = B_SPLINE_CURVE_WITH_KNOTS ( 'NONE', 3,
 ( #46189, #96013, #63486, #129641, #195627, #32049, #97077, #113376, #82914, #99187 ),
 .UNSPECIFIED., .F., .F.,
 ( 4, 3, 3, 4 ),
 ( 1.563658610346436624E-18, 4.502046072369090049E-05, 9.004093402560554187E-05, 0.0001800865003196811215 ),
 .UNSPECIFIED. ) ;
#79177 = CARTESIAN_POINT ( 'NONE',  ( 6.609000000000015085, -6.653734696158637751E-05, 2.100160721423645960 ) ) ;
#79178 = CARTESIAN_POINT ( 'NONE',  ( 8.378048858240820351, 11.86180853700128601, -1.199719254218446718 ) ) ;
#79179 = CARTESIAN_POINT ( 'NONE',  ( 1.330555237386946255, 1.856516968354186892, 0.5143259067744552215 ) ) ;
#79180 = CARTESIAN_POINT ( 'NONE',  ( 6.104347744599991188, 1.959368324604572775, 0.09974838594294095639 ) ) ;
#79181 = CIRCLE ( 'NONE', #155260, 0.9475805310473219834 ) ;
#79182 = CARTESIAN_POINT ( 'NONE',  ( -8.202846631467911820, 9.528741477256060577, 1.199719254218462483 ) ) ;
#79183 = CARTESIAN_POINT ( 'NONE',  ( 4.476163270806094552, 8.373940915915776273, 0.7998128361456462443 ) ) ;
#79184 = CARTESIAN_POINT ( 'NONE',  ( 5.478137895480934105, -2.137967713159651506, -0.4810252310911074525 ) ) ;
#79185 = CARTESIAN_POINT ( 'NONE',  ( 4.172158584703322681, 5.890604320285754980, -1.599625672291256517 ) ) ;
#79186 = CARTESIAN_POINT ( 'NONE',  ( 4.399325512199628641, -1.803763729973751451, 1.015883459259236954 ) ) ;
#79189 = B_SPLINE_CURVE_WITH_KNOTS ( 'NONE', 3,
 ( #66640, #132785, #1649, #77867, #131735, #115497, #51508, #48334 ),
 .UNSPECIFIED., .F., .F.,
 ( 4, 2, 2, 4 ),
 ( 0.000000000000000000, 0.001499836411158092650, 0.002999672822316185299, 0.005999345644632373201 ),
 .UNSPECIFIED. ) ;
#79188 = CARTESIAN_POINT ( 'NONE',  ( -0.6823417656250003738, 0.7802083336747520637, -1.181850606188749264 ) ) ;
#79187 = CARTESIAN_POINT ( 'NONE',  ( -1.420000000000021911, 6.280000000000042881, 2.873333333333347728 ) ) ;
#79190 = VERTEX_POINT ( 'NONE', #135851 ) ;
#79191 = CARTESIAN_POINT ( 'NONE',  ( 4.254688019566841284, 2.229798712500128843, -0.5580973643144919727 ) ) ;
#79193 = EDGE_LOOP ( 'NONE', ( #161979, #196088, #49373, #147330 ) ) ;
#79192 = CARTESIAN_POINT ( 'NONE',  ( 8.270110514656037637, 8.750809809961280550, 0.7216878364870458196 ) ) ;
#79195 = CARTESIAN_POINT ( 'NONE',  ( 0.000000000000000000, -0.5468749995220422155, -3.793834371823813001 ) ) ;
#79194 = CARTESIAN_POINT ( 'NONE',  ( 6.265276383290871109, 7.442482214328385304, -1.082531754730548412 ) ) ;
#79196 = CARTESIAN_POINT ( 'NONE',  ( -7.778383330260381534, -5.907420853759297152, -7.778383330260338901 ) ) ;
#79197 = CARTESIAN_POINT ( 'NONE',  ( -9.801034077160730718, 4.485124939227990382, -6.925749731595153946 ) ) ;
#79198 = CARTESIAN_POINT ( 'NONE',  ( 4.189351911999553479, -0.7420460110593477543, 1.794775118790333135 ) ) ;
#79199 = EDGE_LOOP ( 'NONE', ( #31296, #85186, #68570, #65761 ) ) ;
#79200 = DIRECTION ( 'NONE',  ( 1.000000000000000000, -7.387867266669436732E-31, 0.000000000000000000 ) ) ;
#79201 = EDGE_CURVE ( 'NONE', #58680, #28791, #28562, .T. ) ;
#79202 = ORIENTED_EDGE ( 'NONE', *, *, #163561, .F. ) ;
#79203 = CARTESIAN_POINT ( 'NONE',  ( 5.467032840998240495, -1.503656711810175350, 1.181500457595338505 ) ) ;
#79204 = CARTESIAN_POINT ( 'NONE',  ( 6.616207624681263333, -0.8185094323158810248, -1.518158226148608625 ) ) ;
#79205 = CARTESIAN_POINT ( 'NONE',  ( 4.979703994296570180, -0.7212954316567052881, 1.883311551353183511 ) ) ;
#79206 = CARTESIAN_POINT ( 'NONE',  ( 0.4019237886466816012, 11.17633545031536713, -1.499999999999998668 ) ) ;
#79207 = CARTESIAN_POINT ( 'NONE',  ( 2.086817400036289794, -2.164668306305051804, -0.4287355390964405211 ) ) ;
#79208 = CARTESIAN_POINT ( 'NONE',  ( -3.851925040058333582, 7.508013290127760087, -0.7216878364870458196 ) ) ;
#79210 = CARTESIAN_POINT ( 'NONE',  ( 0.1448901830083254016, -1.363511527656173339, -1.128195317737596293 ) ) ;
#79209 = CARTESIAN_POINT ( 'NONE',  ( 1.675843188381221038, -1.117204103763050016, 1.766894365349908069 ) ) ;
#79211 = CARTESIAN_POINT ( 'NONE',  ( 5.942029771888944545, -1.730864577151491890, -1.034168155301495862 ) ) ;
#79213 = CARTESIAN_POINT ( 'NONE',  ( 3.591970686985697547, -2.289577047158963374, -0.1132367156824985732 ) ) ;
#79212 = CARTESIAN_POINT ( 'NONE',  ( 4.712340909201580885, 7.655425606447271214, -1.199719254218452047 ) ) ;
#79214 = CARTESIAN_POINT ( 'NONE',  ( 1.288542162703592231, 1.315766340102142662, 1.139191825253932366 ) ) ;
#79215 = CARTESIAN_POINT ( 'NONE',  ( -2.651925681381809952, -0.4070128260628267935, -0.1420391113308281661 ) ) ;
#79216 = CARTESIAN_POINT ( 'NONE',  ( 0.8074296549154248437, -1.491244094015523602, 0.8842416791710568935 ) ) ;
#79217 = CARTESIAN_POINT ( 'NONE',  ( -1.360316468750030428, 1.171875000341417117, -4.336808689942017736E-14 ) ) ;
#79218 = CARTESIAN_POINT ( 'NONE',  ( -0.4170821662629227156, 3.033599471985643170, 0.4170821662629036752 ) ) ;
#79219 = EDGE_CURVE ( 'NONE', #35502, #179060, #204152, .T. ) ;
#79220 = CARTESIAN_POINT ( 'NONE',  ( 1.873705115703153679, -0.2670016379083521296, 2.154652869704001272 ) ) ;
#79221 = CARTESIAN_POINT ( 'NONE',  ( 2.835173002801576914, -1.651343842416473917, -1.157098616274463865 ) ) ;
#79222 = CARTESIAN_POINT ( 'NONE',  ( 3.906250000000001776, 1.895863743163997084, -0.7852924748301890467 ) ) ;
#79223 = AXIS2_PLACEMENT_3D ( 'NONE', #12576, #144775, #80800 ) ;
#79224 = CARTESIAN_POINT ( 'NONE',  ( -0.7500000000000006661, 1.139583334016154526, -1.299038105676652011 ) ) ;
#79225 = CARTESIAN_POINT ( 'NONE',  ( 6.147092719882727430, -1.626042154682215468, 1.032876571686857536 ) ) ;
#79226 = CARTESIAN_POINT ( 'NONE',  ( -1.364683531250000748, 12.60937500034139980, 0.000000000000000000 ) ) ;
#79227 = CARTESIAN_POINT ( 'NONE',  ( 3.867602925442710671, -1.848332671738551980, -1.231929692598219050 ) ) ;
#79228 = ORIENTED_EDGE ( 'NONE', *, *, #167641, .F. ) ;
#79229 = CARTESIAN_POINT ( 'NONE',  ( 6.726126798029175902, -7.621055083280628750, 6.709229400514947095 ) ) ;
#79230 = CARTESIAN_POINT ( 'NONE',  ( 1.499999999999985123, -0.7041666666666481778, -0.8660254037844323793 ) ) ;
#79231 = CARTESIAN_POINT ( 'NONE',  ( 9.426996880203592610, 9.892584536526015881, -0.7998128361456281477 ) ) ;
#79232 = CARTESIAN_POINT ( 'NONE',  ( 6.007671464186823407, 9.062681570643055906, 1.082531754730549967 ) ) ;
#79233 = CARTESIAN_POINT ( 'NONE',  ( -10.62873463776380234, 9.799999999999982947, 3.199999999999997957 ) ) ;
#79234 = CARTESIAN_POINT ( 'NONE',  ( 5.460439331044164568, -1.576930981450849867, -0.7368137880037448628 ) ) ;
#79235 = CARTESIAN_POINT ( 'NONE',  ( 3.736726379466179804, -1.890069333072645241, -0.5255722985574098338 ) ) ;
#79237 = CARTESIAN_POINT ( 'NONE',  ( -5.097502569058210753, 7.930541516334467467, -1.082531754730549967 ) ) ;
#79236 = CARTESIAN_POINT ( 'NONE',  ( 3.009020027229115879, 5.597941567487558778, -1.199719254218446718 ) ) ;
#79238 = CARTESIAN_POINT ( 'NONE',  ( -1.443845971921561722, 4.128618707767023999, -0.4218533236949579268 ) ) ;
#79239 = CARTESIAN_POINT ( 'NONE',  ( 4.147957446309138874, 0.7671257181886274035, -2.128492778801443830 ) ) ;
#79240 = CIRCLE ( 'NONE', #13524, 9.523431457505068920 ) ;
#79241 = CARTESIAN_POINT ( 'NONE',  ( 1.697793086734213697, -1.492557772401803318, -1.423914585240863673 ) ) ;
#79242 = CARTESIAN_POINT ( 'NONE',  ( -7.379715684540041565, 7.504089808251839244, 1.040834085586084257E-14 ) ) ;
#79243 = CARTESIAN_POINT ( 'NONE',  ( 2.676973543053912330, -2.164909235287615807, -0.6573374913001366338 ) ) ;
#79244 = VERTEX_POINT ( 'NONE', #52459 ) ;
#79245 = CARTESIAN_POINT ( 'NONE',  ( -1.499999999999997780, 1.931250000682817269, 0.000000000000000000 ) ) ;
#79246 = CARTESIAN_POINT ( 'NONE',  ( 3.374138713240721454, -1.116850685118627728, 1.500355210514233262 ) ) ;
#79247 = CARTESIAN_POINT ( 'NONE',  ( 2.179902339641195397, 1.341075392948913425, 1.099452185880249067 ) ) ;
#79248 = EDGE_CURVE ( 'NONE', #187417, #164674, #163378, .T. ) ;
#79249 = CARTESIAN_POINT ( 'NONE',  ( -0.1230140872038130023, -0.1644519934839226150, -2.256176000670232717 ) ) ;
#79250 = CARTESIAN_POINT ( 'NONE',  ( 6.475599238194152285, 2.210894796874377288, -0.6610463658997690617 ) ) ;
#79251 = CARTESIAN_POINT ( 'NONE',  ( 3.432649856329002880, 2.108609624295390006, 0.4754391814798044069 ) ) ;
#79252 = CARTESIAN_POINT ( 'NONE',  ( 4.839755972451986743, 1.936857930295164065, 0.1413805851513943446 ) ) ;
#79253 = CARTESIAN_POINT ( 'NONE',  ( -3.267151830768959098, 4.834763107362302748, -1.443375672974058777 ) ) ;
#79254 = CARTESIAN_POINT ( 'NONE',  ( 6.327412175546781370, -1.761338861328298089, 0.6302073946208713862 ) ) ;
#79255 =( LENGTH_UNIT ( ) NAMED_UNIT ( * ) SI_UNIT ( .MILLI., .METRE. ) );
#79256 = EDGE_CURVE ( 'NONE', #72298, #200044, #59790, .T. ) ;
#79257 = CARTESIAN_POINT ( 'NONE',  ( 4.553433815925461481, 6.963525196941225737, 1.181321538200299281 ) ) ;
#79258 = DIRECTION ( 'NONE',  ( 0.000000000000000000, 0.000000000000000000, 1.000000000000000000 ) ) ;
#79259 = CARTESIAN_POINT ( 'NONE',  ( 4.923019175537949543, 4.916146257648610352, 0.000000000000000000 ) ) ;
#79260 = CARTESIAN_POINT ( 'NONE',  ( 1.360316468749949825, 1.994791667008131597, 0.7853790794158700406 ) ) ;
#79261 = CARTESIAN_POINT ( 'NONE',  ( 5.520157785563180930, -1.821743191724470634, 0.8647220171385738841 ) ) ;
#79262 = CARTESIAN_POINT ( 'NONE',  ( -9.398826802771548472, 11.98838390803207865, -1.599625672291263179 ) ) ;
#79263 = CARTESIAN_POINT ( 'NONE',  ( 7.365103760721646076, 9.615707025640515937, 1.599625672291281386 ) ) ;
#79264 = CARTESIAN_POINT ( 'NONE',  ( 3.390420931869152721, 6.113185632892752075, -1.199719254218452047 ) ) ;
#79265 = CARTESIAN_POINT ( 'NONE',  ( 3.299243935302543118, 1.439784963707075649, 1.122460502641378755 ) ) ;
#79266 = CARTESIAN_POINT ( 'NONE',  ( 11.92045683181315141, 9.947240721205149683, -1.382340670101858571 ) ) ;
#79267 = EDGE_LOOP ( 'NONE', ( #53420, #131727, #188893, #36911 ) ) ;
#79268 = CARTESIAN_POINT ( 'NONE',  ( -4.706088717274938382, 6.583799151611112954, 1.443375672974058777 ) ) ;
#79269 = CARTESIAN_POINT ( 'NONE',  ( -3.285556943750000070, -3.346874999522041261, 0.000000000000000000 ) ) ;
#79270 = CARTESIAN_POINT ( 'NONE',  ( -7.995557903757128493, 10.35123685918189729, 1.599625672291295375 ) ) ;
#79271 = CARTESIAN_POINT ( 'NONE',  ( 1.318624316974380317, -0.7310098426952565953, -1.883032709213072975 ) ) ;
#79272 = CARTESIAN_POINT ( 'NONE',  ( 1.190261156817543631, 1.266008754425467897, 1.700926646755014593 ) ) ;
#79273 = CARTESIAN_POINT ( 'NONE',  ( -4.125423880308188629, 8.035021303660014880, -0.7998128361456481317 ) ) ;
#79274 = CARTESIAN_POINT ( 'NONE',  ( 1.463465096324652714, -0.4588509492367858766, 1.803342318195770178 ) ) ;
#79275 = CARTESIAN_POINT ( 'NONE',  ( 4.029797971759831121, 5.724516938518342535, -1.599625672291255185 ) ) ;
#79276 = AXIS2_PLACEMENT_3D ( 'NONE', #156315, #73987, #123896 ) ;
#79277 = CARTESIAN_POINT ( 'NONE',  ( 6.702032673877901914, -2.060500267551836018, 0.04777910199381221051 ) ) ;
#79278 = CARTESIAN_POINT ( 'NONE',  ( 6.539686446881147752, -1.556848207870220602, 1.281141925495055123 ) ) ;
#79279 = EDGE_LOOP ( 'NONE', ( #187538, #64018, #110177, #186572 ) ) ;
#79280 = CARTESIAN_POINT ( 'NONE',  ( -8.272446282632566650, 12.80293776304669962, 0.7998128361456481317 ) ) ;
#79281 = CARTESIAN_POINT ( 'NONE',  ( 3.721172816245840842, -0.1328194893376876962, 1.820914920514608459 ) ) ;
#79283 = CARTESIAN_POINT ( 'NONE',  ( -6.007394967034264788, 6.077829431587280062, -0.6506939886842719734 ) ) ;
#79282 = CARTESIAN_POINT ( 'NONE',  ( -3.494969737272722643, 7.299491470118629088, -0.7998128361456481317 ) ) ;
#79284 = CARTESIAN_POINT ( 'NONE',  ( 6.454463653088309272, 6.866155873091829953, 0.6733577401037347254 ) ) ;
#79285 = CARTESIAN_POINT ( 'NONE',  ( 5.888046020683160187, -0.05228737891407529703, 2.015604419750731680 ) ) ;
#79286 = CARTESIAN_POINT ( 'NONE',  ( 6.052668933152094866, -1.581501214056714177, -0.9424504099920794076 ) ) ;
#79287 = CARTESIAN_POINT ( 'NONE',  ( 0.2333690889706682703, 0.003390530909083006028, -2.053566628440507635 ) ) ;
#79288 = CARTESIAN_POINT ( 'NONE',  ( 3.686388391042205726, -1.138424198849327107, 2.007274438705310970 ) ) ;
#79289 = CARTESIAN_POINT ( 'NONE',  ( 4.681308178468477799, 8.683552984847038303, 0.000000000000000000 ) ) ;
#79290 = CARTESIAN_POINT ( 'NONE',  ( 5.554052124568397808, 2.159397089200214559, -0.09991998142631913771 ) ) ;
#79291 = CARTESIAN_POINT ( 'NONE',  ( 5.472687561410540802, 9.536552588287639409, 0.7998128361456462443 ) ) ;
#79292 = CARTESIAN_POINT ( 'NONE',  ( 1.329522225144257774, 0.9558622346672830394, -1.690450677827403103 ) ) ;
#79293 = ORIENTED_EDGE ( 'NONE', *, *, #104706, .F. ) ;
#79294 = AXIS2_PLACEMENT_3D ( 'NONE', #26063, #161423, #208013 ) ;
#79295 = CARTESIAN_POINT ( 'NONE',  ( 4.148081960540086932, -0.2207414774363871957, -2.287749835899715034 ) ) ;
#79296 = DIRECTION ( 'NONE',  ( 0.08676574618400521854, 0.9962285034897236935, 0.0006885664517734813028 ) ) ;
#79297 = CARTESIAN_POINT ( 'NONE',  ( -7.075376061485238566, 9.347967719856493218, 1.599625672291269396 ) ) ;
#79298 = EDGE_CURVE ( 'NONE', #16779, #178259, #27060, .T. ) ;
#79299 = CARTESIAN_POINT ( 'NONE',  ( 4.785944050937030347, -0.8815013282119155136, 1.649949660215948688 ) ) ;
#79300 = VERTEX_POINT ( 'NONE', #75910 ) ;
#79303 = CARTESIAN_POINT ( 'NONE',  ( -4.502189528189771472, 7.410248995266807803, -1.199719254218453823 ) ) ;
#79302 = CARTESIAN_POINT ( 'NONE',  ( -0.7500000000000249800, -0.02708333265051543481, 1.299038105676659116 ) ) ;
#79301 = CARTESIAN_POINT ( 'NONE',  ( 1.898553772666348394, -1.876154101037771582, -0.3696338911259658411 ) ) ;
#79304 = CARTESIAN_POINT ( 'NONE',  ( 4.477303810882872881, 0.001702072213635372200, -2.207063162522747479 ) ) ;
#79305 = CARTESIAN_POINT ( 'NONE',  ( 6.883263157960369583, 7.629137130509070275, 2.546189081643289942 ) ) ;
#79306 = CARTESIAN_POINT ( 'NONE',  ( 4.241003122976366058, 3.842258486427521103, -0.7998128361456211532 ) ) ;
#79307 = CARTESIAN_POINT ( 'NONE',  ( 5.356880090730850696, 9.263794182579101033, 0.7216878364870317197 ) ) ;
#79308 = CARTESIAN_POINT ( 'NONE',  ( -4.295235737431041478, 3.905529869957963029, -0.7998128361456221525 ) ) ;
#79309 = CARTESIAN_POINT ( 'NONE',  ( -7.078765599666485997, 7.431183752465250869, 0.000000000000000000 ) ) ;
#79310 = CARTESIAN_POINT ( 'NONE',  ( 2.055877211876644406, 1.966332055899377762, -0.1412752051469425008 ) ) ;
#79311 = CARTESIAN_POINT ( 'NONE',  ( 0.8335961714901140018, 0.1734020439737720132, 2.301109984577158762 ) ) ;
#79312 = CARTESIAN_POINT ( 'NONE',  ( 2.154674626568295892, -0.5202524484802829585, -1.891573884155263396 ) ) ;
#79313 = CARTESIAN_POINT ( 'NONE',  ( -0.5000000000000247580, 3.172938907704287104, 0.3999999999999698241 ) ) ;
#79314 = CARTESIAN_POINT ( 'NONE',  ( 5.629752743445687990, 1.989327071453067752, -0.5446528645957140480 ) ) ;
#79315 = CARTESIAN_POINT ( 'NONE',  ( 3.524756749872944628, 7.056040608253000279, -0.7216878364870267237 ) ) ;
#79316 = CARTESIAN_POINT ( 'NONE',  ( 5.285699784481295183, 7.260012063351913625, 1.599625672291268286 ) ) ;
#79317 = VERTEX_POINT ( 'NONE', #84952 ) ;
#79318 = CARTESIAN_POINT ( 'NONE',  ( -1.001543065824772872E-14, 5.634375000341415252, 1.575800808251672791 ) ) ;
#79319 = CARTESIAN_POINT ( 'NONE',  ( -0.9311234436981496998, -1.328130369558482293, 3.475000000000000977 ) ) ;
#79320 = CARTESIAN_POINT ( 'NONE',  ( 4.338245966248566177, 4.163634503485842409, 1.214306433183764966E-14 ) ) ;
#79321 = CARTESIAN_POINT ( 'NONE',  ( 0.6026744816367580748, 2.165159614417012879, 0.1613400170472640283 ) ) ;
#79322 = CARTESIAN_POINT ( 'NONE',  ( 6.773376349083131132, -7.473374494058229622, 6.661184041420955992 ) ) ;
#79323 = CARTESIAN_POINT ( 'NONE',  ( -7.317172100870442009, -6.705807707650950356, 7.317172100870468654 ) ) ;
#79324 = CARTESIAN_POINT ( 'NONE',  ( 2.178771278573924608, -0.08713135167291723160, -1.868625915979430729 ) ) ;
#79325 = EDGE_CURVE ( 'NONE', #122534, #101488, #170479, .T. ) ;
#79326 = CONICAL_SURFACE ( 'NONE', #114039, 11.53746066217573762, 0.1181278931043537039 ) ;
#79327 = CARTESIAN_POINT ( 'NONE',  ( 6.573507624224045109, 2.070638407997299257, -0.6205318887850322929 ) ) ;
#79328 = CARTESIAN_POINT ( 'NONE',  ( 6.727182134110205602, 7.053355583909074689, 2.409100679957976165 ) ) ;
#79329 = CARTESIAN_POINT ( 'NONE',  ( -1.402160292154681736E-14, -0.8031249996585825279, -1.575800808251665908 ) ) ;
#79330 = CARTESIAN_POINT ( 'NONE',  ( 2.420441844550869526, -0.7335502799032426191, -1.766186906296034698 ) ) ;
#79331 = CARTESIAN_POINT ( 'NONE',  ( 4.592510532270950740, -0.3890688374885014067, -1.726373200486588377 ) ) ;
#79332 = CARTESIAN_POINT ( 'NONE',  ( 1.770022778749248182, 1.907080152163560971, -0.1419829583147319274 ) ) ;
#79333 = CARTESIAN_POINT ( 'NONE',  ( -6.067437437315529536, 7.037430750744921859, 1.199719254218450271 ) ) ;
#79335 = CARTESIAN_POINT ( 'NONE',  ( 5.325768798837505535, 0.7719732895165082320, -1.753353820041517741 ) ) ;
#79334 = SURFACE_STYLE_FILL_AREA ( #76133 ) ;
#79336 = CIRCLE ( 'NONE', #189562, 11.67999999982603399 ) ;
#79337 = CARTESIAN_POINT ( 'NONE',  ( 6.654754201047359707, -0.5240520113350942699, -1.898494369619908140 ) ) ;
#79338 = CARTESIAN_POINT ( 'NONE',  ( -1.500000000000011324, 5.170833333333356485, 0.8660254037844403729 ) ) ;
#79339 = CARTESIAN_POINT ( 'NONE',  ( 2.443736651115399283, -1.977012053918187906, 0.7674769708189137507 ) ) ;
#79340 = CARTESIAN_POINT ( 'NONE',  ( 3.809456170543987774, 8.470288933811271903, -2.500000000000000444 ) ) ;
#79341 = CARTESIAN_POINT ( 'NONE',  ( 4.821099876132087125, -0.09137817997613774390, 1.868553921495450965 ) ) ;
#79343 = ORIENTED_EDGE ( 'NONE', *, *, #158993, .F. ) ;
#79342 = CARTESIAN_POINT ( 'NONE',  ( 1.506192966688112422, -0.6554880476431452774, -1.704135612709246184 ) ) ;
#79345 = CARTESIAN_POINT ( 'NONE',  ( 4.978641999450219124, 7.938775605734648799, 1.052364473307040305 ) ) ;
#79344 = CARTESIAN_POINT ( 'NONE',  ( 4.319099500008596770, 2.017107695584336557, 0.8957252843501888329 ) ) ;
#79346 = PRESENTATION_LAYER_ASSIGNMENT (  '', '', ( #186480 ) ) ;
#79347 = CARTESIAN_POINT ( 'NONE',  ( 1.364683531249990311, 5.676041667008088432, 0.7879004041258500513 ) ) ;
#79348 = CARTESIAN_POINT ( 'NONE',  ( 2.154800422482431532, -0.5477745769525663722, -1.988566864369076592 ) ) ;
#79349 = CARTESIAN_POINT ( 'NONE',  ( 7.284808609244363353, 7.393364887073558656, 0.7998128361456341429 ) ) ;
#79350 = CARTESIAN_POINT ( 'NONE',  ( -9.013473194986783454, 9.410140237106395134, -0.7998128361456291469 ) ) ;
#79351 = CARTESIAN_POINT ( 'NONE',  ( 0.000000000000000000, 0.5000000000000004441, 0.000000000000000000 ) ) ;
#79352 = CARTESIAN_POINT ( 'NONE',  ( 1.286956418854593220, 3.652345658002546624, 0.4592741676706378895 ) ) ;
#79353 = CARTESIAN_POINT ( 'NONE',  ( 0.9999999999999833467, 9.200000000000018829, -0.3999999999999961919 ) ) ;
#79354 = CARTESIAN_POINT ( 'NONE',  ( 5.345657705538078730, 9.458627433094950021, 0.7998128361456331437 ) ) ;
#79355 = ORIENTED_EDGE ( 'NONE', *, *, #9768, .T. ) ;
#79356 = CARTESIAN_POINT ( 'NONE',  ( 4.088381982606685838, 1.110138344689771239, -1.747393465062855533 ) ) ;
#79357 = CARTESIAN_POINT ( 'NONE',  ( -1.500000000000011324, 5.670833333333358262, 0.8660254037844403729 ) ) ;
#79358 = CARTESIAN_POINT ( 'NONE',  ( 2.952577552874091626, 0.7252333659365679530, 2.036452211405047397 ) ) ;
#79359 = CARTESIAN_POINT ( 'NONE',  ( -5.295344997983027824, 7.654313019038245791, -1.225062028442117423 ) ) ;
#79360 = CARTESIAN_POINT ( 'NONE',  ( 2.807290699014941548, 1.731141667658737449, -1.040073625836896554 ) ) ;
#79361 = CARTESIAN_POINT ( 'NONE',  ( 6.620655732516668834, 7.629137130509086262, 2.673739711112704143 ) ) ;
#79362 = ORIENTED_EDGE ( 'NONE', *, *, #30637, .F. ) ;
#79364 = CARTESIAN_POINT ( 'NONE',  ( 7.944714827928056167, 8.371181508778631652, 0.7216878364870458196 ) ) ;
#79363 = CARTESIAN_POINT ( 'NONE',  ( -3.474999999999998312, -2.070833333333331971, 2.006292185433951047 ) ) ;
#79365 = CARTESIAN_POINT ( 'NONE',  ( -4.624739795592948788, 5.528522862014106920, -1.082531754730549967 ) ) ;
#79366 = CARTESIAN_POINT ( 'NONE',  ( 1.446500318503377125, -1.422605717829699801, 1.429450658469958668 ) ) ;
#79367 = CARTESIAN_POINT ( 'NONE',  ( 6.181208317857348256, 1.509947553572440704, 1.588605474358975478 ) ) ;
#79368 = CARTESIAN_POINT ( 'NONE',  ( -1.201851678989727383E-14, 4.618750000682821266, -1.732050807568863648 ) ) ;
#79369 = CARTESIAN_POINT ( 'NONE',  ( 4.271672842113056312, 0.4137096367802223784, -1.866957553337177611 ) ) ;
#79370 = CARTESIAN_POINT ( 'NONE',  ( -2.930533758848195447, 6.570706485298192234, -0.7998128361456281477 ) ) ;
#79371 = CARTESIAN_POINT ( 'NONE',  ( 6.033015167956792268, 8.061603667414825480, -1.443375672974057666 ) ) ;
#79373 = CARTESIAN_POINT ( 'NONE',  ( 1.950796209937825321, -1.844718841590715863, -0.8146091914792084054 ) ) ;
#79372 = CARTESIAN_POINT ( 'NONE',  ( -9.124274191872636663, 11.66807252865000244, -1.443375672974058777 ) ) ;
#79374 = CARTESIAN_POINT ( 'NONE',  ( -8.012344526598182026E-15, 14.35937500034139802, -1.575800808251669460 ) ) ;
#79375 = CARTESIAN_POINT ( 'NONE',  ( -5.191846479390389568, 5.021852078902356631, 0.7998128361456281477 ) ) ;
#79376 = CARTESIAN_POINT ( 'NONE',  ( 5.438411972298594854, 1.699845694858553857, 0.2911611187441583426 ) ) ;
#79377 = CARTESIAN_POINT ( 'NONE',  ( -0.1394461523061351904, -0.009327122704730000241, -2.280146446826665230 ) ) ;
#79378 = CARTESIAN_POINT ( 'NONE',  ( 9.951321562750607086, 11.67259191370631477, -1.082531754730537088 ) ) ;
#79379 = DIRECTION ( 'NONE',  ( 0.000000000000000000, 0.000000000000000000, -1.000000000000000000 ) ) ;
#79380 = CARTESIAN_POINT ( 'NONE',  ( 3.680148631105580215, 6.380924938676771241, -1.199719254218446718 ) ) ;
#79381 = DIRECTION ( 'NONE',  ( 0.000000000000000000, 1.000000000000000000, 0.000000000000000000 ) ) ;
#79382 = CARTESIAN_POINT ( 'NONE',  ( 1.516557075436252733, 0.8353943144701718726, 1.894387172633307692 ) ) ;
#79383 = ORIENTED_EDGE ( 'NONE', *, *, #202081, .F. ) ;
#79384 = CARTESIAN_POINT ( 'NONE',  ( 4.670457322363490427, 0.6978976414240989357, 1.671844709466139722 ) ) ;
#79385 = CARTESIAN_POINT ( 'NONE',  ( 4.206772801990143584, 8.129928378955675328, 0.7998128361456271485 ) ) ;
#79386 = CARTESIAN_POINT ( 'NONE',  ( 1.347111479062088799E-15, -2.079999999999998295, -11.00000000000000178 ) ) ;
#79387 = CARTESIAN_POINT ( 'NONE',  ( 6.551413666264667590, -1.614568043246225271, 0.8214943993307096681 ) ) ;
#79388 = CARTESIAN_POINT ( 'NONE',  ( 5.519577934094852978, 7.532869904567736974, 1.443375672974064550 ) ) ;
#79389 = CARTESIAN_POINT ( 'NONE',  ( -1.298432343300637860E-14, 2.519999999999999130, -2.000000000000000000 ) ) ;
#79390 = CARTESIAN_POINT ( 'NONE',  ( 3.187623232016934871, -0.8878212517344568067, 2.003729935572157839 ) ) ;
#79391 = VERTEX_POINT ( 'NONE', #29297 ) ;
#79392 = ADVANCED_FACE ( 'NONE', ( #161442 ), #57443, .T. ) ;
#79394 = CARTESIAN_POINT ( 'NONE',  ( 9.264299036839600987, 9.702770385934682551, -0.7998128361456281477 ) ) ;
#79393 = CARTESIAN_POINT ( 'NONE',  ( 0.6253529088778920775, 0.1960189665039281104, -1.952063659030291998 ) ) ;
#79395 = CARTESIAN_POINT ( 'NONE',  ( 4.411684386003834391, -1.181747345438967312, -1.507543049613221386 ) ) ;
#79396 = CARTESIAN_POINT ( 'NONE',  ( 0.000000000000000000, 13.49999999999999822, 0.000000000000000000 ) ) ;
#79397 = DIRECTION ( 'NONE',  ( -0.000000000000000000, -1.000000000000000000, -0.000000000000000000 ) ) ;
#79398 = CARTESIAN_POINT ( 'NONE',  ( 1.364683531249988757, -0.3656249996585800299, 0.000000000000000000 ) ) ;
#79400 = VERTEX_POINT ( 'NONE', #61795 ) ;
#79399 = CARTESIAN_POINT ( 'NONE',  ( 4.202664430556241726, 7.846932902383524144, 0.7216878364870298324 ) ) ;
#79401 = CARTESIAN_POINT ( 'NONE',  ( -8.893785580884703279, 10.43879993486270585, 1.082531754730558626 ) ) ;
#79402 = CARTESIAN_POINT ( 'NONE',  ( 1.569428280142046495, 0.1587979871724466974, -2.155937297210829495 ) ) ;
#79403 = CARTESIAN_POINT ( 'NONE',  ( -4.122561227007127016, 6.967349310553715647, 1.199719254218452935 ) ) ;
#79404 = CARTESIAN_POINT ( 'NONE',  ( 3.054329744828568227, 6.785411478933790264, 0.000000000000000000 ) ) ;
#79405 = CARTESIAN_POINT ( 'NONE',  ( 1.922601709848625440, 1.702220721529534853, 0.6601445126475160574 ) ) ;
#79406 = CARTESIAN_POINT ( 'NONE',  ( -4.416205349749324327, 6.175325546172740765, 1.599625672291267398 ) ) ;
#79407 = CARTESIAN_POINT ( 'NONE',  ( 4.664971680594516279, -1.631047870213175432, -0.8201845326444437978 ) ) ;
#79408 = EDGE_CURVE ( 'NONE', #97632, #168104, #130873, .T. ) ;
#79409 = CARTESIAN_POINT ( 'NONE',  ( 12.04878676029568751, 8.355254920624089365, 5.374760359037731305 ) ) ;
#79410 = CARTESIAN_POINT ( 'NONE',  ( 2.953266587970606150, -1.684550232849800544, 0.9053361341156559439 ) ) ;
#79411 = ORIENTED_EDGE ( 'NONE', *, *, #31316, .F. ) ;
#79412 = CARTESIAN_POINT ( 'NONE',  ( 3.648844292986920479, -0.3817546106285915619, -1.932013994212372854 ) ) ;
#79413 = ORIENTED_EDGE ( 'NONE', *, *, #143526, .T. ) ;
#79414 = CARTESIAN_POINT ( 'NONE',  ( 5.970255158568685161, -1.845527328187264615, -0.6049325008806984982 ) ) ;
#79415 = ORIENTED_EDGE ( 'NONE', *, *, #149244, .F. ) ;
#79416 = CARTESIAN_POINT ( 'NONE',  ( -5.413448473606448985, 9.537716662508005427, 0.000000000000000000 ) ) ;
#79418 = CARTESIAN_POINT ( 'NONE',  ( 4.834296457332984076, -1.136628438424293508, -1.790084250976264002 ) ) ;
#79417 = CARTESIAN_POINT ( 'NONE',  ( 6.017840079619279692, 8.114175741012878973, -1.599625672291281386 ) ) ;
#79419 = DIRECTION ( 'NONE',  ( 0.000000000000000000, 0.000000000000000000, 1.000000000000000000 ) ) ;
#79420 = CARTESIAN_POINT ( 'NONE',  ( 3.158751774003202950, 0.4669426847015486493, 1.854258104404989060 ) ) ;
#79421 = CARTESIAN_POINT ( 'NONE',  ( 4.825890400613210396, 6.946991693042408045, -1.413043630229819048 ) ) ;
#79422 = CARTESIAN_POINT ( 'NONE',  ( 6.983263157960368339, 4.695310640067480001, 2.508805386165738227 ) ) ;
#79423 = ORIENTED_EDGE ( 'NONE', *, *, #144259, .F. ) ;
#79424 = CARTESIAN_POINT ( 'NONE',  ( 3.607351389687783794, 6.366271167014519783, 1.199719254218451159 ) ) ;
#79425 = CARTESIAN_POINT ( 'NONE',  ( 5.637363213272434059, -0.04718591601137950980, 2.012692011999743791 ) ) ;
#79426 = DIRECTION ( 'NONE',  ( 5.578564026256504688E-16, 1.000000000000000000, 9.066213480720158442E-32 ) ) ;
#79427 = CARTESIAN_POINT ( 'NONE',  ( 6.164658409365947556, -1.287482145768016339, 1.294691480910937775 ) ) ;
#79428 = CARTESIAN_POINT ( 'NONE',  ( 0.5376586404672692998, 1.932363751568724641, -0.7437053376125392079 ) ) ;
#79429 = CARTESIAN_POINT ( 'NONE',  ( -7.863365906246061243, 10.19701286208565705, -1.443375672974059665 ) ) ;
#79430 = CARTESIAN_POINT ( 'NONE',  ( -5.773448424614897156, 7.353550462951784716, 1.313087523158409153 ) ) ;
#79431 = CARTESIAN_POINT ( 'NONE',  ( 11.33772463945036790, 10.90000000000000036, -3.600000000000002309 ) ) ;
#79432 = LINE ( 'NONE', #209404, #111593 ) ;
#79433 = CARTESIAN_POINT ( 'NONE',  ( 5.829115978871627135, 8.888053511070525659, 1.199719254218462483 ) ) ;
#79434 = CARTESIAN_POINT ( 'NONE',  ( -5.271422797614988554, 5.044414773505913274, -0.7998128361456221525 ) ) ;
#79435 = CARTESIAN_POINT ( 'NONE',  ( 2.920892028740289081, 5.495125569250587816, 1.199719254218452047 ) ) ;
#79436 = CARTESIAN_POINT ( 'NONE',  ( 0.6823417656249969321, 10.83854166700806765, -1.181850606188757036 ) ) ;
#79437 = CARTESIAN_POINT ( 'NONE',  ( -5.220052836461385404, 6.048815383081766583, -1.199719254218446718 ) ) ;
#79439 = CARTESIAN_POINT ( 'NONE',  ( -4.516274566683622815, 5.401980094953223066, 1.082531754730549078 ) ) ;
#79438 = CARTESIAN_POINT ( 'NONE',  ( 7.987977580929889854, -5.530730635397379302, -7.987977580929920940 ) ) ;
#79440 = AXIS2_PLACEMENT_3D ( 'NONE', #93252, #146271, #159286 ) ;
#79441 = CARTESIAN_POINT ( 'NONE',  ( -4.985647801523292344, 6.839675073242382553, -1.599625672291256295 ) ) ;
#79442 = CARTESIAN_POINT ( 'NONE',  ( 1.586871713678970730, 1.994102569620255228, 0.5559867524188369936 ) ) ;
#79443 = CARTESIAN_POINT ( 'NONE',  ( 2.249754300142119856, 2.075745305004289332, -0.4162820868813913999 ) ) ;
#79444 = CARTESIAN_POINT ( 'NONE',  ( 8.751951852821344247, 10.16936423550178503, -1.199719254218446718 ) ) ;
#79445 = DIRECTION ( 'NONE',  ( 0.000000000000000000, 8.546850786086437571E-32, 1.000000000000000000 ) ) ;
#79446 = CARTESIAN_POINT ( 'NONE',  ( 0.9187298884396404297, -1.430263011927451311, 1.354180262349208075 ) ) ;
#79447 = CARTESIAN_POINT ( 'NONE',  ( 5.239055555121258756, 6.613325079961110298, 1.380154382352281495 ) ) ;
#79448 = CARTESIAN_POINT ( 'NONE',  ( 4.039966587192250103, 7.657118751792200584, 0.7216878364870298324 ) ) ;
#79450 = PLANE ( 'NONE',  #194749 ) ;
#79449 = CARTESIAN_POINT ( 'NONE',  ( 1.737499999999999378, -3.266666666666667496, -3.009438278150925683 ) ) ;
#79451 = B_SPLINE_CURVE_WITH_KNOTS ( 'NONE', 3,
 ( #104191, #21823, #2379, #87931, #68456, #200585, #52234, #118361, #57570, #41341, #143126, #205938, #91157, #6659, #125852, #157211 ),
 .UNSPECIFIED., .F., .F.,
 ( 4, 3, 3, 3, 3, 4 ),
 ( 0.000000000000000000, 6.763659418792604407E-06, 1.351747408346287881E-05, 2.025570936575418784E-05, 2.697948549281415037E-05, 3.136114954460948387E-05 ),
 .UNSPECIFIED. ) ;
#79452 = CARTESIAN_POINT ( 'NONE',  ( 2.924086828919622238, 1.272802903806929953, -1.906236438263966271 ) ) ;
#79453 = CARTESIAN_POINT ( 'NONE',  ( 0.6272434487209905818, -1.734552980249819631, 0.5698080454362154379 ) ) ;
#79454 = CARTESIAN_POINT ( 'NONE',  ( 3.814637755342592307, -0.6046605605216844870, -1.814329123173196834 ) ) ;
#79455 = CARTESIAN_POINT ( 'NONE',  ( 6.042093733545556233, 7.078139439671806699, -1.199719254218452047 ) ) ;
#79456 = CARTESIAN_POINT ( 'NONE',  ( 6.249945625775433555, 10.23542763013927726, -0.7216878364870267237 ) ) ;
#79457 = EDGE_CURVE ( 'NONE', #164408, #91407, #199406, .T. ) ;
#79458 = CARTESIAN_POINT ( 'NONE',  ( 1.301040509920841526, -0.2996390532185671529, -1.990687865782204469 ) ) ;
#79459 = CARTESIAN_POINT ( 'NONE',  ( 1.990992145637654698, 0.1870960246039363450, 1.952785824368876710 ) ) ;
#79460 = CARTESIAN_POINT ( 'NONE',  ( -9.646789991323334590, 11.21334206375407305, 1.199719254218462483 ) ) ;
#79461 = CARTESIAN_POINT ( 'NONE',  ( -7.901704598666176693, 8.113076874732334076, 0.7998128361456602331 ) ) ;
#79462 = CARTESIAN_POINT ( 'NONE',  ( -11.77588451118714730, 7.698608310071745287, 2.073293985440898268 ) ) ;
#79464 = CARTESIAN_POINT ( 'NONE',  ( 3.326767387183640956, 0.04228616847017605679, 1.769505212706389941 ) ) ;
#79463 = CARTESIAN_POINT ( 'NONE',  ( 4.699217343460686536, -0.5580910489941055541, 2.014698706189700594 ) ) ;
#79465 = CARTESIAN_POINT ( 'NONE',  ( 0.6674790882334122877, 15.00000000000000355, 11.66566053519463608 ) ) ;
#79467 = CARTESIAN_POINT ( 'NONE',  ( 0.02373106683711476844, -1.352142385343929387, -1.725327757841053078 ) ) ;
#79466 = CARTESIAN_POINT ( 'NONE',  ( 1.558973042058037439, 8.694236233170199668, -2.499999999999989786 ) ) ;
#79468 = CARTESIAN_POINT ( 'NONE',  ( 4.031004160980892870, -1.202209430963938619, -1.258585379614601596 ) ) ;
#79469 = CARTESIAN_POINT ( 'NONE',  ( 7.391166297744269365, 11.77477778067701664, 1.040834085586084257E-14 ) ) ;
#79470 = CARTESIAN_POINT ( 'NONE',  ( -8.064677165291197269, -5.223431457505076203, 7.446209719563364082 ) ) ;
#79471 = CARTESIAN_POINT ( 'NONE',  ( 4.323420094722703944, -1.284794005617446278, 1.164475704859231131 ) ) ;
#79472 = CARTESIAN_POINT ( 'NONE',  ( 4.422458135217792297, 1.019899284492602698, 1.916704820016806199 ) ) ;
#79473 = CARTESIAN_POINT ( 'NONE',  ( 2.672928840188529609, 6.270167413528593414, 0.000000000000000000 ) ) ;
#79474 = CARTESIAN_POINT ( 'NONE',  ( 6.087125082597877324, 1.679220375458953862, 1.116214469231976869 ) ) ;
#79475 = CARTESIAN_POINT ( 'NONE',  ( 5.531250000000004441, -0.7852924748302730906, -1.895863743163958226 ) ) ;
#79476 = CARTESIAN_POINT ( 'NONE',  ( -3.476130333331279854, 6.301985902010497576, 1.046962579147314498 ) ) ;
#79477 = CARTESIAN_POINT ( 'NONE',  ( 3.170836325157891267, -1.779339148710285867, -0.7386555552950261339 ) ) ;
#79478 = CARTESIAN_POINT ( 'NONE',  ( -6.009258394948636914E-15, 10.46875000068279604, -1.732050807568875195 ) ) ;
#79479 = CARTESIAN_POINT ( 'NONE',  ( 0.1006276693296826175, -1.041319732255343355, 1.962097497535258084 ) ) ;
#79480 = ORIENTED_EDGE ( 'NONE', *, *, #196460, .F. ) ;
#79481 = CARTESIAN_POINT ( 'NONE',  ( 6.883263157960335832, 7.629137130509051623, 2.446189081643288521 ) ) ;
#79482 = CARTESIAN_POINT ( 'NONE',  ( 1.499999999999987121, 3.045833333333353377, -0.8660254037844262731 ) ) ;
#79483 = CARTESIAN_POINT ( 'NONE',  ( 6.322179702674084467, 6.270297829408224111, 1.040834085586084257E-14 ) ) ;
#79485 = CARTESIAN_POINT ( 'NONE',  ( 6.689906388054261299, -1.280585065398877731, -1.486383542710855821 ) ) ;
#79484 = MECHANICAL_DESIGN_GEOMETRIC_PRESENTATION_REPRESENTATION (  '', ( #134861 ), #41483 ) ;
#79486 = CARTESIAN_POINT ( 'NONE',  ( 8.595506201384020883, 9.130438111143927671, 0.7216878364870438212 ) ) ;
#79487 = CARTESIAN_POINT ( 'NONE',  ( 1.499999999999993117, 10.13541666734946922, 0.8660254037844408170 ) ) ;
#79488 = CARTESIAN_POINT ( 'NONE',  ( 4.903208829997618423, 5.749440385532527564, -1.199719254218450271 ) ) ;
#79489 = CARTESIAN_POINT ( 'NONE',  ( 0.07093568767341934533, -0.9480374005119349690, 1.779628194860154222 ) ) ;
#79491 = CARTESIAN_POINT ( 'NONE',  ( 5.301261097381549270, -1.770826635688247386, 1.057502194177829979 ) ) ;
#79490 = CARTESIAN_POINT ( 'NONE',  ( -3.023105066167326882, 5.702484939155337607, -7.499999999999997335 ) ) ;
#79492 = CARTESIAN_POINT ( 'NONE',  ( 4.882344714252594642, 4.868692719482363707, 0.000000000000000000 ) ) ;
#79493 = CARTESIAN_POINT ( 'NONE',  ( -2.930533758848195447, 6.570706485298192234, -0.7998128361456281477 ) ) ;
#79494 = CARTESIAN_POINT ( 'NONE',  ( -0.7500000000000215383, 4.972916667349482012, 1.299038105676671107 ) ) ;
#79495 = CARTESIAN_POINT ( 'NONE',  ( -0.6823417656250003738, 1.217708333674752286, -1.181850606188749264 ) ) ;
#79496 = CARTESIAN_POINT ( 'NONE',  ( 6.854772330626868637, -1.445518619047950981, 1.186913843143226233 ) ) ;
#79497 = CARTESIAN_POINT ( 'NONE',  ( 5.643113243286411063, 0.7107029072939261560, 1.582047324045066095 ) ) ;
#79498 = CARTESIAN_POINT ( 'NONE',  ( 5.565861978284946332, -1.097836388496459037, 1.350534753149737366 ) ) ;
#79499 = CARTESIAN_POINT ( 'NONE',  ( 3.334415713957098681, 5.977569868670206787, -1.199719254218446718 ) ) ;
#79500 = ADVANCED_FACE ( 'NONE', ( #111679 ), #211224, .F. ) ;
#79501 = CARTESIAN_POINT ( 'NONE',  ( 3.175583430956610886, 1.455732557240730696, 1.770799584264992399 ) ) ;
#79502 = CARTESIAN_POINT ( 'NONE',  ( -1.001543065824772872E-14, 5.134375000341421469, 1.575800808251672791 ) ) ;
#79503 = CARTESIAN_POINT ( 'NONE',  ( 1.411775340717499994, 1.237668241052336970, -1.363247244775968259 ) ) ;
#79504 = CARTESIAN_POINT ( 'NONE',  ( 4.108200496220536735, 7.684552599041165166, 0.7063325572433389876 ) ) ;
#79505 = CARTESIAN_POINT ( 'NONE',  ( 0.000000000000000000, 3.999999999999996447, 0.000000000000000000 ) ) ;
#79506 = CARTESIAN_POINT ( 'NONE',  ( 1.799542586263824795, -0.6183211656001773582, 1.717807299235304619 ) ) ;
#79507 = CARTESIAN_POINT ( 'NONE',  ( 2.391250195717840477, -0.7743161457766101208, -1.862016636315230844 ) ) ;
#79508 = CARTESIAN_POINT ( 'NONE',  ( 1.658417429842372393, -1.548019161032044844, 1.551412955586493947 ) ) ;
#79509 = CARTESIAN_POINT ( 'NONE',  ( 7.209027064991026634, 14.97176420577651079, -9.190340992810662968 ) ) ;
#79510 = CARTESIAN_POINT ( 'NONE',  ( 4.471769775969771210, 2.043305595564361088, -0.5093722314385378258 ) ) ;
#79511 = CARTESIAN_POINT ( 'NONE',  ( -6.877010230629689858, 9.046264573866535486, 1.599625672291283607 ) ) ;
#79512 = CARTESIAN_POINT ( 'NONE',  ( 8.232418323234554691, 14.52480782996326880, 8.289887465044873949 ) ) ;
#79513 = ADVANCED_FACE ( 'NONE', ( #14078 ), #48751, .T. ) ;
#79514 = CARTESIAN_POINT ( 'NONE',  ( 1.047426762419433777, 1.826728496382063582, -0.9743617655595809834 ) ) ;
#79515 = CARTESIAN_POINT ( 'NONE',  ( 5.192936529234042808, 6.017179691316550283, -1.199719254218452047 ) ) ;
#79516 = CARTESIAN_POINT ( 'NONE',  ( 0.6801582343749883464, -0.7447916663252535097, 1.178068619123796568 ) ) ;
#79517 = CARTESIAN_POINT ( 'NONE',  ( 4.758503674095369007, 2.114844282287762667, 0.1552407789479764155 ) ) ;
#79519 = ADVANCED_FACE ( 'NONE', ( #176615 ), #63131, .F. ) ;
#79518 = CARTESIAN_POINT ( 'NONE',  ( 6.147073579019600054, -1.539581890156189292, 0.9809480439507823890 ) ) ;
#79520 = EDGE_LOOP ( 'NONE', ( #101836, #15925, #143824, #134606 ) ) ;
#79521 = CARTESIAN_POINT ( 'NONE',  ( -5.173318132066234476, 8.193232366456022930, -1.199719254218453823 ) ) ;
#79522 = CARTESIAN_POINT ( 'NONE',  ( 9.694243528971124846, 11.26870452434320491, 1.199719254218450271 ) ) ;
#79523 = CARTESIAN_POINT ( 'NONE',  ( 6.089020385868848528, 8.197219431637373432, -1.443375672974078761 ) ) ;
#79524 = CARTESIAN_POINT ( 'NONE',  ( 3.475000000000000533, -1.910416665710751305, 2.006292185433948827 ) ) ;
#79525 = CARTESIAN_POINT ( 'NONE',  ( -5.362413449404877852, 6.214902764849178141, -1.199719254218446718 ) ) ;
#79526 = CARTESIAN_POINT ( 'NONE',  ( 6.205353461901607304, 1.844339991697005798, -1.046509186232460697 ) ) ;
#79527 = CARTESIAN_POINT ( 'NONE',  ( 1.184755817749640894, -2.054561091436296838, -0.4616562467647678525 ) ) ;
#79528 = CARTESIAN_POINT ( 'NONE',  ( -6.479871072688648148, 6.524547437750345402, 0.000000000000000000 ) ) ;
#79529 = CARTESIAN_POINT ( 'NONE',  ( 8.041957671200231417, 12.53403438304231976, 1.040834085586084257E-14 ) ) ;
#79530 = CARTESIAN_POINT ( 'NONE',  ( 5.453892037968048001, -0.6717839469763884352, 1.735626407379993186 ) ) ;
#79531 = CARTESIAN_POINT ( 'NONE',  ( 7.670162217029129259, 9.971608557999250166, 1.599625672291281386 ) ) ;
#79532 = CARTESIAN_POINT ( 'NONE',  ( 4.893239572183122554, 4.893064124118063241, -0.6979708156788643203 ) ) ;
#79533 = CARTESIAN_POINT ( 'NONE',  ( -5.307090785106547415, 5.156303768904543894, -0.7998128361456362523 ) ) ;
#79534 = CARTESIAN_POINT ( 'NONE',  ( -9.991996023591624976, 10.75967623705280296, 1.040834085586084257E-14 ) ) ;
#79536 = CARTESIAN_POINT ( 'NONE',  ( 2.189831975649577878, -1.279155337443920404, -1.487614327915102841 ) ) ;
#79535 = CARTESIAN_POINT ( 'NONE',  ( -7.369020184227459858, 8.555943955475521889, 1.199719254218450271 ) ) ;
#79537 = CARTESIAN_POINT ( 'NONE',  ( 0.6026772488060898603, -0.7295331166810551382, -2.035022307366324945 ) ) ;
#79539 = CARTESIAN_POINT ( 'NONE',  ( -6.113138475847556208, 6.011394290285472231, -0.2943476003282770037 ) ) ;
#79538 = CARTESIAN_POINT ( 'NONE',  ( -6.286140498591554326, 7.362860665558790707, 1.199719254218452047 ) ) ;
#79540 = CARTESIAN_POINT ( 'NONE',  ( 1.364683531249988757, 0.8843750003414210248, 0.000000000000000000 ) ) ;
#79541 = CARTESIAN_POINT ( 'NONE',  ( 3.356526315702735186, -0.7047320765170405066, 1.584360681437890550 ) ) ;
#79542 = CARTESIAN_POINT ( 'NONE',  ( 2.941039689149751890, 0.6260299441606477222, -1.624016774299047228 ) ) ;
#79543 = CARTESIAN_POINT ( 'NONE',  ( 6.317736394288122170, 10.31451686007074997, 0.7216878364870438212 ) ) ;
#79544 = CARTESIAN_POINT ( 'NONE',  ( -11.76696981052429614, 4.673730779118272061, -4.995440715239800156 ) ) ;
#79545 = CARTESIAN_POINT ( 'NONE',  ( 2.776696059289599283, -1.970994871289712069, -0.6015693623636628740 ) ) ;
#79546 = CARTESIAN_POINT ( 'NONE',  ( 0.7200771085676247463, -1.701685607325746252, -1.080902626906909747 ) ) ;
#79547 = CARTESIAN_POINT ( 'NONE',  ( 6.925078400183575233, 2.022016365062285104, 2.447829694591229899 ) ) ;
#79548 = CARTESIAN_POINT ( 'NONE',  ( -3.786470039966538970, 7.639575156594750283, 0.000000000000000000 ) ) ;
#79549 = EDGE_CURVE ( 'NONE', #1432, #177149, #191739, .T. ) ;
#79550 = CARTESIAN_POINT ( 'NONE',  ( 1.147272922670502515, -1.552894836003695600, -1.214464739729806730 ) ) ;
#79552 = CARTESIAN_POINT ( 'NONE',  ( -6.956742217587851052, 7.288823140040177506, 0.000000000000000000 ) ) ;
#79551 = CARTESIAN_POINT ( 'NONE',  ( 6.328373294368253354, -0.9077179077918960948, -1.683272687665722467 ) ) ;
#79553 = CARTESIAN_POINT ( 'NONE',  ( -5.112833325684904118, 8.979072956692109031, -0.7216878364870338292 ) ) ;
#79554 = CARTESIAN_POINT ( 'NONE',  ( 5.691390622686558487, 9.861982503101517139, 0.7998128361456341429 ) ) ;
#79555 = CARTESIAN_POINT ( 'NONE',  ( -7.119966945832006289, 8.335658187339330283, 1.199719254218452047 ) ) ;
#79556 = CARTESIAN_POINT ( 'NONE',  ( 0.7330764811492549438, 1.866981473359119237, 0.7708630573498123084 ) ) ;
#79557 = CARTESIAN_POINT ( 'NONE',  ( 4.313705703444643547, -0.3987071732099633503, 2.272742389722400169 ) ) ;
#79558 = CARTESIAN_POINT ( 'NONE',  ( 6.004347769543215030, 1.959566550440184907, 0.09775035808561728656 ) ) ;
#79559 = CARTESIAN_POINT ( 'NONE',  ( 2.430452978529148655, -1.210835280720125917, 1.543375930141199115 ) ) ;
#79560 = CARTESIAN_POINT ( 'NONE',  ( 10.24726517383036928, 10.84956421242393887, 0.000000000000000000 ) ) ;
#79561 = CARTESIAN_POINT ( 'NONE',  ( -0.05211191391743182078, -1.802403943428915412, -0.9041556775107385535 ) ) ;
#79562 = ORIENTED_EDGE ( 'NONE', *, *, #9705, .F. ) ;
#79563 = CARTESIAN_POINT ( 'NONE',  ( 1.288444443960437225, -0.7676182150243222591, -1.973457848717992569 ) ) ;
#79565 = CARTESIAN_POINT ( 'NONE',  ( -8.342344591110322227, 8.627156865917170236, -0.7998128361456291469 ) ) ;
#79564 = CARTESIAN_POINT ( 'NONE',  ( -4.029797971759847997, 5.724516938518342535, -1.599625672291256295 ) ) ;
#79566 = CARTESIAN_POINT ( 'NONE',  ( 1.411775340717499994, 1.237668241052336970, -1.363247244775968259 ) ) ;
#79567 = ORIENTED_EDGE ( 'NONE', *, *, #134419, .T. ) ;
#79568 = CARTESIAN_POINT ( 'NONE',  ( 4.821225769315531373, -1.936335391968559527, -0.9821231961690338741 ) ) ;
#79569 = CARTESIAN_POINT ( 'NONE',  ( 11.95068985293163344, 7.567001936134044371, 0.4555898092883722827 ) ) ;
#79570 = CARTESIAN_POINT ( 'NONE',  ( 2.074623746436579985, 0.9110886696130392481, 1.915067268644244702 ) ) ;
#79571 = CARTESIAN_POINT ( 'NONE',  ( -1.499999999999997780, 4.681250000682819490, 1.214306433183764966E-14 ) ) ;
#79572 = CARTESIAN_POINT ( 'NONE',  ( 7.944187942603509356, 11.35563746875774882, 1.199719254218460707 ) ) ;
#79573 = CARTESIAN_POINT ( 'NONE',  ( -2.788906526875773208E-15, 9.968750000682797818, -1.499999999999998446 ) ) ;
#79574 = CARTESIAN_POINT ( 'NONE',  ( 3.725900457647839392, -1.224662966953151688, -1.657274842633131851 ) ) ;
#79575 = CIRCLE ( 'NONE', #183314, 0.08000000000000004330 ) ;
#79577 = CARTESIAN_POINT ( 'NONE',  ( 0.1515692981730529243, 0.7036590017722235135, 1.701685288394996665 ) ) ;
#79576 = CARTESIAN_POINT ( 'NONE',  ( -7.365103760721662951, 9.615707025640515937, 1.599625672291295375 ) ) ;
#79578 = CARTESIAN_POINT ( 'NONE',  ( -0.6823417656250212460, 3.051041667008084879, 1.181850606188767472 ) ) ;
#79579 =( BOUNDED_SURFACE ( )  B_SPLINE_SURFACE ( 3, 3, ( 
 ( #121030, #137210, #116723, #203232, #52731, #38628, #154515, #37552, #104704, #169684, #167554, #170754, #70020, #150253, #182723, #19155, #135077, #6096, #72164, #138273, #34342, #118865, #201090, #36479, #123181, #206447, #77522, #55944, #92736, #11447 ),
 ( #126363, #105801, #59138, #204287, #93805, #122097, #8249, #43980, #41855, #110099, #40779, #26634, #158781, #192322, #74333, #73237, #140435, #58075, #176110, #141511, #205374, #188061, #139344, #171825, #155582, #159845, #57009, #207519, #109030, #24485 ),
 ( #10378, #25565, #27710, #191255, #124237, #157729, #76454, #9324, #125297, #190197, #42920, #175049, #142562, #107965, #173993, #208568, #39690, #91676, #90597, #23419, #189141, #89530, #60202, #7167, #75398, #106885, #172911, #156656, #84725, #134584 ),
 ( #133518, #200584, #194474, #128506, #35970, #149736, #144707, #1315, #143643, #94866, #28783, #150814, #117291, #209637, #2377, #145775, #183288, #118360, #80734, #100965, #199524, #160920, #51168, #47190, #12514, #61277, #177166, #29858, #68455, #113303 ),
 ( #178243, #78585, #67376, #211776, #179310, #163060, #46117, #193409, #112234, #210718, #63414, #52232, #45053, #34892, #127439, #102048, #111165, #161995, #13585, #79658, #30931, #184347, #167054, #18647, #97007, #19717, #62346, #129566, #14640, #195552 ),
 ( #95939, #168117, #139904, #23978, #152928, #56500, #120510, #137764, #5571, #135626, #171306, #22899, #71650, #121581, #69518, #205934, #203784, #57567, #136694, #122661, #40255, #7726, #104189, #169175, #170238, #154003, #123724, #89014, #86863, #201647 ),
 ( #90080, #37032, #55429, #53295, #189687, #187552, #87930, #39182, #188623, #105268, #41338, #72733, #21822, #155068, #172390, #6656, #138829, #204847, #106366, #156143, #73809, #107447, #173472, #85796, #151876, #3450, #186486, #119427, #4506, #185414 ) ),
 .UNSPECIFIED., .T., .F., .F. ) 
 B_SPLINE_SURFACE_WITH_KNOTS ( ( 4, 3, 4 ),
 ( 4, 2, 2, 2, 2, 2, 2, 2, 2, 2, 2, 2, 2, 2, 4 ),
 ( 0.000000000000000000, 0.5000000000000000000, 1.000000000000000000 ),
 ( 0.3904182756812821231, 0.3921283039710705687, 0.3938383322608589587, 0.3972583888404358499, 0.4040985019995896321, 0.4177787283178971967, 0.4451391809545123257, 0.4999364453639513206, 0.5547656701200603946, 0.5821739285757332460, 0.5958780578035696163, 0.6027301224174878014, 0.6061561547244469494, 0.6078691708779264680, 0.6095821870314059865 ),
 .UNSPECIFIED. ) 
 GEOMETRIC_REPRESENTATION_ITEM ( )  RATIONAL_B_SPLINE_SURFACE ( (
 ( 1.000000000000000000, 1.000000000000000000, 1.000000000000000000, 1.000000000000000000, 1.000000000000000000, 1.000000000000000000, 1.000000000000000000, 1.000000000000000000, 1.000000000000000000, 1.000000000000000000, 1.000000000000000000, 1.000000000000000000, 1.000000000000000000, 1.000000000000000000, 1.000000000000000000, 1.000000000000000000, 1.000000000000000000, 1.000000000000000000, 1.000000000000000000, 1.000000000000000000, 1.000000000000000000, 1.000000000000000000, 1.000000000000000000, 1.000000000000000000, 1.000000000000000000, 1.000000000000000000, 1.000000000000000000, 1.000000000000000000, 1.000000000000000000, 1.000000000000000000),
 ( 0.3333333333333333703, 0.3333333333333333703, 0.3333333333333333703, 0.3333333333333333703, 0.3333333333333333703, 0.3333333333333333703, 0.3333333333333333703, 0.3333333333333333703, 0.3333333333333333703, 0.3333333333333333703, 0.3333333333333333703, 0.3333333333333333703, 0.3333333333333333703, 0.3333333333333333703, 0.3333333333333333703, 0.3333333333333333703, 0.3333333333333333703, 0.3333333333333333703, 0.3333333333333333703, 0.3333333333333333703, 0.3333333333333333703, 0.3333333333333333703, 0.3333333333333333703, 0.3333333333333333703, 0.3333333333333333703, 0.3333333333333333703, 0.3333333333333333703, 0.3333333333333333703, 0.3333333333333333703, 0.3333333333333333703),
 ( 0.3333333333333333703, 0.3333333333333333703, 0.3333333333333333703, 0.3333333333333333703, 0.3333333333333333703, 0.3333333333333333703, 0.3333333333333333703, 0.3333333333333333703, 0.3333333333333333703, 0.3333333333333333703, 0.3333333333333333703, 0.3333333333333333703, 0.3333333333333333703, 0.3333333333333333703, 0.3333333333333333703, 0.3333333333333333703, 0.3333333333333333703, 0.3333333333333333703, 0.3333333333333333703, 0.3333333333333333703, 0.3333333333333333703, 0.3333333333333333703, 0.3333333333333333703, 0.3333333333333333703, 0.3333333333333333703, 0.3333333333333333703, 0.3333333333333333703, 0.3333333333333333703, 0.3333333333333333703, 0.3333333333333333703),
 ( 1.000000000000000000, 1.000000000000000000, 1.000000000000000000, 1.000000000000000000, 1.000000000000000000, 1.000000000000000000, 1.000000000000000000, 1.000000000000000000, 1.000000000000000000, 1.000000000000000000, 1.000000000000000000, 1.000000000000000000, 1.000000000000000000, 1.000000000000000000, 1.000000000000000000, 1.000000000000000000, 1.000000000000000000, 1.000000000000000000, 1.000000000000000000, 1.000000000000000000, 1.000000000000000000, 1.000000000000000000, 1.000000000000000000, 1.000000000000000000, 1.000000000000000000, 1.000000000000000000, 1.000000000000000000, 1.000000000000000000, 1.000000000000000000, 1.000000000000000000),
 ( 0.3333333333333333703, 0.3333333333333333703, 0.3333333333333333703, 0.3333333333333333703, 0.3333333333333333703, 0.3333333333333333703, 0.3333333333333333703, 0.3333333333333333703, 0.3333333333333333703, 0.3333333333333333703, 0.3333333333333333703, 0.3333333333333333703, 0.3333333333333333703, 0.3333333333333333703, 0.3333333333333333703, 0.3333333333333333703, 0.3333333333333333703, 0.3333333333333333703, 0.3333333333333333703, 0.3333333333333333703, 0.3333333333333333703, 0.3333333333333333703, 0.3333333333333333703, 0.3333333333333333703, 0.3333333333333333703, 0.3333333333333333703, 0.3333333333333333703, 0.3333333333333333703, 0.3333333333333333703, 0.3333333333333333703),
 ( 0.3333333333333333703, 0.3333333333333333703, 0.3333333333333333703, 0.3333333333333333703, 0.3333333333333333703, 0.3333333333333333703, 0.3333333333333333703, 0.3333333333333333703, 0.3333333333333333703, 0.3333333333333333703, 0.3333333333333333703, 0.3333333333333333703, 0.3333333333333333703, 0.3333333333333333703, 0.3333333333333333703, 0.3333333333333333703, 0.3333333333333333703, 0.3333333333333333703, 0.3333333333333333703, 0.3333333333333333703, 0.3333333333333333703, 0.3333333333333333703, 0.3333333333333333703, 0.3333333333333333703, 0.3333333333333333703, 0.3333333333333333703, 0.3333333333333333703, 0.3333333333333333703, 0.3333333333333333703, 0.3333333333333333703),
 ( 1.000000000000000000, 1.000000000000000000, 1.000000000000000000, 1.000000000000000000, 1.000000000000000000, 1.000000000000000000, 1.000000000000000000, 1.000000000000000000, 1.000000000000000000, 1.000000000000000000, 1.000000000000000000, 1.000000000000000000, 1.000000000000000000, 1.000000000000000000, 1.000000000000000000, 1.000000000000000000, 1.000000000000000000, 1.000000000000000000, 1.000000000000000000, 1.000000000000000000, 1.000000000000000000, 1.000000000000000000, 1.000000000000000000, 1.000000000000000000, 1.000000000000000000, 1.000000000000000000, 1.000000000000000000, 1.000000000000000000, 1.000000000000000000, 1.000000000000000000) ) ) 
 REPRESENTATION_ITEM ( '' )  SURFACE ( )  );
#79580 = CARTESIAN_POINT ( 'NONE',  ( 1.499745039105476296, 4.349213141111352599, 0.07702037080406516634 ) ) ;
#79581 = CARTESIAN_POINT ( 'NONE',  ( -3.046854503058780139, 2.800000000000024691, -2.500000000000000444 ) ) ;
#79582 = CARTESIAN_POINT ( 'NONE',  ( 2.196875584952286964, -0.6017768564574823564, -2.180865832541518667 ) ) ;
#79583 = CARTESIAN_POINT ( 'NONE',  ( -9.164948653157999559, 10.75515685251491504, -1.082531754730539753 ) ) ;
#79584 = CARTESIAN_POINT ( 'NONE',  ( 2.900440330899815233, -1.785477387793675597, -0.3053432404436141057 ) ) ;
#79585 = CARTESIAN_POINT ( 'NONE',  ( 1.920960065284383678, -1.709437138374754639, 0.8649676252809009869 ) ) ;
#79586 = CARTESIAN_POINT ( 'NONE',  ( 3.121598655985452275, 0.3063859900464052100, -2.047459029603612368 ) ) ;
#79587 = CARTESIAN_POINT ( 'NONE',  ( -1.201851678989727383E-14, 1.884375000341422135, 1.575800808251672791 ) ) ;
#79588 = CARTESIAN_POINT ( 'NONE',  ( 1.533988556244444856, 0.9736202887896376890, -1.714215200822625684 ) ) ;
#79589 = CARTESIAN_POINT ( 'NONE',  ( 6.199827818874126706, -0.6464308959919072839, 1.814938386029739892 ) ) ;
#79590 = CARTESIAN_POINT ( 'NONE',  ( 2.940157781200231746, 1.856316385841882965, 0.2306766016651334850 ) ) ;
#79591 = AXIS2_PLACEMENT_3D ( 'NONE', #141108, #58744, #172508 ) ;
#79593 = CARTESIAN_POINT ( 'NONE',  ( 4.605689926069578277, 8.476745573306274650, -0.2140288463435610078 ) ) ;
#79592 = CARTESIAN_POINT ( 'NONE',  ( 1.383892495861089644, 2.130622466349596511, -0.8869745915042435147 ) ) ;
#79594 = CARTESIAN_POINT ( 'NONE',  ( 2.875287963320713569, -0.1852811808005799254, 1.851819283609082323 ) ) ;
#79595 = CARTESIAN_POINT ( 'NONE',  ( 0.6823417656249899377, 3.092708333674754062, 1.181850606188765695 ) ) ;
#79596 = CARTESIAN_POINT ( 'NONE',  ( 5.723111435942265679, -1.863175293877845418, -0.8853075346121098699 ) ) ;
#79597 = CARTESIAN_POINT ( 'NONE',  ( -5.087333953625788219, 6.958308917361963886, 1.599625672291267398 ) ) ;
#79598 = CARTESIAN_POINT ( 'NONE',  ( 7.949158136313996259, 8.168439335321471262, 1.040834085586084257E-14 ) ) ;
#79599 = CARTESIAN_POINT ( 'NONE',  ( -1.423138288543982055, 3.910258984626137746, 0.4995221786828126787 ) ) ;
#79600 = CARTESIAN_POINT ( 'NONE',  ( 6.299853487814777608, -0.7131585336714525436, 1.981663801677714831 ) ) ;
#79601 = CARTESIAN_POINT ( 'NONE',  ( -1.364683531250012516, 2.551041667008089320, -0.7879004041258289570 ) ) ;
#79602 = CARTESIAN_POINT ( 'NONE',  ( 5.518883860308030798, 1.994880785013030788, 0.8329173350848093627 ) ) ;
#79603 = CARTESIAN_POINT ( 'NONE',  ( 6.551426717330563143, -1.803173079755305608, 0.9099084737219197416 ) ) ;
#79604 = CARTESIAN_POINT ( 'NONE',  ( -1.364683531250014514, -0.9697916663252473812, 0.7879004041258379498 ) ) ;
#79605 = CARTESIAN_POINT ( 'NONE',  ( -5.585596099150193616, 6.579245539505756746, -1.082531754730544860 ) ) ;
#79608 = CARTESIAN_POINT ( 'NONE',  ( 5.680503174445848735, 5.729601246382692636, 1.040834085586084257E-14 ) ) ;
#79607 = CARTESIAN_POINT ( 'NONE',  ( 6.925078400183550364, 2.474256779287649088, 2.140290375984225335 ) ) ;
#79606 = CARTESIAN_POINT ( 'NONE',  ( 5.363132282657546490, 8.414682208812571673, -1.199719254218452047 ) ) ;
#79609 = CARTESIAN_POINT ( 'NONE',  ( -4.492547798081878874, 6.334668079219206049, 1.599625672291263179 ) ) ;
#79610 = CARTESIAN_POINT ( 'NONE',  ( 4.171111447311355747, 1.799123655847803205, -0.9110083886025857058 ) ) ;
#79611 = CARTESIAN_POINT ( 'NONE',  ( -7.714753101375940503, 8.959299025482085455, 1.199719254218462483 ) ) ;
#79613 = CARTESIAN_POINT ( 'NONE',  ( -7.566859129758459979, 8.000626204239226880, 0.000000000000000000 ) ) ;
#79612 = CARTESIAN_POINT ( 'NONE',  ( -8.676855123066019360, 11.14608361504227574, -1.443375672974059665 ) ) ;
#79614 = CARTESIAN_POINT ( 'NONE',  ( -1.001543065824772872E-14, 5.571875000341416140, 1.575800808251672791 ) ) ;
#79616 = CARTESIAN_POINT ( 'NONE',  ( 0.6823417656249934904, 9.692708333674735499, 1.181850606188764807 ) ) ;
#79615 = CARTESIAN_POINT ( 'NONE',  ( 5.770447993230207295, -1.374857387916775364, 1.668144713590607120 ) ) ;
#79617 = CARTESIAN_POINT ( 'NONE',  ( 0.000000000000000000, 0.2000000000000057288, 0.000000000000000000 ) ) ;
#79618 = CARTESIAN_POINT ( 'NONE',  ( -11.73318219666202999, 7.416709190724854572, 2.527811172656401428 ) ) ;
#79620 = CARTESIAN_POINT ( 'NONE',  ( 5.712517600013328867, 1.944077172375497486, 0.5350714256760413789 ) ) ;
#79619 = CARTESIAN_POINT ( 'NONE',  ( -7.171900071504748730, 8.429933507252760805, -1.082531754730549078 ) ) ;
#79621 = CARTESIAN_POINT ( 'NONE',  ( 1.364683531249986537, -0.8239583329919186738, 0.7879004041258500513 ) ) ;
#79622 = CARTESIAN_POINT ( 'NONE',  ( 1.418105696869888410, 1.160834107949513472, -1.275986549933407543 ) ) ;
#79623 = CARTESIAN_POINT ( 'NONE',  ( 5.411639590510088027, 6.342609606130419131, -1.199719254218452047 ) ) ;
#79625 = CARTESIAN_POINT ( 'NONE',  ( 5.559725510055676168, 8.644040974110419384, 1.199719254218451159 ) ) ;
#79624 = CARTESIAN_POINT ( 'NONE',  ( 7.131225611108088280, 9.342849184424693476, 1.443375672974076540 ) ) ;
#79626 = CARTESIAN_POINT ( 'NONE',  ( -11.71717583921413208, 8.541564709976100289, -2.387000931153457461 ) ) ;
#79627 = CARTESIAN_POINT ( 'NONE',  ( 6.081297793977560318, 1.728434112010367674, -0.7156336962577531935 ) ) ;
#79628 = CARTESIAN_POINT ( 'NONE',  ( 1.242838715397933225, 1.940741670474394498, 0.5346661475282618037 ) ) ;
#79629 = CARTESIAN_POINT ( 'NONE',  ( 0.000000000000000000, 0.5999999999999998668, 0.000000000000000000 ) ) ;
#79630 = CARTESIAN_POINT ( 'NONE',  ( 3.030518406005321186, 1.227118389542980026, -1.833929004854919054 ) ) ;
#79631 = ADVANCED_FACE ( 'NONE', ( #85495 ), #86567, .T. ) ;
#79632 = CARTESIAN_POINT ( 'NONE',  ( 5.295835511405859286, -1.530271966869084954, -1.540324818649402072 ) ) ;
#79633 = VERTEX_POINT ( 'NONE', #98560 ) ;
#79634 = CARTESIAN_POINT ( 'NONE',  ( 0.7499999999999885647, -0.2666666666666442365, 1.299038105676657340 ) ) ;
#79635 = CARTESIAN_POINT ( 'NONE',  ( 10.19536832735223975, 10.99694392477354477, 0.000000000000000000 ) ) ;
#79637 = CARTESIAN_POINT ( 'NONE',  ( 2.091422941747251851, -0.4390073250180904219, 1.967893905867940996 ) ) ;
#79636 = CARTESIAN_POINT ( 'NONE',  ( 3.721430941620011534, 1.819509361161365524, 1.088713516244857571 ) ) ;
#79639 = ORIENTED_EDGE ( 'NONE', *, *, #33991, .F. ) ;
#79638 = CARTESIAN_POINT ( 'NONE',  ( 1.880848235559588799, -1.657448921354220506, -0.7316143304627804600 ) ) ;
#79640 = CARTESIAN_POINT ( 'NONE',  ( 7.374709211190586089, 7.568525266002632534, 0.000000000000000000 ) ) ;
#79641 = VERTEX_POINT ( 'NONE', #148382 ) ;
#79643 = EDGE_CURVE ( 'NONE', #193413, #160443, #198168, .T. ) ;
#79642 = CIRCLE ( 'NONE', #159264, 0.07999999999999946043 ) ;
#79644 = CARTESIAN_POINT ( 'NONE',  ( 5.799137018343234473, 7.788745826199009237, -1.599625672291262513 ) ) ;
#79646 = CARTESIAN_POINT ( 'NONE',  ( 1.569406966088880084, 1.323937531303821968, 1.384834552875470415 ) ) ;
#79645 = CARTESIAN_POINT ( 'NONE',  ( -3.554208825076827782, 7.298327395898266623, 0.7998128361456341429 ) ) ;
#79647 = DIRECTION ( 'NONE',  ( -0.7613463080411786432, 0.000000000000000000, -0.6483454320283800199 ) ) ;
#79648 = CARTESIAN_POINT ( 'NONE',  ( -4.862871242741148237, 4.993698027119869209, -0.7753252576984640543 ) ) ;
#79649 = CARTESIAN_POINT ( 'NONE',  ( 4.948362878863507675, 8.716914425408678113, -0.7216878364870267237 ) ) ;
#79650 = CARTESIAN_POINT ( 'NONE',  ( -0.6823417656250246877, 0.3635416670080895973, 1.181850606188755259 ) ) ;
#79651 = FACE_OUTER_BOUND ( 'NONE', #121183, .T. ) ;
#79652 = CARTESIAN_POINT ( 'NONE',  ( -8.109748439268576803, 12.61312361245537517, 0.7998128361456481317 ) ) ;
#79653 = CARTESIAN_POINT ( 'NONE',  ( 4.821240550277555492, -0.1094919189667045711, 2.159058991224649393 ) ) ;
#79654 = CARTESIAN_POINT ( 'NONE',  ( -5.980555157403903976, 6.149938236492225485, 0.000000000000000000 ) ) ;
#79655 = CARTESIAN_POINT ( 'NONE',  ( 4.068855497876973537, 7.761098824249525130, -0.7216878364870338292 ) ) ;
#79656 = CARTESIAN_POINT ( 'NONE',  ( 2.637105894733019262, 1.998242115483703341, 0.7103459930332192140 ) ) ;
#79658 = CARTESIAN_POINT ( 'NONE',  ( -12.06809232949933275, 5.701620653239091396, -4.345812045493805620 ) ) ;
#79657 = CARTESIAN_POINT ( 'NONE',  ( 0.7499999999999920064, 5.733333333333353821, 1.299038105676669330 ) ) ;
#79659 = CARTESIAN_POINT ( 'NONE',  ( 3.057844483195955032, 1.962173284599289858, -0.1898399627659839439 ) ) ;
#79660 = CARTESIAN_POINT ( 'NONE',  ( 5.220932206144772714, 1.444093599275039885, -1.253800916539760113 ) ) ;
#79661 = ORIENTED_EDGE ( 'NONE', *, *, #192419, .T. ) ;
#79662 = DIRECTION ( 'NONE',  ( 0.000000000000000000, 1.000000000000000000, 0.000000000000000000 ) ) ;
#79663 = CARTESIAN_POINT ( 'NONE',  ( 0.2564123431100414074, -2.069877475643782994, -0.05227228806716639753 ) ) ;
#79664 = CARTESIAN_POINT ( 'NONE',  ( 2.572129589083424150, -1.858482343604623610, -0.5632287606567585314 ) ) ;
#79665 = ORIENTED_EDGE ( 'NONE', *, *, #99125, .F. ) ;
#79666 = CARTESIAN_POINT ( 'NONE',  ( 2.295757763869426871, 5.519548059767960702, 0.4031905389056070765 ) ) ;
#79668 = CARTESIAN_POINT ( 'NONE',  ( -10.62873463776380056, 9.799999999999998934, -3.200000000000001510 ) ) ;
#79667 = CARTESIAN_POINT ( 'NONE',  ( -5.912764389335557702, 8.951956649983198844, 1.082531754730550855 ) ) ;
#79670 = CARTESIAN_POINT ( 'NONE',  ( 6.657217119509961201, 7.725507046638470321, -1.199719254218446718 ) ) ;
#79669 = CARTESIAN_POINT ( 'NONE',  ( 2.168024591681999791, -1.285456077792548335, 1.648657952768191715 ) ) ;
#79671 = CARTESIAN_POINT ( 'NONE',  ( 3.553645660113312399, 7.160020680191912845, -1.734723475976807094E-15 ) ) ;
#79673 = ORIENTED_EDGE ( 'NONE', *, *, #90947, .F. ) ;
#79672 = CARTESIAN_POINT ( 'NONE',  ( 6.393217174440144035, -0.09883813596619006603, -1.909861267343159863 ) ) ;
#79674 = CARTESIAN_POINT ( 'NONE',  ( 3.897267319706390065, 1.864829029706360330, -1.179861312946443697 ) ) ;
#79675 = CARTESIAN_POINT ( 'NONE',  ( 3.522699392456357881, 1.401646575410384843, -1.704459333586108016 ) ) ;
#79676 = CARTESIAN_POINT ( 'NONE',  ( 9.271078113646423091, 9.710679308875986848, 1.040834085586084257E-14 ) ) ;
#79677 = CARTESIAN_POINT ( 'NONE',  ( -1.360316468750013108, 2.921875000341411788, -1.734723475976807094E-14 ) ) ;
#79678 = CARTESIAN_POINT ( 'NONE',  ( 2.033716200607054159, -1.854476301366870805, 0.4660679227486630438 ) ) ;
#79679 = STYLED_ITEM ( 'NONE', ( #151982 ), #55192 ) ;
#79680 = CARTESIAN_POINT ( 'NONE',  ( 8.940712233207955606, 12.51824914112961729, 1.199719254218450271 ) ) ;
#79681 = CARTESIAN_POINT ( 'NONE',  ( 4.580570967453869713, 1.276285970795057345, -1.630082184409971324 ) ) ;
#79683 = CARTESIAN_POINT ( 'NONE',  ( 3.362350911093567873, 0.9703303321016673033, 1.931748911306984784 ) ) ;
#79682 = CARTESIAN_POINT ( 'NONE',  ( -3.195971524519394702, 4.751719416737803847, -1.599625672291262513 ) ) ;
#79684 = CARTESIAN_POINT ( 'NONE',  ( 4.933237592207079025, -1.549687834843778811, -1.549900206446311657 ) ) ;
#79685 = DIRECTION ( 'NONE',  ( -0.2684563758389304500, -5.222015543130708508E-15, 0.9632918427306581544 ) ) ;
#79686 =( LENGTH_UNIT ( ) NAMED_UNIT ( * ) SI_UNIT ( .MILLI., .METRE. ) );
#79687 = CARTESIAN_POINT ( 'NONE',  ( -0.07580519709491854996, 7.079373232791049020, 2.120991669647492639 ) ) ;
#79688 = CARTESIAN_POINT ( 'NONE',  ( 6.073126464278658432, 6.050012061272033392, 0.000000000000000000 ) ) ;
#79689 = CARTESIAN_POINT ( 'NONE',  ( -3.285556943750000070, -2.646874999522041971, 0.000000000000000000 ) ) ;
#79690 = CARTESIAN_POINT ( 'NONE',  ( -4.787964524281469458, 5.614988695530339413, -1.199719254218453823 ) ) ;
#79691 = CARTESIAN_POINT ( 'NONE',  ( 0.5982800022500452952, -0.2930678230431381648, 1.994870242743536304 ) ) ;
#79692 = CARTESIAN_POINT ( 'NONE',  ( -8.134528978519403708, 11.47373899403920205, 1.082531754730549967 ) ) ;
#79693 = CARTESIAN_POINT ( 'NONE',  ( 4.803616497939601437, -1.596918191575155133, -1.317456641179854726 ) ) ;
#79694 = CARTESIAN_POINT ( 'NONE',  ( 2.877471820773948252, 1.829258416151048561, -0.6045268202574998195 ) ) ;
#79695 = CARTESIAN_POINT ( 'NONE',  ( 6.169547404874395014, 1.460173559465412829, 1.533355976833279621 ) ) ;
#79696 = CARTESIAN_POINT ( 'NONE',  ( 4.310602774141044868, 7.116454772218158809, -1.199719254218452047 ) ) ;
#79697 = DIRECTION ( 'NONE',  ( 0.000000000000000000, 0.000000000000000000, -1.000000000000000000 ) ) ;
#79698 = CARTESIAN_POINT ( 'NONE',  ( 4.522284192717240359, 0.9245163773116799044, 1.738918859443546516 ) ) ;
#79699 = CARTESIAN_POINT ( 'NONE',  ( 6.140627040082555332, -1.939752761746313059, 1.221158637518650503 ) ) ;
#79700 = CARTESIAN_POINT ( 'NONE',  ( 4.353998665852670591, 1.825246345946249571, -0.04724550102237072557 ) ) ;
#79701 = CARTESIAN_POINT ( 'NONE',  ( 5.383996398402570271, 9.295429874862735531, 0.000000000000000000 ) ) ;
#79702 = CARTESIAN_POINT ( 'NONE',  ( 3.660338285565247762, 7.214219066560688454, 1.040834085586084257E-14 ) ) ;
#79703 = CARTESIAN_POINT ( 'NONE',  ( -5.956828388357799042, 8.042995434541133193, 1.599625672291263179 ) ) ;
#79704 = CARTESIAN_POINT ( 'NONE',  ( 6.540882763950133238, 6.595727744222092959, 0.000000000000000000 ) ) ;
#79705 = ORIENTED_EDGE ( 'NONE', *, *, #63015, .T. ) ;
#79707 = CARTESIAN_POINT ( 'NONE',  ( 5.660407656431548418, 2.011079132963066840, 0.09461074985974733675 ) ) ;
#79706 = CARTESIAN_POINT ( 'NONE',  ( 1.100829259350871281, -0.4471758257712907247, 1.786007343351428966 ) ) ;
#79708 = CARTESIAN_POINT ( 'NONE',  ( 6.539654151966706408, -1.780142272834178918, 1.453760081647121671 ) ) ;
#79709 = CARTESIAN_POINT ( 'NONE',  ( 5.928557400228100960, -1.247251702497784942, 1.514172074262534196 ) ) ;
#79710 = CARTESIAN_POINT ( 'NONE',  ( -6.718228810771495141, 7.796687353110217877, 1.199719254218450271 ) ) ;
#79711 = CARTESIAN_POINT ( 'NONE',  ( -5.298539104842322267, 5.076050465271134016, 0.7998128361456341429 ) ) ;
#79712 = CARTESIAN_POINT ( 'NONE',  ( -6.296835998904160014, 6.311006518335105397, 0.000000000000000000 ) ) ;
#79714 = CARTESIAN_POINT ( 'NONE',  ( 6.297684251969362101, -0.5920937881782936119, 1.667988322058571393 ) ) ;
#79713 = CARTESIAN_POINT ( 'NONE',  ( 1.540690653510309538, -1.764467595836321401, 1.121255944808132288 ) ) ;
#79715 = CARTESIAN_POINT ( 'NONE',  ( -2.788906526875773208E-15, 9.437499999999998224, -1.499999999999998446 ) ) ;
#79716 = CARTESIAN_POINT ( 'NONE',  ( -0.2102771530458277249, 5.719403664101017526, -2.797728457938574387 ) ) ;
#79717 = CARTESIAN_POINT ( 'NONE',  ( 1.153398195617076682, 0.7042877955899041753, 1.591771711926233346 ) ) ;
#79718 = CARTESIAN_POINT ( 'NONE',  ( 7.284808609244363353, 7.393364887073558656, 0.7998128361456341429 ) ) ;
#79720 = CARTESIAN_POINT ( 'NONE',  ( 0.3282377607281143916, 1.636164550367421144, 1.224999999999978995 ) ) ;
#79719 = CYLINDRICAL_SURFACE ( 'NONE', #2966, 6.200000000000000178 ) ;
#79721 = CARTESIAN_POINT ( 'NONE',  ( 2.050978400279603875, -1.384275906022333968, -1.028850351009907849 ) ) ;
#79722 = CARTESIAN_POINT ( 'NONE',  ( 1.646283778714407342, 0.6915601415973006150, 2.079641132013386517 ) ) ;
#79723 = CARTESIAN_POINT ( 'NONE',  ( -0.1229578505166153690, -0.3670672422863025530, -1.699768244568555353 ) ) ;
#79724 = CARTESIAN_POINT ( 'NONE',  ( 4.248781725523794073, 0.5872999373685274804, 2.127227798101683387 ) ) ;
#79725 = CARTESIAN_POINT ( 'NONE',  ( -10.90756946389101323, 4.636105284860334130, -4.485523696119589232 ) ) ;
#79726 = CARTESIAN_POINT ( 'NONE',  ( 1.833130710876787584, -2.060620742141227701, -0.6837463184809766670 ) ) ;
#79727 = CARTESIAN_POINT ( 'NONE',  ( 0.3811277156573149583, 1.704729334087114578, -0.6539457117896373406 ) ) ;
#79728 = CARTESIAN_POINT ( 'NONE',  ( 2.149754410345839251, 2.075462379332591478, -0.4182697058867020923 ) ) ;
#79729 = CARTESIAN_POINT ( 'NONE',  ( 3.511198595814909673, 7.040222761851984146, 0.7216878364870233931 ) ) ;
#79730 = ORIENTED_EDGE ( 'NONE', *, *, #54696, .F. ) ;
#79732 = CARTESIAN_POINT ( 'NONE',  ( 0.6823417656249882723, -0.5947916663252492686, 1.181850606188755259 ) ) ;
#79731 = CARTESIAN_POINT ( 'NONE',  ( 2.244040508683461166, 2.291928982054102004, 0.05232369179298743123 ) ) ;
#79733 =( NAMED_UNIT ( * ) PLANE_ANGLE_UNIT ( ) SI_UNIT ( $, .RADIAN. ) );
#79734 = CARTESIAN_POINT ( 'NONE',  ( 4.385172619016207918, 7.203452924572514959, 1.199719254218462483 ) ) ;
#79735 = CARTESIAN_POINT ( 'NONE',  ( 5.567086426426935297, -1.752359028239593997, 1.364940763008470226 ) ) ;
#79736 = CARTESIAN_POINT ( 'NONE',  ( -7.714226216495749355, 8.102278128774251797, 1.040834085586084257E-14 ) ) ;
#79737 = CARTESIAN_POINT ( 'NONE',  ( 5.992340707560163793, 6.093411701682730275, 0.7216878364870317197 ) ) ;
#79738 = CARTESIAN_POINT ( 'NONE',  ( -6.846504384776755714, 9.971043634672792422, -1.082531754730537088 ) ) ;
#79739 = CARTESIAN_POINT ( 'NONE',  ( 4.990809943606266508, 6.915973915664348937, -1.443375672974068769 ) ) ;
#79740 = VERTEX_POINT ( 'NONE', #181915 ) ;
#79741 = CARTESIAN_POINT ( 'NONE',  ( 3.551407868487792552, -1.352154898762620849, 1.496051317864899088 ) ) ;
#79743 = CARTESIAN_POINT ( 'NONE',  ( 2.307554651200398599, -1.654038752482372088, -1.231991790176652612 ) ) ;
#79742 = CARTESIAN_POINT ( 'NONE',  ( 5.126954644262057492, 9.133197518281081173, 0.7998128361456462443 ) ) ;
#79744 = CARTESIAN_POINT ( 'NONE',  ( -11.84668730067608422, 13.39999999999998259, 1.399999999999998357 ) ) ;
#79745 = CARTESIAN_POINT ( 'NONE',  ( 5.519577934094864524, 5.612131475965050242, 0.7216878364870328300 ) ) ;
#79746 = EDGE_LOOP ( 'NONE', ( #133195, #57979, #32776, #92293 ) ) ;
#79747 = FACE_OUTER_BOUND ( 'NONE', #6641, .T. ) ;
#79748 = CARTESIAN_POINT ( 'NONE',  ( -1.364683531250010295, 5.530208333674751842, 0.7879004041258379498 ) ) ;
#79749 = CARTESIAN_POINT ( 'NONE',  ( 5.332042502257137606, 2.158596015244533373, 0.3771327725019049670 ) ) ;
#79750 = CARTESIAN_POINT ( 'NONE',  ( 2.303361484738715159, 1.314996338066702242, -1.528741580717301263 ) ) ;
#79751 = CARTESIAN_POINT ( 'NONE',  ( 2.401689157922583640, -0.7064633820979376866, -1.700523668893457296 ) ) ;
#79752 = CARTESIAN_POINT ( 'NONE',  ( 8.633844893804129228, 8.967240552393299424, -0.7998128361456211532 ) ) ;
#79753 = CARTESIAN_POINT ( 'NONE',  ( 5.526323803393728085, 1.085782926936417425, -1.467421699745217412 ) ) ;
#79754 = CARTESIAN_POINT ( 'NONE',  ( 6.117814597332064785, 0.2004318333163370436, 2.006446488866588496 ) ) ;
#79755 = CARTESIAN_POINT ( 'NONE',  ( -7.365103760721662951, 9.615707025640515937, 1.599625672291295375 ) ) ;
#79757 = CARTESIAN_POINT ( 'NONE',  ( -5.173318132066234476, 8.193232366456022930, -1.199719254218453823 ) ) ;
#79756 = CARTESIAN_POINT ( 'NONE',  ( 5.612299388031473768, -1.011774156007083869, -2.023756622241212000 ) ) ;
#79758 = CARTESIAN_POINT ( 'NONE',  ( 0.8738170914556376845, 2.029154634757854847, -0.5636997952245518251 ) ) ;
#79759 = CARTESIAN_POINT ( 'NONE',  ( -7.099629715411508890, 8.311931418515415615, 1.199719254218452047 ) ) ;
#79760 = CARTESIAN_POINT ( 'NONE',  ( 10.37606763316019531, 10.99983374830873650, 0.7998128361456462443 ) ) ;
#79761 = DIRECTION ( 'NONE',  ( 0.000000000000000000, -0.000000000000000000, 1.000000000000000000 ) ) ;
#79763 = ADVANCED_FACE ( 'NONE', ( #199223 ), #186182, .T. ) ;
#79762 = CARTESIAN_POINT ( 'NONE',  ( -7.714753101375940503, 8.959299025482085455, 1.199719254218462483 ) ) ;
#79765 = UNCERTAINTY_MEASURE_WITH_UNIT (LENGTH_MEASURE( 1.000000000000000082E-05 ), #187316, 'distance_accuracy_value', 'NONE');
#79764 = B_SPLINE_CURVE_WITH_KNOTS ( 'NONE', 3,
 ( #208046, #76982, #59674, #28245, #13040, #60736 ),
 .UNSPECIFIED., .F., .F.,
 ( 4, 2, 4 ),
 ( 0.000000000000000000, 0.0001030949158708173365, 0.0002061898317416346730 ),
 .UNSPECIFIED. ) ;
#79766 = CARTESIAN_POINT ( 'NONE',  ( 6.999862025036645008, -6.532648833121171172, -6.392587740394702678 ) ) ;
#79767 = CARTESIAN_POINT ( 'NONE',  ( 3.051993976407674225, 6.574760382535328240, -0.7216878364870338292 ) ) ;
#79768 = CARTESIAN_POINT ( 'NONE',  ( 4.716373530444390560, 6.815548562371487762, -1.235710759775530798 ) ) ;
#79769 = CARTESIAN_POINT ( 'NONE',  ( -8.595506201384022660, 11.05117653974661529, 1.443375672974064550 ) ) ;
#79771 = CARTESIAN_POINT ( 'NONE',  ( 2.338390812749164827, -1.283062462031187456, -1.813217020134863411 ) ) ;
#79770 = CARTESIAN_POINT ( 'NONE',  ( 2.004293344102888508, -0.9022931611136343344, 1.919180038594799687 ) ) ;
#79772 = CARTESIAN_POINT ( 'NONE',  ( 3.486133158594716510E-16, 0.8750000006828204668, 1.224999999999968336 ) ) ;
#79774 = CARTESIAN_POINT ( 'NONE',  ( -6.123442655227560927, 7.173046514967467147, 1.199719254218452047 ) ) ;
#79773 = AXIS2_PLACEMENT_3D ( 'NONE', #92236, #191814, #77005 ) ;
#79775 = CARTESIAN_POINT ( 'NONE',  ( 6.582647274634798151, 7.638508894284114170, 1.199719254218462483 ) ) ;
#79776 = CARTESIAN_POINT ( 'NONE',  ( 3.332423539472821439, -1.170687260143790320, 1.574129132985650825 ) ) ;
#79777 = CARTESIAN_POINT ( 'NONE',  ( 6.959412922516382771, 7.013736585890911535, 0.7998128361456341429 ) ) ;
#79778 = CARTESIAN_POINT ( 'NONE',  ( -4.082753340799282427, 7.529786358835235838, 0.5248769202933333267 ) ) ;
#79779 = CARTESIAN_POINT ( 'NONE',  ( 4.383363735919856730, 4.008345868194933104, -0.7998128361456211532 ) ) ;
#79780 = CARTESIAN_POINT ( 'NONE',  ( -4.828112100242291760, 6.726159765073026264, -1.443375672974066548 ) ) ;
#79781 = CARTESIAN_POINT ( 'NONE',  ( -6.507550544879489252, 9.575597488125954015, 1.082531754730548412 ) ) ;
#79782 = CARTESIAN_POINT ( 'NONE',  ( 1.916421503514931679, -2.120014230100770725, 0.05699577502370903326 ) ) ;
#79783 = CARTESIAN_POINT ( 'NONE',  ( -4.098307573080856692, 8.003385611894792362, 0.7998128361456352531 ) ) ;
#79784 = CARTESIAN_POINT ( 'NONE',  ( 4.504844740329728481, 1.672958716126593082, -1.369014088531981255 ) ) ;
#79785 = CARTESIAN_POINT ( 'NONE',  ( 2.401689157922583640, -0.7064633820979376866, -1.700523668893457296 ) ) ;
#79786 = CARTESIAN_POINT ( 'NONE',  ( -4.191772670604852813, 7.388608026231708870, 0.8008250379338277547 ) ) ;
#79787 = CARTESIAN_POINT ( 'NONE',  ( -1.364683531250000748, 0.07187500034142035865, 0.000000000000000000 ) ) ;
#79788 = CARTESIAN_POINT ( 'NONE',  ( 6.316323101372843141, 1.626595589989995982, 0.6193309307870945579 ) ) ;
#79789 = CARTESIAN_POINT ( 'NONE',  ( 11.55950211276791251, 9.719999999999998863, -3.221476510067114329 ) ) ;
#79790 = CARTESIAN_POINT ( 'NONE',  ( 5.192409644353875642, 5.160158794608717514, 1.040834085586084257E-14 ) ) ;
#79791 = CARTESIAN_POINT ( 'NONE',  ( -11.33772463945036968, 19.00000000000000000, -3.680000000000002824 ) ) ;
#79792 = MECHANICAL_DESIGN_GEOMETRIC_PRESENTATION_REPRESENTATION (  '', ( #180141 ), #200820 ) ;
#79793 = CARTESIAN_POINT ( 'NONE',  ( 2.747127081003514881, -1.797865629537301668, 1.199965651887124896 ) ) ;
#79794 = CARTESIAN_POINT ( 'NONE',  ( 4.112657547701242144, 0.6818919214185631406, -1.897407125352356339 ) ) ;
#79795 = CARTESIAN_POINT ( 'NONE',  ( -10.11401940567025548, 10.90203684947788076, 1.040834085586084257E-14 ) ) ;
#79796 = CARTESIAN_POINT ( 'NONE',  ( 2.131903390035182255, -1.411712784473453830, -1.637176306262012826 ) ) ;
#79797 = EDGE_CURVE ( 'NONE', #60268, #120459, #190267, .T. ) ;
#79798 = CARTESIAN_POINT ( 'NONE',  ( 2.706272882855005335, -0.7510657119417161187, -1.822867458954416708 ) ) ;
#79799 = CARTESIAN_POINT ( 'NONE',  ( -6.569768201793956486, 6.780247303854220142, 0.5133454205821968985 ) ) ;
#79800 = CARTESIAN_POINT ( 'NONE',  ( 4.194824786304445219, 1.561856751782536135, 1.154042840620983057 ) ) ;
#79803 = VERTEX_POINT ( 'NONE', #154774 ) ;
#79802 = DIRECTION ( 'NONE',  ( -0.000000000000000000, 1.000000000000000000, -0.000000000000000000 ) ) ;
#79801 = CARTESIAN_POINT ( 'NONE',  ( -8.256552360598034213, 11.61609960646427986, 1.082531754730549967 ) ) ;
#79804 = CARTESIAN_POINT ( 'NONE',  ( -3.757017964318317471, 6.436919154129725484, 1.082531754730549967 ) ) ;
#79805 = CARTESIAN_POINT ( 'NONE',  ( 5.083381250481017410, 4.895309311841474553, 0.7998128361456352531 ) ) ;
#79807 = ORIENTED_EDGE ( 'NONE', *, *, #95387, .T. ) ;
#79806 = CARTESIAN_POINT ( 'NONE',  ( -3.657667580636712934, 7.489305620709952649, -0.7998128361456481317 ) ) ;
#79808 = CARTESIAN_POINT ( 'NONE',  ( -7.768458830506062007, 11.04665715469030296, 1.082531754730549967 ) ) ;
#79809 = CARTESIAN_POINT ( 'NONE',  ( 1.589210545419886378, -0.3244246349418925535, -2.182665228674217861 ) ) ;
#79810 = CARTESIAN_POINT ( 'NONE',  ( 3.285556943750000514, -2.063541666188710266, 1.896917185911906500 ) ) ;
#79811 = CARTESIAN_POINT ( 'NONE',  ( 4.768382384511014038, -0.8351381170168621360, -1.775225883709200980 ) ) ;
#79812 = CARTESIAN_POINT ( 'NONE',  ( -1.364683531250010295, 5.551041667008087543, -0.7879004041258300672 ) ) ;
#79813 = CARTESIAN_POINT ( 'NONE',  ( 1.499999999999989120, 4.285416667349482900, 0.8660254037844524744 ) ) ;
#79814 = CARTESIAN_POINT ( 'NONE',  ( 5.406339766261963220, 6.489514674222595758, -1.307707983115678152 ) ) ;
#79815 = CARTESIAN_POINT ( 'NONE',  ( 0.07499057489267992038, 0.7202342490539682673, -2.037914685249627045 ) ) ;
#79816 = CARTESIAN_POINT ( 'NONE',  ( 4.083814069670049562, -1.821384084514931612, -0.2681248149544179227 ) ) ;
#79817 = ORIENTED_EDGE ( 'NONE', *, *, #120271, .T. ) ;
#79818 = CARTESIAN_POINT ( 'NONE',  ( 1.360316468749967589, -0.2552083329918390930, 0.7853790794158500566 ) ) ;
#79819 = CARTESIAN_POINT ( 'NONE',  ( -6.995117189646935962, 10.24838825697502109, 1.199719254218453823 ) ) ;
#79820 = CARTESIAN_POINT ( 'NONE',  ( -3.741687207247254676, 7.309126141856352454, 1.040834085586084257E-14 ) ) ;
#79821 = CARTESIAN_POINT ( 'NONE',  ( 6.381110825713084189, -1.939362502171553482, -0.8581636585355473246 ) ) ;
#79822 = B_SPLINE_CURVE_WITH_KNOTS ( 'NONE', 3,
 ( #86590, #200319, #33574, #35698 ),
 .UNSPECIFIED., .F., .F.,
 ( 4, 4 ),
 ( 0.000000000000000000, 9.170750103614487298E-05 ),
 .UNSPECIFIED. ) ;
#79823 = SURFACE_SIDE_STYLE ('',( #194640 ) ) ;
#79824 = CARTESIAN_POINT ( 'NONE',  ( 7.149227073107712549, 7.235186428247455837, -0.7998128361456281477 ) ) ;
#79825 = ORIENTED_EDGE ( 'NONE', *, *, #137160, .F. ) ;
#79826 = CARTESIAN_POINT ( 'NONE',  ( 6.468051757712944827, 1.055310785928347928, 1.769903775486596054 ) ) ;
#79829 = CARTESIAN_POINT ( 'NONE',  ( 3.579498943475650563, -0.9044721095569520086, 1.603693017070174864 ) ) ;
#79828 = CARTESIAN_POINT ( 'NONE',  ( 1.433807476322545904, 1.104820645310525373, 1.497481488779895731 ) ) ;
#79827 = CARTESIAN_POINT ( 'NONE',  ( 0.4999999999999952260, 3.172938907704321743, -0.4000000000000062395 ) ) ;
#79830 = CARTESIAN_POINT ( 'NONE',  ( 6.435316467980822353, 10.65961964595298817, 1.040834085586084257E-14 ) ) ;
#79831 = FACE_BOUND ( 'NONE', #65514, .T. ) ;
#79832 = PRESENTATION_LAYER_ASSIGNMENT (  '', '', ( #121350 ) ) ;
#79833 = CARTESIAN_POINT ( 'NONE',  ( -5.610041701004606196, 9.767075427805856691, -0.7998128361456362523 ) ) ;
#79834 = CARTESIAN_POINT ( 'NONE',  ( -5.810221930991193690E-16, 2.125000000682803147, 1.224999999999976774 ) ) ;
#79835 = CARTESIAN_POINT ( 'NONE',  ( 3.123846942790895476, -2.126788776302591888, 0.5888931905130634359 ) ) ;
#79836 = CARTESIAN_POINT ( 'NONE',  ( 5.518922325393873507, 2.087324940739025525, 0.8731552084927389767 ) ) ;
#79837 = AXIS2_PLACEMENT_3D ( 'NONE', #30059, #13787, #129776 ) ;
#79838 = CARTESIAN_POINT ( 'NONE',  ( -5.694061328059534688, 8.626526735169329996, 1.082531754730548412 ) ) ;
#79839 = CARTESIAN_POINT ( 'NONE',  ( 6.328355405667826616, -0.8624701743435190249, -1.593140579868371987 ) ) ;
#79840 = CARTESIAN_POINT ( 'NONE',  ( 5.805858164762184082, -1.070174230454253639, -1.588719782701804695 ) ) ;
#79841 = CARTESIAN_POINT ( 'NONE',  ( -1.284279953904132077, 3.159610286488902187, -0.7749999999999935829 ) ) ;
#79842 = CARTESIAN_POINT ( 'NONE',  ( 6.684453402082996654, -1.835023323784425564, -0.3624468955198830722 ) ) ;
#79843 = CARTESIAN_POINT ( 'NONE',  ( 6.426204213344836269, 0.9576725794440078543, 1.595564698446788388 ) ) ;
#79844 = CARTESIAN_POINT ( 'NONE',  ( -0.001355188237250771121, 15.43765366524399596, 11.93721149935645265 ) ) ;
#79845 = CARTESIAN_POINT ( 'NONE',  ( 6.227411129102443432, -1.664988906758845921, 0.6005623136680103835 ) ) ;
#79846 = CARTESIAN_POINT ( 'NONE',  ( 0.8136858238772455287, -1.282993010278702606, -1.555696519147983459 ) ) ;
#79848 = CARTESIAN_POINT ( 'NONE',  ( 2.754625382576633807, 0.7102545713932090221, 1.982823988820613170 ) ) ;
#79847 = CARTESIAN_POINT ( 'NONE',  ( -7.804689982961090955, 12.25722208009664094, 0.7998128361456481317 ) ) ;
#79849 = CARTESIAN_POINT ( 'NONE',  ( 9.772729797352075920, 10.29593960653257234, -0.7998128361456281477 ) ) ;
#79851 = CARTESIAN_POINT ( 'NONE',  ( -8.533967624797991647, 12.04371376465130439, -1.199719254218446718 ) ) ;
#79850 = CARTESIAN_POINT ( 'NONE',  ( -0.7500000000000249800, -0.3083333333333132531, 1.299038105676659116 ) ) ;
#79852 = CARTESIAN_POINT ( 'NONE',  ( -0.9782388782689256379, 3.999999999999989786, 0.3999999999999559464 ) ) ;
#79853 = CARTESIAN_POINT ( 'NONE',  ( 3.427994306938833002, -1.989183439576122758, 0.3493681432537446563 ) ) ;
#79854 = CARTESIAN_POINT ( 'NONE',  ( 1.364683531249988535, 3.655208333674750509, -0.7879004041258239610 ) ) ;
#79855 = CARTESIAN_POINT ( 'NONE',  ( 3.277320446201373638, 4.846626492033466072, 1.599625672291267398 ) ) ;
#79856 = CARTESIAN_POINT ( 'NONE',  ( 3.638091081701349871, 0.9754702174074175725, -1.929073278114090684 ) ) ;
#79857 = CARTESIAN_POINT ( 'NONE',  ( 5.677832469072920496, 9.846164657218904992, 0.000000000000000000 ) ) ;
#79858 = CARTESIAN_POINT ( 'NONE',  ( 5.345657705538078730, 9.458627433094950021, 0.7998128361456331437 ) ) ;
#79859 = CARTESIAN_POINT ( 'NONE',  ( 8.554831740098649107, 11.96409221588171157, 1.082531754730546636 ) ) ;
#79861 = CARTESIAN_POINT ( 'NONE',  ( 9.245229451055090308, 14.18885291725855424, -7.650713753047223342 ) ) ;
#79860 = CARTESIAN_POINT ( 'NONE',  ( 0.8718042753090318175, -0.3185811321036461363, 2.147578089749022645 ) ) ;
#79862 = CARTESIAN_POINT ( 'NONE',  ( -7.551528373131759508, 7.912463978182924684, 1.040834085586084257E-14 ) ) ;
#79863 = CARTESIAN_POINT ( 'NONE',  ( -1.402160292154681736E-14, 1.196875000341419026, -1.575800808251659024 ) ) ;
#79864 = CARTESIAN_POINT ( 'NONE',  ( 2.419692422129790632, -1.264489869534379141, -1.789777738334753732 ) ) ;
#79865 = CARTESIAN_POINT ( 'NONE',  ( 0.2638905955352529031, 7.233311467405346029, 1.984662505942447419 ) ) ;
#79866 = CARTESIAN_POINT ( 'NONE',  ( 2.536292628665572479, 1.067014414141453704, -1.995120597088717806 ) ) ;
#79867 = CARTESIAN_POINT ( 'NONE',  ( -7.588813295347149435, 9.876701482703580837, -1.599625672291263179 ) ) ;
#79868 = CARTESIAN_POINT ( 'NONE',  ( -3.917943204224921150, 5.594019709727598766, -1.443375672974051449 ) ) ;
#79869 = CARTESIAN_POINT ( 'NONE',  ( -0.6823417656250212460, 3.863541667008085767, 1.181850606188767472 ) ) ;
#79870 = CARTESIAN_POINT ( 'NONE',  ( 4.943016831304842817, 7.975319854387232787, 1.017975537214605319 ) ) ;
#79871 = CARTESIAN_POINT ( 'NONE',  ( -0.7500000000000179856, 11.04166666666666430, 1.299038105676658228 ) ) ;
#79872 = CARTESIAN_POINT ( 'NONE',  ( 5.045042558060919724, 8.899983727797476263, -0.7216878364870458196 ) ) ;
#79873 = CARTESIAN_POINT ( 'NONE',  ( 3.286155083303475166, -1.742946490318267205, -0.3057894240724549628 ) ) ;
#79874 = CARTESIAN_POINT ( 'NONE',  ( 8.910733272679570049, 11.41894145625809820, -1.599625672291255185 ) ) ;
#79875 = CARTESIAN_POINT ( 'NONE',  ( 6.405322867445039314, 1.831175526881479776, 1.231239259074583092 ) ) ;
#79876 = CARTESIAN_POINT ( 'NONE',  ( 0.6823417656249934904, 9.692708333674735499, 1.181850606188764807 ) ) ;
#79877 = CARTESIAN_POINT ( 'NONE',  ( -4.797606254389363833, 6.690569611577942943, 1.599625672291263179 ) ) ;
#79878 = CARTESIAN_POINT ( 'NONE',  ( 5.747672784407955149, 1.986098415631059932, -0.3474865836668520336 ) ) ;
#79879 = ORIENTED_EDGE ( 'NONE', *, *, #98822, .T. ) ;
#79880 = ADVANCED_FACE ( 'NONE', ( #189393 ), #156916, .T. ) ;
#79881 = CARTESIAN_POINT ( 'NONE',  ( 4.188257260935820625, -1.850246793840780279, -0.2747695030091561463 ) ) ;
#79882 = CARTESIAN_POINT ( 'NONE',  ( 3.274343992483694787, -1.016290647400164282, -1.803532422793553636 ) ) ;
#79883 =( GEOMETRIC_REPRESENTATION_CONTEXT ( 3 ) GLOBAL_UNCERTAINTY_ASSIGNED_CONTEXT ( ( #155951 ) ) GLOBAL_UNIT_ASSIGNED_CONTEXT ( ( #39291, #188739, #108627 ) ) REPRESENTATION_CONTEXT ( 'NONE', 'WORKASPACE' ) );
#79884 = CARTESIAN_POINT ( 'NONE',  ( -7.444835747235459600, 8.818634805597074688, 1.082531754730549078 ) ) ;
#79885 = CARTESIAN_POINT ( 'NONE',  ( -11.01135777277261951, 11.00625186781170939, 1.399999999999998579 ) ) ;
#79886 = CARTESIAN_POINT ( 'NONE',  ( -10.30104275384242740, 4.689840931292195592, -5.506867539468097483 ) ) ;
#79887 = PRESENTATION_STYLE_ASSIGNMENT (( #193641 ) ) ;
#79888 = CARTESIAN_POINT ( 'NONE',  ( 1.364683531249988535, 4.967708333674756283, -0.7879004041258300672 ) ) ;
#79889 = EDGE_CURVE ( 'NONE', #45106, #58157, #211917, .T. ) ;
#79890 = CARTESIAN_POINT ( 'NONE',  ( 2.963279974173158138, 1.655882904019840840, 1.051842618152734499 ) ) ;
#79891 = CARTESIAN_POINT ( 'NONE',  ( 1.071638489536786309, 1.528508772698906837, -1.314793605459969150 ) ) ;
#79892 = CARTESIAN_POINT ( 'NONE',  ( -3.122120512896910505, 6.864500708346841229, 0.7998128361456352531 ) ) ;
#79894 = FILL_AREA_STYLE_COLOUR ( '', #160953 ) ;
#79893 = CARTESIAN_POINT ( 'NONE',  ( 7.747594715205354809, 11.12627870345989756, -1.199719254218446718 ) ) ;
#79895 = CARTESIAN_POINT ( 'NONE',  ( 1.405301488743180061, -0.4598193086536165319, 1.813012767170335993 ) ) ;
#79896 = CARTESIAN_POINT ( 'NONE',  ( -1.364683531249997417, 4.259375000341424133, 1.214306433183764966E-14 ) ) ;
#79897 = CARTESIAN_POINT ( 'NONE',  ( 1.424089148264463089, -1.997494042244374768, 0.2507359931839692191 ) ) ;
#79899 = CARTESIAN_POINT ( 'NONE',  ( 2.355205625472241771, 0.1007552864207492405, -2.114937101796029673 ) ) ;
#79898 = CARTESIAN_POINT ( 'NONE',  ( -6.344852701515500293, 9.385783337534627790, 1.082531754730548412 ) ) ;
#79900 = CARTESIAN_POINT ( 'NONE',  ( 7.695629581373169437, 14.38868833749761400, -9.210593468082514335 ) ) ;
#79901 = CARTESIAN_POINT ( 'NONE',  ( 3.402844027952243167, 0.5003511028610057032, 2.008882729757965890 ) ) ;
#79902 = B_SPLINE_CURVE_WITH_KNOTS ( 'NONE', 3,
 ( #27960, #208823, #26883, #75650, #172091, #73505, #174243, #207765, #108218, #125548, #142816 ),
 .UNSPECIFIED., .F., .F.,
 ( 4, 1, 1, 1, 1, 1, 1, 1, 4 ),
 ( 0.000000000000000000, 0.2255234228546724728, 0.3973271701647976828, 0.5245128843546777997, 0.6161923999872991331, 0.6815320185768301009, 0.7298552812456317040, 0.7704940248801678271, 1.000000000000000000 ),
 .UNSPECIFIED. ) ;
#79903 = CARTESIAN_POINT ( 'NONE',  ( 6.668631453075247073, 8.873432343378178544, -1.599625672291281386 ) ) ;
#79905 = CARTESIAN_POINT ( 'NONE',  ( 3.297657676621871925, 4.870353260857385180, 1.599625672291267398 ) ) ;
#79904 = CARTESIAN_POINT ( 'NONE',  ( 6.035123006257053113, -1.513425687198214353, -1.442577094899047063 ) ) ;
#79907 = ORIENTED_EDGE ( 'NONE', *, *, #184582, .F. ) ;
#79906 = CARTESIAN_POINT ( 'NONE',  ( 4.436427218767265757, 1.790408935156896586, 0.3557191534368231434 ) ) ;
#79908 = CARTESIAN_POINT ( 'NONE',  ( 8.866142388332804103, 12.43125098877526113, -1.199719254218446718 ) ) ;
#79909 = CARTESIAN_POINT ( 'NONE',  ( 4.952636518945733535, 6.537114055553957748, -2.442608363190508669 ) ) ;
#79910 = CARTESIAN_POINT ( 'NONE',  ( 9.691970092379245116, 13.38142374607198803, 8.152522038325429321 ) ) ;
#79911 = CIRCLE ( 'NONE', #65973, 0.08000000000000020983 ) ;
#79912 = CARTESIAN_POINT ( 'NONE',  ( -10.41980074470002648, 5.020554563858687480, 5.279403930596816785 ) ) ;
#79913 = CARTESIAN_POINT ( 'NONE',  ( -0.6823417656250003738, 11.21354166700806765, 1.181850606188754593 ) ) ;
#79914 = CARTESIAN_POINT ( 'NONE',  ( 5.145129553670328981, 0.1446803459003667691, 1.906877450533929874 ) ) ;
#79915 = CARTESIAN_POINT ( 'NONE',  ( -7.974166903131914452, 12.45494515362926435, -0.7998128361456281477 ) ) ;
#79916 = CARTESIAN_POINT ( 'NONE',  ( 7.416473721875251890, 8.611306416064660851, 1.199719254218462483 ) ) ;
#79917 = CARTESIAN_POINT ( 'NONE',  ( 1.360316468749987129, 1.796875000341410900, -3.295974604355933479E-14 ) ) ;
#79918 = CARTESIAN_POINT ( 'NONE',  ( 4.839897649954202130, 4.748894801142428790, -0.7216878364870197293 ) ) ;
#79919 = ADVANCED_FACE ( 'NONE', ( #6358 ), #34021, .T. ) ;
#79920 = CARTESIAN_POINT ( 'NONE',  ( 1.499999999999993117, 9.854166666666671404, 0.8660254037844408170 ) ) ;
#79921 = CARTESIAN_POINT ( 'NONE',  ( 0.7140992756325338364, 1.701125707204935944, 0.7050099338341904165 ) ) ;
#79922 = ORIENTED_EDGE ( 'NONE', *, *, #61688, .F. ) ;
#79923 = VECTOR ( 'NONE', #204018, 1000.000000000000000 ) ;
#79924 = SURFACE_STYLE_USAGE ( .BOTH. , #96210 ) ;
#79925 = CARTESIAN_POINT ( 'NONE',  ( 4.235518730357812345, -1.288231833625707701, -1.356488508162751128 ) ) ;
#79926 = CARTESIAN_POINT ( 'NONE',  ( 0.07700591528349547132, 1.369316849116916091, -2.165014180211277228 ) ) ;
#79927 = CARTESIAN_POINT ( 'NONE',  ( 7.126746022638799971, 8.343567110280638133, 1.199719254218452047 ) ) ;
#79928 = LINE ( 'NONE', #30125, #91549 ) ;
#79929 = CARTESIAN_POINT ( 'NONE',  ( -6.401963353335964335, 6.822014978843597532, 0.5293317295896986518 ) ) ;
#79930 = CARTESIAN_POINT ( 'NONE',  ( -4.934804725694212912, 8.701096580044490381, -0.7216878364870207285 ) ) ;
#79931 = CARTESIAN_POINT ( 'NONE',  ( 5.183294799126148433, 4.941598775268944976, 1.040834085586084257E-14 ) ) ;
#79932 = CARTESIAN_POINT ( 'NONE',  ( 0.7253723109368491739, 0.1984653623241394993, -1.959446941136263831 ) ) ;
#79933 = EDGE_CURVE ( 'NONE', #53115, #171829, #4403, .T. ) ;
#79934 = CARTESIAN_POINT ( 'NONE',  ( 2.284780001213771783, 1.617805504991537635, -1.203372706716873575 ) ) ;
#79935 = CARTESIAN_POINT ( 'NONE',  ( -7.700141177557535244, 11.07091624287075859, -1.199719254218446718 ) ) ;
#79936 = CARTESIAN_POINT ( 'NONE',  ( 4.355912491740495440, 8.303924683664389406, 0.000000000000000000 ) ) ;
#79937 = CARTESIAN_POINT ( 'NONE',  ( -6.966220764712148572, 6.002124920821316323, 2.500000000000000444 ) ) ;
#79938 = CARTESIAN_POINT ( 'NONE',  ( 2.220887445055406584, 0.001640320231081903845, 2.191629467496846839 ) ) ;
#79939 = FACE_OUTER_BOUND ( 'NONE', #153731, .T. ) ;
#79940 = CARTESIAN_POINT ( 'NONE',  ( -9.484092147959342967, 11.02352791316275216, 1.199719254218462483 ) ) ;
#79941 = ADVANCED_FACE ( 'NONE', ( #21525 ), #66550, .F. ) ;
#79942 = FACE_OUTER_BOUND ( 'NONE', #18160, .T. ) ;
#79943 = CARTESIAN_POINT ( 'NONE',  ( 10.25877837909742318, 3.235871879154605057, -5.476282928277127482 ) ) ;
#79944 = CARTESIAN_POINT ( 'NONE',  ( 5.248414862265931902, 5.295774558831261913, 0.000000000000000000 ) ) ;
#79945 = CARTESIAN_POINT ( 'NONE',  ( 9.097684769969825780, 10.57271930550834860, -1.199719254218446718 ) ) ;
#79946 = CARTESIAN_POINT ( 'NONE',  ( 6.634017235788401301, 6.634108284708264414, 0.7998128361456341429 ) ) ;
#79947 = DIRECTION ( 'NONE',  ( 1.000000000000000000, 0.000000000000000000, 0.000000000000000000 ) ) ;
#79948 = CARTESIAN_POINT ( 'NONE',  ( 5.207740401424913124, 9.089797878388800711, -0.7216878364870458196 ) ) ;
#79949 = ORIENTED_EDGE ( 'NONE', *, *, #153604, .T. ) ;
#79951 = CARTESIAN_POINT ( 'NONE',  ( 1.787745399045566730, 1.925802014453177557, -0.5863169366013292194 ) ) ;
#79950 = CARTESIAN_POINT ( 'NONE',  ( 5.319803798718575116, 1.092037692397327620, -1.482314076171886708 ) ) ;
#79952 = CARTESIAN_POINT ( 'NONE',  ( 4.077728334586081083, 1.628699396557086398, -1.621930329367648138 ) ) ;
#79954 = CARTESIAN_POINT ( 'NONE',  ( 1.902945097309636013, -1.575467964945817867, 0.9901336090045903537 ) ) ;
#79953 = CARTESIAN_POINT ( 'NONE',  ( -0.1290005225502918740, 6.946858002156244716, -2.769053915224591211 ) ) ;
#79955 = CARTESIAN_POINT ( 'NONE',  ( 0.000000000000000000, -1.596874999522041705, -3.793834371823813001 ) ) ;
#79956 = CARTESIAN_POINT ( 'NONE',  ( 6.983263157960363898, -0.009046620988246927009, 2.153544821522495933 ) ) ;
#79957 = CARTESIAN_POINT ( 'NONE',  ( 5.713130151434068438, 1.559639147136464343, -1.106415316399149473 ) ) ;
#79958 = CARTESIAN_POINT ( 'NONE',  ( -7.323375529675950624, 11.69568855126397011, -0.7998128361456291469 ) ) ;
#79959 = CARTESIAN_POINT ( 'NONE',  ( -4.665414256878293031, 7.496714828783040296, -1.082531754730549967 ) ) ;
#79961 = CARTESIAN_POINT ( 'NONE',  ( 3.959713429720784106, 1.856571849420919795, -0.2284545790810637578 ) ) ;
#79960 = CARTESIAN_POINT ( 'NONE',  ( 5.091392180243133225, -0.7513228403347729234, 1.951278057808901512 ) ) ;
#79962 = CARTESIAN_POINT ( 'NONE',  ( 6.155038550924139429, 9.164333495178082600, 1.082531754730558626 ) ) ;
#79963 = CARTESIAN_POINT ( 'NONE',  ( 5.548353751603532835, -1.447698842669535413, 1.137588655622793876 ) ) ;
#79964 = CARTESIAN_POINT ( 'NONE',  ( 4.196412238629597447, 4.854568018944682706, -1.199719254218452047 ) ) ;
#79965 = CARTESIAN_POINT ( 'NONE',  ( 0.9782388782688926643, 3.999999999999968914, 0.3999999999999576672 ) ) ;
#79966 = CARTESIAN_POINT ( 'NONE',  ( 5.215364217145412873, -0.2476331258763775356, 1.706884187403294728 ) ) ;
#79967 = CARTESIAN_POINT ( 'NONE',  ( -5.713871673155502151, 8.753601821068331290, 1.199719254218452047 ) ) ;
#79968 = PRODUCT_DEFINITION_FORMATION_WITH_SPECIFIED_SOURCE ( 'ANY', '', #14337, .NOT_KNOWN. ) ;
#79969 = CARTESIAN_POINT ( 'NONE',  ( 0.8790820841908916217, -0.4200629052855206491, -1.682323782590444461 ) ) ;
#79970 = CARTESIAN_POINT ( 'NONE',  ( 0.000000000000000000, 3.447199233515649386, 12.00000000000000178 ) ) ;
#79971 =( GEOMETRIC_REPRESENTATION_CONTEXT ( 3 ) GLOBAL_UNCERTAINTY_ASSIGNED_CONTEXT ( ( #13177 ) ) GLOBAL_UNIT_ASSIGNED_CONTEXT ( ( #106243, #158156, #24926 ) ) REPRESENTATION_CONTEXT ( 'NONE', 'WORKASPACE' ) );
#79972 =( NAMED_UNIT ( * ) PLANE_ANGLE_UNIT ( ) SI_UNIT ( $, .RADIAN. ) );
#79973 = CARTESIAN_POINT ( 'NONE',  ( 4.469693783504245843, -0.3772167039018388124, 2.137918043537301305 ) ) ;
#79974 = CARTESIAN_POINT ( 'NONE',  ( 3.088313589057069208, -1.798746773638896457, -0.3115406389907551810 ) ) ;
#79975 = CARTESIAN_POINT ( 'NONE',  ( 0.8835585337332928502, -1.864609544942645414, 0.6100022000963196689 ) ) ;
#79976 = CARTESIAN_POINT ( 'NONE',  ( 0.1580148589572556717, 1.223040929162301449, 1.728066982087714809 ) ) ;
#79977 = CIRCLE ( 'NONE', #201022, 0.7500000000000011102 ) ;
#79979 = CARTESIAN_POINT ( 'NONE',  ( -1.201851678989727383E-14, 4.259375000341417028, -1.575800808251660134 ) ) ;
#79978 = CARTESIAN_POINT ( 'NONE',  ( 6.567932727852480390, -1.414834124515697011, 1.804577934655810401 ) ) ;
#79980 = CARTESIAN_POINT ( 'NONE',  ( 5.736990052184824940, 5.898621588824067175, 2.499999999981530330 ) ) ;
#79981 = CARTESIAN_POINT ( 'NONE',  ( 7.377608144130607393, 11.75895993479440982, -0.7998128361456291469 ) ) ;
#79982 = CARTESIAN_POINT ( 'NONE',  ( 2.912858673564645784, -0.6176872867308530468, -2.028511212565413224 ) ) ;
#79983 = CARTESIAN_POINT ( 'NONE',  ( -4.772106882330247046, 4.669805572247793357, -0.7216878364870207285 ) ) ;
#79984 = CARTESIAN_POINT ( 'NONE',  ( 4.651856102820254968, 7.480896982382013505, -1.082531754730548412 ) ) ;
#79985 = CARTESIAN_POINT ( 'NONE',  ( -4.785665035499573783, 5.645992631913323123, 1.082531754730558626 ) ) ;
#79986 = CARTESIAN_POINT ( 'NONE',  ( 0.3739936534635743270, -2.030981289472892026, 0.4004457479018645460 ) ) ;
#79988 = CARTESIAN_POINT ( 'NONE',  ( -1.500000000000008216, 13.53125000068279604, 3.469446951953614189E-15 ) ) ;
#79987 = CARTESIAN_POINT ( 'NONE',  ( 6.883263157960341161, 7.051904271082326758, 2.751962465287846271 ) ) ;
#79990 = VERTEX_POINT ( 'NONE', #112613 ) ;
#79989 = CARTESIAN_POINT ( 'NONE',  ( 2.684490341743519082, 1.190536367853095578, 1.875150363231482098 ) ) ;
#79991 = CARTESIAN_POINT ( 'NONE',  ( 1.178858319146030009, 1.745148694481736484, 1.496268366688303653 ) ) ;
#79993 = CARTESIAN_POINT ( 'NONE',  ( 5.243062877513432696, -0.2472539590166565604, -2.047610945800168114 ) ) ;
#79992 = CARTESIAN_POINT ( 'NONE',  ( 4.681643115420508039, 4.356338477612361260, 0.7998128361456341429 ) ) ;
#79995 = CARTESIAN_POINT ( 'NONE',  ( -1.737499999999997824, -1.341666666666668117, 3.009438278150925683 ) ) ;
#79994 = CARTESIAN_POINT ( 'NONE',  ( 4.355912491740495440, 8.303924683664389406, 0.000000000000000000 ) ) ;
#79996 = CARTESIAN_POINT ( 'NONE',  ( 5.143339171537801846, 7.093924681584509173, 1.599625672291269396 ) ) ;
#79997 = CARTESIAN_POINT ( 'NONE',  ( 0.2329586101569866563, 0.008238550247445517935, -1.845944905557160398 ) ) ;
#79998 = CARTESIAN_POINT ( 'NONE',  ( 5.073706409418358376, -1.018251046719556685, 1.533866337327425278 ) ) ;
#79999 = CARTESIAN_POINT ( 'NONE',  ( 3.845709127770629010, 7.638411082374393146, 0.7998128361456321445 ) ) ;
#80000 = CARTESIAN_POINT ( 'NONE',  ( 1.676317214473854067, -1.636236659294947104, -0.5456935059391133658 ) ) ;
#80001 = CARTESIAN_POINT ( 'NONE',  ( 0.7082206942033396624, 1.197301205363930254, -1.622488844446705381 ) ) ;
#80002 = CARTESIAN_POINT ( 'NONE',  ( 1.758794133653733827, 2.198278648980501515, -0.6719540409268388581 ) ) ;
#80003 = CARTESIAN_POINT ( 'NONE',  ( 0.6823417656249899377, 3.988541667008085767, -1.181850606188754593 ) ) ;
#80004 = CARTESIAN_POINT ( 'NONE',  ( 2.003560550249494199, 1.880309486893988913, 1.257863985149072938 ) ) ;
#80005 = CARTESIAN_POINT ( 'NONE',  ( 4.477239461409222798, 0.0005595100435150377523, -2.106257355078521964 ) ) ;
#80006 = CARTESIAN_POINT ( 'NONE',  ( -6.455090533882193782, 9.584670485287619002, -1.082531754730549967 ) ) ;
#80007 = CARTESIAN_POINT ( 'NONE',  ( 2.336827959689928846, -1.583187595272864900, 0.7909824253358921364 ) ) ;
#80008 = CARTESIAN_POINT ( 'NONE',  ( 5.099838337034727331, 9.101561826515851550, -0.7998128361456281477 ) ) ;
#80010 = CARTESIAN_POINT ( 'NONE',  ( 5.284854174503876401, 2.022835781599085614, -1.078525118384612735 ) ) ;
#80009 = CARTESIAN_POINT ( 'NONE',  ( 5.682275777458851707, 6.762314840857718501, 1.082531754730549078 ) ) ;
#80012 = EDGE_CURVE ( 'NONE', #6228, #212297, #81109, .T. ) ;
#80011 = CARTESIAN_POINT ( 'NONE',  ( -3.924195396151603177, 6.665646164563756138, 1.199719254218464037 ) ) ;
#80013 = CARTESIAN_POINT ( 'NONE',  ( 5.951666246274797345, 7.966696592119163256, 1.443375672974062551 ) ) ;
#80014 = CARTESIAN_POINT ( 'NONE',  ( -1.500000000000013101, 1.879166666666692187, -0.8660254037844313801 ) ) ;
#80015 = CARTESIAN_POINT ( 'NONE',  ( 6.468989383178811892, -1.718075365336281246, 1.407709432230166202 ) ) ;
#80016 = CARTESIAN_POINT ( 'NONE',  ( 5.103566685217446164, -2.181124530238859549, 0.2125310249164805709 ) ) ;
#80017 = CARTESIAN_POINT ( 'NONE',  ( -5.220052836461385404, 6.048815383081766583, -1.199719254218446718 ) ) ;
#80018 = DIRECTION ( 'NONE',  ( 3.451266460341927524E-31, -0.6000000000000035305, 0.7999999999999974909 ) ) ;
#80019 = CARTESIAN_POINT ( 'NONE',  ( 6.633471380297788045, -0.1541069161683609745, 2.086224335282916620 ) ) ;
#80020 = CARTESIAN_POINT ( 'NONE',  ( -1.201851678989727383E-14, 3.571875000341422357, 1.575800808251672791 ) ) ;
#80021 = CARTESIAN_POINT ( 'NONE',  ( 2.877471820773948252, 1.829258416151048561, -0.6045268202574998195 ) ) ;
#80022 = CARTESIAN_POINT ( 'NONE',  ( 0.6823417656249969321, 9.276041667008065872, -1.181850606188757036 ) ) ;
#80023 = CARTESIAN_POINT ( 'NONE',  ( -3.456965981804629884, 6.976951378839947537, 1.040834085586084257E-14 ) ) ;
#80024 = CARTESIAN_POINT ( 'NONE',  ( 5.484674493353773883, -1.343714522216314489, 1.640574901390474460 ) ) ;
#80025 = CARTESIAN_POINT ( 'NONE',  ( -5.587368702607575344, 8.572328348800551723, 1.082531754730550855 ) ) ;
#80026 = ORIENTED_EDGE ( 'NONE', *, *, #55423, .F. ) ;
#80028 = CARTESIAN_POINT ( 'NONE',  ( 3.903157637975605443, 4.019672535764859056, -0.7873708795828464613 ) ) ;
#80027 = CARTESIAN_POINT ( 'NONE',  ( -4.014622883422329203, 6.737458226417744278, -1.082531754730546636 ) ) ;
#80029 = CARTESIAN_POINT ( 'NONE',  ( 4.059776932288224671, 6.823824623389866950, 1.199719254218462483 ) ) ;
#80030 = CARTESIAN_POINT ( 'NONE',  ( 5.706567001488551227, 1.626822141722890303, 0.8623401093873286349 ) ) ;
#80031 = CARTESIAN_POINT ( 'NONE',  ( 0.7500000000000006661, 11.11458333401613174, 1.299038105676657340 ) ) ;
#80032 = CARTESIAN_POINT ( 'NONE',  ( 0.5137346906103140709, 6.676840427790344812, -3.535787237050524112 ) ) ;
#80033 = CARTESIAN_POINT ( 'NONE',  ( 1.364683531249988535, 3.467708333674749621, -0.7879004041258239610 ) ) ;
#80034 = CARTESIAN_POINT ( 'NONE',  ( 1.944474315927123387, -1.398120440366573680, -1.036317219087657504 ) ) ;
#80035 = CARTESIAN_POINT ( 'NONE',  ( 4.744990575102895569, 5.598539094783909320, -1.082531754730548412 ) ) ;
#80036 = CARTESIAN_POINT ( 'NONE',  ( -2.788906526875773208E-15, 10.96875000068279427, -1.499999999999998446 ) ) ;
#80037 = CARTESIAN_POINT ( 'NONE',  ( -0.6823417656250246877, 0.1135416670080893753, 1.181850606188755259 ) ) ;
#80038 = CARTESIAN_POINT ( 'NONE',  ( 6.684453901184132185, -2.118919246787358102, -0.4271090584619871566 ) ) ;
#80039 = CARTESIAN_POINT ( 'NONE',  ( -8.462260433223891098, 13.02438760540324481, -0.7998128361456281477 ) ) ;
#80040 = AXIS2_PLACEMENT_3D ( 'NONE', #99293, #198882, #50528 ) ;
#80041 = CARTESIAN_POINT ( 'NONE',  ( -6.846504384776774366, 7.089935991768773427, -0.7216878364870267237 ) ) ;
#80042 = CARTESIAN_POINT ( 'NONE',  ( 5.506754051192107369, 1.639644015412666800, -1.408845030788405506 ) ) ;
#80044 = VERTEX_POINT ( 'NONE', #50742 ) ;
#80043 = CARTESIAN_POINT ( 'NONE',  ( -5.144392941742557568, 4.966489618313220333, -0.7998128361456362523 ) ) ;
#80045 = CARTESIAN_POINT ( 'NONE',  ( -1.364683531250010295, 3.780208333674750953, 0.7879004041258379498 ) ) ;
#80046 = CARTESIAN_POINT ( 'NONE',  ( 5.975845355540164938, 1.172130763738386650, 1.584922449839619052 ) ) ;
#80047 = CARTESIAN_POINT ( 'NONE',  ( 5.219963594993116018, -1.465640877661518626, -0.9259742478883812300 ) ) ;
#80049 = CARTESIAN_POINT ( 'NONE',  ( 1.435386855117400717, -1.590506285900999295, -1.507976327226906443 ) ) ;
#80048 = CARTESIAN_POINT ( 'NONE',  ( -0.6801582343749917881, 0.4322916670080681478, 1.178068619123841643 ) ) ;
#80050 = CARTESIAN_POINT ( 'NONE',  ( 3.083396755883772933, -0.1683641986609325514, -2.301487591144059763 ) ) ;
#80051 = CARTESIAN_POINT ( 'NONE',  ( 6.151650338133601181, 0.6026783403972060249, -1.970659962842249424 ) ) ;
#80052 = CARTESIAN_POINT ( 'NONE',  ( 1.552571996792909248, -1.665377644223103637, -0.9986158231547156428 ) ) ;
#80053 = CARTESIAN_POINT ( 'NONE',  ( -6.548225005276122168, 6.741943382351338165, 0.7216878364870317197 ) ) ;
#80054 = PRODUCT ( 'screw coil', 'screw coil', '', ( #119792 ) ) ;
#80056 = ADVANCED_FACE ( 'NONE', ( #115802 ), #11875, .F. ) ;
#80055 = CARTESIAN_POINT ( 'NONE',  ( -3.169574050544739841, 6.919863168935977527, -0.7998128361456481317 ) ) ;
#80057 = DIRECTION ( 'NONE',  ( -0.9980789807931677027, -0.06195440338564740107, 0.000000000000000000 ) ) ;
#80058 = CARTESIAN_POINT ( 'NONE',  ( 4.060867369437678676, 0.5686956411946364476, 2.042824496258560441 ) ) ;
#80059 =( NAMED_UNIT ( * ) PLANE_ANGLE_UNIT ( ) SI_UNIT ( $, .RADIAN. ) );
#80060 = CARTESIAN_POINT ( 'NONE',  ( 2.320935597664942396, 0.9480396085976348086, -1.779626998253575509 ) ) ;
#80061 = CARTESIAN_POINT ( 'NONE',  ( -6.710922848640111127, 6.931757532942661726, 0.7216878364870317197 ) ) ;
#80062 = CARTESIAN_POINT ( 'NONE',  ( 4.999154358079874960, 1.837129776665728187, -1.222328095618854693 ) ) ;
#80063 = CARTESIAN_POINT ( 'NONE',  ( -11.84668730067608422, 10.19999999999999929, -1.320000000000001616 ) ) ;
#80064 = LINE ( 'NONE', #211116, #131105 ) ;
#80065 = CARTESIAN_POINT ( 'NONE',  ( -5.413448473606448985, 9.537716662508005427, 0.000000000000000000 ) ) ;
#80067 = CARTESIAN_POINT ( 'NONE',  ( 1.173530994449854870, -3.042800438942089514, 3.270848514539542506 ) ) ;
#80066 = CARTESIAN_POINT ( 'NONE',  ( -4.845071979149651042, 8.194897641035423064, 0.9605101338234197650 ) ) ;
#80068 = ORIENTED_EDGE ( 'NONE', *, *, #117177, .F. ) ;
#80069 = CARTESIAN_POINT ( 'NONE',  ( 4.381749043697905854, 1.344797980244310631, 1.561758987969330992 ) ) ;
#80070 = CARTESIAN_POINT ( 'NONE',  ( 4.086551013974742297, 7.685627118797787816, -0.6322510406990735632 ) ) ;
#80071 = CARTESIAN_POINT ( 'NONE',  ( 0.2132228467416317219, 6.504871514021060896, -3.125808945088798474 ) ) ;
#80072 = CARTESIAN_POINT ( 'NONE',  ( -4.985647801523292344, 6.839675073242382553, -1.599625672291256295 ) ) ;
#80073 = CARTESIAN_POINT ( 'NONE',  ( -5.061990249855848667, 6.999017606288844284, -1.599625672291271394 ) ) ;
#80074 = CARTESIAN_POINT ( 'NONE',  ( 3.932289538495234549, -1.040048408385336964, -1.731156807262229425 ) ) ;
#80075 = CARTESIAN_POINT ( 'NONE',  ( 0.7499999999999885647, 0.2333333333333562076, 1.299038105676657340 ) ) ;
#80077 = CARTESIAN_POINT ( 'NONE',  ( 9.897088948295943212, 11.60932053017587506, 1.082531754730548412 ) ) ;
#80076 = CARTESIAN_POINT ( 'NONE',  ( -5.492988512192097161, 6.437516681426083132, 1.199719254218452935 ) ) ;
#80078 = CARTESIAN_POINT ( 'NONE',  ( 8.132193210098487057, 8.381980254736715708, 1.040834085586084257E-14 ) ) ;
#80079 = AXIS2_PLACEMENT_3D ( 'NONE', #190106, #86216, #154423 ) ;
#80080 = CARTESIAN_POINT ( 'NONE',  ( 3.010674446437047624, 1.493694004556917365, -1.420165857245965668 ) ) ;
#80081 = CARTESIAN_POINT ( 'NONE',  ( 3.059220373557011818, -1.198860207862334049, 1.621182619130703273 ) ) ;
#80082 = DIRECTION ( 'NONE',  ( 0.000000000000000000, -1.000000000000000000, 0.000000000000000000 ) ) ;
#80083 = CARTESIAN_POINT ( 'NONE',  ( 4.143988507271280319, 7.986403691791820414, -0.7998128361456221525 ) ) ;
#80084 = CARTESIAN_POINT ( 'NONE',  ( 0.8316833483592298570, 1.813467871694788069, 0.3170515863319539052 ) ) ;
#80085 = CARTESIAN_POINT ( 'NONE',  ( 0.1183777584694784279, -2.261842813846013822, 0.4569907027171058456 ) ) ;
#80086 = CARTESIAN_POINT ( 'NONE',  ( 5.143339171537801846, 7.093924681584509173, 1.599625672291269396 ) ) ;
#80087 = CARTESIAN_POINT ( 'NONE',  ( 2.970174626046932609, 1.153603175066318931, 1.827835936144058371 ) ) ;
#80088 = CARTESIAN_POINT ( 'NONE',  ( -3.714570900464290393, 5.356752022006865843, 1.443375672974064550 ) ) ;
#80089 = CARTESIAN_POINT ( 'NONE',  ( 4.083301318022297899, 1.702923931485133879, 1.258099284506300153 ) ) ;
#80090 = PRESENTATION_LAYER_ASSIGNMENT (  '', '', ( #176897 ) ) ;
#80091 = EDGE_CURVE ( 'NONE', #71069, #148246, #97383, .T. ) ;
#80092 = FACE_OUTER_BOUND ( 'NONE', #52715, .T. ) ;
#80093 = CARTESIAN_POINT ( 'NONE',  ( 1.094370286708164386, -0.4508366001288487412, -1.815394955969009239 ) ) ;
#80094 = CARTESIAN_POINT ( 'NONE',  ( 4.575049868665863606, 0.0009985144121069796600, -1.971640593447765655 ) ) ;
#80095 = CARTESIAN_POINT ( 'NONE',  ( 5.137907791644652278, 2.014008302827663854, -0.1037760698975112861 ) ) ;
#80097 = CARTESIAN_POINT ( 'NONE',  ( 8.039621902779343188, 12.32338328664385507, -0.7216878364870328300 ) ) ;
#80096 = CARTESIAN_POINT ( 'NONE',  ( -0.6823417656250003738, 2.717708333674753618, -1.181850606188749264 ) ) ;
#80099 = CARTESIAN_POINT ( 'NONE',  ( 6.217421135136044441, -0.2594034420708571931, 2.089956235961006659 ) ) ;
#80098 = CARTESIAN_POINT ( 'NONE',  ( -7.009729113465285266, 8.136771039586342624, -1.199719254218446718 ) ) ;
#80100 = CARTESIAN_POINT ( 'NONE',  ( 6.602015318333181781, 0.7961593463888805289, -1.911361562896146671 ) ) ;
#80101 = CARTESIAN_POINT ( 'NONE',  ( 4.496500501226593727, 8.397667684739696270, 0.7998128361456462443 ) ) ;
#80102 = CARTESIAN_POINT ( 'NONE',  ( -5.930802130974132780, 9.006687355190106103, -1.199719254218440723 ) ) ;
#80103 = CARTESIAN_POINT ( 'NONE',  ( -1.580223361175689734, 8.746992034114509096, 2.465615386491402106 ) ) ;
#80104 = CARTESIAN_POINT ( 'NONE',  ( 5.014510501881845883, 1.360076575639699081, -1.427402630902480762 ) ) ;
#80105 = CARTESIAN_POINT ( 'NONE',  ( 6.029558467290160984, -0.2429869472727399504, 2.005020512606956018 ) ) ;
#80106 = CARTESIAN_POINT ( 'NONE',  ( -0.7500000000000006661, -0.1104166659838465292, -1.299038105676652011 ) ) ;
#80107 = CARTESIAN_POINT ( 'NONE',  ( 4.442184936073533486, 0.9892916563519343898, -2.085014998049372625 ) ) ;
#80108 = CARTESIAN_POINT ( 'NONE',  ( 2.131754086930433001, 1.975065156136386335, -0.5945119761870448771 ) ) ;
#80109 = CARTESIAN_POINT ( 'NONE',  ( 7.049876689426101350, 9.247942109129029475, -1.443375672974057666 ) ) ;
#80110 = CARTESIAN_POINT ( 'NONE',  ( 5.716698046817569434, 6.698511138489155137, -1.199719254218452047 ) ) ;
#80111 = CARTESIAN_POINT ( 'NONE',  ( 5.435893244436359240, 5.306573304789342416, -0.7998128361456481317 ) ) ;
#80112 = CARTESIAN_POINT ( 'NONE',  ( -0.6823417656250212460, 1.863541667008083991, 1.181850606188755259 ) ) ;
#80113 = CARTESIAN_POINT ( 'NONE',  ( -2.996596126518174419, 14.55175791338114699, 11.58266829935393005 ) ) ;
#80114 = CARTESIAN_POINT ( 'NONE',  ( 7.253248993186735660, 7.564471368247083660, 0.7216878364870317197 ) ) ;
#80115 = CARTESIAN_POINT ( 'NONE',  ( 4.106061665437168884, 0.7349691374628541940, -2.043110004675054103 ) ) ;
#80116 = CARTESIAN_POINT ( 'NONE',  ( -4.434925645001631445, 8.188180662561569179, 0.7216878364870504825 ) ) ;
#80118 = CARTESIAN_POINT ( 'NONE',  ( 3.386116603743833497, -0.3623624896987759914, -1.805063595765175499 ) ) ;
#80117 = CARTESIAN_POINT ( 'NONE',  ( -2.792616454734997866, 6.201876930592042925, 0.7216878364870317197 ) ) ;
#80120 = CARTESIAN_POINT ( 'NONE',  ( 6.720655732516657821, 4.700665033810172311, 2.388972926809574737 ) ) ;
#80119 = CARTESIAN_POINT ( 'NONE',  ( 1.364683531249988535, 4.155208333674753618, -0.7879004041258239610 ) ) ;
#80121 = CARTESIAN_POINT ( 'NONE',  ( 5.776942576169182608, 2.025397260235710206, -0.8375503648087383457 ) ) ;
#80122 = CARTESIAN_POINT ( 'NONE',  ( 7.104593929172385636, 14.55347104122142810, 9.619174111504673164 ) ) ;
#80123 = CARTESIAN_POINT ( 'NONE',  ( 6.508658281791896094, 1.681912584842374159, -1.513523023287469016 ) ) ;
#80124 = CARTESIAN_POINT ( 'NONE',  ( -5.085529380082158823, 6.726364094520411285, -1.441608068093344741 ) ) ;
#80125 = CARTESIAN_POINT ( 'NONE',  ( 4.624709440338444111, 8.453137518702421360, 0.3515692964491355932 ) ) ;
#80126 = CARTESIAN_POINT ( 'NONE',  ( -5.383996397958228819, 8.335060660042973524, 1.082531754730550855 ) ) ;
#80127 = FACE_OUTER_BOUND ( 'NONE', #32580, .T. ) ;
#80128 = CARTESIAN_POINT ( 'NONE',  ( 6.731742716130249882, -1.158518921844574834, -1.337957499386055682 ) ) ;
#80129 = AXIS2_PLACEMENT_3D ( 'NONE', #32006, #212863, #34118 ) ;
#80130 = CARTESIAN_POINT ( 'NONE',  ( 4.231111847260408787, 1.841413651135707985, 0.8138496092669408322 ) ) ;
#80131 = CARTESIAN_POINT ( 'NONE',  ( 6.331821432781979730, 7.345878745455822312, -1.199719254218445830 ) ) ;
#80132 = CARTESIAN_POINT ( 'NONE',  ( 3.223755556863156180, -2.030008631501342808, 0.5602397303039460263 ) ) ;
#80133 = CARTESIAN_POINT ( 'NONE',  ( 2.513182649960711945, -1.786459940013595205, 0.6919045257178286779 ) ) ;
#80134 = CIRCLE ( 'NONE', #177091, 0.08000000000000025147 ) ;
#80135 = CARTESIAN_POINT ( 'NONE',  ( 3.334415713957098681, 5.977569868670206787, -1.199719254218446718 ) ) ;
#80137 = EDGE_CURVE ( 'NONE', #93347, #37648, #122022, .T. ) ;
#80136 = CARTESIAN_POINT ( 'NONE',  ( 3.648844292986920479, -0.3817546106285915619, -1.932013994212372854 ) ) ;
#80138 = CARTESIAN_POINT ( 'NONE',  ( 2.201827603038747139, -1.870314503716500099, 0.04339327950253490246 ) ) ;
#80139 = CARTESIAN_POINT ( 'NONE',  ( 2.260140581184489239, -1.961506502764579052, 0.04509734162668613960 ) ) ;
#80142 = EDGE_LOOP ( 'NONE', ( #111775, #24924, #65416, #189531 ) ) ;
#80141 = CARTESIAN_POINT ( 'NONE',  ( 1.160255710619631397, 1.910328232974867868, 0.09094507755665059978 ) ) ;
#80140 = CARTESIAN_POINT ( 'NONE',  ( 3.861678741103656165, 1.711552447172806968, -0.2133835738165473228 ) ) ;
#80144 = CARTESIAN_POINT ( 'NONE',  ( 5.233084105194869551, 6.167981546557892436, -1.082531754730548412 ) ) ;
#80143 = CARTESIAN_POINT ( 'NONE',  ( 1.436444770134176485, 1.085300811998829662, -1.921501399296850821 ) ) ;
#80145 = CARTESIAN_POINT ( 'NONE',  ( 1.364683531249988535, 1.426041667008083991, 0.7879004041258500513 ) ) ;
#80146 = CARTESIAN_POINT ( 'NONE',  ( 7.214910300766615769, 11.56914578420308715, -0.7998128361456291469 ) ) ;
#80147 = CARTESIAN_POINT ( 'NONE',  ( 6.737182200980119440, -1.669782060861616291, 0.8434366901180422316 ) ) ;
#80148 = CARTESIAN_POINT ( 'NONE',  ( 2.404166168890689903, 5.245195659253913512, -0.8707498557368191783 ) ) ;
#80149 = CARTESIAN_POINT ( 'NONE',  ( 6.438344962566215024, -1.112565956905732456, 1.745730973219234317 ) ) ;
#80150 =( BOUNDED_SURFACE ( )  B_SPLINE_SURFACE ( 3, 2, ( 
 ( #60813, #79196, #143183 ),
 ( #28314, #92288, #145311 ),
 ( #159380, #209174, #30461 ),
 ( #192932, #108568, #13118 ),
 ( #144254, #124833, #77053 ),
 ( #46721, #194003, #126974 ),
 ( #161532, #174595, #58685 ),
 ( #96546, #177776, #111769 ) ),
 .UNSPECIFIED., .F., .F., .T. ) 
 B_SPLINE_SURFACE_WITH_KNOTS ( ( 4, 2, 2, 4 ),
 ( 3, 3 ),
 ( 0.000000000000000000, 0.0004924884914732710617, 0.0007387327372099065925, 0.0009849769829465421234 ),
 ( 0.000000000000000000, 1.000000000000000000 ),
 .UNSPECIFIED. ) 
 GEOMETRIC_REPRESENTATION_ITEM ( )  RATIONAL_B_SPLINE_SURFACE ( (
 ( 1.000000000000000000, 0.7045118851637580670, 1.000000000000000000),
 ( 1.000000000000000000, 0.7593505504065410916, 1.000000000000000000),
 ( 1.000000000000000000, 0.8104906253031848307, 1.000000000000000000),
 ( 1.000000000000000000, 0.8722646935501724430, 1.000000000000000000),
 ( 1.000000000000000000, 0.8905178607894502774, 1.000000000000000000),
 ( 1.000000000000000000, 0.9170530604353909210, 1.000000000000000000),
 ( 1.000000000000000000, 0.9248184710077167470, 1.000000000000000000),
 ( 1.000000000000000000, 0.9238795325112880708, 1.000000000000000000) ) ) 
 REPRESENTATION_ITEM ( '' )  SURFACE ( )  );
#80151 = CARTESIAN_POINT ( 'NONE',  ( 1.311079954825690619, -1.633285661836245906, 1.272233187909928454 ) ) ;
#80152 = CARTESIAN_POINT ( 'NONE',  ( -1.500000000000013101, 1.379166666666689745, -0.8660254037844313801 ) ) ;
#80153 = CARTESIAN_POINT ( 'NONE',  ( 7.124973419181436007, 8.271222729588529887, -1.199719254218446718 ) ) ;
#80154 = CARTESIAN_POINT ( 'NONE',  ( -8.528242318195895066, 9.908369778438709474, 1.199719254218462483 ) ) ;
#80155 = CARTESIAN_POINT ( 'NONE',  ( 6.039231080244466199, 6.010467446565510130, 0.7998128361456352531 ) ) ;
#80156 = CARTESIAN_POINT ( 'NONE',  ( 5.778019675193696969, 2.089136139637823852, -0.3624112956793351659 ) ) ;
#80157 = CARTESIAN_POINT ( 'NONE',  ( 4.598150373690133463, 5.393538853173795111, -1.199719254218452047 ) ) ;
#80158 = CARTESIAN_POINT ( 'NONE',  ( -1.201851678989727383E-14, 2.321875000341416584, 1.575800808251672791 ) ) ;
#80159 = VERTEX_POINT ( 'NONE', #212154 ) ;
#80161 = EDGE_CURVE ( 'NONE', #118044, #77503, #30236, .T. ) ;
#80160 = CARTESIAN_POINT ( 'NONE',  ( 1.499999999999987121, 2.004166666666684637, 0.8660254037844524744 ) ) ;
#80163 = CARTESIAN_POINT ( 'NONE',  ( 3.979481780810941949, 4.601482484822914998, 1.199719254218464037 ) ) ;
#80162 = CARTESIAN_POINT ( 'NONE',  ( 6.742638286788313451, -1.923764577213080029, -0.3838556375530403630 ) ) ;
#80164 = CARTESIAN_POINT ( 'NONE',  ( 4.024767406304472495, 2.001204788683898617, -0.2439926020210633206 ) ) ;
#80165 = CARTESIAN_POINT ( 'NONE',  ( 3.784325452683900526, -0.6063896298742013080, -1.817255877250848473 ) ) ;
#80166 = DIRECTION ( 'NONE',  ( 0.000000000000000000, -0.000000000000000000, 1.000000000000000000 ) ) ;
#80167 = CARTESIAN_POINT ( 'NONE',  ( 1.980270094416748394, -2.150034404144373301, -0.4237573071887782983 ) ) ;
#80168 = CARTESIAN_POINT ( 'NONE',  ( -1.906195883197663310, 3.231669652568780027, 0.4612786727877704052 ) ) ;
#80169 = CARTESIAN_POINT ( 'NONE',  ( -1.500000000000015099, 0.9104166673494835660, -0.8660254037844313801 ) ) ;
#80170 = CARTESIAN_POINT ( 'NONE',  ( 4.746344407351839045, 1.031357595523854309, -1.728805965807812095 ) ) ;
#80171 = CARTESIAN_POINT ( 'NONE',  ( -5.831978632172702071, 9.955725504176825780, 0.7998128361456481317 ) ) ;
#80173 = CARTESIAN_POINT ( 'NONE',  ( 5.571900387404195243, -0.9513999510230609635, 1.891474119154999745 ) ) ;
#80172 = CARTESIAN_POINT ( 'NONE',  ( -3.741687207691642314, 6.348756928073427730, 1.082531754730560403 ) ) ;
#80174 = CARTESIAN_POINT ( 'NONE',  ( 1.364683531249996529, 9.026041667008060543, 0.7879004041258405033 ) ) ;
#80175 = B_SPLINE_CURVE_WITH_KNOTS ( 'NONE', 3,
 ( #34761, #118225, #2241, #33704, #181025, #100835 ),
 .UNSPECIFIED., .F., .F.,
 ( 4, 2, 4 ),
 ( 0.000000000000000000, 0.0003205138222656014457, 0.0006410276445312028913 ),
 .UNSPECIFIED. ) ;
#80177 = CARTESIAN_POINT ( 'NONE',  ( -7.445362632559989535, 8.715286488521982733, 1.199719254218452047 ) ) ;
#80176 = CARTESIAN_POINT ( 'NONE',  ( 1.944979630195432074, -1.681012947115037015, -1.242954243213564292 ) ) ;
#80179 = ORIENTED_EDGE ( 'NONE', *, *, #179626, .T. ) ;
#80178 = CARTESIAN_POINT ( 'NONE',  ( 1.201696739578085982, -1.724958192343982510, -0.005827584801694830549 ) ) ;
#80180 = CARTESIAN_POINT ( 'NONE',  ( 7.474622759835693131, 7.614814729430110951, -0.7998128361456281477 ) ) ;
#80181 = CARTESIAN_POINT ( 'NONE',  ( -1.242505562683348774, 13.26115344136356455, 0.8107168586029942503 ) ) ;
#80182 = CARTESIAN_POINT ( 'NONE',  ( 7.668547801473440728, -6.765616048178509701, 7.886602582589920196 ) ) ;
#80183 = CARTESIAN_POINT ( 'NONE',  ( -0.4356160240586524068, -9.063431457505059186, 9.626717610576628559 ) ) ;
#80185 = CARTESIAN_POINT ( 'NONE',  ( 8.039621902779343188, 12.32338328664385507, -0.7216878364870328300 ) ) ;
#80184 = CARTESIAN_POINT ( 'NONE',  ( 7.630541526392844887, 7.796719957080126662, 0.7998128361456341429 ) ) ;
#80186 = ORIENTED_EDGE ( 'NONE', *, *, #211770, .T. ) ;
#80187 = CARTESIAN_POINT ( 'NONE',  ( 0.000000000000000000, -0.5000000000000005551, 3.099999999999999201 ) ) ;
#80189 = CARTESIAN_POINT ( 'NONE',  ( 1.998415993447474559, -1.776625121221590220, -0.3526093829155519388 ) ) ;
#80188 = CARTESIAN_POINT ( 'NONE',  ( 4.369470645354133431, 8.319742529546998000, 0.7998128361456271485 ) ) ;
#80190 = CARTESIAN_POINT ( 'NONE',  ( -5.533699252672048985, 9.607732894759390518, -0.7998128361456231517 ) ) ;
#80191 = CARTESIAN_POINT ( 'NONE',  ( 4.566398809704347528, 4.221886787610169556, -0.7998128361456211532 ) ) ;
#80192 = CARTESIAN_POINT ( 'NONE',  ( 6.384963997392946844, 6.413822516572072807, 0.7998128361456352531 ) ) ;
#80193 = CARTESIAN_POINT ( 'NONE',  ( 2.754343952779594318, 1.798010375687082218, 0.2196673718751484539 ) ) ;
#80194 = CARTESIAN_POINT ( 'NONE',  ( 6.539320575229249144, 0.007148032025052972194, 1.896977914940492393 ) ) ;
#80195 = CARTESIAN_POINT ( 'NONE',  ( 4.768780016659259324, 6.770301073365750710, 1.244442160714388068 ) ) ;
#80196 = CARTESIAN_POINT ( 'NONE',  ( 8.419250204406344196, 12.76628297187536809, 1.040834085586084257E-14 ) ) ;
#80197 = VERTEX_POINT ( 'NONE', #128876 ) ;
#80198 = CARTESIAN_POINT ( 'NONE',  ( 2.752234738034575301, -1.855867026150724186, -0.1399345609422244507 ) ) ;
#80199 = CARTESIAN_POINT ( 'NONE',  ( 0.8432031700210621539, 0.3724620109286616576, -1.878856871602401224 ) ) ;
#80200 = CARTESIAN_POINT ( 'NONE',  ( 6.827182134110199030, 0.001020705822914885546, 1.910856149448316721 ) ) ;
#80201 = CARTESIAN_POINT ( 'NONE',  ( -11.97181042169641074, 13.88000000000000078, 0.8318531151397159373 ) ) ;
#80202 = CARTESIAN_POINT ( 'NONE',  ( 4.000000000000012434, 6.499999999999999112, 0.7500000000000006661 ) ) ;
#80203 = AXIS2_PLACEMENT_3D ( 'NONE', #158096, #154885, #122475 ) ;
#80204 = CARTESIAN_POINT ( 'NONE',  ( 4.651083699394226834, 8.303454393088664176, 0.4639335724816190942 ) ) ;
#80205 =( NAMED_UNIT ( * ) SI_UNIT ( $, .STERADIAN. ) SOLID_ANGLE_UNIT ( ) );
#80206 = DIRECTION ( 'NONE',  ( 0.000000000000000000, 1.000000000000000000, 0.000000000000000000 ) ) ;
#80207 = CARTESIAN_POINT ( 'NONE',  ( 8.609064354997688184, 9.146255957026539818, 1.040834085586084257E-14 ) ) ;
#80208 = CARTESIAN_POINT ( 'NONE',  ( 4.328926673881399623, -1.836050571085739769, -0.7129182788949259830 ) ) ;
#80209 = EDGE_CURVE ( 'NONE', #46203, #96430, #212045, .T. ) ;
#80210 = CARTESIAN_POINT ( 'NONE',  ( -5.416646063859567484, 6.278174148379618735, 1.199719254218450271 ) ) ;
#80211 = CARTESIAN_POINT ( 'NONE',  ( -0.1231583423410937961, 7.054063922337696191, 3.955400951015612065 ) ) ;
#80212 = CARTESIAN_POINT ( 'NONE',  ( -3.096762063222531225, 6.448889905702306358, -0.7260975201865252915 ) ) ;
#80213 = CARTESIAN_POINT ( 'NONE',  ( 6.544889499999918314, -1.757580744090202041, -1.308772488114395616 ) ) ;
#80214 = SURFACE_SIDE_STYLE ('',( #99663 ) ) ;
#80215 = CARTESIAN_POINT ( 'NONE',  ( 5.403319659429405952, 1.574929826682970990, 1.109050863186450853 ) ) ;
#80216 = CARTESIAN_POINT ( 'NONE',  ( -6.344325816190970357, 9.489131654609717970, 1.199719254218452047 ) ) ;
#80217 = EDGE_CURVE ( 'NONE', #106888, #171296, #111814, .T. ) ;
#80218 = CARTESIAN_POINT ( 'NONE',  ( -1.219999999999995977, 5.900000000000024336, 1.229247124133362667E-14 ) ) ;
#80219 = CARTESIAN_POINT ( 'NONE',  ( 2.280145854635793334, 1.358931147977986420, 1.738775483816151768 ) ) ;
#80220 =( NAMED_UNIT ( * ) PLANE_ANGLE_UNIT ( ) SI_UNIT ( $, .RADIAN. ) );
#80221 = CARTESIAN_POINT ( 'NONE',  ( 0.3867804997886997720, -1.801505969789623629, -0.6421655129100201087 ) ) ;
#80222 = ORIENTED_EDGE ( 'NONE', *, *, #149964, .F. ) ;
#80223 = ORIENTED_EDGE ( 'NONE', *, *, #170032, .F. ) ;
#80224 = CARTESIAN_POINT ( 'NONE',  ( 6.965690641875434075, -0.4316760948062084990, 1.928339623932231239 ) ) ;
#80225 = CARTESIAN_POINT ( 'NONE',  ( 1.558044835347382362, -1.372074245553561722, 1.374660786877460072 ) ) ;
#80226 = EDGE_LOOP ( 'NONE', ( #82825, #46886, #76841, #83326, #27713 ) ) ;
#80227 = CARTESIAN_POINT ( 'NONE',  ( 0.6497672626537411844, -0.2439889887937417567, -2.001205234435725622 ) ) ;
#80229 = CARTESIAN_POINT ( 'NONE',  ( 5.946130789595732935, -0.8379359121385165921, 1.661726607698276181 ) ) ;
#80228 = CARTESIAN_POINT ( 'NONE',  ( -6.642568916052639771, 6.714361588341672515, 0.000000000000000000 ) ) ;
#80230 = CARTESIAN_POINT ( 'NONE',  ( 4.688087255275310561, 8.691461907788344377, -0.7998128361456381397 ) ) ;
#80231 = CARTESIAN_POINT ( 'NONE',  ( -6.137101742630204804, 5.375560105519675780, 2.500000000000000888 ) ) ;
#80232 = CARTESIAN_POINT ( 'NONE',  ( 1.451998047841835060, 7.315968950352750966, -4.301760722580861618 ) ) ;
#80233 = CARTESIAN_POINT ( 'NONE',  ( -6.067437437315529536, 7.037430750744921859, 1.199719254218450271 ) ) ;
#80234 = CARTESIAN_POINT ( 'NONE',  ( -8.086512275908061653, 8.398962174839683215, 0.000000000000000000 ) ) ;
#80235 = CARTESIAN_POINT ( 'NONE',  ( 1.681448347407452193, 1.514353137444489406, 1.584415833815432162 ) ) ;
#80236 = CARTESIAN_POINT ( 'NONE',  ( 2.738383840280320669, 6.138605547061593448, 0.7216878364870338292 ) ) ;
#80237 = ORIENTED_EDGE ( 'NONE', *, *, #170444, .T. ) ;
#80238 = AXIS2_PLACEMENT_3D ( 'NONE', #76042, #142144, #89111 ) ;
#80239 = CARTESIAN_POINT ( 'NONE',  ( 0.3645075752534727709, 3.999999999999974243, -0.9782388703847851863 ) ) ;
#80240 = CARTESIAN_POINT ( 'NONE',  ( 0.000000000000000000, 1.000000000000000888, 0.000000000000000000 ) ) ;
#80241 = CARTESIAN_POINT ( 'NONE',  ( 1.734698295210383767, 0.1775668987445792879, 1.817036636966688823 ) ) ;
#80242 = CARTESIAN_POINT ( 'NONE',  ( -3.810004860640155311, 4.403759411290286252, 1.199719254218462483 ) ) ;
#80243 =( BOUNDED_SURFACE ( )  B_SPLINE_SURFACE ( 1, 2, ( 
 ( #45001, #178190, #29806, #95892, #161945, #76403, #145726, #42874, #63364, #175001, #26587, #126312, #11394, #127384, #77472, #111111, #129520, #47136, #30880, #163007, #177115, #14589, #59090, #176061, #191211, #158734, #160868, #143591, #147824, #52444, #1522, #212792, #115376, #116430, #99071, #81742, #98020, #117505, #131612, #118570, #68662, #167266, #164075, #17774, #102253, #197611, #64430, #213842, #65461, #18851, #168327, #49255, #101177, #133731, #449, #80686, #67586, #181370, #146777, #183497, #184556, #200793, #82800, #148876, #32994, #165124, #130574, #199738, #51384, #16715, #48206, #132660, #35106, #66517, #198664, #31936, #84935, #151024, #134786, #50312, #196564, #114318, #182423, #36177, #34050, #100123, #166185, #83862, #149953, #180316, #2593, #15655, #6862, #170449, #137970, #41550, #202931, #169389, #135834, #171519, #203989, #54574, #155281, #20974, #120722, #87071, #185623, #19922, #38324, #56712, #37256, #186695, #104400, #22034, #153141, #7941, #122881, #106579, #3652, #55637, #72941, #88145, #86008, #4716, #70791, #154212, #136904, #5784, #71861, #121793, #189905, #152082, #139044, #69730, #201859, #188839, #53505, #172607, #187761 ),
 ( #119640, #39391, #105486, #23112, #24183, #89229, #205070, #40475, #90287, #156356, #206148, #74031, #140122, #57776, #123937, #107663, #103326, #210414, #75097, #95646, #141207, #58841, #158484, #43684, #159543, #126059, #11140, #144412, #176866, #62056, #194173, #93502, #13290, #177941, #10083, #94569, #124998, #127132, #76157, #26331, #145481, #160613, #91368, #208273, #209330, #192022, #129278, #174757, #45818, #193103, #92445, #111939, #211477, #142262, #190955, #42620, #59905, #29555, #60978, #77217, #27404, #157429, #28478, #63113, #109802, #44753, #12214, #110860, #128211, #207218, #78285, #79363, #161697, #195252, #46888, #173691, #143336, #25267, #175811, #9022, #108730, #150775, #200546, #68414, #134541, #31692, #147574, #197366, #47961, #182171, #81496, #15405, #33800, #132418, #113001, #163827, #65217, #16467, #80429, #131369, #32741, #200, #199482, #114077, #213593, #50063, #116186, #97767, #84688, #82547, #165941, #99879, #17526, #83614, #180068, #149696, #14340, #34852, #146529, #212546, #49007, #115125, #98823, #181121, #164872, #1277, #67335, #133480, #51128, #148634, #167015, #117250, #66270, #183249, #64187, #198419, #100927, #18608, #2337 ) ),
 .UNSPECIFIED., .F., .F., .F. ) 
 B_SPLINE_SURFACE_WITH_KNOTS ( ( 2, 2 ),
 ( 3, 2, 2, 2, 2, 2, 2, 2, 2, 2, 2, 2, 2, 2, 2, 2, 2, 2, 2, 2, 2, 2, 2, 2, 2, 2, 2, 2, 2, 2, 2, 2, 2, 2, 2, 2, 2, 2, 2, 2, 2, 2, 2, 2, 2, 2, 2, 2, 2, 2, 2, 2, 2, 2, 2, 2, 2, 2, 2, 2, 2, 2, 2, 2, 2, 2, 2, 2, 2, 3 ),
 ( 0.000000000000000000, 1.000000000000000000 ),
 ( 0.000000000000000000, 0.01388888888888888812, 0.02777777777777777624, 0.04166666666666666435, 0.05555555555555555247, 0.06944444444444444753, 0.08333333333333332871, 0.09722222222222222376, 0.1111111111111111049, 0.1250000000000000000, 0.1388888888888888951, 0.1527777777777777901, 0.1666666666666666574, 0.1805555555555555525, 0.1944444444444444475, 0.2083333333333333426, 0.2222222222222222099, 0.2361111111111111049, 0.2500000000000000000, 0.2638888888888888951, 0.2777777777777777901, 0.2916666666666666852, 0.3055555555555555802, 0.3194444444444444198, 0.3333333333333333148, 0.3472222222222222099, 0.3611111111111111049, 0.3750000000000000000, 0.3888888888888888951, 0.4027777777777777901, 0.4166666666666666852, 0.4305555555555555802, 0.4444444444444444198, 0.4583333333333333148, 0.4722222222222222099, 0.4861111111111111049, 0.5000000000000000000, 0.5138888888888888395, 0.5277777777777777901, 0.5416666666666666297, 0.5555555555555555802, 0.5694444444444444198, 0.5833333333333333703, 0.5972222222222222099, 0.6111111111111111605, 0.6250000000000000000, 0.6388888888888888395, 0.6527777777777777901, 0.6666666666666666297, 0.6805555555555555802, 0.6944444444444444198, 0.7083333333333333703, 0.7222222222222222099, 0.7361111111111111605, 0.7500000000000000000, 0.7638888888888888395, 0.7777777777777777901, 0.7916666666666666297, 0.8055555555555555802, 0.8194444444444444198, 0.8333333333333333703, 0.8472222222222222099, 0.8611111111111111605, 0.8750000000000000000, 0.8888888888888888395, 0.9027777777777777901, 0.9166666666666666297, 0.9305555555555555802, 0.9444444444444444198, 0.9523586252412667985 ),
 .UNSPECIFIED. ) 
 GEOMETRIC_REPRESENTATION_ITEM ( )  RATIONAL_B_SPLINE_SURFACE ( (
 ( 1.000000000000000000, 0.8660254037844387076, 1.000000000000000000, 0.8660254037844387076, 1.000000000000000000, 0.8660254037844387076, 1.000000000000000000, 0.8660254037844387076, 1.000000000000000000, 0.8660254037844387076, 1.000000000000000000, 0.8660254037844387076, 1.000000000000000000, 0.8660254037844387076, 1.000000000000000000, 0.8660254037844387076, 1.000000000000000000, 0.8660254037844387076, 1.000000000000000000, 0.8660254037844387076, 1.000000000000000000, 0.8660254037844387076, 1.000000000000000000, 0.8660254037844387076, 1.000000000000000000, 0.8660254037844387076, 1.000000000000000000, 0.8660254037844387076, 1.000000000000000000, 0.8660254037844387076, 1.000000000000000000, 0.8660254037844387076, 1.000000000000000000, 0.8660254037844387076, 1.000000000000000000, 0.8660254037844387076, 1.000000000000000000, 0.8660254037844387076, 1.000000000000000000, 0.8660254037844387076, 1.000000000000000000, 0.8660254037844387076, 1.000000000000000000, 0.8660254037844387076, 1.000000000000000000, 0.8660254037844387076, 1.000000000000000000, 0.8660254037844387076, 1.000000000000000000, 0.8660254037844387076, 1.000000000000000000, 0.8660254037844387076, 1.000000000000000000, 0.8660254037844387076, 1.000000000000000000, 0.8660254037844387076, 1.000000000000000000, 0.8660254037844387076, 1.000000000000000000, 0.8660254037844387076, 1.000000000000000000, 0.8660254037844387076, 1.000000000000000000, 0.8660254037844387076, 1.000000000000000000, 0.8660254037844387076, 1.000000000000000000, 0.8660254037844387076, 1.000000000000000000, 0.8660254037844387076, 1.000000000000000000, 0.8660254037844387076, 1.000000000000000000, 0.8660254037844387076, 1.000000000000000000, 0.8660254037844387076, 1.000000000000000000, 0.8660254037844387076, 1.000000000000000000, 0.8660254037844387076, 1.000000000000000000, 0.8660254037844387076, 1.000000000000000000, 0.8660254037844387076, 1.000000000000000000, 0.8660254037844387076, 1.000000000000000000, 0.8660254037844387076, 1.000000000000000000, 0.8660254037844387076, 1.000000000000000000, 0.8660254037844387076, 1.000000000000000000, 0.8660254037844387076, 1.000000000000000000, 0.8660254037844387076, 1.000000000000000000, 0.8660254037844387076, 1.000000000000000000, 0.8660254037844387076, 1.000000000000000000, 0.8660254037844387076, 1.000000000000000000, 0.8660254037844387076, 1.000000000000000000, 0.8660254037844387076, 1.000000000000000000, 0.8660254037844387076, 1.000000000000000000, 0.8660254037844387076, 1.000000000000000000, 0.8660254037844387076, 1.000000000000000000, 0.8660254037844387076, 1.000000000000000000, 0.8660254037844387076, 1.000000000000000000, 0.8660254037844387076, 1.000000000000000000, 0.8660254037844387076, 1.000000000000000000, 0.8660254037844387076, 1.000000000000000000, 0.8660254037844387076, 1.000000000000000000, 0.8660254037844387076, 1.000000000000000000, 0.8660254037844387076, 1.000000000000000000, 0.8660254037844387076, 1.000000000000000000, 0.8660254037844387076, 1.000000000000000000, 0.8660254037844387076, 1.000000000000000000, 0.8660254037844387076, 1.000000000000000000, 0.9236584592825519691, 0.9343189473637074638),
 ( 1.000000000000000000, 0.8660254037844387076, 1.000000000000000000, 0.8660254037844387076, 1.000000000000000000, 0.8660254037844387076, 1.000000000000000000, 0.8660254037844387076, 1.000000000000000000, 0.8660254037844387076, 1.000000000000000000, 0.8660254037844387076, 1.000000000000000000, 0.8660254037844387076, 1.000000000000000000, 0.8660254037844387076, 1.000000000000000000, 0.8660254037844387076, 1.000000000000000000, 0.8660254037844387076, 1.000000000000000000, 0.8660254037844387076, 1.000000000000000000, 0.8660254037844387076, 1.000000000000000000, 0.8660254037844387076, 1.000000000000000000, 0.8660254037844387076, 1.000000000000000000, 0.8660254037844387076, 1.000000000000000000, 0.8660254037844387076, 1.000000000000000000, 0.8660254037844387076, 1.000000000000000000, 0.8660254037844387076, 1.000000000000000000, 0.8660254037844387076, 1.000000000000000000, 0.8660254037844387076, 1.000000000000000000, 0.8660254037844387076, 1.000000000000000000, 0.8660254037844387076, 1.000000000000000000, 0.8660254037844387076, 1.000000000000000000, 0.8660254037844387076, 1.000000000000000000, 0.8660254037844387076, 1.000000000000000000, 0.8660254037844387076, 1.000000000000000000, 0.8660254037844387076, 1.000000000000000000, 0.8660254037844387076, 1.000000000000000000, 0.8660254037844387076, 1.000000000000000000, 0.8660254037844387076, 1.000000000000000000, 0.8660254037844387076, 1.000000000000000000, 0.8660254037844387076, 1.000000000000000000, 0.8660254037844387076, 1.000000000000000000, 0.8660254037844387076, 1.000000000000000000, 0.8660254037844387076, 1.000000000000000000, 0.8660254037844387076, 1.000000000000000000, 0.8660254037844387076, 1.000000000000000000, 0.8660254037844387076, 1.000000000000000000, 0.8660254037844387076, 1.000000000000000000, 0.8660254037844387076, 1.000000000000000000, 0.8660254037844387076, 1.000000000000000000, 0.8660254037844387076, 1.000000000000000000, 0.8660254037844387076, 1.000000000000000000, 0.8660254037844387076, 1.000000000000000000, 0.8660254037844387076, 1.000000000000000000, 0.8660254037844387076, 1.000000000000000000, 0.8660254037844387076, 1.000000000000000000, 0.8660254037844387076, 1.000000000000000000, 0.8660254037844387076, 1.000000000000000000, 0.8660254037844387076, 1.000000000000000000, 0.8660254037844387076, 1.000000000000000000, 0.8660254037844387076, 1.000000000000000000, 0.8660254037844387076, 1.000000000000000000, 0.8660254037844387076, 1.000000000000000000, 0.8660254037844387076, 1.000000000000000000, 0.8660254037844387076, 1.000000000000000000, 0.8660254037844387076, 1.000000000000000000, 0.8660254037844387076, 1.000000000000000000, 0.8660254037844387076, 1.000000000000000000, 0.8660254037844387076, 1.000000000000000000, 0.8660254037844387076, 1.000000000000000000, 0.8660254037844387076, 1.000000000000000000, 0.8660254037844387076, 1.000000000000000000, 0.8660254037844387076, 1.000000000000000000, 0.8660254037844387076, 1.000000000000000000, 0.8660254037844387076, 1.000000000000000000, 0.8660254037844387076, 1.000000000000000000, 0.8660254037844387076, 1.000000000000000000, 0.9236584592825519691, 0.9343189473637074638) ) ) 
 REPRESENTATION_ITEM ( '' )  SURFACE ( )  );
#80244 = CARTESIAN_POINT ( 'NONE',  ( 0.1009995753616283604, 2.612933547399907130, -1.997555607063249195 ) ) ;
#80245 = CARTESIAN_POINT ( 'NONE',  ( 6.609000000000011532, 3.695567819995113634, 2.514302272609474809 ) ) ;
#80246 = CARTESIAN_POINT ( 'NONE',  ( 9.915090410295563927, 10.46202698829998567, -0.7998128361456281477 ) ) ;
#80247 = CARTESIAN_POINT ( 'NONE',  ( 6.234959169399230561, 0.1841439077357870380, 1.816378869960999509 ) ) ;
#80248 = CARTESIAN_POINT ( 'NONE',  ( 4.996903459272754588, 0.3314677610860050638, 1.933379042443456486 ) ) ;
#80249 = CARTESIAN_POINT ( 'NONE',  ( -8.311311860377216476, 9.655284244316948872, -1.199719254218446718 ) ) ;
#80250 = CARTESIAN_POINT ( 'NONE',  ( 6.145923705696426431, 6.064665832934283962, 0.7998128361456341429 ) ) ;
#80251 = CARTESIAN_POINT ( 'NONE',  ( 5.056268342064010213, -1.587557771011731678, 1.511049258477934032 ) ) ;
#80252 = B_SPLINE_CURVE_WITH_KNOTS ( 'NONE', 3,
 ( #129682, #96052, #13694, #196723, #116589, #63528, #147986, #132820, #195666, #163170 ),
 .UNSPECIFIED., .F., .F.,
 ( 4, 2, 2, 2, 4 ),
 ( 0.001965249434206598270, 0.002424473194169422634, 0.002883696954132246131, 0.003342920714095069627, 0.003802144474057893558 ),
 .UNSPECIFIED. ) ;
#80253 = CARTESIAN_POINT ( 'NONE',  ( 5.820528018968444961, 5.685037531751635953, 0.7998128361456341429 ) ) ;
#80254 = CARTESIAN_POINT ( 'NONE',  ( 4.100488025649267954, 2.059819936833905185, 0.2079151390043249559 ) ) ;
#80256 = CARTESIAN_POINT ( 'NONE',  ( -1.201851678989727383E-14, 1.384375000341419693, 1.575800808251672791 ) ) ;
#80255 = SURFACE_STYLE_USAGE ( .BOTH. , #1108 ) ;
#80257 = EDGE_LOOP ( 'NONE', ( #40796, #135320, #151450 ) ) ;
#80258 = CARTESIAN_POINT ( 'NONE',  ( 4.571052534358505781, -1.084669189052098082, 2.026668040654127090 ) ) ;
#80259 = CARTESIAN_POINT ( 'NONE',  ( 7.537970219518073556, 9.817384560903001045, -1.443375672974057666 ) ) ;
#80261 = CARTESIAN_POINT ( 'NONE',  ( -3.619663825168619731, 7.166765529431275539, 1.040834085586084257E-14 ) ) ;
#80260 = CARTESIAN_POINT ( 'NONE',  ( 6.536439455564164724, 7.758839131980592718, 1.082531754730549967 ) ) ;
#80262 = CARTESIAN_POINT ( 'NONE',  ( 6.620655732516673275, 1.290356161719278028, 1.942653802560645460 ) ) ;
#80263 = DIRECTION ( 'NONE',  ( 0.000000000000000000, 0.000000000000000000, 1.000000000000000000 ) ) ;
#80264 = CARTESIAN_POINT ( 'NONE',  ( 3.538947879116743689, -1.471199320522957876, -1.267674678009507394 ) ) ;
#80265 = ORIENTED_EDGE ( 'NONE', *, *, #96386, .F. ) ;
#80266 = CARTESIAN_POINT ( 'NONE',  ( -0.03130284803980282887, -9.439835433791163410, 9.605218923937870912 ) ) ;
#80267 = CARTESIAN_POINT ( 'NONE',  ( 4.922078805074791674, -1.902621863305080430, 0.1933406509087298719 ) ) ;
#80268 = FACE_OUTER_BOUND ( 'NONE', #177770, .T. ) ;
#80269 = CARTESIAN_POINT ( 'NONE',  ( 4.682452625960944026, -1.673401091975829091, -0.4171936932430859168 ) ) ;
#80270 = CARTESIAN_POINT ( 'NONE',  ( 4.751185534883737738, 0.1928377863454934504, -2.007255887737584121 ) ) ;
#80271 = CARTESIAN_POINT ( 'NONE',  ( 4.905072937705025282, -1.228516145343660826, -1.942733121961652376 ) ) ;
#80272 = CARTESIAN_POINT ( 'NONE',  ( 0.000000000000000000, -0.8934598047668927956, -3.291472234583660672 ) ) ;
#80273 = CARTESIAN_POINT ( 'NONE',  ( 0.3994152196779980346, 1.832435997337564348, -1.229551327501000380 ) ) ;
#80275 = CARTESIAN_POINT ( 'NONE',  ( -5.831415467653581430, 5.975941931783510519, 0.7216878364870257245 ) ) ;
#80274 = CARTESIAN_POINT ( 'NONE',  ( -8.805130697071332335, 12.36007068230351358, 1.199719254218462483 ) ) ;
#80276 = CARTESIAN_POINT ( 'NONE',  ( 5.483597806724121781, 1.189268614677735592, 1.310771863001722437 ) ) ;
#80277 = CARTESIAN_POINT ( 'NONE',  ( 4.623672751230786027, 0.3474658942751900903, 1.986100912583692812 ) ) ;
#80279 = CARTESIAN_POINT ( 'NONE',  ( 1.588225008415785844, -2.281566021618782081, -0.2212011980115625998 ) ) ;
#80278 = CARTESIAN_POINT ( 'NONE',  ( 7.062871678076271920, 7.204714810702593120, -0.7998128361456341429 ) ) ;
#80280 = CARTESIAN_POINT ( 'NONE',  ( 1.394060603838151779, 1.424319145653055507, -0.9997159833949519347 ) ) ;
#80281 = CARTESIAN_POINT ( 'NONE',  ( 11.91294103507058288, 11.11460089956400843, -1.446263142085487674 ) ) ;
#80282 = CARTESIAN_POINT ( 'NONE',  ( 1.071195256775770543, 1.317505809736085665, -1.127239923523750909 ) ) ;
#80283 = CARTESIAN_POINT ( 'NONE',  ( -0.6801582343750438575, 0.6302083336747199560, -1.178068619123869398 ) ) ;
#80284 = CARTESIAN_POINT ( 'NONE',  ( -0.4288785890452732064, 3.049942316455313218, 0.4196807566830707548 ) ) ;
#80285 = CARTESIAN_POINT ( 'NONE',  ( 1.522189222387077656, 2.139176736804601298, -0.3705008953195278454 ) ) ;
#80286 = CARTESIAN_POINT ( 'NONE',  ( 2.782435679340321766, -0.5899881929209308540, -1.928257399728677601 ) ) ;
#80287 = AXIS2_PLACEMENT_3D ( 'NONE', #185238, #169004, #5404 ) ;
#80288 = CARTESIAN_POINT ( 'NONE',  ( -0.7500000000000006661, 0.8895833340161543035, -1.299038105676652011 ) ) ;
#80289 = CARTESIAN_POINT ( 'NONE',  ( 0.2000540296341560831, -1.925883223908849251, -0.05090804828828016798 ) ) ;
#80290 = CARTESIAN_POINT ( 'NONE',  ( -1.364683531250014514, 12.83854166700806232, -0.7879004041258335089 ) ) ;
#80291 = CARTESIAN_POINT ( 'NONE',  ( 2.408681662258719047, -2.215777464676274011, -0.1586666079704464882 ) ) ;
#80292 = VERTEX_POINT ( 'NONE', #15020 ) ;
#80294 = STYLED_ITEM ( 'NONE', ( #60244 ), #50933 ) ;
#80293 = CARTESIAN_POINT ( 'NONE',  ( 6.773846765316628549, -7.473374494057231310, 6.773846765316613450 ) ) ;
#80295 = CARTESIAN_POINT ( 'NONE',  ( -1.402160292154681736E-14, -1.037499999999977662, 1.732050807568877637 ) ) ;
#80296 = CARTESIAN_POINT ( 'NONE',  ( 7.052212457402625922, 11.37933163361175382, -0.7998128361456291469 ) ) ;
#80297 = CARTESIAN_POINT ( 'NONE',  ( 0.000000000000000000, -9.919999999999998153, 0.000000000000000000 ) ) ;
#80298 =( NAMED_UNIT ( * ) PLANE_ANGLE_UNIT ( ) SI_UNIT ( $, .RADIAN. ) );
#80299 = CARTESIAN_POINT ( 'NONE',  ( 5.618645907585640309, -0.03427301787072359329, 1.740288698465036976 ) ) ;
#80300 = CARTESIAN_POINT ( 'NONE',  ( 3.279693232472491893, -1.891448704997201302, 0.5207070127687256633 ) ) ;
#80302 = CARTESIAN_POINT ( 'NONE',  ( -6.670248388243482651, 9.765411638717282017, 1.082531754730548412 ) ) ;
#80301 = CARTESIAN_POINT ( 'NONE',  ( 2.686486993802192913, 6.285985259411197568, 0.7998128361456362523 ) ) ;
#80303 = DIRECTION ( 'NONE',  ( -0.000000000000000000, 1.000000000000000000, -0.000000000000000000 ) ) ;
#80304 = CARTESIAN_POINT ( 'NONE',  ( 4.640055761359395348, 0.9730784542925293712, -2.042606338686814738 ) ) ;
#80305 = CARTESIAN_POINT ( 'NONE',  ( 0.9770945003616584579, 1.905102050789074353, 0.7911672170514363334 ) ) ;
#80306 = CARTESIAN_POINT ( 'NONE',  ( -6.938021921891187382, 9.117444880338284818, -1.599625672291263179 ) ) ;
#80307 = CARTESIAN_POINT ( 'NONE',  ( 2.729655337971720552, -2.111368630554604220, 0.8135341271046038214 ) ) ;
#80308 = ORIENTED_EDGE ( 'NONE', *, *, #1901, .F. ) ;
#80309 = CARTESIAN_POINT ( 'NONE',  ( 1.499999999999987121, 1.285416667349485120, 0.8660254037844524744 ) ) ;
#80310 = CARTESIAN_POINT ( 'NONE',  ( 3.426877311086639288, 0.04264493303338459662, 1.870215716092846314 ) ) ;
#80311 = CARTESIAN_POINT ( 'NONE',  ( 2.654579492894239223, 0.9294799389642364185, 1.463784073337747849 ) ) ;
#80312 = CARTESIAN_POINT ( 'NONE',  ( 6.251546423958431298, 2.185849743821382862, -0.1592787069685035195 ) ) ;
#80313 = CARTESIAN_POINT ( 'NONE',  ( 0.1127427399064059588, -0.9454589178800475446, -1.991880357201977425 ) ) ;
#80314 = CARTESIAN_POINT ( 'NONE',  ( 4.258765444007106105, -1.603684720688375975, 1.449730421305382544 ) ) ;
#80315 = CARTESIAN_POINT ( 'NONE',  ( 4.470608273529505183, -0.001430698596973853159, -1.942124712226586558 ) ) ;
#80316 = CARTESIAN_POINT ( 'NONE',  ( -8.618179199781044630, 13.20629283305325963, 0.7998128361456341429 ) ) ;
#80317 = DIRECTION ( 'NONE',  ( 8.638326563840814399E-31, 0.000000000000000000, 1.000000000000000000 ) ) ;
#80318 = CARTESIAN_POINT ( 'NONE',  ( 4.078835981324096416, 7.487686104445945290, 0.5747339805607706298 ) ) ;
#80319 = CARTESIAN_POINT ( 'NONE',  ( -7.721398836998370818, -5.827195405469540290, 7.721398836998400128 ) ) ;
#80320 = CARTESIAN_POINT ( 'NONE',  ( 4.760321332173959696, 4.726332107057286791, 0.000000000000000000 ) ) ;
#80321 = CARTESIAN_POINT ( 'NONE',  ( -5.670636218918978066, 5.580440108352386019, 0.2509703219331788637 ) ) ;
#80322 = CARTESIAN_POINT ( 'NONE',  ( 5.906875006520014182, -1.122496024291631755, -1.674889250513518446 ) ) ;
#80323 = CARTESIAN_POINT ( 'NONE',  ( -8.482597663644387609, 13.04811437422715414, -0.7998128361456281477 ) ) ;
#80324 = CARTESIAN_POINT ( 'NONE',  ( 6.936968151686458306, 11.24487994360957188, 0.7998128361456462443 ) ) ;
#80325 = CARTESIAN_POINT ( 'NONE',  ( 3.984117037569365305, 5.741498858621315371, 1.599625672291261402 ) ) ;
#80327 = CARTESIAN_POINT ( 'NONE',  ( -4.187547269546461948, 7.837270521969020187, 0.3263639828635342410 ) ) ;
#80326 = CARTESIAN_POINT ( 'NONE',  ( 3.193790821891542731, -0.7392406677243367197, 1.669511829839696260 ) ) ;
#80328 = CARTESIAN_POINT ( 'NONE',  ( -0.1296875068448125057, 2.889142263448498227, -2.315371602238533555 ) ) ;
#80329 = EDGE_LOOP ( 'NONE', ( #151411, #45799, #61960, #152198, #110102, #187351 ) ) ;
#80330 = CARTESIAN_POINT ( 'NONE',  ( -4.868786560638931782, 6.773613302202437403, 1.443375672974058777 ) ) ;
#80331 = CARTESIAN_POINT ( 'NONE',  ( 1.001543065824772753E-15, -3.959374999522043304, 3.793834371823811669 ) ) ;
#80332 = CARTESIAN_POINT ( 'NONE',  ( -8.809047120577080392, 11.30030761213851953, 1.599625672291269396 ) ) ;
#80333 = CARTESIAN_POINT ( 'NONE',  ( 6.270176981224262924, 2.014133449145325105, -0.1505704652167982327 ) ) ;
#80334 = CARTESIAN_POINT ( 'NONE',  ( 0.9793288802587530872, -1.918618388578940737, -0.9032494106611321794 ) ) ;
#80335 = VERTEX_POINT ( 'NONE', #195935 ) ;
#80336 = CARTESIAN_POINT ( 'NONE',  ( -6.283277845290492714, 6.295188672452495915, -0.7998128361456362523 ) ) ;
#80337 = CARTESIAN_POINT ( 'NONE',  ( 2.377597188713850507, -1.806433865756534640, 0.4466691629738496760 ) ) ;
#80338 = PRESENTATION_LAYER_ASSIGNMENT (  '', '', ( #31953 ) ) ;
#80339 = CARTESIAN_POINT ( 'NONE',  ( 3.867100128395839942, 5.534702787927018974, -1.599625672291255185 ) ) ;
#80340 = CARTESIAN_POINT ( 'NONE',  ( 0.1984014031938194922, -2.161264429664040421, -0.05129915172277095536 ) ) ;
#80341 = CARTESIAN_POINT ( 'NONE',  ( 6.381482430641396419, -0.5404875331735843336, -1.942542459342583294 ) ) ;
#80342 = ORIENTED_EDGE ( 'NONE', *, *, #4745, .T. ) ;
#80343 = DIRECTION ( 'NONE',  ( 0.000000000000000000, -1.000000000000000000, 0.000000000000000000 ) ) ;
#80344 = DIRECTION ( 'NONE',  ( 3.330669073875479482E-16, -3.330669073875479482E-16, -1.000000000000000000 ) ) ;
#80347 = EDGE_LOOP ( 'NONE', ( #213002, #45741, #80068, #48402 ) ) ;
#80346 = CARTESIAN_POINT ( 'NONE',  ( 0.07680821025393863577, 2.892152076732486421, -2.299782885777381658 ) ) ;
#80345 = CARTESIAN_POINT ( 'NONE',  ( -5.666381855868691808, 5.575476684793721383, 0.000000000000000000 ) ) ;
#80348 = CARTESIAN_POINT ( 'NONE',  ( 6.378761646814803399, 6.917158162233129737, 0.8102004381213165907 ) ) ;
#80349 = CARTESIAN_POINT ( 'NONE',  ( 6.063827332385394620, 1.649827434358666967, -1.158513616066357832 ) ) ;
#80350 = CARTESIAN_POINT ( 'NONE',  ( 4.154132678086497776, -1.362845063541193946, 1.238102162693654584 ) ) ;
#80351 = B_SPLINE_CURVE_WITH_KNOTS ( 'NONE', 3,
 ( #143471, #194310, #45951, #113132 ),
 .UNSPECIFIED., .F., .F.,
 ( 4, 4 ),
 ( 0.000000000000000000, 0.0002602974955195480741 ),
 .UNSPECIFIED. ) ;
#80352 = CARTESIAN_POINT ( 'NONE',  ( -0.02299388927986567924, 4.093419149701410298, -2.466026074291859160 ) ) ;
#80353 = CARTESIAN_POINT ( 'NONE',  ( 3.422812307543467103, 1.464285610008815963, -1.783632237398341536 ) ) ;
#80354 = CARTESIAN_POINT ( 'NONE',  ( 4.518610335104485287, 8.493738834255713854, 0.000000000000000000 ) ) ;
#80355 = CARTESIAN_POINT ( 'NONE',  ( 5.747404748698970778, -1.700087083557629386, -1.334863535946126722 ) ) ;
#80356 = CARTESIAN_POINT ( 'NONE',  ( 8.118635056484817980, 8.366162408854107113, 0.7998128361456481317 ) ) ;
#80357 = CARTESIAN_POINT ( 'NONE',  ( 1.382261328670054246, -0.2867773604850975544, -1.920668630092968732 ) ) ;
#80358 = ADVANCED_FACE ( 'NONE', ( #83228 ), #25300, .T. ) ;
#80359 = CARTESIAN_POINT ( 'NONE',  ( -2.937312835655025101, 6.578615408239493867, 1.040834085586084257E-14 ) ) ;
#80360 = ORIENTED_EDGE ( 'NONE', *, *, #152637, .F. ) ;
#80361 = EDGE_CURVE ( 'NONE', #108697, #71069, #211092, .T. ) ;
#80362 = CARTESIAN_POINT ( 'NONE',  ( 4.552342272275657464, 2.055464322635578878, -1.028527531867760914 ) ) ;
#80363 = DIRECTION ( 'NONE',  ( 0.000000000000000000, 0.000000000000000000, -1.000000000000000000 ) ) ;
#80364 = CARTESIAN_POINT ( 'NONE',  ( -4.573896719763875574, 6.429575154514868274, -1.599625672291271394 ) ) ;
#80365 = CIRCLE ( 'NONE', #121870, 11.18000000000000149 ) ;
#80366 = CARTESIAN_POINT ( 'NONE',  ( 4.487079325084206260, 1.670935625628103605, -0.8411387520786617333 ) ) ;
#80369 = CARTESIAN_POINT ( 'NONE',  ( -5.101610940492132151, 9.173906207207963348, -0.7998128361456362523 ) ) ;
#80368 = CARTESIAN_POINT ( 'NONE',  ( -1.500000000000013101, -0.2979166659838501929, 0.8660254037844403729 ) ) ;
#80367 = CARTESIAN_POINT ( 'NONE',  ( 1.002048865836258518, -0.8573748960705518396, 1.709468765625526521 ) ) ;
#80370 = CARTESIAN_POINT ( 'NONE',  ( 2.297764732281985633, 1.706874461811638044, 1.398895601573101111 ) ) ;
#80371 = CARTESIAN_POINT ( 'NONE',  ( 0.1399997263886003374, 0.002789056014650820314, -1.999853399661279063 ) ) ;
#80372 = CARTESIAN_POINT ( 'NONE',  ( 4.715538499454675403, 4.395883092318884522, 1.214306433183764966E-14 ) ) ;
#80373 = CARTESIAN_POINT ( 'NONE',  ( 6.983858524370782916, 7.320458831286981827, 0.7216878364870328300 ) ) ;
#80374 = CARTESIAN_POINT ( 'NONE',  ( -3.379006598303881059, 4.965260336153046516, -1.599625672291256295 ) ) ;
#80375 = CARTESIAN_POINT ( 'NONE',  ( -6.007671464186866928, 8.102312356341712984, 1.443375672974058777 ) ) ;
#80376 = CARTESIAN_POINT ( 'NONE',  ( 1.264844077314925652, -1.780367465076490019, -0.8468111885079774304 ) ) ;
#80377 = CARTESIAN_POINT ( 'NONE',  ( 0.9566253870459644482, 2.304745586553739400, -0.1165920040033379956 ) ) ;
#80378 = CARTESIAN_POINT ( 'NONE',  ( 2.049198471137442912, 1.708465938063120637, -0.9642302061752603404 ) ) ;
#80379 = CARTESIAN_POINT ( 'NONE',  ( 5.260619331934998755, -0.6897241169346832734, -1.943984935097947675 ) ) ;
#80380 = CARTESIAN_POINT ( 'NONE',  ( 4.853455804012222430, 5.725081861844796727, 1.082531754730560403 ) ) ;
#80381 = CARTESIAN_POINT ( 'NONE',  ( 3.854260808034858155, 7.718664386007802136, -0.7998128361456362523 ) ) ;
#80382 = ORIENTED_EDGE ( 'NONE', *, *, #183135, .F. ) ;
#80383 = CARTESIAN_POINT ( 'NONE',  ( 1.364683531249988535, 5.467708333674750953, -0.7879004041258300672 ) ) ;
#80384 = CARTESIAN_POINT ( 'NONE',  ( 10.85717823004580218, -6.836271227032193032, -0.3852658704378455479 ) ) ;
#80385 = CARTESIAN_POINT ( 'NONE',  ( 4.351804119862229037, 4.179452349368450115, -0.7216878364870188411 ) ) ;
#80386 = CARTESIAN_POINT ( 'NONE',  ( 0.3917816989358015034, -1.985425474602352525, 0.8787674391965931697 ) ) ;
#80388 = CARTESIAN_POINT ( 'NONE',  ( 5.558836782162522638, 7.518240855878357110, -1.384758111419039039 ) ) ;
#80387 = DIRECTION ( 'NONE',  ( -0.000000000000000000, 1.000000000000000000, -0.000000000000000000 ) ) ;
#80389 = DIRECTION ( 'NONE',  ( 1.276756478318932585E-15, -1.000000000000000000, 1.665334536937738262E-16 ) ) ;
#80390 = CARTESIAN_POINT ( 'NONE',  ( -1.737500000000000266, -1.808333333333332016, -3.009438278150923907 ) ) ;
#80391 = CARTESIAN_POINT ( 'NONE',  ( 2.266681450017640653, -1.708379500633325998, -0.7622673669660309237 ) ) ;
#80392 = CARTESIAN_POINT ( 'NONE',  ( 6.274726406708529325, -2.050348626090079840, -0.6846857035173321560 ) ) ;
#80393 = CARTESIAN_POINT ( 'NONE',  ( -5.609631208091558463, 6.340496262503443781, 1.197921296376257994 ) ) ;
#80395 = CARTESIAN_POINT ( 'NONE',  ( 6.727182134110203826, 2.985950691969770254, 2.264927069331075238 ) ) ;
#80394 = SURFACE_STYLE_FILL_AREA ( #96678 ) ;
#80396 = ADVANCED_FACE ( 'NONE', ( #72309 ), #85378, .T. ) ;
#80397 = CARTESIAN_POINT ( 'NONE',  ( -0.6823417656250003738, -0.5322916663252491576, -1.181850606188749264 ) ) ;
#80398 = CARTESIAN_POINT ( 'NONE',  ( 2.684119430630255820, 1.024705199231435993, 1.614373862881289590 ) ) ;
#80399 = CARTESIAN_POINT ( 'NONE',  ( 4.135448415848129500, -1.220878049459400039, -1.281573189658680612 ) ) ;
#80400 = CARTESIAN_POINT ( 'NONE',  ( 2.086439996564274146, -1.175226666667992914, 1.508458442701497315 ) ) ;
#80401 = CARTESIAN_POINT ( 'NONE',  ( -4.446184310277715213, 7.274633231044262516, -1.199719254218452047 ) ) ;
#80403 = CARTESIAN_POINT ( 'NONE',  ( 5.659766488261158024, 1.145116341927857384, 1.535488998638125047 ) ) ;
#80402 = CARTESIAN_POINT ( 'NONE',  ( 2.331613029862944941, -3.165258756643079430, -2.416022285627570820 ) ) ;
#80404 = CARTESIAN_POINT ( 'NONE',  ( 6.812958078942359386, -1.523254609455872322, 1.248309864861799401 ) ) ;
#80405 = CARTESIAN_POINT ( 'NONE',  ( -1.001543065824772872E-14, 4.462500000000024336, 1.732050807568877637 ) ) ;
#80406 = CARTESIAN_POINT ( 'NONE',  ( 2.496466685713152334, -1.086271176545396067, 1.821091972856798913 ) ) ;
#80407 = CARTESIAN_POINT ( 'NONE',  ( 4.715616592392388284, -1.834479983729628616, 0.3652084810651031743 ) ) ;
#80409 = VERTEX_POINT ( 'NONE', #134164 ) ;
#80408 = CARTESIAN_POINT ( 'NONE',  ( 0.4865809202317071813, -0.2202831055867389420, -1.812292406919484344 ) ) ;
#80411 = CARTESIAN_POINT ( 'NONE',  ( 0.000000000000000000, 12.22000000000000064, 0.000000000000000000 ) ) ;
#80410 = CARTESIAN_POINT ( 'NONE',  ( 4.125739685719872263, -2.112183141943014153, 0.6395159525410462065 ) ) ;
#80412 = CARTESIAN_POINT ( 'NONE',  ( -1.364683531250014514, -0.4697916663252449943, 0.7879004041258379498 ) ) ;
#80413 = CARTESIAN_POINT ( 'NONE',  ( 2.014201374223419272, 2.057289675485386216, -0.1496214851241447485 ) ) ;
#80414 = CARTESIAN_POINT ( 'NONE',  ( 4.774442650306744085, 8.721933525333202653, -0.7998128361456281477 ) ) ;
#80415 = CARTESIAN_POINT ( 'NONE',  ( -6.530223543276495235, 10.77034456713125188, -0.7998128361456291469 ) ) ;
#80416 = CARTESIAN_POINT ( 'NONE',  ( 10.24048609702354717, 10.84165528948263457, -0.7998128361456281477 ) ) ;
#80417 = CARTESIAN_POINT ( 'NONE',  ( 11.97929049433705551, 11.30000000000000249, -0.7046979865771820783 ) ) ;
#80418 = DIRECTION ( 'NONE',  ( 0.000000000000000000, 0.000000000000000000, -1.000000000000000000 ) ) ;
#80419 = CARTESIAN_POINT ( 'NONE',  ( 1.499999999999959588, 7.750000000000000000, -10.86128356754324820 ) ) ;
#80420 = VERTEX_POINT ( 'NONE', #100560 ) ;
#80421 = CARTESIAN_POINT ( 'NONE',  ( 4.510256325466165173, 2.069976601481211542, -0.04757507122059301263 ) ) ;
#80422 = CARTESIAN_POINT ( 'NONE',  ( 0.7499999999999902300, 5.316666666666685082, -1.299038105676658228 ) ) ;
#80423 = CARTESIAN_POINT ( 'NONE',  ( 1.493687833870473547, 1.635750924671933282, 1.413141523588061776 ) ) ;
#80424 = CARTESIAN_POINT ( 'NONE',  ( -6.290641498436300161, 6.895329709839009169, -0.7498213622291228786 ) ) ;
#80425 = CARTESIAN_POINT ( 'NONE',  ( 2.561199701127094830, -1.677907875943387639, 1.123823742627054312 ) ) ;
#80426 = CARTESIAN_POINT ( 'NONE',  ( 5.202472899321463728, 6.442273364155400195, -1.196158869778561673 ) ) ;
#80427 = VERTEX_POINT ( 'NONE', #71236 ) ;
#80428 = EDGE_CURVE ( 'NONE', #91093, #173456, #120090, .T. ) ;
#80430 = CARTESIAN_POINT ( 'NONE',  ( 8.134528978519385944, 8.592631351135175066, -0.7216878364870267237 ) ) ;
#80429 = CARTESIAN_POINT ( 'NONE',  ( -1.737500000000000266, -2.858333333333334281, -3.009438278150923907 ) ) ;
#80431 = CARTESIAN_POINT ( 'NONE',  ( 0.03132844593996673976, -5.600264386820933638, 10.94526678918448681 ) ) ;
#80432 = CARTESIAN_POINT ( 'NONE',  ( -5.139949632912262700, 5.169231791251960750, 0.7216878364870257245 ) ) ;
#80433 = CARTESIAN_POINT ( 'NONE',  ( 0.1105650446291406575, 1.931126588553159884, 0.5807481968119408977 ) ) ;
#80434 = CARTESIAN_POINT ( 'NONE',  ( 5.021103811603734535, -2.081066139062941023, 0.6872292908843835590 ) ) ;
#80435 =( BOUNDED_CURVE ( )  B_SPLINE_CURVE ( 2, ( #4346, #70413, #87764, #68288, #19550, #67216, #134421, #101883, #35804 ),
 .UNSPECIFIED., .F., .T. ) 
 B_SPLINE_CURVE_WITH_KNOTS ( ( 3, 2, 2, 2, 3 ),
 ( 0.3958333333333333703, 0.4027777777777777901, 0.4166666666666666852, 0.4305555555555555802, 0.4375000000000000000 ),
 .UNSPECIFIED. ) 
 CURVE ( )  GEOMETRIC_REPRESENTATION_ITEM ( )  RATIONAL_B_SPLINE_CURVE ( ( 0.9330127018922194093, 0.9330127018922196314, 1.000000000000000000, 0.8660254037844387076, 1.000000000000000000, 0.8660254037844387076, 1.000000000000000000, 0.9330127018922194093, 0.9330127018922194093 ) ) 
 REPRESENTATION_ITEM ( '' )  );
#80436 = CARTESIAN_POINT ( 'NONE',  ( -0.7499999999999972244, 4.889583334016150751, -1.299038105676652899 ) ) ;
#80437 = CARTESIAN_POINT ( 'NONE',  ( 4.957238921819991262, -1.637161358497842389, 0.9882132959125531357 ) ) ;
#80438 = CARTESIAN_POINT ( 'NONE',  ( -3.578462479003122976, 6.262291094557191684, 1.199719254218464037 ) ) ;
#80439 = CARTESIAN_POINT ( 'NONE',  ( 5.870317324592803310, 7.871789516823500144, -1.443375672974057666 ) ) ;
#80441 = CARTESIAN_POINT ( 'NONE',  ( 2.196888872880573551, 1.802427395782604247, 0.9040921628407010413 ) ) ;
#80440 = CARTESIAN_POINT ( 'NONE',  ( -7.822691444960696572, 12.07029775252209092, -0.7216878364870267237 ) ) ;
#80442 = CARTESIAN_POINT ( 'NONE',  ( -1.364683531250010295, 12.44270833367473372, 0.7879004041258445001 ) ) ;
#80443 = CARTESIAN_POINT ( 'NONE',  ( -5.002032328799064231, 4.800402236545811441, -0.7998128361456362523 ) ) ;
#80444 = CARTESIAN_POINT ( 'NONE',  ( 5.016472913109910614, 1.187476848380929928, -1.251119849200056366 ) ) ;
#80445 = CARTESIAN_POINT ( 'NONE',  ( 8.174640274396848483, 8.501778173076651512, 0.7998128361456291469 ) ) ;
#80446 = CARTESIAN_POINT ( 'NONE',  ( 10.23604278863759909, 11.04439746293979496, 0.000000000000000000 ) ) ;
#80447 = CARTESIAN_POINT ( 'NONE',  ( -6.772457744868586538, -7.185026885899632454, -6.662118508819935947 ) ) ;
#80448 = EDGE_CURVE ( 'NONE', #19237, #201806, #4548, .T. ) ;
#80449 = CARTESIAN_POINT ( 'NONE',  ( -1.445103857048130047, 8.688264192037886247, 2.625611233228264840 ) ) ;
#80450 = ORIENTED_EDGE ( 'NONE', *, *, #56226, .F. ) ;
#80452 = AXIS2_PLACEMENT_3D ( 'NONE', #144021, #32360, #61657 ) ;
#80451 = DIRECTION ( 'NONE',  ( -0.000000000000000000, -0.000000000000000000, -1.000000000000000000 ) ) ;
#80453 = ORIENTED_EDGE ( 'NONE', *, *, #106488, .F. ) ;
#80454 = CARTESIAN_POINT ( 'NONE',  ( 5.373626179778474565, 0.3473841915581803996, -1.777664473148509838 ) ) ;
#80455 = CARTESIAN_POINT ( 'NONE',  ( 5.825163275726873202, 6.825053905550038991, 1.199719254218452047 ) ) ;
#80456 = DIRECTION ( 'NONE',  ( 0.7592566023653005702, -0.6507913734559639396, 0.000000000000000000 ) ) ;
#80457 = CARTESIAN_POINT ( 'NONE',  ( 5.654893700716965732, 0.3597771647365927694, 1.775199357419085411 ) ) ;
#80458 = CARTESIAN_POINT ( 'NONE',  ( 5.180624093753221970, 9.058162186105164437, 0.000000000000000000 ) ) ;
#80459 = CARTESIAN_POINT ( 'NONE',  ( -11.89844258446856529, 9.771473106700385713, -1.560502987793169094 ) ) ;
#80460 = CARTESIAN_POINT ( 'NONE',  ( 3.398540877415173966, 1.727514402264049620, -1.348270469230819391 ) ) ;
#80462 = CARTESIAN_POINT ( 'NONE',  ( 9.240045382913317340, 10.73880668727576015, -1.199719254218446718 ) ) ;
#80461 = CARTESIAN_POINT ( 'NONE',  ( 0.2913577194270203785, -1.795273245208812485, 0.7915465721433642132 ) ) ;
#80463 = CARTESIAN_POINT ( 'NONE',  ( 3.673361179623610084, 1.389826993061950899, 1.318567953439080620 ) ) ;
#80464 = CARTESIAN_POINT ( 'NONE',  ( -1.499999999999995559, 8.673756432004008587, 2.614717076620615810 ) ) ;
#80465 = DIRECTION ( 'NONE',  ( 1.000000000000000000, -0.000000000000000000, -0.000000000000000000 ) ) ;
#80466 = CARTESIAN_POINT ( 'NONE',  ( 1.364683531249986537, -0.8447916663252468261, -0.7879004041258309554 ) ) ;
#80468 = ORIENTED_EDGE ( 'NONE', *, *, #94915, .T. ) ;
#80467 = CARTESIAN_POINT ( 'NONE',  ( 4.528060117284222308, 8.226561203566173930, 0.7216878364870438212 ) ) ;
#80469 = EDGE_CURVE ( 'NONE', #74826, #132173, #184078, .T. ) ;
#80470 = CARTESIAN_POINT ( 'NONE',  ( -9.381879110976678149, 11.00824238663667565, 1.082531754730558626 ) ) ;
#80471 = CARTESIAN_POINT ( 'NONE',  ( 2.219795081190904629, -2.096929600374438429, 0.5247480557022954351 ) ) ;
#80472 = CARTESIAN_POINT ( 'NONE',  ( -5.098748287191073203, 8.106234214101666780, 1.199719254218452935 ) ) ;
#80473 = CARTESIAN_POINT ( 'NONE',  ( 4.258142763143749399, 7.125527769379820242, 1.199719254218451159 ) ) ;
#80474 = CARTESIAN_POINT ( 'NONE',  ( 1.905030480050071251, 1.515927946353814892, 1.016894063925778635 ) ) ;
#80475 = CARTESIAN_POINT ( 'NONE',  ( -4.223528545856940042, 4.886203710709899006, -1.199719254218446718 ) ) ;
#80476 = EDGE_CURVE ( 'NONE', #21552, #39666, #166631, .T. ) ;
#80477 = CARTESIAN_POINT ( 'NONE',  ( 3.961776442328440506, 1.811803316853294765, -0.2231971713724384965 ) ) ;
#80478 = CARTESIAN_POINT ( 'NONE',  ( 12.51085889473690749, 7.557192264108227420, 4.121037430627751519 ) ) ;
#80479 = ORIENTED_EDGE ( 'NONE', *, *, #12043, .F. ) ;
#80480 = CARTESIAN_POINT ( 'NONE',  ( 3.314863512866594863, -1.493043793209645864, 1.284631214971102775 ) ) ;
#80481 = EDGE_LOOP ( 'NONE', ( #117897, #210864, #63016, #24583 ) ) ;
#80482 = CARTESIAN_POINT ( 'NONE',  ( 4.722180519508206054, 1.859554500701779745, 0.5601121866093302648 ) ) ;
#80483 = VERTEX_POINT ( 'NONE', #184992 ) ;
#80484 = CARTESIAN_POINT ( 'NONE',  ( -5.427006627220116286, 9.553534508390610469, -0.7998128361456362523 ) ) ;
#80486 = CARTESIAN_POINT ( 'NONE',  ( 5.572555445586866441, 0.8612648569810870125, 1.938019255899057658 ) ) ;
#80485 = CARTESIAN_POINT ( 'NONE',  ( 5.668190738965027897, 8.770583741171307679, -1.199719254218452047 ) ) ;
#80487 = DIRECTION ( 'NONE',  ( -0.000000000000000000, 1.000000000000000000, -0.000000000000000000 ) ) ;
#80488 = CARTESIAN_POINT ( 'NONE',  ( 2.824755571612533434, 1.383597569638248315, -1.320258682893655999 ) ) ;
#80489 = CARTESIAN_POINT ( 'NONE',  ( 5.125043568333415678, 6.701081866602433657, -1.409791652392645700 ) ) ;
#80490 = PLANE ( 'NONE',  #211947 ) ;
#80491 = ORIENTED_EDGE ( 'NONE', *, *, #41681, .T. ) ;
#80492 = CARTESIAN_POINT ( 'NONE',  ( 5.876533236880477240, 5.820653295974182129, 0.7998128361456352531 ) ) ;
#80493 = VECTOR ( 'NONE', #178248, 1000.000000000000000 ) ;
#80494 = CARTESIAN_POINT ( 'NONE',  ( 4.705731023397805579, 1.493295645070455535, 1.350234862845017592 ) ) ;
#80495 = CARTESIAN_POINT ( 'NONE',  ( -0.4820161904281213272, 2.981954314639482018, 1.941394296928433238 ) ) ;
#80496 = CARTESIAN_POINT ( 'NONE',  ( 5.215394836314163562, -0.2642288504575221464, 1.806346989861665087 ) ) ;
#80497 = CARTESIAN_POINT ( 'NONE',  ( 0.4321921490204432281, 1.190796696626210682, 1.693455153822187587 ) ) ;
#80498 = CARTESIAN_POINT ( 'NONE',  ( -8.514157279702036618, 9.035531035848267223, -0.7216878364870278340 ) ) ;
#80499 = CARTESIAN_POINT ( 'NONE',  ( -6.019435214058361794, 7.168094078216475040, 1.196694171119830008 ) ) ;
#80500 = CARTESIAN_POINT ( 'NONE',  ( 1.737500000000001155, -2.989583332377417690, 3.009438278150922130 ) ) ;
#80501 = CARTESIAN_POINT ( 'NONE',  ( 5.383624799460786647, 1.257121276536907750, 1.385457850027263182 ) ) ;
#80502 = CARTESIAN_POINT ( 'NONE',  ( 5.289652487626049115, 9.323011668872403845, 0.7998128361456462443 ) ) ;
#80503 = CARTESIAN_POINT ( 'NONE',  ( 1.854049621773927514, 5.499999999999998224, -0.7500000000000006661 ) ) ;
#80504 = CARTESIAN_POINT ( 'NONE',  ( -1.364683531250000748, 10.67187500034139802, 0.000000000000000000 ) ) ;
#80505 = CARTESIAN_POINT ( 'NONE',  ( -5.168682875307782254, 7.053215992657626110, -1.599625672291256295 ) ) ;
#80507 = CARTESIAN_POINT ( 'NONE',  ( -6.312203035614172286, 9.521931420595302953, -1.199719254218452047 ) ) ;
#80506 = CARTESIAN_POINT ( 'NONE',  ( -11.97178994924802353, 11.37999993797205178, -0.8322011300497250685 ) ) ;
#80508 = CARTESIAN_POINT ( 'NONE',  ( -4.069418662396130593, 7.899405539437467816, -0.7998128361456281477 ) ) ;
#80509 = AXIS2_PLACEMENT_3D ( 'NONE', #121500, #154986, #174454 ) ;
#80510 = CARTESIAN_POINT ( 'NONE',  ( 1.024380955673375393, 1.017105081308821379, 1.803069775380027995 ) ) ;
#80511 = CARTESIAN_POINT ( 'NONE',  ( 2.214611691679416072, 2.054518390865597954, 0.5110800211125585690 ) ) ;
#80512 = CARTESIAN_POINT ( 'NONE',  ( 6.740374924288304648, 11.01552117831172062, 1.040834085586084257E-14 ) ) ;
#80513 = DIRECTION ( 'NONE',  ( -1.000000000000000000, -0.000000000000000000, -5.551115123125765446E-17 ) ) ;
#80514 = CARTESIAN_POINT ( 'NONE',  ( 0.5320047819624426078, 1.129344350875445935, 1.613283618269464981 ) ) ;
#80515 = CARTESIAN_POINT ( 'NONE',  ( 4.363209728991265024, 7.389406413240373617, 1.150570763150955633 ) ) ;
#80516 = CARTESIAN_POINT ( 'NONE',  ( 4.528060117284229413, 7.266191989264828344, 1.082531754730558626 ) ) ;
#80518 = DIRECTION ( 'NONE',  ( -0.000000000000000000, -1.000000000000000000, -0.000000000000000000 ) ) ;
#80517 = CARTESIAN_POINT ( 'NONE',  ( 3.130865642711470276, -4.000192543527539613, -1.507748429708645199 ) ) ;
#80519 = CARTESIAN_POINT ( 'NONE',  ( 2.361634033267061561, 2.247686861432355077, -0.4490786020208848983 ) ) ;
#80520 = CARTESIAN_POINT ( 'NONE',  ( 0.6096330727367264002, -1.817201089070449971, 0.1759225495863714350 ) ) ;
#80521 = CARTESIAN_POINT ( 'NONE',  ( 2.724755696555291262, 1.382288352666941389, -1.321784923088549446 ) ) ;
#80522 = ORIENTED_EDGE ( 'NONE', *, *, #147028, .F. ) ;
#80523 = CARTESIAN_POINT ( 'NONE',  ( 8.080296363620359301, 8.529359967086321603, 1.040834085586084257E-14 ) ) ;
#80524 = CIRCLE ( 'NONE', #198166, 5.500000000000005329 ) ;
#80525 = CARTESIAN_POINT ( 'NONE',  ( 1.248292583380994136, 0.9887404755159521219, -1.753579541237253903 ) ) ;
#80526 = CARTESIAN_POINT ( 'NONE',  ( 1.270277045833507312, -0.8771146801004360283, -1.754798696806989078 ) ) ;
#80527 = CARTESIAN_POINT ( 'NONE',  ( -7.811469059767924605, 12.26513100303794168, -0.7998128361456281477 ) ) ;
#80528 = CARTESIAN_POINT ( 'NONE',  ( -7.335124800193271177, 8.516399340768996851, -1.199719254218452935 ) ) ;
#80529 = DIRECTION ( 'NONE',  ( 0.000000000000000000, 0.000000000000000000, 1.000000000000000000 ) ) ;
#80530 = EDGE_CURVE ( 'NONE', #167173, #50158, #152957, .T. ) ;
#80532 = CARTESIAN_POINT ( 'NONE',  ( 2.852158073610413513, 0.5945245674133512459, 1.667141438756434058 ) ) ;
#80531 = CARTESIAN_POINT ( 'NONE',  ( 3.890639641997388765, 1.766133395052928101, -1.118410975085604608 ) ) ;
#80533 = CARTESIAN_POINT ( 'NONE',  ( -3.501245407925418274, 15.99999999999932321, 11.28115623562629466 ) ) ;
#80535 = CARTESIAN_POINT ( 'NONE',  ( 6.527265088719197195, -1.491963682546100900, -1.740339723829595453 ) ) ;
#80534 = CARTESIAN_POINT ( 'NONE',  ( 1.499999999998155698, 8.627523663849286706, -2.580000000000244764 ) ) ;
#80536 = CARTESIAN_POINT ( 'NONE',  ( 4.329842768969596634, 1.707365525456190358, 0.3361313568818121156 ) ) ;
#80537 = VECTOR ( 'NONE', #142094, 1000.000000000000000 ) ;
#80538 = CARTESIAN_POINT ( 'NONE',  ( 8.727698198895078363, 11.20540053684285553, -1.599625672291257406 ) ) ;
#80539 = CARTESIAN_POINT ( 'NONE',  ( -7.461813752226491125, -6.074287852078599670, 6.844806938814765651 ) ) ;
#80540 = CARTESIAN_POINT ( 'NONE',  ( 4.587041898695760622, 1.066698363585473652, -1.366732696162711314 ) ) ;
#80541 = CARTESIAN_POINT ( 'NONE',  ( 4.844266001044335468, -1.027726779992131023, 1.912555630771580084 ) ) ;
#80542 = CARTESIAN_POINT ( 'NONE',  ( 4.009460741339333723, 5.700790169694431420, -1.599625672291256295 ) ) ;
#80543 = CARTESIAN_POINT ( 'NONE',  ( 5.489470343000498076, -0.4852711138302409077, 1.957169415941109047 ) ) ;
#80544 = CARTESIAN_POINT ( 'NONE',  ( 5.750000000000004441, 3.273043269275614537E-13, 2.052068128417940951 ) ) ;
#80545 = CARTESIAN_POINT ( 'NONE',  ( 1.499999999999989120, 5.035416667349487341, 0.8660254037844524744 ) ) ;
#80546 = CARTESIAN_POINT ( 'NONE',  ( 3.733351708207183428, -1.780342035418970736, 0.7362343730293962052 ) ) ;
#80547 = CARTESIAN_POINT ( 'NONE',  ( -6.009258394948636914E-15, 9.718750000682803147, -1.732050807568875195 ) ) ;
#80548 = CARTESIAN_POINT ( 'NONE',  ( 6.258078541936050065, 0.8512804341574469191, -2.052012918514530160 ) ) ;
#80549 = VERTEX_POINT ( 'NONE', #86449 ) ;
#80550 = CARTESIAN_POINT ( 'NONE',  ( 6.883263157960364254, 2.447565407927353220, 2.329071302269662080 ) ) ;
#80551 = CARTESIAN_POINT ( 'NONE',  ( 0.7499999999999885647, 3.316666666666689967, -1.299038105676658228 ) ) ;
#80552 = CARTESIAN_POINT ( 'NONE',  ( 5.986088515633498197, 6.942523675449257858, -1.199719254218446718 ) ) ;
#80553 = CARTESIAN_POINT ( 'NONE',  ( 1.313460851834074905, 1.813262283420258525, -1.282816764689881373 ) ) ;
#80554 = CARTESIAN_POINT ( 'NONE',  ( -1.420000000000001039, 6.280000000000042881, -2.873333333333329520 ) ) ;
#80555 = CARTESIAN_POINT ( 'NONE',  ( 7.049876689426101350, 9.247942109129029475, -1.443375672974057666 ) ) ;
#80556 = CARTESIAN_POINT ( 'NONE',  ( 0.3124725659141594503, 7.215207000027920259, 2.082817582596224515 ) ) ;
#80557 = CARTESIAN_POINT ( 'NONE',  ( 6.034787771858531435, 10.05468647722803865, 0.000000000000000000 ) ) ;
#80558 = CARTESIAN_POINT ( 'NONE',  ( -3.472296738875691346, 6.104744391113324120, 1.082531754730549967 ) ) ;
#80560 = CARTESIAN_POINT ( 'NONE',  ( 5.459457826130150515, 1.684308464339222100, 1.190431669587647567 ) ) ;
#80559 = CARTESIAN_POINT ( 'NONE',  ( -0.4288785890453234995, 3.049942316455299451, -0.4196807566834767078 ) ) ;
#80561 = CARTESIAN_POINT ( 'NONE',  ( 4.883600829025052548, 4.870158186716897042, -0.06686181454683927383 ) ) ;
#80562 = CARTESIAN_POINT ( 'NONE',  ( -4.334856428067329404, 6.080418470877079429, -1.599625672291256295 ) ) ;
#80563 = CARTESIAN_POINT ( 'NONE',  ( 0.7499999999999902300, 4.847916667349482012, -1.299038105676658228 ) ) ;
#80564 = CARTESIAN_POINT ( 'NONE',  ( 0.6823417656249882723, -0.6572916663252492686, 1.181850606188755259 ) ) ;
#80565 = CARTESIAN_POINT ( 'NONE',  ( 6.678970768140332304, -0.09217866350584581758, -1.868372134486769420 ) ) ;
#80566 = CARTESIAN_POINT ( 'NONE',  ( 5.396976841598324803, -0.7867719702298915374, -1.545497150229415251 ) ) ;
#80567 = CARTESIAN_POINT ( 'NONE',  ( 4.018918099032080526, -1.663992213871115178, 0.5101021115980988174 ) ) ;
#80568 = CARTESIAN_POINT ( 'NONE',  ( 2.822068529938852155, 6.444163718237301275, -0.7998128361456291469 ) ) ;
#80569 = CARTESIAN_POINT ( 'NONE',  ( 3.456809812625420975, -2.022294432149398080, -1.079448172897869540 ) ) ;
#80570 = CARTESIAN_POINT ( 'NONE',  ( -1.201851678989727383E-14, 5.509375000341415252, -1.575800808251660134 ) ) ;
#80571 = CARTESIAN_POINT ( 'NONE',  ( 1.569984571489828173, -1.747861548559765721, -0.5788160320587890650 ) ) ;
#80572 = FACE_OUTER_BOUND ( 'NONE', #201599, .T. ) ;
#80573 = CARTESIAN_POINT ( 'NONE',  ( -11.82065545612590363, 8.157852845329689018, 2.282521414035399321 ) ) ;
#80574 = CARTESIAN_POINT ( 'NONE',  ( 1.764397251013736234, -1.293498944356825664, 1.288518760371157201 ) ) ;
#80575 = ADVANCED_FACE ( 'NONE', ( #167695 ), #1962, .T. ) ;
#80576 = CARTESIAN_POINT ( 'NONE',  ( 2.742814741689561853, 2.006446121045248887, -0.2004354718553730264 ) ) ;
#80577 = CARTESIAN_POINT ( 'NONE',  ( 1.095947417326826212, -2.191629467406099430, 0.003159298377679310623 ) ) ;
#80578 = CARTESIAN_POINT ( 'NONE',  ( 10.08935753863141471, 13.93683245669168969, -7.381900748183195304 ) ) ;
#80579 = CARTESIAN_POINT ( 'NONE',  ( 4.032330418399681093, 1.128390736420165519, -1.777953997047557744 ) ) ;
#80580 = CARTESIAN_POINT ( 'NONE',  ( -6.177711549321182716, 10.35908057418338402, 0.7998128361456481317 ) ) ;
#80581 = CARTESIAN_POINT ( 'NONE',  ( 7.122954113691880806, 13.97688634340336833, 9.257467215448135889 ) ) ;
#80582 = CARTESIAN_POINT ( 'NONE',  ( 1.398975865466948632, 0.4019745351953528112, 2.030794141931663521 ) ) ;
#80583 = CARTESIAN_POINT ( 'NONE',  ( 5.705283713252285338, 5.550585841749444249, -0.7998128361456211532 ) ) ;
#80584 = CARTESIAN_POINT ( 'NONE',  ( -3.505400730386704341E-15, 2.703125000341406459, 1.570758158831794260 ) ) ;
#80586 = B_SPLINE_CURVE_WITH_KNOTS ( 'NONE', 3,
 ( #67583, #196560, #35103, #36174 ),
 .UNSPECIFIED., .F., .F.,
 ( 4, 4 ),
 ( 0.000000000000000000, 0.0005691741557773217965 ),
 .UNSPECIFIED. ) ;
#80585 = CARTESIAN_POINT ( 'NONE',  ( 3.879626234357834047, 0.2581020070546445888, -2.104639248629774251 ) ) ;
#80587 = CONTEXT_DEPENDENT_SHAPE_REPRESENTATION ( #47860, #62732 ) ;
#80588 = CARTESIAN_POINT ( 'NONE',  ( 6.076747101522134820, -1.735163100867884500, -0.5679748894881069265 ) ) ;
#80589 = ORIENTED_EDGE ( 'NONE', *, *, #57473, .F. ) ;
#80590 = CARTESIAN_POINT ( 'NONE',  ( -4.308458954092677651, 8.248562223075252220, -0.7998128361456362523 ) ) ;
#80591 = CARTESIAN_POINT ( 'NONE',  ( 9.317477881089539338, 11.89347683273640932, 1.599625672291279388 ) ) ;
#80592 = CARTESIAN_POINT ( 'NONE',  ( 5.180624093753221970, 9.058162186105164437, 0.000000000000000000 ) ) ;
#80593 = CARTESIAN_POINT ( 'NONE',  ( -3.474999999999998312, -3.427083332377419467, 2.006292185433951047 ) ) ;
#80594 = CARTESIAN_POINT ( 'NONE',  ( -4.554649539187067830, 7.401175998105142817, 1.199719254218464037 ) ) ;
#80595 = CARTESIAN_POINT ( 'NONE',  ( 2.847920605731304011, -1.359688658692468355, -1.493726022120341224 ) ) ;
#80596 = CARTESIAN_POINT ( 'NONE',  ( 0.7804679756576750060, -1.169858290841051307, 1.750926281551241415 ) ) ;
#80597 = CARTESIAN_POINT ( 'NONE',  ( -4.769436176957319695, 8.786368983084006601, 0.7998128361456281477 ) ) ;
#80598 = CARTESIAN_POINT ( 'NONE',  ( 7.865701674222579598, 12.32840238656838139, -0.7998128361456352531 ) ) ;
#80599 = CARTESIAN_POINT ( 'NONE',  ( 5.647250314520869452, 1.642094101250504146, -0.8754911610409812361 ) ) ;
#80600 = CARTESIAN_POINT ( 'NONE',  ( 8.697719238366680372, 10.10609285197134533, 1.199719254218462483 ) ) ;
#80601 = CARTESIAN_POINT ( 'NONE',  ( -0.4153311931459124362, 3.919672248384428404, 0.5000000000000073275 ) ) ;
#80602 = ORIENTED_EDGE ( 'NONE', *, *, #164742, .T. ) ;
#80603 = CARTESIAN_POINT ( 'NONE',  ( -4.176793841461789114, 7.030620694084159794, -1.199719254218455378 ) ) ;
#80604 = CARTESIAN_POINT ( 'NONE',  ( -8.487040972474682476, 12.84537220128841817, 0.7216878364870338292 ) ) ;
#80605 =( GEOMETRIC_REPRESENTATION_CONTEXT ( 3 ) GLOBAL_UNCERTAINTY_ASSIGNED_CONTEXT ( ( #28371 ) ) GLOBAL_UNIT_ASSIGNED_CONTEXT ( ( #141855, #191605, #116556 ) ) REPRESENTATION_CONTEXT ( 'NONE', 'WORKASPACE' ) );
#80607 = CARTESIAN_POINT ( 'NONE',  ( 1.838261372102001800, -1.052240823716396267, 1.655630454418555830 ) ) ;
#80606 = CARTESIAN_POINT ( 'NONE',  ( -5.831978632172702071, 9.955725504176825780, 0.7998128361456481317 ) ) ;
#80608 = CARTESIAN_POINT ( 'NONE',  ( 6.807514186891733488, -0.4511856701074740683, 2.018123631040650068 ) ) ;
#80609 = VECTOR ( 'NONE', #23110, 1000.000000000000000 ) ;
#80611 = CARTESIAN_POINT ( 'NONE',  ( -5.641245921709659328, 6.318796091258308323, 1.170641968482153850 ) ) ;
#80610 = CARTESIAN_POINT ( 'NONE',  ( -6.798487682609798632, 6.896266815991691779, 0.7998128361456341429 ) ) ;
#80612 = CARTESIAN_POINT ( 'NONE',  ( 1.364683531249986537, 0.3635416670080869328, 0.7879004041258500513 ) ) ;
#80613 = CARTESIAN_POINT ( 'NONE',  ( 2.653305042933405300, -0.2923731341353021373, -1.708803492460549744 ) ) ;
#80614 = CARTESIAN_POINT ( 'NONE',  ( 1.165484214331854895, -1.106714608479087092, 1.343107696387570549 ) ) ;
#80616 = CARTESIAN_POINT ( 'NONE',  ( 7.619319141200072920, 7.991553207595983643, 0.7216878364870317197 ) ) ;
#80615 = CARTESIAN_POINT ( 'NONE',  ( 6.147156021580305385, -1.953063626952681542, 1.228987080356194195 ) ) ;
#80617 = CARTESIAN_POINT ( 'NONE',  ( -11.80100919632472589, 4.809168931535662495, -4.927235675632552159 ) ) ;
#80618 = CARTESIAN_POINT ( 'NONE',  ( 2.882161881593125585, -1.062215874558822826, 1.765801728998709352 ) ) ;
#80619 = CARTESIAN_POINT ( 'NONE',  ( 5.681030059326015014, 6.586622143090519188, -1.199719254218445830 ) ) ;
#80620 = EDGE_CURVE ( 'NONE', #86803, #211691, #166870, .T. ) ;
#80621 = EDGE_CURVE ( 'NONE', #119003, #50845, #132498, .T. ) ;
#80622 = CARTESIAN_POINT ( 'NONE',  ( 1.423203639035979906, 0.8144988626696235690, 1.844428818423976546 ) ) ;
#80623 = CARTESIAN_POINT ( 'NONE',  ( 6.825078400183544503, 6.034152930826206962, 2.739236550662868197 ) ) ;
#80624 = CARTESIAN_POINT ( 'NONE',  ( -5.418418667316934112, 6.350518529071726981, -1.199719254218453823 ) ) ;
#80625 = CARTESIAN_POINT ( 'NONE',  ( 0.7957029915596275371, -0.7116629262611442464, 1.838703523458279143 ) ) ;
#80627 = CARTESIAN_POINT ( 'NONE',  ( -6.292392690518223475, 6.513748691792265788, -0.7216878364870338292 ) ) ;
#80626 = CARTESIAN_POINT ( 'NONE',  ( 4.148624843374196125, 1.876505540506741010, 0.3678670841067502861 ) ) ;
#80628 = CARTESIAN_POINT ( 'NONE',  ( -7.241463443030476732, 7.620997903056574430, 0.000000000000000000 ) ) ;
#80629 = CARTESIAN_POINT ( 'NONE',  ( 6.526270840131753737, 8.707344961610770540, -1.599625672291283607 ) ) ;
#80630 = CARTESIAN_POINT ( 'NONE',  ( -6.770317605177755382, 8.992066187497757213, 1.599625672291269396 ) ) ;
#80631 = CARTESIAN_POINT ( 'NONE',  ( 0.6803390939152150763, 0.9973279206440927025, 1.756184504224398202 ) ) ;
#80632 = CARTESIAN_POINT ( 'NONE',  ( 0.000000000000000000, 14.48195938056239385, 0.000000000000000000 ) ) ;
#80633 = CARTESIAN_POINT ( 'NONE',  ( 4.190657675959572614, -2.281913287836007331, -0.3425691479843806508 ) ) ;
#80634 = CARTESIAN_POINT ( 'NONE',  ( 5.441838459065293065, 1.316327937319297758, 1.454900926449454124 ) ) ;
#80635 = EDGE_CURVE ( 'NONE', #146910, #126115, #184389, .T. ) ;
#80636 = CARTESIAN_POINT ( 'NONE',  ( 1.639427129605858902, 1.814645582613241714, -0.7458448512465406521 ) ) ;
#80637 = CARTESIAN_POINT ( 'NONE',  ( -4.959585264500673496, 4.680604318205876524, 1.214306433183764966E-14 ) ) ;
#80638 = CARTESIAN_POINT ( 'NONE',  ( -0.03452862918938356951, -1.956592590566148093, -0.4871966601913205186 ) ) ;
#80639 = ORIENTED_EDGE ( 'NONE', *, *, #24646, .F. ) ;
#80640 = CARTESIAN_POINT ( 'NONE',  ( 1.446650934045516701, -1.493148645901293925, 1.501467539593546840 ) ) ;
#80642 = CARTESIAN_POINT ( 'NONE',  ( -6.723954117373590833, 9.932031339322813679, -1.199719254218440723 ) ) ;
#80641 = CARTESIAN_POINT ( 'NONE',  ( -5.610376637956639101, 5.439860920571172542, 0.000000000000000000 ) ) ;
#80643 = CARTESIAN_POINT ( 'NONE',  ( 1.165666007907351309, -1.169451938622353859, 1.422036577929463030 ) ) ;
#80644 = VERTEX_POINT ( 'NONE', #202300 ) ;
#80645 = CARTESIAN_POINT ( 'NONE',  ( 4.645498245716852992, 1.942073188235559522, -0.9706016350095565404 ) ) ;
#80646 = CARTESIAN_POINT ( 'NONE',  ( 11.46937510643195779, 8.378953184613939342, -3.376433863712082761 ) ) ;
#80647 = CARTESIAN_POINT ( 'NONE',  ( 2.144932638433934002, 2.058100890041581810, 0.5106320605416380110 ) ) ;
#80648 = CARTESIAN_POINT ( 'NONE',  ( 1.499999999999989120, 3.056250000682818158, 1.214306433183764966E-14 ) ) ;
#80649 = CARTESIAN_POINT ( 'NONE',  ( 9.023114925094663619, 10.48572115315399245, 1.199719254218453823 ) ) ;
#80650 = CARTESIAN_POINT ( 'NONE',  ( 11.84668730067608244, 13.40000000000000036, -1.320000000000001616 ) ) ;
#80651 = CARTESIAN_POINT ( 'NONE',  ( 3.462233735546389468, 0.9232262379769129446, 1.842458217425169131 ) ) ;
#80652 = VECTOR ( 'NONE', #86348, 1000.000000000000000 ) ;
#80654 = CARTESIAN_POINT ( 'NONE',  ( 0.1691535571452691677, 1.059206136818511501, 1.505872603892892458 ) ) ;
#80653 = CARTESIAN_POINT ( 'NONE',  ( -8.910733272679575379, 11.41894145625809820, -1.599625672291263179 ) ) ;
#80655 = CARTESIAN_POINT ( 'NONE',  ( -0.6823417656249969321, 3.717708333674754506, -1.181850606188749264 ) ) ;
#80656 = CARTESIAN_POINT ( 'NONE',  ( -0.02244404828160086532, 2.859736408857795009, -2.677210243787793598 ) ) ;
#80657 = CARTESIAN_POINT ( 'NONE',  ( 1.449495214452817038, 4.332601206217148615, -0.3909641857570877455 ) ) ;
#80658 = CARTESIAN_POINT ( 'NONE',  ( 0.4521680116954321371, 0.6883007682146925488, -2.096869779678663281 ) ) ;
#80659 = CARTESIAN_POINT ( 'NONE',  ( 0.9840795919474578657, 1.519885296779641681, 1.676025758627389450 ) ) ;
#80660 = CARTESIAN_POINT ( 'NONE',  ( -8.324343129110692630, 12.65555805069709550, 0.7216878364870338292 ) ) ;
#80661 = CARTESIAN_POINT ( 'NONE',  ( 2.355456482938292240, -1.344675202547132464, -1.214172642412311598 ) ) ;
#80662 = CARTESIAN_POINT ( 'NONE',  ( 1.622146050056040512, 1.895417417167859497, 0.2770879218524437415 ) ) ;
#80663 = CARTESIAN_POINT ( 'NONE',  ( 3.016144355299533952, 2.060630728401948275, -0.2003171163396169074 ) ) ;
#80664 = CARTESIAN_POINT ( 'NONE',  ( 1.364683531249988757, 0.9468750003414211358, 0.000000000000000000 ) ) ;
#80665 = CARTESIAN_POINT ( 'NONE',  ( 1.235163454902254765, -1.783154728128878652, 0.8411200730164528627 ) ) ;
#80666 = CARTESIAN_POINT ( 'NONE',  ( 6.586557377926046897, -1.889895688126231876, -0.3729288831034789364 ) ) ;
#80667 = CARTESIAN_POINT ( 'NONE',  ( 3.274138816734498025, -1.115311402298941656, 1.501645261301733481 ) ) ;
#80669 = CARTESIAN_POINT ( 'NONE',  ( 5.364009635805341958, 7.578432035813580825, -1.241402483855597039 ) ) ;
#80668 = CARTESIAN_POINT ( 'NONE',  ( 0.8038796212130067120, 1.889748380504801650, 1.324265523043531845 ) ) ;
#80670 = CARTESIAN_POINT ( 'NONE',  ( 3.015880874418576330, 1.852360388558017545, -0.1794404841957262797 ) ) ;
#80671 = CARTESIAN_POINT ( 'NONE',  ( 0.6823417656249899377, 2.842708333674753618, 1.181850606188765695 ) ) ;
#80672 = CARTESIAN_POINT ( 'NONE',  ( 4.896965771356657449, 0.3494220250804170314, 2.032713711554866354 ) ) ;
#80673 = AXIS2_PLACEMENT_3D ( 'NONE', #22487, #6238, #37701 ) ;
#80674 = CARTESIAN_POINT ( 'NONE',  ( -4.550733115681270036, 8.460939068270139529, 0.7998128361456481317 ) ) ;
#80675 = CARTESIAN_POINT ( 'NONE',  ( 11.00592705432737972, 13.61019307346892759, 1.444010445236424856 ) ) ;
#80676 = CARTESIAN_POINT ( 'NONE',  ( 6.141652715049399802, -1.522797514780509065, -1.454946885519771582 ) ) ;
#80677 = CARTESIAN_POINT ( 'NONE',  ( -1.364683531250012516, 3.051041667008083547, -0.7879004041258289570 ) ) ;
#80678 = CARTESIAN_POINT ( 'NONE',  ( 6.520800673124607982, 2.014292100380775885, 0.7847517145297827623 ) ) ;
#80679 = CARTESIAN_POINT ( 'NONE',  ( 1.083273795380396143, -0.8277460070302902206, 1.644747122058511035 ) ) ;
#80680 = CARTESIAN_POINT ( 'NONE',  ( 5.162762804107727810, 0.5884847259931770269, 1.932018068032066438 ) ) ;
#80681 = CARTESIAN_POINT ( 'NONE',  ( -4.596923820214036560, 8.483565078729160547, 0.2266403168418751335 ) ) ;
#80682 = CARTESIAN_POINT ( 'NONE',  ( -4.609409038966234995, 7.361099064560491456, -1.082531754730549967 ) ) ;
#80683 = EDGE_CURVE ( 'NONE', #211122, #27064, #93171, .T. ) ;
#80684 = CIRCLE ( 'NONE', #7987, 0.08000000000000020983 ) ;
#80687 = CARTESIAN_POINT ( 'NONE',  ( 3.701012746850603996, 7.261672604726938651, 1.040834085586084257E-14 ) ) ;
#80686 = CARTESIAN_POINT ( 'NONE',  ( 3.285556943750000514, -1.713541666188707735, 1.896917185911906500 ) ) ;
#80685 = CARTESIAN_POINT ( 'NONE',  ( 7.700104897918568447, 7.948153567185284096, 0.000000000000000000 ) ) ;
#80688 = CARTESIAN_POINT ( 'NONE',  ( -6.168033539574333979, 6.160736982450306876, 0.7998128361456281477 ) ) ;
#80689 = CARTESIAN_POINT ( 'NONE',  ( 3.819546216251490822, -1.394084564108012403, -1.457236891723237449 ) ) ;
#80690 = CARTESIAN_POINT ( 'NONE',  ( -7.340850106795412167, 10.65174332698158643, 1.199719254218453823 ) ) ;
#80692 = CARTESIAN_POINT ( 'NONE',  ( -6.224601922005509991, 10.27613631906616476, 0.7216878364870267237 ) ) ;
#80691 = CARTESIAN_POINT ( 'NONE',  ( -3.789667630219657912, 4.380032642466370696, 1.199719254218462483 ) ) ;
#80693 = DIRECTION ( 'NONE',  ( 0.000000000000000000, 0.000000000000000000, -1.000000000000000000 ) ) ;
#80695 = CARTESIAN_POINT ( 'NONE',  ( 0.6823417656249969321, 9.526041667008065872, -1.181850606188757036 ) ) ;
#80694 = CARTESIAN_POINT ( 'NONE',  ( 6.473507614529132148, 2.070149491355821159, -0.6224772505839873959 ) ) ;
#80696 = CARTESIAN_POINT ( 'NONE',  ( 0.000000000000000000, 13.49999999999999822, -1.500000000000000222 ) ) ;
#80697 = CARTESIAN_POINT ( 'NONE',  ( -11.81798298708319273, 7.794783740815080186, -1.819802677367790444 ) ) ;
#80699 = CARTESIAN_POINT ( 'NONE',  ( 5.150017624212761547, 0.9963180513538304472, 1.753022482293864481 ) ) ;
#80698 = CARTESIAN_POINT ( 'NONE',  ( -6.521108698048783126, 7.670676904887464786, -1.082531754730543083 ) ) ;
#80700 = CARTESIAN_POINT ( 'NONE',  ( -1.402160292154681736E-14, -0.4906249996585810846, -1.575800808251665908 ) ) ;
#80701 = VECTOR ( 'NONE', #170354, 1000.000000000000000 ) ;
#80702 = CARTESIAN_POINT ( 'NONE',  ( 1.875234852168044641, 1.651158054356154148, -0.4988350824523117844 ) ) ;
#80703 = CARTESIAN_POINT ( 'NONE',  ( 5.923986774528332333, 5.876015756563318426, -0.7998128361456481317 ) ) ;
#80705 = CARTESIAN_POINT ( 'NONE',  ( 6.481679955784983349, 9.719654494127929922, -1.199719254218452047 ) ) ;
#80704 = CARTESIAN_POINT ( 'NONE',  ( 6.805829924380108586, 8.963220883242035697, 1.443375672974076540 ) ) ;
#80706 = CARTESIAN_POINT ( 'NONE',  ( -10.52211599421016786, 5.354012650763439574, -5.769493145238611120 ) ) ;
#80707 = CARTESIAN_POINT ( 'NONE',  ( 0.2448899766094528307, -1.362147681959727574, -1.129672978174221631 ) ) ;
#80708 = CARTESIAN_POINT ( 'NONE',  ( 1.295565486743395889, 1.859180707359459284, -0.7724582428273608636 ) ) ;
#80709 = DIRECTION ( 'NONE',  ( -0.8660254037844411501, -0.4999999999999956146, 5.551115123125779621E-17 ) ) ;
#80710 = CARTESIAN_POINT ( 'NONE',  ( 2.784424029790978139, -1.135345490304447091, 1.892179603154810597 ) ) ;
#80711 = CARTESIAN_POINT ( 'NONE',  ( 5.629782814718605977, 2.094415894289668678, -0.5717063696269225614 ) ) ;
#80712 = ORIENTED_EDGE ( 'NONE', *, *, #48284, .T. ) ;
#80713 = CARTESIAN_POINT ( 'NONE',  ( 4.706615602599436343, 5.520081620234675412, 1.199719254218452935 ) ) ;
#80715 = CARTESIAN_POINT ( 'NONE',  ( 1.423454079394898653, -1.462460055423293825, -1.388472309132340099 ) ) ;
#80714 = CARTESIAN_POINT ( 'NONE',  ( 3.528090983593739516, -2.088826311502915090, 0.3641918842257965139 ) ) ;
#80716 = CARTESIAN_POINT ( 'NONE',  ( 2.548825626188336635, 0.2254045845835982720, 1.797452833117135329 ) ) ;
#80717 = CARTESIAN_POINT ( 'NONE',  ( 4.525389411911321602, 8.501647757197021704, -0.7998128361456381397 ) ) ;
#80718 = VERTEX_POINT ( 'NONE', #156801 ) ;
#80719 = CARTESIAN_POINT ( 'NONE',  ( 6.205881626753210867, 8.263281202677319470, 1.599625672291281386 ) ) ;
#80721 = CARTESIAN_POINT ( 'NONE',  ( 1.059628844421168559, 1.143981278108822108, 1.536452684808758962 ) ) ;
#80720 = CARTESIAN_POINT ( 'NONE',  ( -3.632695093457760649, 6.325562478087638496, -1.199719254218452047 ) ) ;
#80722 = CARTESIAN_POINT ( 'NONE',  ( -10.95308175811721085, 9.799999999999998934, -1.800000000000001155 ) ) ;
#80723 = CARTESIAN_POINT ( 'NONE',  ( -4.887223063278990587, 4.917640739834122421, -0.4608172110749644834 ) ) ;
#80724 = CARTESIAN_POINT ( 'NONE',  ( 4.324687812634874895, 7.989293514808604613, 0.7216878364870317197 ) ) ;
#80725 = CARTESIAN_POINT ( 'NONE',  ( -0.6823417656250246877, 0.1135416670080893753, 1.181850606188755259 ) ) ;
#80726 = CARTESIAN_POINT ( 'NONE',  ( 11.84668730067608600, 10.89999999999998259, 1.319999999999998286 ) ) ;
#80727 = CARTESIAN_POINT ( 'NONE',  ( -9.806625181386236179, 10.33548422123910449, -0.7998128361456291469 ) ) ;
#80728 = EDGE_CURVE ( 'NONE', #127020, #24518, #209355, .T. ) ;
#80729 = CARTESIAN_POINT ( 'NONE',  ( 4.768538688506021472, -1.414568798902924307, 1.634688457493836289 ) ) ;
#80730 = CARTESIAN_POINT ( 'NONE',  ( -4.177320726786315497, 7.887641591310407208, -0.7216878364870458196 ) ) ;
#80731 = CARTESIAN_POINT ( 'NONE',  ( 6.224601922449876312, 6.434659462379210382, 0.000000000000000000 ) ) ;
#80732 = CARTESIAN_POINT ( 'NONE',  ( 2.109781586379317897, 1.642293606977158538, 1.341614810521203349 ) ) ;
#80734 = CARTESIAN_POINT ( 'NONE',  ( -11.88731729969462059, 7.000411858491159656, -4.404230128874679906 ) ) ;
#80733 = DIRECTION ( 'NONE',  ( 1.214306433183764966E-17, 1.000000000000000000, 5.200010849845536803E-32 ) ) ;
#80735 = CARTESIAN_POINT ( 'NONE',  ( 3.444560810740458390, 0.4755345817112103246, 1.913044316819292767 ) ) ;
#80736 = CARTESIAN_POINT ( 'NONE',  ( 5.871340715825057011, -1.643613990083541143, -0.9773822251149253404 ) ) ;
#80737 = VERTEX_POINT ( 'NONE', #159987 ) ;
#80739 = EDGE_CURVE ( 'NONE', #96695, #44793, #103507, .T. ) ;
#80738 = CARTESIAN_POINT ( 'NONE',  ( -1.201851678989727383E-14, 4.587500000000024336, -1.732050807568863648 ) ) ;
#80740 = CARTESIAN_POINT ( 'NONE',  ( 0.4146172280090759665, 0.7909515328246279342, 1.913518691844050323 ) ) ;
#80741 = CARTESIAN_POINT ( 'NONE',  ( 1.816251609031571457, 1.811968324836669142, 0.6989759121980871903 ) ) ;
#80742 = ORIENTED_EDGE ( 'NONE', *, *, #107910, .T. ) ;
#80743 = CARTESIAN_POINT ( 'NONE',  ( -3.471769853551161411, 6.208092708188416076, 1.199719254218452935 ) ) ;
#80745 = CARTESIAN_POINT ( 'NONE',  ( 6.393551957296131683, 9.616838495890963401, 1.199719254218452047 ) ) ;
#80744 = CARTESIAN_POINT ( 'NONE',  ( -7.268579750702168774, 7.652633595340216921, -0.7216878364870338292 ) ) ;
#80747 = CARTESIAN_POINT ( 'NONE',  ( 7.145310649601935182, 8.294949498412453437, -1.199719254218446718 ) ) ;
#80746 = CARTESIAN_POINT ( 'NONE',  ( 2.273483640244071680, 1.287084957891961423, 1.647379119656503965 ) ) ;
#80748 = CARTESIAN_POINT ( 'NONE',  ( 6.360183458142179447, 6.592837920686898556, -0.7216878364870458196 ) ) ;
#80750 = EDGE_LOOP ( 'NONE', ( #98916, #153350, #155326, #44968 ) ) ;
#80749 = CARTESIAN_POINT ( 'NONE',  ( 5.953752735127215701, -1.388294428863137586, -1.315342447896154843 ) ) ;
#80751 = CARTESIAN_POINT ( 'NONE',  ( 4.424592250794217030, 1.359014646446855767, -1.738718759629573896 ) ) ;
#80752 = CARTESIAN_POINT ( 'NONE',  ( 2.837189949676882428, 0.2689455771197127310, 2.190246129917215789 ) ) ;
#80753 = CARTESIAN_POINT ( 'NONE',  ( -11.92619526913700057, 12.69999999999998153, 1.328859060402682868 ) ) ;
#80754 = CARTESIAN_POINT ( 'NONE',  ( 1.805181101471531546, 1.663141274854248230, -0.9436981260437929953 ) ) ;
#80755 = CARTESIAN_POINT ( 'NONE',  ( 11.04536101718726293, 0.000000000000000000, -1.100000000000002087 ) ) ;
#80756 = CARTESIAN_POINT ( 'NONE',  ( 0.000000000000000000, -0.8934598047668927956, -3.291472234583660672 ) ) ;
#80757 = CARTESIAN_POINT ( 'NONE',  ( 4.193848433072798088, -1.425472641756184489, -1.501718461524886195 ) ) ;
#80758 = AXIS2_PLACEMENT_3D ( 'NONE', #16931, #132877, #83011 ) ;
#80760 = CARTESIAN_POINT ( 'NONE',  ( 1.674925575805393585, -2.052671086741376882, -0.6780288057936025847 ) ) ;
#80759 = CARTESIAN_POINT ( 'NONE',  ( -3.277320446201389181, 4.846626492033466072, 1.599625672291267398 ) ) ;
#80761 = CARTESIAN_POINT ( 'NONE',  ( 3.368858348882136422, 0.05182064297618373117, -2.191103300807801801 ) ) ;
#80762 = CARTESIAN_POINT ( 'NONE',  ( -5.842658511366215279, 6.642451456931087073, 0.9392888627727929984 ) ) ;
#80763 = CARTESIAN_POINT ( 'NONE',  ( 0.9311234436981489226, -2.303119629485602005, 3.475000000000000533 ) ) ;
#80764 = CARTESIAN_POINT ( 'NONE',  ( -5.975952631313489860, 15.44727933881517323, 10.36472687262296510 ) ) ;
#80765 = CARTESIAN_POINT ( 'NONE',  ( 6.412080304620304538, 6.445458208337293549, -0.7998128361456481317 ) ) ;
#80766 = CARTESIAN_POINT ( 'NONE',  ( 1.364683531250000303, 14.31770833367473372, -0.7879004041258355073 ) ) ;
#80767 = CARTESIAN_POINT ( 'NONE',  ( -5.178288325776719603, 5.006034233019745372, 0.000000000000000000 ) ) ;
#80768 = UNCERTAINTY_MEASURE_WITH_UNIT (LENGTH_MEASURE( 1.000000000000000082E-05 ), #78182, 'distance_accuracy_value', 'NONE');
#80769 = CARTESIAN_POINT ( 'NONE',  ( 0.1764080092822375156, 1.496053712750060383, 1.352152247781977179 ) ) ;
#80770 = EDGE_CURVE ( 'NONE', #175679, #140850, #123955, .T. ) ;
#80771 = CIRCLE ( 'NONE', #66962, 0.07999999999999990452 ) ;
#80772 = CARTESIAN_POINT ( 'NONE',  ( -8.487040972474682476, 12.84537220128841817, 0.7216878364870338292 ) ) ;
#80773 = CARTESIAN_POINT ( 'NONE',  ( 4.522371119077151391, 0.9712943915625820157, 1.828230030883712498 ) ) ;
#80774 = CARTESIAN_POINT ( 'NONE',  ( 2.754421912756400026, 0.6492094756798562072, 1.813941749866236242 ) ) ;
#80775 = CARTESIAN_POINT ( 'NONE',  ( 6.187133403942106646, 1.760427041935657799, 1.175965560660442444 ) ) ;
#80776 = CARTESIAN_POINT ( 'NONE',  ( 5.769158057814842699, 6.689438141327490150, 1.199719254218462483 ) ) ;
#80777 = CARTESIAN_POINT ( 'NONE',  ( 9.405838923370410498, 3.553052382342013704, 7.381490207074219434 ) ) ;
#80778 = CARTESIAN_POINT ( 'NONE',  ( 3.942214172571806508, -0.9744538365985645489, 1.711425102584500202 ) ) ;
#80779 = CARTESIAN_POINT ( 'NONE',  ( 5.472717818731657857, -0.05164252020756903566, -2.291847404020570966 ) ) ;
#80780 = CARTESIAN_POINT ( 'NONE',  ( 4.529811765687052016, -1.125283923072720071, -1.437579299059896343 ) ) ;
#80781 = CARTESIAN_POINT ( 'NONE',  ( 5.397554552016204710, 9.311247720745345902, 0.7216878364870317197 ) ) ;
#80782 = CARTESIAN_POINT ( 'NONE',  ( 4.324687812634887329, 6.068555086205916105, 1.443375672974062551 ) ) ;
#80783 = CARTESIAN_POINT ( 'NONE',  ( -6.740338644649361832, 7.892758502626242567, -1.199719254218452047 ) ) ;
#80784 = CARTESIAN_POINT ( 'NONE',  ( 6.364626766972446781, 6.390095747748157251, 0.7998128361456352531 ) ) ;
#80785 = ORIENTED_EDGE ( 'NONE', *, *, #125818, .F. ) ;
#80786 = CARTESIAN_POINT ( 'NONE',  ( 4.957293921627444533, -1.724444360862188885, 1.038707789177233831 ) ) ;
#80787 = CARTESIAN_POINT ( 'NONE',  ( 6.170549959107765936, 1.581869261771509994, 1.668023173554062266 ) ) ;
#80788 = CARTESIAN_POINT ( 'NONE',  ( 5.770351633785986145, -0.8788013674413885923, -1.753946858050984048 ) ) ;
#80789 = CARTESIAN_POINT ( 'NONE',  ( -7.867809214632013770, 8.073532260025807261, 1.040834085586084257E-14 ) ) ;
#80790 = CARTESIAN_POINT ( 'NONE',  ( -4.192495815123836955, 5.914331089109674089, -1.599625672291256295 ) ) ;
#80791 = CARTESIAN_POINT ( 'NONE',  ( -7.721398836998370818, -5.907420853759296264, 7.721398836998400128 ) ) ;
#80792 = CARTESIAN_POINT ( 'NONE',  ( -4.938913097128142304, 8.984092056616635347, -0.7998128361456362523 ) ) ;
#80794 = CARTESIAN_POINT ( 'NONE',  ( 6.702016551492756768, -1.769339222028827319, 0.04870252428828580893 ) ) ;
#80793 = CARTESIAN_POINT ( 'NONE',  ( 1.136401537022444508, 0.4113854086121961351, 2.049693714879106121 ) ) ;
#80795 = LINE ( 'NONE', #48311, #67532 ) ;
#80796 = CARTESIAN_POINT ( 'NONE',  ( 6.421825219014824171, 1.115965409679237963, -1.589096094497045142 ) ) ;
#80797 = CARTESIAN_POINT ( 'NONE',  ( -1.364683531249997417, 3.321875000341423245, 1.214306433183764966E-14 ) ) ;
#80798 = CARTESIAN_POINT ( 'NONE',  ( 0.8369945909703061515, 0.7069334548283608965, -1.590575932886540755 ) ) ;
#80799 = CARTESIAN_POINT ( 'NONE',  ( 4.964256800898067645, 8.943383367689749619, 0.7998128361456462443 ) ) ;
#80800 = DIRECTION ( 'NONE',  ( 0.000000000000000000, 0.000000000000000000, 1.000000000000000000 ) ) ;
#80801 = CARTESIAN_POINT ( 'NONE',  ( 1.277515311556869593, 1.024738337535425758, 1.387312573235904845 ) ) ;
#80802 = CARTESIAN_POINT ( 'NONE',  ( 1.206853476500208133, 1.935082376036290075, 1.028754739392373496 ) ) ;
#80803 = CARTESIAN_POINT ( 'NONE',  ( 4.125739685719872263, -2.112183141943014153, 0.6395159525410462065 ) ) ;
#80804 = CARTESIAN_POINT ( 'NONE',  ( 1.850661656762859542, -2.160338676232275823, -0.2159047328044171599 ) ) ;
#80805 = CARTESIAN_POINT ( 'NONE',  ( -1.499999999999946709, 7.750000000000000000, 15.75000000000000711 ) ) ;
#80806 = CARTESIAN_POINT ( 'NONE',  ( 2.483745868283081748, -0.6592627125163934565, 2.012192174959149149 ) ) ;
#80807 = CARTESIAN_POINT ( 'NONE',  ( 6.539320575229291777, 2.092415259949731432, 2.107292781797183601 ) ) ;
#80808 = EDGE_LOOP ( 'NONE', ( #93266, #183080, #194085, #71174 ) ) ;
#80810 = CARTESIAN_POINT ( 'NONE',  ( -0.6823417656250003738, 0.5302083336747518416, -1.181850606188749264 ) ) ;
#80809 = CARTESIAN_POINT ( 'NONE',  ( 3.035043143063915760, -2.020573557004992971, 1.082744910948540307 ) ) ;
#80811 = CARTESIAN_POINT ( 'NONE',  ( -3.449547071718236158, -1.000000000000000888, -2.024999999999992806 ) ) ;
#80812 = CARTESIAN_POINT ( 'NONE',  ( 3.897079088924235712, 6.634010472798538949, 1.199719254218462483 ) ) ;
#80813 = CARTESIAN_POINT ( 'NONE',  ( 5.127666992232062348, -0.3272401999867382560, 2.196937980255990741 ) ) ;
#80814 = CARTESIAN_POINT ( 'NONE',  ( -7.239690840017442675, 7.548653522882887934, 0.7216878364870317197 ) ) ;
#80815 = CARTESIAN_POINT ( 'NONE',  ( 4.202664430556241726, 7.846932902383524144, 0.7216878364870298324 ) ) ;
#80816 = VECTOR ( 'NONE', #17490, 1000.000000000000000 ) ;
#80817 = CARTESIAN_POINT ( 'NONE',  ( -7.334597914868741242, 8.619747657844088806, -1.082531754730543083 ) ) ;
#80818 = STYLED_ITEM ( 'NONE', ( #159412 ), #115007 ) ;
#80819 = CARTESIAN_POINT ( 'NONE',  ( 5.072158865288233009, 7.010880990960010273, 1.443375672974065660 ) ) ;
#80820 = VERTEX_POINT ( 'NONE', #171972 ) ;
#80821 = CARTESIAN_POINT ( 'NONE',  ( 3.182267690267494231, 1.591318367894577701, 1.238320962759748234 ) ) ;
#80823 = CARTESIAN_POINT ( 'NONE',  ( 1.832955167792608364, -1.957230265441430417, -0.6508311760726466222 ) ) ;
#80822 = CARTESIAN_POINT ( 'NONE',  ( 6.317209508963599340, 9.457495962844502557, 1.199719254218462483 ) ) ;
#80824 = CARTESIAN_POINT ( 'NONE',  ( -11.92619525870747665, 13.52622296793678380, 1.328859154005173959 ) ) ;
#80825 = CARTESIAN_POINT ( 'NONE',  ( 4.028181036591620412, 7.713645286083276709, -0.7216878364870338292 ) ) ;
#80826 = AXIS2_PLACEMENT_3D ( 'NONE', #60867, #58739, #206044 ) ;
#80827 = CARTESIAN_POINT ( 'NONE',  ( -7.960263458454529761, -6.452016313277124659, -7.960263458454494234 ) ) ;
#80828 = CARTESIAN_POINT ( 'NONE',  ( -1.364683531250010295, 4.280208333674753618, 0.7879004041258379498 ) ) ;
#80829 = CARTESIAN_POINT ( 'NONE',  ( 4.611385148785618782, -2.149487334021232599, 0.4259423572047504880 ) ) ;
#80830 = CARTESIAN_POINT ( 'NONE',  ( 2.654922836763852878, 1.081066371885472277, 1.701947380796410059 ) ) ;
#80831 = CARTESIAN_POINT ( 'NONE',  ( 1.452429406588066740, -1.579491434881035827, -0.9459884711465746943 ) ) ;
#80832 = CARTESIAN_POINT ( 'NONE',  ( 7.151035956204054855, 10.43029348462504124, 1.199719254218460707 ) ) ;
#80833 = CARTESIAN_POINT ( 'NONE',  ( 5.631824825758743991, -1.159798792365024145, -1.409841961918213427 ) ) ;
#80834 = AXIS2_PLACEMENT_3D ( 'NONE', #163888, #80487, #31751 ) ;
#80835 = CARTESIAN_POINT ( 'NONE',  ( 6.328750030911493241, 0.7691242348151774433, -1.864167186630163009 ) ) ;
#80836 = CARTESIAN_POINT ( 'NONE',  ( -6.516665389662827934, 10.75452672124865217, 0.000000000000000000 ) ) ;
#80838 = CARTESIAN_POINT ( 'NONE',  ( -6.954406449166956605, 7.078172043641714595, -0.7998128361456362523 ) ) ;
#80837 = CARTESIAN_POINT ( 'NONE',  ( 4.434621138646507532, 2.218105251380130483, 0.4453182654360221537 ) ) ;
#80839 = CARTESIAN_POINT ( 'NONE',  ( 0.4168064962662480499, 1.450752768847368257, -1.526948433937134197 ) ) ;
#80840 = CARTESIAN_POINT ( 'NONE',  ( -5.264308783856126439, 9.363720357799287797, -0.7998128361456362523 ) ) ;
#80841 = CARTESIAN_POINT ( 'NONE',  ( 4.229010956685672618, -1.930657356216297860, -0.7480826485904977785 ) ) ;
#80842 = CARTESIAN_POINT ( 'NONE',  ( 9.752392566931574081, 10.27221283770866300, -0.7998128361456281477 ) ) ;
#80843 = FACE_OUTER_BOUND ( 'NONE', #137875, .T. ) ;
#80844 = CARTESIAN_POINT ( 'NONE',  ( 8.378074386687000441, 33.50815134976858900, 15.76159487570644124 ) ) ;
#80845 = CARTESIAN_POINT ( 'NONE',  ( -7.178152263431422320, 10.46192917639026554, 1.199719254218453823 ) ) ;
#80846 = CARTESIAN_POINT ( 'NONE',  ( -4.609409038966248318, 5.440360635957812718, -1.082531754730544860 ) ) ;
#80847 = CARTESIAN_POINT ( 'NONE',  ( 8.188198428010544205, 8.517596018959260107, 0.000000000000000000 ) ) ;
#80848 = CARTESIAN_POINT ( 'NONE',  ( 4.554780495368041748, 6.962214942802684270, -1.182099088617315497 ) ) ;
#80849 = CARTESIAN_POINT ( 'NONE',  ( -10.31739171031960822, 11.13930453823545186, 1.040834085586084257E-14 ) ) ;
#80850 = CARTESIAN_POINT ( 'NONE',  ( 3.182088186068011915, 2.166492470972399165, -0.4902054615175278629 ) ) ;
#80851 = CARTESIAN_POINT ( 'NONE',  ( -0.3000000000000380695, 3.975028841772282107, 0.9637995837462106641 ) ) ;
#80852 = CARTESIAN_POINT ( 'NONE',  ( -6.611536185319534908, 7.742488966741438716, 1.199719254218452047 ) ) ;
#80853 = CARTESIAN_POINT ( 'NONE',  ( 6.986529229743720926, 7.045372277656132276, -0.7998128361456281477 ) ) ;
#80854 = CARTESIAN_POINT ( 'NONE',  ( 3.244534624505683418, -1.932379277470747558, -0.3379807920969243873 ) ) ;
#80855 = CARTESIAN_POINT ( 'NONE',  ( 5.769158057814842699, 6.689438141327490150, 1.199719254218462483 ) ) ;
#80857 =( BOUNDED_CURVE ( )  B_SPLINE_CURVE ( 2, ( #210852, #143781, #113437 ),
 .UNSPECIFIED., .F., .T. ) 
 B_SPLINE_CURVE_WITH_KNOTS ( ( 3, 3 ),
 ( 0.3392857142857143571, 0.3402546486199640174 ),
 .UNSPECIFIED. ) 
 CURVE ( )  GEOMETRIC_REPRESENTATION_ITEM ( )  RATIONAL_B_SPLINE_CURVE ( ( 0.9999999999999987788, 0.9781914855199952408, 0.9634829932421007381 ) ) 
 REPRESENTATION_ITEM ( '' )  );
#80856 = CARTESIAN_POINT ( 'NONE',  ( -4.043761313400059620, 7.584134902449670257, 0.3518898875958225703 ) ) ;
#80858 = CARTESIAN_POINT ( 'NONE',  ( 4.304877467538922531, 4.981110786005563007, 1.199719254218464037 ) ) ;
#80859 = CARTESIAN_POINT ( 'NONE',  ( -5.045042558060949034, 6.018876084893449274, 1.082531754730549078 ) ) ;
#80860 = CARTESIAN_POINT ( 'NONE',  ( -7.212574532790102744, 8.477387045419011002, -1.082531754730550855 ) ) ;
#80861 = CARTESIAN_POINT ( 'NONE',  ( 2.320699612028754188, -0.8158636990020677882, -1.957571985684476212 ) ) ;
#80862 = CARTESIAN_POINT ( 'NONE',  ( -4.599959256786493533, 8.588645909551377855, 0.000000000000000000 ) ) ;
#80863 = CARTESIAN_POINT ( 'NONE',  ( 4.170900312159072421, -2.016029151617684256, -0.7805680927704603533 ) ) ;
#80864 = CARTESIAN_POINT ( 'NONE',  ( 2.999365392321148960, -1.839032331094083927, 0.09308366406014098593 ) ) ;
#80865 = CARTESIAN_POINT ( 'NONE',  ( -4.183520347117292815, 7.398805986154902037, 0.7851016128354749712 ) ) ;
#80866 = CARTESIAN_POINT ( 'NONE',  ( -1.364683531250014514, -0.4072916663252447167, 0.7879004041258379498 ) ) ;
#80867 = CARTESIAN_POINT ( 'NONE',  ( 5.279165678654878846, 1.172930834070673889, 1.285866470927458094 ) ) ;
#80868 = CARTESIAN_POINT ( 'NONE',  ( 4.911989969715272686, 4.726297878971393196, 2.420000000000010587 ) ) ;
#80869 = CARTESIAN_POINT ( 'NONE',  ( 5.694061328059515148, 5.745419092265303007, -0.7216878364870207285 ) ) ;
#80870 = EDGE_CURVE ( 'NONE', #186457, #164855, #190333, .T. ) ;
#80872 = CARTESIAN_POINT ( 'NONE',  ( 2.624079441566569582, -1.243859440641072123, -1.767801033134681843 ) ) ;
#80871 = PRODUCT_RELATED_PRODUCT_CATEGORY ( 'part', '', ( #31690 ) ) ;
#80873 = CARTESIAN_POINT ( 'NONE',  ( 4.341172599035714619, -1.163090190446917083, 1.646587424817484324 ) ) ;
#80874 = CARTESIAN_POINT ( 'NONE',  ( -7.646435447983039424, 11.86466575604815787, 0.000000000000000000 ) ) ;
#80875 = CARTESIAN_POINT ( 'NONE',  ( 1.956163130892615731, 2.155914767609674598, -0.1587918856347721730 ) ) ;
#80876 = CARTESIAN_POINT ( 'NONE',  ( 2.723849342626927239, -1.131982996307562273, -1.613792087129195085 ) ) ;
#80877 = CARTESIAN_POINT ( 'NONE',  ( 6.509000000000045638, 3.691181720027385094, 2.614238911931165088 ) ) ;
#80878 = CARTESIAN_POINT ( 'NONE',  ( 4.106929586529986409, -0.3288250506029398168, 1.913867117139455676 ) ) ;
#80881 = ORIENTED_EDGE ( 'NONE', *, *, #211067, .T. ) ;
#80880 = CARTESIAN_POINT ( 'NONE',  ( 7.720982897393566802, -9.999999999999994671, -7.834948825496929281 ) ) ;
#80879 = CARTESIAN_POINT ( 'NONE',  ( -9.463228032214294316, 10.14278024711257764, 1.040834085586084257E-14 ) ) ;
#80882 = CARTESIAN_POINT ( 'NONE',  ( -3.973948422136981407, 5.729635473950147606, -1.443375672974066548 ) ) ;
#80883 = CARTESIAN_POINT ( 'NONE',  ( 4.411198876399872404, 6.239761003923544713, -1.599625672291273171 ) ) ;
#80885 = VERTEX_POINT ( 'NONE', #108102 ) ;
#80884 = CARTESIAN_POINT ( 'NONE',  ( -6.303615075710993665, 6.318915441276411471, -0.7998128361456362523 ) ) ;
#80886 = CARTESIAN_POINT ( 'NONE',  ( -8.473482818416675499, 9.948446711983361723, -1.082531754730543083 ) ) ;
#80887 = CARTESIAN_POINT ( 'NONE',  ( 1.307976841356368602, -0.5351398426680589182, 2.140771676462468687 ) ) ;
#80888 = CARTESIAN_POINT ( 'NONE',  ( 3.285556943749998737, -2.355208332855375453, -1.896917185911906500 ) ) ;
#80889 = EDGE_CURVE ( 'NONE', #3320, #171576, #104798, .T. ) ;
#80890 = CARTESIAN_POINT ( 'NONE',  ( 5.383633123045536983, -1.864019207510819953, 0.6117972396969260096 ) ) ;
#80891 = CARTESIAN_POINT ( 'NONE',  ( 0.6823417656249899377, 4.738541667008086655, -1.181850606188754593 ) ) ;
#80892 = CARTESIAN_POINT ( 'NONE',  ( -1.500000000000013101, 2.660416667349483788, -0.8660254037844313801 ) ) ;
#80893 = CARTESIAN_POINT ( 'NONE',  ( 0.07459516483346911864, 0.007201286963446140027, -1.755573347271717211 ) ) ;
#80894 = CARTESIAN_POINT ( 'NONE',  ( 4.822110771479974467, 1.762745816080556915, 0.5315184756640098929 ) ) ;
#80895 = EDGE_LOOP ( 'NONE', ( #8792, #57282, #7477, #10037, #59188 ) ) ;
#80896 = CARTESIAN_POINT ( 'NONE',  ( -3.355169270512988773E-14, -0.7968749996585455797, 1.570758158831762286 ) ) ;
#80897 = CARTESIAN_POINT ( 'NONE',  ( -6.672584156219988571, 10.93643194889866521, -0.7998128361456291469 ) ) ;
#80898 = CARTESIAN_POINT ( 'NONE',  ( -15.75000000000000000, 13.40000000000000036, -1.400000000000001910 ) ) ;
#80899 = CARTESIAN_POINT ( 'NONE',  ( 5.554972086574996304, 0.4156608669513594534, 2.079290889414136423 ) ) ;
#80900 =( LENGTH_UNIT ( ) NAMED_UNIT ( * ) SI_UNIT ( .MILLI., .METRE. ) );
#80901 = CARTESIAN_POINT ( 'NONE',  ( 5.799137018343234473, 7.788745826199009237, -1.599625672291262513 ) ) ;
#80902 = CARTESIAN_POINT ( 'NONE',  ( 6.573517591324530507, 1.973370851288195338, -0.5938938365465350477 ) ) ;
#80905 = CARTESIAN_POINT ( 'NONE',  ( 3.649809678215182096, 0.6660801477775115664, 1.716721118343276453 ) ) ;
#80904 = CARTESIAN_POINT ( 'NONE',  ( 0.3263015691194782741, -1.220318288589719913, 1.405194318597773329 ) ) ;
#80903 = CARTESIAN_POINT ( 'NONE',  ( 10.62873463776380056, 12.29999999999998295, 3.199999999999997957 ) ) ;
#80906 = CARTESIAN_POINT ( 'NONE',  ( 8.446893396513862839, 9.813462703143045474, -1.199719254218445830 ) ) ;
#80907 = SURFACE_SIDE_STYLE ('',( #62515 ) ) ;
#80908 = AXIS2_PLACEMENT_3D ( 'NONE', #48786, #131158, #197149 ) ;
#80909 = CARTESIAN_POINT ( 'NONE',  ( -5.759181390754928742, 9.941071732514568993, 0.000000000000000000 ) ) ;
#80910 = CARTESIAN_POINT ( 'NONE',  ( 0.3282377607281127818, 2.238835450998152954, -1.225000000000007860 ) ) ;
#80911 = CARTESIAN_POINT ( 'NONE',  ( 3.633602750639616019, -2.039237483250630589, 0.8441791899983088765 ) ) ;
#80912 = CARTESIAN_POINT ( 'NONE',  ( 5.975896723952917711, 1.340560379189212226, 1.822362705929107429 ) ) ;
#80913 = CARTESIAN_POINT ( 'NONE',  ( -7.402388683381436074, 7.738467673474211495, 0.7216878364870317197 ) ) ;
#80914 = CARTESIAN_POINT ( 'NONE',  ( 5.625234629914776185, 1.601787910378251967, 0.8462062870350762767 ) ) ;
#80915 = CARTESIAN_POINT ( 'NONE',  ( 5.454270856000166923, -1.210104932453776039, 1.485173795633880633 ) ) ;
#80916 = CARTESIAN_POINT ( 'NONE',  ( -1.001543065824772872E-14, 5.384375000341415252, 1.575800808251672791 ) ) ;
#80917 = CARTESIAN_POINT ( 'NONE',  ( 5.823093596695693819, -0.04436734784114480107, 1.870300906237104988 ) ) ;
#80918 = CARTESIAN_POINT ( 'NONE',  ( 5.476954007041204164, 1.719599228052148154, 0.7121796456092708283 ) ) ;
#80919 = CARTESIAN_POINT ( 'NONE',  ( -0.4634916963857354522, 7.369626292149011881, 4.459501722865318207 ) ) ;
#80920 = CARTESIAN_POINT ( 'NONE',  ( 0.1275333129481092398, -1.147091320445620566, -1.478225367208672703 ) ) ;
#80921 = CARTESIAN_POINT ( 'NONE',  ( 1.305875433988498813, -1.124247956386617009, -1.673852571057245830 ) ) ;
#80923 = CARTESIAN_POINT ( 'NONE',  ( 3.000711368280566393, -0.6119465431162304236, -2.015196771704963030 ) ) ;
#80922 = CARTESIAN_POINT ( 'NONE',  ( -8.642432853707342488, 12.17025653171218558, 1.199719254218462483 ) ) ;
#80924 = CARTESIAN_POINT ( 'NONE',  ( 7.723341061279088038, 12.16231500480096983, -0.7998128361456291469 ) ) ;
#80925 = CARTESIAN_POINT ( 'NONE',  ( -9.287498920561160887, 10.79416914786490089, -1.199719254218441611 ) ) ;
#80926 = PRESENTATION_STYLE_ASSIGNMENT (( #165367 ) ) ;
#80927 = CARTESIAN_POINT ( 'NONE',  ( 3.217061457047249551, 1.589534765328611154, -1.246005657720136606 ) ) ;
#80928 = CARTESIAN_POINT ( 'NONE',  ( 1.364683531249988535, 3.405208333674749621, -0.7879004041258239610 ) ) ;
#80929 = CARTESIAN_POINT ( 'NONE',  ( 4.033714395265605823, 4.664753868353354704, -1.199719254218446718 ) ) ;
#80930 = CARTESIAN_POINT ( 'NONE',  ( 2.952577552874091626, 0.7252333659365679530, 2.036452211405047397 ) ) ;
#80931 = CARTESIAN_POINT ( 'NONE',  ( 6.609999999999971010, 7.629137130509032971, 2.879999999999991456 ) ) ;
#80933 = DIRECTION ( 'NONE',  ( 0.000000000000000000, 0.000000000000000000, -1.000000000000000000 ) ) ;
#80932 = CARTESIAN_POINT ( 'NONE',  ( 6.156284269057003655, 9.340026192945279249, -1.199719254218452047 ) ) ;
#80934 = CARTESIAN_POINT ( 'NONE',  ( 9.693716643646601128, 10.41168362711695750, 0.7216878364870438212 ) ) ;
#80935 = CARTESIAN_POINT ( 'NONE',  ( 7.506010991098318819, 15.48982135686440031, -9.369134107302478753 ) ) ;
#80936 = CARTESIAN_POINT ( 'NONE',  ( -6.534666852106790103, 10.56760239419251590, 0.7216878364870458196 ) ) ;
#80937 = CARTESIAN_POINT ( 'NONE',  ( -1.364683531250014514, 0.7385416670080887647, -0.7879004041258289570 ) ) ;
#80938 = CARTESIAN_POINT ( 'NONE',  ( 0.9959476074029065540, -2.191739723303194332, 0.005169097091584088505 ) ) ;
#80939 = CARTESIAN_POINT ( 'NONE',  ( -4.140487720836006247, 5.732536712720713190, 1.378239279427504238 ) ) ;
#80940 = CARTESIAN_POINT ( 'NONE',  ( 2.905426592119991991, 1.910755973352752379, 1.211346930818749890 ) ) ;
#80941 = CARTESIAN_POINT ( 'NONE',  ( -7.832860060393135093, 10.16142270859057462, 1.599625672291295375 ) ) ;
#80942 = CARTESIAN_POINT ( 'NONE',  ( -2.602802303699316866, 5.980427087717073320, 1.040834085586084257E-14 ) ) ;
#80943 = CARTESIAN_POINT ( 'NONE',  ( 1.364683531249988535, 3.717708333674750953, -0.7879004041258239610 ) ) ;
#80944 = CARTESIAN_POINT ( 'NONE',  ( 5.614387949662905442, 7.370906683214474953, 1.237392280610301931 ) ) ;
#80945 = CARTESIAN_POINT ( 'NONE',  ( 1.499999999999997113, 10.64583333333333037, -0.8660254037844378194 ) ) ;
#80946 = CARTESIAN_POINT ( 'NONE',  ( 3.067887898442204442, 6.801229324816399746, 0.7998128361456271485 ) ) ;
#80947 = CARTESIAN_POINT ( 'NONE',  ( 3.725649928583890436, -1.052200936647734286, -1.422817597083583241 ) ) ;
#80948 = CARTESIAN_POINT ( 'NONE',  ( 10.24726517383036928, 10.84956421242393887, 0.000000000000000000 ) ) ;
#80949 = CARTESIAN_POINT ( 'NONE',  ( 6.422910180798067969, 2.056742032306459578, 0.8002587082300142152 ) ) ;
#80950 = CARTESIAN_POINT ( 'NONE',  ( -0.6823417656250003738, 9.151041667008065872, 1.181850606188754593 ) ) ;
#80951 = VERTEX_POINT ( 'NONE', #208714 ) ;
#80952 = CARTESIAN_POINT ( 'NONE',  ( -5.936491157937300756, 8.019268665717216749, 1.599625672291263179 ) ) ;
#80953 = CARTESIAN_POINT ( 'NONE',  ( 4.640250013031629095, 0.7743308749140092040, 1.862011755488258480 ) ) ;
#80954 = VERTEX_POINT ( 'NONE', #59276 ) ;
#80955 = CARTESIAN_POINT ( 'NONE',  ( 3.362029495745801899, 0.8400119854848132617, 1.671504782411597612 ) ) ;
#80956 = CARTESIAN_POINT ( 'NONE',  ( 3.168866831888625946, 1.502704456927813403, -1.424286459396295390 ) ) ;
#80957 = CARTESIAN_POINT ( 'NONE',  ( -6.089020385868850305, 10.11795786024005572, -0.7216878364870338292 ) ) ;
#80958 = CARTESIAN_POINT ( 'NONE',  ( -0.5993518605652793374, 3.417525394178890785, -0.2595036419143044726 ) ) ;
#80959 = CARTESIAN_POINT ( 'NONE',  ( -9.970593631352514308, 5.552127128363319564, -5.997086463700067149 ) ) ;
#80960 = CARTESIAN_POINT ( 'NONE',  ( -5.000214209863262482, 4.798281097787373994, 0.2926532548524369837 ) ) ;
#80961 = EDGE_CURVE ( 'NONE', #19959, #101924, #110239, .T. ) ;
#80962 = MECHANICAL_DESIGN_GEOMETRIC_PRESENTATION_REPRESENTATION (  '', ( #150089 ), #112128 ) ;
#80963 = CARTESIAN_POINT ( 'NONE',  ( -1.364683531250010295, 4.592708333674755394, 0.7879004041258379498 ) ) ;
#80964 = CARTESIAN_POINT ( 'NONE',  ( 1.441514601552947417, -1.799640695080907182, 0.6472408003148701905 ) ) ;
#80965 = CARTESIAN_POINT ( 'NONE',  ( 2.488659587246494276, 1.902222718079676689, 0.4795239450603656084 ) ) ;
#80966 = CARTESIAN_POINT ( 'NONE',  ( 1.212267286723569981, -1.587592435625035270, -1.242539042498117086 ) ) ;
#80967 = CARTESIAN_POINT ( 'NONE',  ( -5.971440312176176768, 5.931378217152456500, 0.000000000000000000 ) ) ;
#80969 = CARTESIAN_POINT ( 'NONE',  ( -11.35610322553117513, 12.48578371070822790, 3.553412924323499755 ) ) ;
#80968 = CARTESIAN_POINT ( 'NONE',  ( 8.178592977541601527, 10.56477777859713463, 1.599625672291281386 ) ) ;
#80971 = ADVANCED_FACE ( 'NONE', ( #43062, #175188 ), #7307, .T. ) ;
#80970 = CARTESIAN_POINT ( 'NONE',  ( 0.1806930697454533219, -0.1309388314422038346, -1.840455529407057256 ) ) ;
#80972 = CARTESIAN_POINT ( 'NONE',  ( -1.364683531250012516, 3.030208333674755394, 0.7879004041258379498 ) ) ;
#80973 = CARTESIAN_POINT ( 'NONE',  ( 2.338141740155843085, -1.162522942608142928, -1.643444077351646326 ) ) ;
#80974 = B_SPLINE_CURVE_WITH_KNOTS ( 'NONE', 3,
 ( #199586, #51229, #117353, #183351, #68512, #36027, #102105, #19775, #85857, #119488, #151931, #185475, #3506, #37099, #103178, #169239, #123790, #156211, #155135, #107510, #187613, #24040, #40325, #170297, #41400, #9934, #138895, #57631, #74945, #190807, #39241, #6717, #105333, #188689, #56568, #203847, #189748, #173539, #106430, #38179, #171370, #172453, #22963, #89078, #72795, #7787, #142112, #104251, #204914, #5632, #21885, #26181, #207063, #25113, #58693, #87994, #122726, #124841, #90143, #121646, #73880, #139973, #205995, #42467, #91216, #157277, #92296, #108577, #8866, #174605, #154067, #141056, #158340, #76009, #208125, #59754, #186550, #71713, #137826, #55492, #77061, #162601, #192942, #28322, #31536, #147417, #13127, #128056, #79205, #194012, #93352, #10987, #97611, #126983, #145322, #143191, #159389, #212383, #209182, #60822, #176709, #80270, #81338, #15251, #110709, #163668, #130171, #213442, #46730, #44594, #211323, #94418, #160457, #125914, #112842, #43533, #12065, #146368, #78134, #178858, #144264, #210257, #61895, #191873, #30469, #96554, #45661, #111779, #177785, #64025, #29401, #95493, #161540, #129117, #62948, #196163, #47804, #109656, #14177, #195093, #175658, #27246, #113917, #179913, #185209, #116027, #168976, #165789, #2178, #131221, #84528, #118164, #66112, #151679, #36833, #182012, #16306, #148480, #33643, #135427, #166855, #132255, #82391, #65065, #83456, #101847, #48, #17372, #52038, #167917, #86661, #99717, #198262, #119225, #34704, #184149, #35773, #149536, #197209, #49905, #1122, #32585, #102916, #152728, #20577, #48849, #67184, #114963, #19514, #133321, #180963, #100773, #85591, #3249, #199323, #98662, #50970, #117092, #183092, #18451, #150617, #164717, #68254, #134387, #200390, #69317, #201449, #53092, #88814, #58433, #189494, #202518, #174339, #55236, #171109, #122464, #186281, #22702, #138629, #106167, #90950, #170036, #72532, #41138, #71454, #121383, #124586, #25917, #172194, #6455, #23783, #204653, #37918, #103992, #190546, #5375, #89889, #21622, #87730, #157017, #153802, #56302, #107248, #173269, #92025, #108318, #203584, #42203, #8601, #4310, #139708, #137567, #155940, #187356, #38986, #70381, #205731, #136497, #105071, #24849, #154872, #188422, #206800, #40058, #7526, #54168, #57367, #74685, #73609, #123529, #140786, #120306, #60554, #10729, #109390, #161268, #127794, #178589, #162338, #63755, #78929, #195901, #76799, #179654, #194820, #47536, #129915, #208920, #113650, #44328, #95218, #9670, #177518, #211054, #159128, #30197, #31274, #126714, #175395, #26981, #192674, #142920, #110450, #176451, #93086, #158083, #28063, #46455, #94156, #160195, #145052, #112577, #75746, #11797, #77871, #96286, #143994, #212117, #128838, #141858, #207865, #13921, #209986, #61628, #193749, #45395, #111512, #59489, #125646, #29131, #12854, #80001, #62678, #146107, #191608, #43270, #199063, #99466, #50709, #165525, #64817, #213190, #19262, #52842, #164462, #130963, #151425, #83194, #49642, #149276, #67991, #51794, #118977, #201202, #82132, #135187, #101593, #69067, #18189, #48593, #116835, #81077, #17116, #184956, #2998, #97349, #147163, #196955, #133065, #857, #85344, #16048, #181754, #163406, #84274, #134133, #214226, #114711, #66923, #117913, #65854, #180706, #100525, #182836, #183905, #167661, #14981 ),
 .UNSPECIFIED., .F., .F.,
 ( 4, 1, 1, 1, 1, 1, 1, 1, 1, 1, 1, 1, 1, 1, 1, 1, 1, 1, 1, 1, 1, 1, 1, 1, 1, 1, 1, 1, 1, 1, 1, 1, 1, 1, 1, 1, 1, 1, 1, 1, 1, 1, 1, 1, 1, 1, 1, 1, 1, 1, 1, 1, 1, 1, 1, 1, 1, 1, 1, 1, 1, 1, 1, 1, 1, 1, 1, 1, 1, 1, 1, 1, 1, 1, 1, 1, 1, 1, 1, 1, 1, 1, 1, 1, 1, 1, 1, 1, 1, 1, 1, 1, 1, 1, 1, 1, 1, 1, 1, 1, 1, 1, 1, 1, 1, 1, 1, 1, 1, 1, 1, 1, 1, 1, 1, 1, 1, 1, 1, 1, 1, 1, 1, 1, 1, 1, 1, 1, 1, 1, 1, 1, 1, 1, 1, 1, 1, 1, 1, 1, 1, 1, 1, 1, 1, 1, 1, 1, 1, 1, 1, 1, 1, 1, 1, 1, 1, 1, 1, 1, 1, 1, 1, 1, 1, 1, 1, 1, 1, 1, 1, 1, 1, 1, 1, 1, 1, 1, 1, 1, 1, 1, 1, 1, 1, 1, 1, 1, 1, 1, 1, 1, 1, 1, 1, 1, 1, 1, 1, 1, 1, 1, 1, 1, 1, 1, 1, 1, 1, 1, 1, 1, 1, 1, 1, 1, 1, 1, 1, 1, 1, 1, 1, 1, 1, 1, 1, 1, 1, 1, 1, 1, 1, 1, 1, 1, 1, 1, 1, 1, 1, 1, 1, 1, 1, 1, 1, 1, 1, 1, 1, 1, 1, 1, 1, 1, 1, 1, 1, 1, 1, 1, 1, 1, 1, 1, 1, 1, 1, 1, 1, 1, 1, 1, 1, 1, 1, 1, 1, 1, 1, 1, 1, 1, 1, 1, 1, 1, 1, 1, 1, 1, 1, 1, 1, 1, 1, 1, 1, 1, 1, 1, 1, 1, 1, 1, 1, 1, 1, 1, 1, 1, 1, 1, 1, 1, 1, 1, 1, 1, 1, 1, 1, 1, 1, 1, 1, 1, 1, 1, 1, 1, 1, 1, 1, 1, 1, 1, 1, 1, 1, 1, 1, 1, 1, 1, 1, 1, 1, 1, 1, 1, 1, 1, 1, 1, 1, 1, 1, 1, 1, 1, 1, 1, 1, 1, 1, 1, 1, 1, 1, 1, 1, 1, 1, 1, 1, 1, 1, 1, 1, 1, 1, 1, 4 ),
 ( 0.000000000000000000, 0.002600034503794030130, 0.005208798665460326327, 0.007813183304800875098, 0.01041632952039499814, 0.01302078637366306003, 0.01562487905948694092, 0.01822913957756216313, 0.02083328395591756144, 0.02343739818322774712, 0.02604168118785421884, 0.02864568517727394958, 0.03125004130332968699, 0.03385401862675675722, 0.03645834363201481965, 0.03906241290072134942, 0.04166661303991354287, 0.04427083116291704451, 0.04687488238457573897, 0.04947921467585455341, 0.05208318889621989245, 0.05468754274347345512, 0.05729155431138267807, 0.05989582568988525285, 0.06249996760622017478, 0.06510408932096034551, 0.06770837349117478365, 0.07031237295078232585, 0.07291672927807971161, 0.07552070761765239393, 0.07812503204114096267, 0.08072910085791458468, 0.08333330089851145872, 0.08593751883178461781, 0.08854156980611090078, 0.09114590188302622298, 0.09374987588873062716, 0.09635422952249227124, 0.09895824087764454324, 0.1015625120427016276, 0.1041666537503683765, 0.1067707752516706410, 0.1093750592157429480, 0.1119790584643299974, 0.1145834145867499904, 0.1171873927198607973, 0.1197917169388799108, 0.1223957855539345302, 0.1249999853896588409, 0.1276042031245507580, 0.1302082538950744550, 0.1328125857752754935, 0.1354165595809520839, 0.1380209130188291833, 0.1406249241787864424, 0.1432291951479887082, 0.1458333366646657747, 0.1484374579699756502, 0.1510417417453218114, 0.1536457408005802994, 0.1562500967354857329, 0.1588540746797905134, 0.1614583987117299280, 0.1640624671426803571, 0.1666666667910262079, 0.1692708843450304312, 0.1718749349293641482, 0.1744792666302357464, 0.1770832402535473249, 0.1796875935129024493, 0.1822916044953091785, 0.1848958752860835608, 0.1875000166293293857, 0.1901041377562054102, 0.1927084213602507368, 0.1953124202398235920, 0.1979167760045740521, 0.2005207537777317084, 0.2031250776399721736, 0.2057291459044250093, 0.2083333453828807025, 0.2109375627734847158, 0.2135416131892344249, 0.2161459447281551538, 0.2187499181867580689, 0.2213542712849473904, 0.2239582821074418695, 0.2265625527372090720, 0.2291666939245756707, 0.2317708148905701926, 0.2343750983407339450, 0.2369790970622578097, 0.2395834526742069426, 0.2421874302938704648, 0.2447917540037867212, 0.2473958221193426621, 0.2500000214453905190, 0.2526042386900758108, 0.2552082889548416555, 0.2578126203491843960, 0.2604165936607292231, 0.2630209466151033904, 0.2656249572953180982, 0.2682292277814931625, 0.2708333688305272213, 0.2734374896531870935, 0.2760417729668830367, 0.2786457715479891406, 0.2812501270244852081, 0.2838541045083020076, 0.2864584280832634389, 0.2890624960675178268, 0.2916666952586349781, 0.2942709123748779576, 0.2968749625062547248, 0.2994792937733871119, 0.3020832669555192918, 0.3046876197834237909, 0.3072916303389863768, 0.3098959006989794318, 0.3125000416272227799, 0.3151041623240899980, 0.3177084455187270673, 0.3203124439770417831, 0.3229167993354283839, 0.3255207767010412923, 0.3281251001584127303, 0.3307291680289564662, 0.3333333671026155187, 0.3359375841078879321, 0.3385416341234662174, 0.3411459652807516951, 0.3437499383511121720, 0.3463542910698884647, 0.3489583015184220538, 0.3515625717696388985, 0.3541667125946290073, 0.3567708331832410984, 0.3593751162762241491, 0.3619791146293697692, 0.3645834698869864221, 0.3671874471520340522, 0.3697917705091763874, 0.3723958382835964032, 0.3750000372572658280, 0.3776042541690359799, 0.3802083040864021046, 0.3828126351512001757, 0.3854166081274262856, 0.3880209607544118922, 0.3906249711135359459, 0.3932292412733790488, 0.3958333820126498370, 0.3984375025105409418, 0.4010417855192715542, 0.4036457837848667074, 0.4062501389590495449, 0.4088541161411674008, 0.4114584394154381930, 0.4140625071113177014, 0.4166667060024629166, 0.4192709228381954478, 0.4218749726749327911, 0.4244793036646000717, 0.4270832765643259310, 0.4296876291168554296, 0.4322916394041865784, 0.4348959094900549660, 0.4375000501611374104, 0.4401041705858387276, 0.4427084535277153732, 0.4453124517233759683, 0.4479168068314584583, 0.4505207839482789911, 0.4531251071570330247, 0.4557291747919532399, 0.4583333736180368323, 0.4609375903951940523, 0.4635416401688834398, 0.4661459711007739370, 0.4687499439416310532, 0.4713542964370365795, 0.4739583066701890113, 0.4765625766994796009, 0.4791667173199026797, 0.4817708376889431876, 0.4843751205813623395, 0.4869791187247021202, 0.4895834737840155659, 0.4921874508531692838, 0.4947917740137594000, 0.4973958416052992049, 0.5000000403837819851, 0.5026042571198243714, 0.5052083068480445194, 0.5078126377395105751, 0.5104166105391289010, 0.5130209629947408700, 0.5156249731913270518, 0.5182292431814352618, 0.5208333837687260104, 0.5234375040996330775, 0.5260417869599895990, 0.5286457850686206994, 0.5312501400964950715, 0.5338541171356111503, 0.5364584402653888029, 0.5390625078311259699, 0.5416667065794673608, 0.5442709232918542250, 0.5468749729921829061, 0.5494793038605755298, 0.5520832766365837418, 0.5546876290697317913, 0.5572916392473630243, 0.5598959092156829964, 0.5625000497873680061, 0.5651041700976676685, 0.5677084529433557014, 0.5703124510348895893, 0.5729168060486536929, 0.5755207830753605869, 0.5781251061916765632, 0.5807291737491879768, 0.5833333724848467350, 0.5859375891910368894, 0.5885416388810509325, 0.5911459697437208005, 0.5937499425137473530, 0.5963542949417601768, 0.5989583051180477069, 0.6015625750819736384, 0.6041667156555785567, 0.6067708359627971282, 0.6093751188112106476, 0.6119791169032582356, 0.6145834719202413199, 0.6171874489521673723, 0.6197917720723722379, 0.6223958396392350600, 0.6250000383796699976, 0.6276042550971219214, 0.6302083047943985994, 0.6328126356686964993, 0.6354166084503697354, 0.6380209608905765828, 0.6406249710831318778, 0.6432292410600577437, 0.6458333816531092175, 0.6484375019747732338, 0.6510417848433065480, 0.6536457829534795261, 0.6562501379910111732, 0.6588541150457848383, 0.6614584381872300467, 0.6640625057810221055, 0.6666667045436925898, 0.6692709212898660942, 0.6718749710119833463, 0.6744793019152608426, 0.6770832747262099938, 0.6796876271959411131, 0.6822916374223763070, 0.6848959074296973037, 0.6875000480597228680, 0.6901041684133596421, 0.6927084513194080584, 0.6953124494653194487, 0.6979168045407300180, 0.7005207816359816375, 0.7031251048160196415, 0.7057291724543196532, 0.7083333712566866058, 0.7109375880490425015, 0.7135416378135795989, 0.7161459687631898108, 0.7187499416210458847, 0.7213542941376326345, 0.7239583044155618596, 0.7265625744706748490, 0.7291667151552034820, 0.7317708355583423252, 0.7343751185193033715, 0.7369791167185673064, 0.7395834718491895998, 0.7421874490025512916, 0.7447917722385364314, 0.7473958399389256657, 0.7500000387984516736, 0.7526042556544531026, 0.7552083054789914263, 0.7578126364922896929, 0.7604166094146853627, 0.7630209619954617661, 0.7656249723425013753, 0.7682292424628052174, 0.7708333832193684509, 0.7734375036895410060, 0.7760417867228139865, 0.7786457849930478181, 0.7812501401962168579, 0.7838541174253229604, 0.7864584407346123518, 0.7890625085146746320, 0.7916667074488250577, 0.7942709243859374935, 0.7968749742880611997, 0.7994793053824050810, 0.8020832783869765725, 0.8046876310492792062, 0.8072916414830481058, 0.8098959116859448804, 0.8125000525320774658, 0.8151041730868179291, 0.8177084562098055898, 0.8203124545686294455, 0.8229168098616829186, 0.8255207871841712119, 0.8281251105841250792, 0.8307291784614470043, 0.8333333774876906519, 0.8359375945233833427, 0.8385416445206798075, 0.8411459757134309712, 0.8437499488178175078, 0.8463543015789862789, 0.8489583121171074831, 0.8515625824200027116, 0.8541667233732427311, 0.8567708440300897399, 0.8593751272601987123, 0.8619791257252362726, 0.8645834811255164176, 0.8671874585590289009, 0.8697917820670107991, 0.8723958500591838527, 0.8750000491949933012, 0.8776042663467393812, 0.8802083164568000884, 0.8828126477653241988, 0.8854166209871692228, 0.8880209738645485906, 0.8906249845246493324, 0.8932292549449527552, 0.8958333960228427317, 0.8984375167993386979, 0.9010418001539796107, 0.9036457987428592187, 0.9062501542677121602, 0.9088541318298947180, 0.9114584554632734203, 0.9140625235878931942, 0.9166667228507454634, 0.9192709401360219523, 0.9218749903764450471, 0.9244793218181143191, 0.9270832951750564987, 0.9296876481859919217, 0.9322916589857459524, 0.9348959295408556525, 0.9375000707608250883, 0.9401041916746273319, 0.9427084751713679101, 0.9453124739016935951, 0.9479168295687272483, 0.9505208072738278169, 0.9531251310501845930, 0.9557291993520028450, 0.9583333987332913750, 0.9609376160454207172, 0.9635416666839513589, 0.9661459986354887786, 0.9687499708159389433, 0.9713543235632202677, 0.9739583390673558494, 0.9765626083347638264, 0.9791667417950460361, 0.9817708662416058107, 0.9843751381318576188, 0.9869792129215403387, 0.9895836736503123010, 0.9921868305638316121, 0.9947912020913856068, 0.9973999845648282569, 1.000000000000000000 ),
 .UNSPECIFIED. ) ;
#80976 = CARTESIAN_POINT ( 'NONE',  ( 2.232168359954420200, 2.116822148135434567, 0.04868514642705767947 ) ) ;
#80975 = CARTESIAN_POINT ( 'NONE',  ( -7.714226216495749355, 8.102278128774251797, 1.040834085586084257E-14 ) ) ;
#80978 = ADVANCED_FACE ( 'NONE', ( #114503 ), #56168, .F. ) ;
#80977 = CARTESIAN_POINT ( 'NONE',  ( 1.499999999999822364, 7.388542872122566330, 4.154462424328215775 ) ) ;
#80979 = CARTESIAN_POINT ( 'NONE',  ( 4.018080225218490398, 2.055083638104511223, -0.2504045000601487492 ) ) ;
#80980 = CARTESIAN_POINT ( 'NONE',  ( 3.736153849017632922, 6.516540702899320081, -1.199719254218453823 ) ) ;
#80982 = CARTESIAN_POINT ( 'NONE',  ( 4.325214697959421706, 5.004837554829479451, 1.199719254218462483 ) ) ;
#80981 = CARTESIAN_POINT ( 'NONE',  ( 5.367163668781920194, 2.014996964747676422, -0.5569773519958736152 ) ) ;
#80984 = VERTEX_POINT ( 'NONE', #161055 ) ;
#80983 = CARTESIAN_POINT ( 'NONE',  ( 3.768406797884563897, -1.226484811506942441, 1.352366043108324201 ) ) ;
#80985 = CARTESIAN_POINT ( 'NONE',  ( 8.540746701604824409, 12.05162268759261224, -1.199719254218446718 ) ) ;
#80986 = SURFACE_SIDE_STYLE ('',( #163310 ) ) ;
#80987 = CARTESIAN_POINT ( 'NONE',  ( 10.13949827731025088, 13.65534166205038424, -7.300436427310208032 ) ) ;
#80988 = CARTESIAN_POINT ( 'NONE',  ( 6.739307351729481255, -1.974284904759715298, 0.9861035376414882814 ) ) ;
#80989 = CARTESIAN_POINT ( 'NONE',  ( -0.6823417656250039265, 10.63020833367472839, -1.181850606188755259 ) ) ;
#80990 = ORIENTED_EDGE ( 'NONE', *, *, #179458, .T. ) ;
#80991 = CARTESIAN_POINT ( 'NONE',  ( 5.672493831469004100, 0.7790509395085333244, 1.746586765831580124 ) ) ;
#80992 = CARTESIAN_POINT ( 'NONE',  ( -10.45741655484220267, 11.09474082360439873, -0.7998128361456221525 ) ) ;
#80993 = CARTESIAN_POINT ( 'NONE',  ( 6.934105498385400246, 10.17720795050327354, -1.199719254218441611 ) ) ;
#80994 = CARTESIAN_POINT ( 'NONE',  ( 0.6801582343749900117, 1.338541667008072533, -1.178068619123872729 ) ) ;
#80995 = CARTESIAN_POINT ( 'NONE',  ( 4.324687812634882000, 7.028924300507257250, 1.082531754730558626 ) ) ;
#80996 = CARTESIAN_POINT ( 'NONE',  ( 10.99620347397582698, -6.863457517656843088, -0.2978015046999226700 ) ) ;
#80997 = CARTESIAN_POINT ( 'NONE',  ( 8.358554193140776079, 14.08791053918336367, -8.548382748741554238 ) ) ;
#80998 = CARTESIAN_POINT ( 'NONE',  ( 0.3976880421775743080, -0.6195963491163229975, -1.733980255833281969 ) ) ;
#80999 = EDGE_LOOP ( 'NONE', ( #119413, #28347, #178406, #105509 ) ) ;
#81000 = CARTESIAN_POINT ( 'NONE',  ( -6.749980374757255319, 8.968339418673846097, 1.599625672291269396 ) ) ;
#81001 = CARTESIAN_POINT ( 'NONE',  ( 5.114452126850835612, 1.290914414355217366, -1.353902443742838191 ) ) ;
#81002 = CARTESIAN_POINT ( 'NONE',  ( -0.02299388927992032997, 1.367829385570513923, -2.164798317653505944 ) ) ;
#81003 = CARTESIAN_POINT ( 'NONE',  ( -5.000000000000009770, 3.850000000000006306, 6.071532165918824830E-15 ) ) ;
#81004 = CARTESIAN_POINT ( 'NONE',  ( 0.07968937610752521716, 14.48238360795788893, 11.99973206003776660 ) ) ;
#81005 = EDGE_CURVE ( 'NONE', #173182, #99531, #88169, .T. ) ;
#81006 = CARTESIAN_POINT ( 'NONE',  ( -6.453317930424837812, 7.591587675992828466, 1.082531754730549967 ) ) ;
#81007 = CARTESIAN_POINT ( 'NONE',  ( 5.983225862332436584, 5.874851682342960402, 0.7998128361456341429 ) ) ;
#81008 = CARTESIAN_POINT ( 'NONE',  ( 1.604289258337993296, 1.966964933800469106, 0.1018061066037061896 ) ) ;
#81009 = CARTESIAN_POINT ( 'NONE',  ( 2.478138860811992306, -2.011206848916185397, -0.1455134472309257965 ) ) ;
#81010 = CARTESIAN_POINT ( 'NONE',  ( -6.970863535720637216, 11.28442455831609337, 0.7998128361456481317 ) ) ;
#81011 = CARTESIAN_POINT ( 'NONE',  ( 6.527324610336440180, 6.579909898339485252, 0.7998128361456331437 ) ) ;
#81012 = CARTESIAN_POINT ( 'NONE',  ( 6.883263157960362477, -0.004191378316371896506, 2.053658919477070910 ) ) ;
#81013 = CARTESIAN_POINT ( 'NONE',  ( 3.082162360440068749, -2.159116730143955998, -0.3741398933536920768 ) ) ;
#81014 = CARTESIAN_POINT ( 'NONE',  ( 0.000000000000000000, 4.000000000000003553, 0.000000000000000000 ) ) ;
#81015 = CARTESIAN_POINT ( 'NONE',  ( -10.32183501870554387, 10.93656236477829502, 0.7998128361456462443 ) ) ;
#81016 = CARTESIAN_POINT ( 'NONE',  ( 5.070386261830877928, 5.978167395966564435, -1.082531754730548412 ) ) ;
#81017 = CARTESIAN_POINT ( 'NONE',  ( 4.258669648468281110, 6.061810238003387141, 1.443375672974058777 ) ) ;
#81018 = CARTESIAN_POINT ( 'NONE',  ( 8.934986926605834157, 10.38290515491702770, -1.199719254218446718 ) ) ;
#81019 =( BOUNDED_SURFACE ( )  B_SPLINE_SURFACE ( 3, 2, ( 
 ( #178084, #31836, #148775 ),
 ( #129416, #160758, #98967 ),
 ( #344, #162901, #14483 ),
 ( #147719, #78432, #50210 ) ),
 .UNSPECIFIED., .F., .F., .T. ) 
 B_SPLINE_SURFACE_WITH_KNOTS ( ( 4, 4 ),
 ( 3, 3 ),
 ( 4.712388980384689674, 6.283185307179586232 ),
 ( 0.000000000000000000, 1.000000000000000000 ),
 .UNSPECIFIED. ) 
 GEOMETRIC_REPRESENTATION_ITEM ( )  RATIONAL_B_SPLINE_SURFACE ( (
 ( 1.000000000000000000, 0.7071067811865286989, 1.000000000000000000),
 ( 1.000000000000000000, 0.8014503788334959022, 1.000000000000000000),
 ( 1.000000000000000000, 0.8676977444973670295, 1.000000000000000000),
 ( 1.000000000000000000, 0.8661919058288164441, 1.000000000000000000) ) ) 
 REPRESENTATION_ITEM ( '' )  SURFACE ( )  );
#81020 = CARTESIAN_POINT ( 'NONE',  ( -4.823892679392753458, 8.212814747032918916, -0.9657451781678332292 ) ) ;
#81021 = CARTESIAN_POINT ( 'NONE',  ( 5.885648082108190238, 7.959951743916638733, 1.443375672974065660 ) ) ;
#81022 = ORIENTED_EDGE ( 'NONE', *, *, #25737, .F. ) ;
#81024 = CARTESIAN_POINT ( 'NONE',  ( 1.401040355039730345, -0.2976371227399738917, -1.990864243493442709 ) ) ;
#81023 = CARTESIAN_POINT ( 'NONE',  ( 4.405690278861111864, -0.7914791229979671883, -1.662609734262666894 ) ) ;
#81025 = CARTESIAN_POINT ( 'NONE',  ( 3.427438825619326668, 1.030710970775401414, 2.054361689694866211 ) ) ;
#81027 = CARTESIAN_POINT ( 'NONE',  ( 1.604125426503384411, 1.858527726531463697, 0.09786615749988146484 ) ) ;
#81026 = CARTESIAN_POINT ( 'NONE',  ( 4.053524740805938720, 3.831459740469437936, 1.214306433183764966E-14 ) ) ;
#81029 = CARTESIAN_POINT ( 'NONE',  ( -1.642778471874998480, -2.501041666188707158, 2.845375778867863303 ) ) ;
#81028 = APPLICATION_CONTEXT ( 'automotive_design' ) ;
#81030 = FILL_AREA_STYLE ('',( #194775 ) ) ;
#81031 = CARTESIAN_POINT ( 'NONE',  ( 6.170165192347925931, 1.906784905861274693, -0.1475879885542986936 ) ) ;
#81032 = CARTESIAN_POINT ( 'NONE',  ( -7.296259222448620463, 11.66405285949874759, 0.7998128361456481317 ) ) ;
#81033 = CARTESIAN_POINT ( 'NONE',  ( -5.316205630334251531, 9.216340645449683677, -0.7216878364870338292 ) ) ;
#81035 = CARTESIAN_POINT ( 'NONE',  ( 3.115926070338378207, -0.9207206926411042325, -1.628290677324291780 ) ) ;
#81034 = CARTESIAN_POINT ( 'NONE',  ( 4.845306142872277455, 0.6545843485197681000, -1.985720288498250774 ) ) ;
#81036 = CARTESIAN_POINT ( 'NONE',  ( 7.971831135155394321, 8.402817200543854170, -0.7216878364870267237 ) ) ;
#81037 = B_SPLINE_CURVE_WITH_KNOTS ( 'NONE', 3,
 ( #10899, #107422, #90058, #173447, #157185, #60729 ),
 .UNSPECIFIED., .F., .F.,
 ( 4, 2, 4 ),
 ( 0.000000000000000000, 0.0003473417695167272832, 0.0006946835390334545664 ),
 .UNSPECIFIED. ) ;
#81038 = CARTESIAN_POINT ( 'NONE',  ( 5.636236351835953506, 0.3653394402399374741, 1.804471444190151930 ) ) ;
#81039 = CARTESIAN_POINT ( 'NONE',  ( 4.871457266011829823, 4.577788319968905562, -0.7998128361456221525 ) ) ;
#81041 = CARTESIAN_POINT ( 'NONE',  ( 3.683011284406639607, 7.448596931783069586, 0.7998128361456321445 ) ) ;
#81040 = CARTESIAN_POINT ( 'NONE',  ( -0.08058608058608254798, -8.407420853759283830, -10.99970480893080804 ) ) ;
#81042 = CARTESIAN_POINT ( 'NONE',  ( 4.740679804603589176, 0.2991043602584910199, 1.698571524128352994 ) ) ;
#81043 = CARTESIAN_POINT ( 'NONE',  ( -4.726989112658928072, 8.666571064744069020, 1.040834085586084257E-14 ) ) ;
#81044 = FACE_OUTER_BOUND ( 'NONE', #64724, .T. ) ;
#81045 = FILL_AREA_STYLE ('',( #16013 ) ) ;
#81046 = DIRECTION ( 'NONE',  ( 0.000000000000000000, -1.000000000000000000, 0.000000000000000000 ) ) ;
#81047 = CARTESIAN_POINT ( 'NONE',  ( 5.243124948155760912, -0.2588677773407067617, -2.155501751117256948 ) ) ;
#81048 = CARTESIAN_POINT ( 'NONE',  ( 3.211362085483655981, -0.3553965070040401852, 1.790585553824732390 ) ) ;
#81050 = EDGE_CURVE ( 'NONE', #88615, #43706, #198485, .T. ) ;
#81049 = CARTESIAN_POINT ( 'NONE',  ( 0.7605091544688712402, -0.6555486260201286441, -1.849146037077718852 ) ) ;
#81051 = CARTESIAN_POINT ( 'NONE',  ( 5.717987565503318770, 1.041469840191568963, -1.843387895306993318 ) ) ;
#81053 = CARTESIAN_POINT ( 'NONE',  ( -0.6823417656249969321, 3.530208333674754506, -1.181850606188749264 ) ) ;
#81052 = CARTESIAN_POINT ( 'NONE',  ( 5.882448709439383805, -0.3326909364035086081, -2.268010969791500742 ) ) ;
#81054 = CARTESIAN_POINT ( 'NONE',  ( 4.905525160106620319, 6.476373528817379821, 2.499999999999998668 ) ) ;
#81055 = CARTESIAN_POINT ( 'NONE',  ( 9.185812768458653466, 10.67553530374532045, 1.199719254218453823 ) ) ;
#81056 = CARTESIAN_POINT ( 'NONE',  ( 1.032067064438058068, -2.067986175307830798, 0.4682213744369929098 ) ) ;
#81057 = CARTESIAN_POINT ( 'NONE',  ( -5.124618876285560454, 5.081069565195661220, 0.7216878364870317197 ) ) ;
#81058 = DIRECTION ( 'NONE',  ( 0.000000000000000000, 1.000000000000000000, 0.000000000000000000 ) ) ;
#81059 = CARTESIAN_POINT ( 'NONE',  ( -5.273758565591545988, 6.215435083687305351, 1.082531754730546636 ) ) ;
#81060 = CARTESIAN_POINT ( 'NONE',  ( 6.754729744842355110, -0.5704115468931982846, -2.094772688322795506 ) ) ;
#81062 = CARTESIAN_POINT ( 'NONE',  ( -6.009258394948636914E-15, 11.96875000068279604, -1.732050807568875195 ) ) ;
#81061 = CARTESIAN_POINT ( 'NONE',  ( 6.983263157960391432, 4.691677264508577139, 2.616375093613742209 ) ) ;
#81064 = ORIENTED_EDGE ( 'NONE', *, *, #175600, .F. ) ;
#81063 = CARTESIAN_POINT ( 'NONE',  ( 2.385647502782287432, 0.1060323020976374625, -2.218877139873560278 ) ) ;
#81065 = CARTESIAN_POINT ( 'NONE',  ( 6.293592298849589817, 1.492257802130890765, -1.356297202127904944 ) ) ;
#81067 = CARTESIAN_POINT ( 'NONE',  ( 5.120015017920454881, 2.040880116263335431, -0.2974388374509198685 ) ) ;
#81066 = CARTESIAN_POINT ( 'NONE',  ( 4.792970997630896512, 5.550553237779539018, 1.199719254218464037 ) ) ;
#81069 = CARTESIAN_POINT ( 'NONE',  ( -3.475000000000000533, -1.750000000000001554, 0.000000000000000000 ) ) ;
#81068 = CARTESIAN_POINT ( 'NONE',  ( 4.342354338126830804, 8.288106837781779035, -0.7998128361456381397 ) ) ;
#81070 = CARTESIAN_POINT ( 'NONE',  ( 4.715203562502613188, 8.723097599553565118, 0.7998128361456341429 ) ) ;
#81071 = CARTESIAN_POINT ( 'NONE',  ( 3.285556943750000514, -3.551041666188707424, 1.896917185911906500 ) ) ;
#81072 = CARTESIAN_POINT ( 'NONE',  ( 0.1331565106231328843, 0.003911343561965873426, -1.946049565259087455 ) ) ;
#81073 = CARTESIAN_POINT ( 'NONE',  ( 5.812015183962491172, 1.231757822100377320, -1.368757117762291253 ) ) ;
#81074 = CARTESIAN_POINT ( 'NONE',  ( 6.017121246366603060, 5.914396297049491658, 1.040834085586084257E-14 ) ) ;
#81075 = CARTESIAN_POINT ( 'NONE',  ( 6.471393748265519719, 5.229711127717882491, -2.499999999999995115 ) ) ;
#81076 = CARTESIAN_POINT ( 'NONE',  ( 1.447837905203141373, 1.722567860661971206, 0.08979103728979326293 ) ) ;
#81077 = CARTESIAN_POINT ( 'NONE',  ( 0.1808755166769344391, 1.673851406602990366, -1.124249698880399162 ) ) ;
#81078 = CARTESIAN_POINT ( 'NONE',  ( 0.6823417656249899377, 4.488541667008086655, -1.181850606188754593 ) ) ;
#81079 = CARTESIAN_POINT ( 'NONE',  ( 2.671453201960610091, 0.1136055399131811194, -2.259690131287622084 ) ) ;
#81080 = CARTESIAN_POINT ( 'NONE',  ( 4.565121803138184831, -1.881030885445551304, -0.9473677958443439406 ) ) ;
#81081 = CARTESIAN_POINT ( 'NONE',  ( -4.496464221587651799, 5.274905009054215554, 1.199719254218452935 ) ) ;
#81082 = CARTESIAN_POINT ( 'NONE',  ( 2.371989033382770895, -1.092842237840240482, 1.391882982410238556 ) ) ;
#81083 = CARTESIAN_POINT ( 'NONE',  ( 6.368579470117202490, 8.453095353268645695, 1.599625672291281386 ) ) ;
#81084 = CARTESIAN_POINT ( 'NONE',  ( 4.190878879955609371, 7.903459436674603822, -0.7216878364870338292 ) ) ;
#81085 = CARTESIAN_POINT ( 'NONE',  ( -6.925517538482230506, 6.974191971184389160, 0.7998128361456341429 ) ) ;
#81086 = CARTESIAN_POINT ( 'NONE',  ( 1.499999999999987121, 2.795833333333352488, -0.8660254037844262731 ) ) ;
#81087 = CARTESIAN_POINT ( 'NONE',  ( -0.02240927558793281635, -1.987202795932199839, -0.9927825048469391955 ) ) ;
#81088 = CARTESIAN_POINT ( 'NONE',  ( 3.820431320580887302, 2.080737768064028437, 0.6879518193209921417 ) ) ;
#81089 = CARTESIAN_POINT ( 'NONE',  ( -5.773074481320628948, 5.629675071162500544, 0.000000000000000000 ) ) ;
#81090 = DIRECTION ( 'NONE',  ( -1.000000000000000000, -0.000000000000000000, -5.551115123125765446E-17 ) ) ;
#81091 = DIRECTION ( 'NONE',  ( 0.000000000000000000, 0.000000000000000000, -1.000000000000000000 ) ) ;
#81092 = CARTESIAN_POINT ( 'NONE',  ( -1.364683531250012516, 3.030208333674755394, 0.7879004041258379498 ) ) ;
#81093 = CARTESIAN_POINT ( 'NONE',  ( -0.6823417656250003738, 9.151041667008065872, 1.181850606188754593 ) ) ;
#81094 = CARTESIAN_POINT ( 'NONE',  ( -3.416291520963659512, 5.969128626890772615, 1.082531754730560403 ) ) ;
#81095 = CARTESIAN_POINT ( 'NONE',  ( 6.240501835383900797, 1.219778281852833546, -1.734492557903525523 ) ) ;
#81096 = CARTESIAN_POINT ( 'NONE',  ( -6.129694847154220305, 8.244672969803623630, -1.443375672974066548 ) ) ;
#81097 = ORIENTED_EDGE ( 'NONE', *, *, #14168, .F. ) ;
#81099 = CARTESIAN_POINT ( 'NONE',  ( -5.273758566035884776, 5.255065869904374409, 0.000000000000000000 ) ) ;
#81098 = CARTESIAN_POINT ( 'NONE',  ( -5.533136088152923904, 6.588318536667425285, 1.082531754730549078 ) ) ;
#81100 = CARTESIAN_POINT ( 'NONE',  ( 5.250031796989762967, 7.148123067953287446, 1.599625672291267398 ) ) ;
#81101 = CARTESIAN_POINT ( 'NONE',  ( 6.304252605626877504, 1.359535501544101077, -1.241908024382516018 ) ) ;
#81102 = FILL_AREA_STYLE_COLOUR ( '', #24928 ) ;
#81103 = CARTESIAN_POINT ( 'NONE',  ( -0.08896015505786540600, 7.049507384512283537, -3.948637857577287580 ) ) ;
#81104 = CARTESIAN_POINT ( 'NONE',  ( -1.364683531249997417, 3.571875000341423245, 1.214306433183764966E-14 ) ) ;
#81105 = CARTESIAN_POINT ( 'NONE',  ( 2.331276520414362174, 0.8190846186081652824, -1.535621120930601213 ) ) ;
#81106 = CARTESIAN_POINT ( 'NONE',  ( 0.000000000000000000, 0.9000000000000014655, 0.000000000000000000 ) ) ;
#81107 = CARTESIAN_POINT ( 'NONE',  ( 11.78331023100045627, 12.29999999999998295, 1.799999999999999600 ) ) ;
#81108 = CARTESIAN_POINT ( 'NONE',  ( -1.364683531250014514, -0.4072916663252447167, 0.7879004041258379498 ) ) ;
#81109 = LINE ( 'NONE', #12890, #187646 ) ;
#81110 = EDGE_CURVE ( 'NONE', #202176, #87871, #205449, .T. ) ;
#81111 = CARTESIAN_POINT ( 'NONE',  ( 6.104392421991035711, -0.7735064434604683736, -2.018760209060527888 ) ) ;
#81112 = CIRCLE ( 'NONE', #18787, 2.324999999999998845 ) ;
#81113 = CARTESIAN_POINT ( 'NONE',  ( -10.15913717534155047, 10.74674821418697057, 0.7998128361456462443 ) ) ;
#81114 = CARTESIAN_POINT ( 'NONE',  ( -5.056828107772848746, 8.843457192469559303, -0.7216878364870207285 ) ) ;
#81115 = CARTESIAN_POINT ( 'NONE',  ( 5.893488898593548520, 1.633865717575968324, 1.415524914074948404 ) ) ;
#81117 = ORIENTED_EDGE ( 'NONE', *, *, #22766, .F. ) ;
#81116 = CARTESIAN_POINT ( 'NONE',  ( -3.363304624641834106, 6.081549941127532222, -1.199719254218452047 ) ) ;
#81118 = CARTESIAN_POINT ( 'NONE',  ( -1.201851678989727383E-14, 4.946875000341420581, -1.575800808251660134 ) ) ;
#81120 = ADVANCED_FACE ( 'NONE', ( #82982 ), #78721, .T. ) ;
#81119 = CARTESIAN_POINT ( 'NONE',  ( 5.694591516259816188, -0.4762896487527890632, -1.912855984147985744 ) ) ;
#81121 = CARTESIAN_POINT ( 'NONE',  ( 4.833154173618329885, -1.132187431169606739, 1.313192701189482614 ) ) ;
#81123 = CARTESIAN_POINT ( 'NONE',  ( 2.068174269828721101, -1.345378145056834063, 1.729934933326432445 ) ) ;
#81122 = CARTESIAN_POINT ( 'NONE',  ( -1.360316468750014884, -0.8593749996585950957, -6.938893903907228378E-15 ) ) ;
#81124 = CARTESIAN_POINT ( 'NONE',  ( 3.733692867724636599, -2.133222801268436442, 0.8804087197434546930 ) ) ;
#81125 = CARTESIAN_POINT ( 'NONE',  ( 4.358703909566331802, -1.529595902882211256, 1.381216288725060082 ) ) ;
#81126 = CARTESIAN_POINT ( 'NONE',  ( 1.183423309950997870, -0.8736912582980368436, 1.734375191483277900 ) ) ;
#81127 = CARTESIAN_POINT ( 'NONE',  ( -6.521108698048791119, 6.710307690586118312, -0.7216878364870267237 ) ) ;
#81128 = CARTESIAN_POINT ( 'NONE',  ( -3.494969737272722643, 7.299491470118629088, -0.7998128361456481317 ) ) ;
#81129 = CARTESIAN_POINT ( 'NONE',  ( -5.608757509019104859, 5.636543682890225782, -0.3643211599073498674 ) ) ;
#81130 = CARTESIAN_POINT ( 'NONE',  ( 3.832379111121624327, -1.093062754469842579, -1.817066923117337751 ) ) ;
#81131 = CARTESIAN_POINT ( 'NONE',  ( 7.065207446497155708, 9.336104335703744539, 0.000000000000000000 ) ) ;
#81132 = CARTESIAN_POINT ( 'NONE',  ( 2.584611472894111195, -0.6298744119781033435, 1.915600275669691488 ) ) ;
#81133 = CARTESIAN_POINT ( 'NONE',  ( -6.860062538390436337, 7.105753837651378468, 1.040834085586084257E-14 ) ) ;
#81134 = CARTESIAN_POINT ( 'NONE',  ( 4.225739626866775289, -2.112672615930260900, 0.6375689414055001336 ) ) ;
#81135 = CARTESIAN_POINT ( 'NONE',  ( 3.865483193227626124, 7.523831135491951372, -0.7216878364870337181 ) ) ;
#81136 = CARTESIAN_POINT ( 'NONE',  ( -1.432719062495390716, -3.042800438942089514, 3.165902886691621010 ) ) ;
#81137 = COLOUR_RGB ( '', 0.40784314, 0.44705882, 0.49803922) ;
#81138 = DIRECTION ( 'NONE',  ( 0.000000000000000000, 0.7766560405360211083, 0.6299249119529329866 ) ) ;
#81139 = CARTESIAN_POINT ( 'NONE',  ( -6.400331034103001748, 9.624747418832267698, 1.199719254218452935 ) ) ;
#81141 = CARTESIAN_POINT ( 'NONE',  ( -9.260383576709818598, -9.448429295179884946, 0.1616405965916382914 ) ) ;
#81140 = CARTESIAN_POINT ( 'NONE',  ( -5.638125304375204649, 7.460809226315815224, 1.342380602066863160 ) ) ;
#81142 = CARTESIAN_POINT ( 'NONE',  ( 1.224999999999958789, 2.104166666666714036, 0.7072540797572757221 ) ) ;
#81143 = EDGE_LOOP ( 'NONE', ( #122265, #77132 ) ) ;
#81144 = CARTESIAN_POINT ( 'NONE',  ( 4.575106920794588916, 0.002012451770977418796, -2.061077815012714254 ) ) ;
#81145 = DIRECTION ( 'NONE',  ( 0.3281536732072464768, -0.000000000000000000, -0.9446243521954066358 ) ) ;
#81146 = CARTESIAN_POINT ( 'NONE',  ( 0.2943368945748013332, -8.203192640252304102, 9.495705940876563389 ) ) ;
#81147 = CARTESIAN_POINT ( 'NONE',  ( -5.928993247877788697, 5.811580298812519807, 0.7998128361456341429 ) ) ;
#81148 = CARTESIAN_POINT ( 'NONE',  ( 3.141275609595588492, 0.05172059693002092201, 2.019191109193402056 ) ) ;
#81149 = CARTESIAN_POINT ( 'NONE',  ( -1.402160292154681736E-14, -0.03749999999998095135, 1.732050807568877637 ) ) ;
#81150 = CARTESIAN_POINT ( 'NONE',  ( 10.23604278863759909, 11.04439746293979496, 0.000000000000000000 ) ) ;
#81151 = CARTESIAN_POINT ( 'NONE',  ( 7.121056995675668411, 9.330985799753529264, -1.599625672291262513 ) ) ;
#81152 = CARTESIAN_POINT ( 'NONE',  ( 3.116143102785688068, -1.014332071340098285, -1.793896330205650980 ) ) ;
#81153 = DIRECTION ( 'NONE',  ( 0.000000000000000000, 0.000000000000000000, 1.000000000000000000 ) ) ;
#81154 = CARTESIAN_POINT ( 'NONE',  ( 4.710568305744190276, 7.583081225755162968, 1.199719254218462483 ) ) ;
#81155 = FACE_OUTER_BOUND ( 'NONE', #138890, .T. ) ;
#81157 = AXIS2_PLACEMENT_3D ( 'NONE', #112503, #178514, #49565 ) ;
#81156 = CARTESIAN_POINT ( 'NONE',  ( 1.622747808203903963, -1.734053015003593101, 0.6191010992530541213 ) ) ;
#81158 = ADVANCED_FACE ( 'NONE', ( #148011 ), #85249, .T. ) ;
#81159 = CARTESIAN_POINT ( 'NONE',  ( 6.235036409211808461, 0.2120174297785166195, 2.196685143856290878 ) ) ;
#81160 = CARTESIAN_POINT ( 'NONE',  ( 6.574778147984297938, 6.635272358928617997, -0.7998128361456481317 ) ) ;
#81161 = CARTESIAN_POINT ( 'NONE',  ( 2.144033130777025065, 0.8294244109963678779, -1.996327601563187670 ) ) ;
#81162 = CARTESIAN_POINT ( 'NONE',  ( -4.961921032921567054, 4.891255414604337659, 0.7216878364870317197 ) ) ;
#81163 = CARTESIAN_POINT ( 'NONE',  ( 1.376185782568883020, -2.007256511855738612, -0.1928315418098166534 ) ) ;
#81164 = CARTESIAN_POINT ( 'NONE',  ( 2.443060400399544196, 1.412781429710145975, 1.812861393458516268 ) ) ;
#81165 = CARTESIAN_POINT ( 'NONE',  ( 3.001048869802141805, 2.786623193720118685, -2.499999999999995115 ) ) ;
#81166 = CARTESIAN_POINT ( 'NONE',  ( -0.4092328571444365237, 6.441158382021245465, 3.221544509361615738 ) ) ;
#81167 = CARTESIAN_POINT ( 'NONE',  ( 3.994965595081632959, 1.666078911148192843, -1.053691615683423510 ) ) ;
#81168 =( GEOMETRIC_REPRESENTATION_CONTEXT ( 3 ) GLOBAL_UNCERTAINTY_ASSIGNED_CONTEXT ( ( #145064 ) ) GLOBAL_UNIT_ASSIGNED_CONTEXT ( ( #120361, #87786, #141907 ) ) REPRESENTATION_CONTEXT ( 'NONE', 'WORKASPACE' ) );
#81169 = CARTESIAN_POINT ( 'NONE',  ( 4.768767694835816862, -0.2516295123269947642, -2.000731945836851544 ) ) ;
#81172 = EDGE_CURVE ( 'NONE', #169017, #80483, #134615, .T. ) ;
#81171 = CARTESIAN_POINT ( 'NONE',  ( 8.825994812371966702, 12.28044913353391898, -1.082531754730543083 ) ) ;
#81170 = CARTESIAN_POINT ( 'NONE',  ( -1.364683531249997417, 3.759375000341423689, 1.214306433183764966E-14 ) ) ;
#81174 = CARTESIAN_POINT ( 'NONE',  ( 6.287733905706966553, 1.451067878312240822, 1.526644127000365003 ) ) ;
#81173 = CARTESIAN_POINT ( 'NONE',  ( -5.716734326456539783, 9.821273814174633188, -0.7998128361456231517 ) ) ;
#81175 = CARTESIAN_POINT ( 'NONE',  ( 6.144996677366851401, -0.2998803957653916608, -2.048400609436632269 ) ) ;
#81176 = CARTESIAN_POINT ( 'NONE',  ( 5.632522751473472589, 8.658694745772667289, -1.199719254218440723 ) ) ;
#81177 = CARTESIAN_POINT ( 'NONE',  ( -5.038826645773246682, 9.030381520044109322, 0.7998128361456481317 ) ) ;
#81178 = CARTESIAN_POINT ( 'NONE',  ( 1.947641667917405117, 3.752373307046534379, -0.4616076617488063527 ) ) ;
#81179 = CARTESIAN_POINT ( 'NONE',  ( 6.328379800955010737, -0.9556441952764772596, -1.779432800462784847 ) ) ;
#81180 = CARTESIAN_POINT ( 'NONE',  ( -0.7500000000000249800, 0.2229166673494847872, 1.299038105676659116 ) ) ;
#81181 = CARTESIAN_POINT ( 'NONE',  ( 4.178580530314169650, -1.330465218273884087, 1.885386248989364466 ) ) ;
#81182 = COLOUR_RGB ( '', 0.66274510, 0.83137255, 0.94901961) ;
#81183 = CARTESIAN_POINT ( 'NONE',  ( 2.448158969691970555, -0.8859891528392377369, 1.862743816677481679 ) ) ;
#81184 = CARTESIAN_POINT ( 'NONE',  ( 6.127922243696800386, 10.09306701771420656, -0.7216878364870267237 ) ) ;
#81185 = CARTESIAN_POINT ( 'NONE',  ( 6.530187263637528439, 7.647581891445782709, -1.199719254218452047 ) ) ;
#81186 = CARTESIAN_POINT ( 'NONE',  ( 3.901714345682657292, 7.774026846596938434, 0.7998128361456271485 ) ) ;
#81187 = CARTESIAN_POINT ( 'NONE',  ( -1.364683531250012516, 0.8427083336747532849, 0.7879004041258379498 ) ) ;
#81188 = CARTESIAN_POINT ( 'NONE',  ( 5.564695703766185275, 5.456842840674144490, 0.000000000000000000 ) ) ;
#81189 = CARTESIAN_POINT ( 'NONE',  ( 6.656690234185433042, 7.828855363713562276, -1.082531754730543971 ) ) ;
#81191 = CARTESIAN_POINT ( 'NONE',  ( -1.408069224121404561, 3.464533069549484701, -0.5223881139200234891 ) ) ;
#81190 = CARTESIAN_POINT ( 'NONE',  ( 3.824824921856139870, -1.460638251479762229, 1.606552252625459420 ) ) ;
#81192 = CARTESIAN_POINT ( 'NONE',  ( 0.4499999999999504396, 3.999999999999996891, 0.9353126743250794739 ) ) ;
#81194 = CARTESIAN_POINT ( 'NONE',  ( 2.507154105146496725, -1.820902139252629448, 0.2722148935128121394 ) ) ;
#81193 = CARTESIAN_POINT ( 'NONE',  ( -4.826339496784927796, 5.693446170079573321, 1.082531754730560403 ) ) ;
#81195 = CARTESIAN_POINT ( 'NONE',  ( -1.001543065824772872E-14, 5.071875000341421469, 1.575800808251672791 ) ) ;
#81196 = CARTESIAN_POINT ( 'NONE',  ( 5.267185993530860699, 2.112242253262315739, -0.5839428218426812034 ) ) ;
#81197 = CARTESIAN_POINT ( 'NONE',  ( 8.648791051114949724, 13.73763115593600048, 8.318960809290519620 ) ) ;
#81198 = CARTESIAN_POINT ( 'NONE',  ( 5.805634902324096736, -0.5560928936223124008, 2.193004490925544392 ) ) ;
#81199 = CARTESIAN_POINT ( 'NONE',  ( -5.732732414299474222, 6.256854150074313559, -1.080652830874342163 ) ) ;
#81200 = CARTESIAN_POINT ( 'NONE',  ( 4.757636082118741783, 8.295611710538327799, 0.7840751985381082534 ) ) ;
#81201 = CARTESIAN_POINT ( 'NONE',  ( -5.275531169048909952, 7.248148678680751189, -1.443375672974066548 ) ) ;
#81202 = CARTESIAN_POINT ( 'NONE',  ( 3.716343503921665459, 6.389465617000312569, -1.082531754730549967 ) ) ;
#81203 = CARTESIAN_POINT ( 'NONE',  ( 6.889980056308100842, -0.7542815031014777905, 1.599730008835710482 ) ) ;
#81204 = CARTESIAN_POINT ( 'NONE',  ( 3.949861574111676266, -1.389792608731334811, -1.456582260380126392 ) ) ;
#81205 = CARTESIAN_POINT ( 'NONE',  ( 7.579171565239241737, 8.801120566655981747, 1.199719254218462483 ) ) ;
#81206 = CARTESIAN_POINT ( 'NONE',  ( 3.065558131891146676, 0.3103791954156452371, -2.082839965623133782 ) ) ;
#81207 = CARTESIAN_POINT ( 'NONE',  ( 2.003404541029256691, -1.857510701737439929, 0.4675905980212178292 ) ) ;
#81208 = CARTESIAN_POINT ( 'NONE',  ( 4.532503425670185493, 4.182342172903648070, 1.214306433183764966E-14 ) ) ;
#81209 = CARTESIAN_POINT ( 'NONE',  ( 3.437912432318380507, 1.247599126489881138, 1.524034350268144156 ) ) ;
#81210 = CARTESIAN_POINT ( 'NONE',  ( 0.1450994221751950586, -1.442925249786636943, -1.190247126510869613 ) ) ;
#81211 = CARTESIAN_POINT ( 'NONE',  ( 0.9066075625437097774, 0.5660373911110065936, 1.878450800843839419 ) ) ;
#81214 = EDGE_LOOP ( 'NONE', ( #33614, #200569, #203589, #69433, #197196 ) ) ;
#81213 = CARTESIAN_POINT ( 'NONE',  ( 0.5098338327763075606, -0.6861045072398126443, 1.785269576063217567 ) ) ;
#81212 = CARTESIAN_POINT ( 'NONE',  ( 3.932037377198682737, 0.9205326289291086983, -1.458499330894097668 ) ) ;
#81216 = CARTESIAN_POINT ( 'NONE',  ( 5.341549334104194635, 6.294524313618772737, 1.082531754730558626 ) ) ;
#81215 = CARTESIAN_POINT ( 'NONE',  ( 1.735297346119796691, 0.2185962045802778420, 2.196029071591873993 ) ) ;
#81217 = CARTESIAN_POINT ( 'NONE',  ( 0.6823417656249899377, 0.6552083336747518416, 1.181850606188755259 ) ) ;
#81218 = CARTESIAN_POINT ( 'NONE',  ( 11.81907076198591966, 11.25731224596471769, 1.592066415281218505 ) ) ;
#81219 = CARTESIAN_POINT ( 'NONE',  ( 6.901817408925516872, -6.554751161430712791, -6.500815859343259895 ) ) ;
#81220 = AXIS2_PLACEMENT_3D ( 'NONE', #29081, #32275, #65796 ) ;
#81221 = CARTESIAN_POINT ( 'NONE',  ( 6.473496638176248652, -0.2593738453590052617, 2.053908440964563376 ) ) ;
#81222 = CARTESIAN_POINT ( 'NONE',  ( 0.8189040078958352842, -1.500748464528355974, 1.426492703164506937 ) ) ;
#81223 = CARTESIAN_POINT ( 'NONE',  ( 1.499999999999987121, 1.254166666666689300, 0.8660254037844524744 ) ) ;
#81224 = CARTESIAN_POINT ( 'NONE',  ( 7.287671262545424966, 8.461036880179857889, -1.199719254218451159 ) ) ;
#81225 = CARTESIAN_POINT ( 'NONE',  ( -8.877891658850122880, 9.251961778280284321, 0.7998128361456462443 ) ) ;
#81226 = CARTESIAN_POINT ( 'NONE',  ( 6.215487077222150880, 6.216099443039444949, 0.000000000000000000 ) ) ;
#81227 = CARTESIAN_POINT ( 'NONE',  ( 5.285831659486547984, 2.043504495962459977, -0.5658664308652374686 ) ) ;
#81228 = CARTESIAN_POINT ( 'NONE',  ( 4.004454267989866700, 5.765225627445230927, 1.599625672291262513 ) ) ;
#81229 = CARTESIAN_POINT ( 'NONE',  ( -1.364683531250012516, 1.780208333674757615, 0.7879004041258379498 ) ) ;
#81230 = ORIENTED_EDGE ( 'NONE', *, *, #183845, .T. ) ;
#81231 = CARTESIAN_POINT ( 'NONE',  ( 1.499999999999989120, 2.504166666666687302, 0.8660254037844524744 ) ) ;
#81233 = CARTESIAN_POINT ( 'NONE',  ( 5.657830175604453338, 5.495223381160312393, 0.7998128361456341429 ) ) ;
#81232 = CARTESIAN_POINT ( 'NONE',  ( 6.461383593301071926, 1.630371061775518271, 1.090930979547571456 ) ) ;
#81234 = CARTESIAN_POINT ( 'NONE',  ( 4.059922587279920947, 1.704677108394496043, -1.076152822228809480 ) ) ;
#81235 = CARTESIAN_POINT ( 'NONE',  ( 3.924928585964591932, -1.664043332733669667, 0.9490909334420574162 ) ) ;
#81236 = CARTESIAN_POINT ( 'NONE',  ( -1.882262909678039886, 3.299172163371803190, -0.4004916885352671763 ) ) ;
#81237 = CARTESIAN_POINT ( 'NONE',  ( 1.224469250947546328, 2.113408192816915943, 0.5798510048089372537 ) ) ;
#81238 = CARTESIAN_POINT ( 'NONE',  ( 0.1333692844072316419, 7.629137130509075604, -2.653547345224521514 ) ) ;
#81239 = CARTESIAN_POINT ( 'NONE',  ( 2.688565094423268853, -0.3157439183511835945, -1.843535313746543336 ) ) ;
#81240 = CARTESIAN_POINT ( 'NONE',  ( 0.7499999999999885647, -0.2354166659838466402, 1.299038105676657340 ) ) ;
#81241 = CARTESIAN_POINT ( 'NONE',  ( -7.542413527904030524, 7.693903958843159252, 1.040834085586084257E-14 ) ) ;
#81243 = CARTESIAN_POINT ( 'NONE',  ( 5.185217826725932788, 1.731529828693706641, 1.218147590116857026 ) ) ;
#81242 = CARTESIAN_POINT ( 'NONE',  ( -4.934804725694231564, 5.819988937140460727, -1.082531754730544860 ) ) ;
#81244 = B_SPLINE_CURVE_WITH_KNOTS ( 'NONE', 3,
 ( #181519, #166341, #211885, #82953 ),
 .UNSPECIFIED., .F., .F.,
 ( 4, 4 ),
 ( 0.000000000000000000, 0.0001938699898735654636 ),
 .UNSPECIFIED. ) ;
#81246 = ADVANCED_FACE ( 'NONE', ( #166121 ), #107480, .T. ) ;
#81245 = CARTESIAN_POINT ( 'NONE',  ( -1.499999999999964029, 6.999999999999999112, 9.886859966642596476 ) ) ;
#81248 = DIRECTION ( 'NONE',  ( -1.000000000000000000, 0.000000000000000000, 0.000000000000000000 ) ) ;
#81247 = CARTESIAN_POINT ( 'NONE',  ( 2.120754239039924549, 0.003043923042475667976, 2.090933975095090158 ) ) ;
#81250 = ORIENTED_EDGE ( 'NONE', *, *, #154830, .T. ) ;
#81249 = CARTESIAN_POINT ( 'NONE',  ( 1.166562959395722077, -1.556812811267356711, -0.7427251802107991407 ) ) ;
#81251 = CARTESIAN_POINT ( 'NONE',  ( 5.438792177376376991, 9.497007973581119700, 1.040834085586084257E-14 ) ) ;
#81252 = CARTESIAN_POINT ( 'NONE',  ( 6.825078400183569372, -0.002763825414428438751, 2.044262525762723826 ) ) ;
#81253 = CARTESIAN_POINT ( 'NONE',  ( 0.03749947599223481948, -9.978860283170366330, 9.579600585153697168 ) ) ;
#81254 = CARTESIAN_POINT ( 'NONE',  ( 9.508009452561562824, 4.000000000000000888, 7.612500000000001599 ) ) ;
#81256 = CARTESIAN_POINT ( 'NONE',  ( 7.565086526301031178, 11.76975868075249387, 1.040834085586084257E-14 ) ) ;
#81255 = CARTESIAN_POINT ( 'NONE',  ( 7.820355676984174664, 8.018169799436671852, -0.7998128361456281477 ) ) ;
#81257 = ORIENTED_EDGE ( 'NONE', *, *, #140838, .F. ) ;
#81258 = CARTESIAN_POINT ( 'NONE',  ( -15.75000000000000000, 10.90000000000000036, -1.100000000000002087 ) ) ;
#81260 = CARTESIAN_POINT ( 'NONE',  ( 1.330386229028382772, 1.216896677575128205, -1.342046333077246967 ) ) ;
#81259 = CARTESIAN_POINT ( 'NONE',  ( 5.773793314573267388, 7.829454515125894964, 1.599625672291268286 ) ) ;
#81261 = CARTESIAN_POINT ( 'NONE',  ( -6.344325816190970357, 9.489131654609717970, 1.199719254218452047 ) ) ;
#81262 = CARTESIAN_POINT ( 'NONE',  ( 3.845709127770629010, 7.638411082374393146, 0.7998128361456321445 ) ) ;
#81263 = CARTESIAN_POINT ( 'NONE',  ( 5.794130544993763898, 7.853181283949808744, 1.599625672291269396 ) ) ;
#81264 = CARTESIAN_POINT ( 'NONE',  ( 6.539320575229274013, 7.053493080409727334, 2.394893457813539683 ) ) ;
#81265 = CARTESIAN_POINT ( 'NONE',  ( 1.499999999999989120, 6.280000000000035776, 2.775557561562891351E-14 ) ) ;
#81266 = CARTESIAN_POINT ( 'NONE',  ( 4.553433815925461481, 6.963525196941225737, 1.181321538200299281 ) ) ;
#81267 = CARTESIAN_POINT ( 'NONE',  ( 7.754900677336718395, 11.99120852362745460, -0.7216878364870267237 ) ) ;
#81268 = ORIENTED_EDGE ( 'NONE', *, *, #55036, .F. ) ;
#81269 = CARTESIAN_POINT ( 'NONE',  ( 3.051044903872371261, 1.597643715361036998, -0.9542115197753370248 ) ) ;
#81270 = EDGE_CURVE ( 'NONE', #109478, #209652, #101712, .T. ) ;
#81271 = CARTESIAN_POINT ( 'NONE',  ( 0.2982578006338062471, 1.320465477219048722, -1.388022668363431356 ) ) ;
#81272 = CARTESIAN_POINT ( 'NONE',  ( 6.493193421754636319, 1.675589973874438643, -0.9503142578028888066 ) ) ;
#81273 = CIRCLE ( 'NONE', #105564, 10.24999999999999822 ) ;
#81274 = DIRECTION ( 'NONE',  ( 0.000000000000000000, 0.000000000000000000, 1.000000000000000000 ) ) ;
#81275 = CARTESIAN_POINT ( 'NONE',  ( -1.843739406749240750, 8.920000000000001705, 0.7750000000000013545 ) ) ;
#81276 = CARTESIAN_POINT ( 'NONE',  ( 4.735857411151594754, 8.202189375375613878, -0.7076125000919450958 ) ) ;
#81277 = PRESENTATION_STYLE_ASSIGNMENT (( #30410 ) ) ;
#81278 = CARTESIAN_POINT ( 'NONE',  ( -4.121315508874280553, 3.910548969882488901, -0.7216878364870207285 ) ) ;
#81279 = STYLED_ITEM ( 'NONE', ( #98607 ), #189006 ) ;
#81280 = CARTESIAN_POINT ( 'NONE',  ( 7.592202833972727660, 11.80139437303613015, -0.7216878364870267237 ) ) ;
#81281 = CARTESIAN_POINT ( 'NONE',  ( 5.190276988288149873, 1.015767153246112775, -1.687157232322311629 ) ) ;
#81282 = CARTESIAN_POINT ( 'NONE',  ( 1.805496089173063590, 1.843435535509674317, -1.047849062051922076 ) ) ;
#81283 = CARTESIAN_POINT ( 'NONE',  ( -5.636439174979254396, 7.598931675607687453, -1.599625672291256295 ) ) ;
#81284 = CARTESIAN_POINT ( 'NONE',  ( -10.63776469506859534, 5.877592587992107376, 5.457754955663538965 ) ) ;
#81285 = CARTESIAN_POINT ( 'NONE',  ( 4.924072945520472366, 4.709449622720799589, 0.000000000000000000 ) ) ;
#81286 = CARTESIAN_POINT ( 'NONE',  ( 6.228506716250251429, 0.2110190803071687604, 2.181275323772186692 ) ) ;
#81287 = CARTESIAN_POINT ( 'NONE',  ( 1.419999999999999485, 7.176846818246214177, 4.202462424328220258 ) ) ;
#81288 = CARTESIAN_POINT ( 'NONE',  ( 4.735331810261827812, -1.761409202268785057, 0.7803939243795944281 ) ) ;
#81289 = CARTESIAN_POINT ( 'NONE',  ( -6.826694039680798021, 7.923230120171105284, -1.199719254218446718 ) ) ;
#81290 = CARTESIAN_POINT ( 'NONE',  ( 0.4108170757193031486, 1.585627777896590151, 0.9046078287104839522 ) ) ;
#81291 = CARTESIAN_POINT ( 'NONE',  ( 0.8212658843103730621, 2.040464674744349338, 0.8412164853940640175 ) ) ;
#81292 = CARTESIAN_POINT ( 'NONE',  ( 7.034482758620714371, 5.227586206896606136, 1.214306433183764966E-14 ) ) ;
#81293 = CARTESIAN_POINT ( 'NONE',  ( -0.03866526371284068064, -9.261493551422349313, 9.500000000000152767 ) ) ;
#81294 = ORIENTED_EDGE ( 'NONE', *, *, #147718, .F. ) ;
#81295 = CARTESIAN_POINT ( 'NONE',  ( -1.734723475976807094E-15, 2.999999999999988898, -6.938893903907228378E-15 ) ) ;
#81296 = ORIENTED_EDGE ( 'NONE', *, *, #11376, .T. ) ;
#81297 = CARTESIAN_POINT ( 'NONE',  ( 5.840667653085179545, -1.920577060998058583, -0.4351772876184378247 ) ) ;
#81298 = CARTESIAN_POINT ( 'NONE',  ( 0.9955321287432462585, -1.942234967994656669, 0.001507142460104027087 ) ) ;
#81299 = CARTESIAN_POINT ( 'NONE',  ( 6.608760977740426590, 0.8891218545476579083, -2.119637956729656381 ) ) ;
#81301 = CARTESIAN_POINT ( 'NONE',  ( 5.155058861800134729, 1.548501282276077529, -1.031774840880594901 ) ) ;
#81300 = CARTESIAN_POINT ( 'NONE',  ( -6.038177310039794854, 8.137902509836795417, -1.599625672291271394 ) ) ;
#81302 = CARTESIAN_POINT ( 'NONE',  ( 4.864343252252968597, 8.897093904262280972, 0.000000000000000000 ) ) ;
#81303 = CARTESIAN_POINT ( 'NONE',  ( -15.75000000000000000, 10.89999999999998259, 3.199999999999997957 ) ) ;
#81304 = CARTESIAN_POINT ( 'NONE',  ( 4.076333666143569623, 3.981184372846183983, -0.7419984331740974159 ) ) ;
#81305 = CARTESIAN_POINT ( 'NONE',  ( -7.217017841176048165, 7.314275657660511243, 1.040834085586084257E-14 ) ) ;
#81306 = CARTESIAN_POINT ( 'NONE',  ( -5.901542003698421190, 10.10715911428198055, 0.000000000000000000 ) ) ;
#81307 = CARTESIAN_POINT ( 'NONE',  ( 1.980270094416748394, -2.150034404144373301, -0.4237573071887782983 ) ) ;
#81308 = CARTESIAN_POINT ( 'NONE',  ( 3.877268743828258479, 7.467304601200877023, 0.7216878364870298324 ) ) ;
#81309 = ORIENTED_EDGE ( 'NONE', *, *, #195648, .F. ) ;
#81310 = CARTESIAN_POINT ( 'NONE',  ( 5.692136587293079586, 5.855332880448198551, 2.500000000000010658 ) ) ;
#81311 = CARTESIAN_POINT ( 'NONE',  ( 1.892912435568369744, 1.589020553905008626, -0.8988452475950716725 ) ) ;
#81312 = CARTESIAN_POINT ( 'NONE',  ( -2.272963308585411735, 5.803540959991587478, 0.7998128361456341429 ) ) ;
#81313 = CARTESIAN_POINT ( 'NONE',  ( -6.434009798946909164, 6.877700593631734804, -0.7366733183416813713 ) ) ;
#81314 = CARTESIAN_POINT ( 'NONE',  ( 6.509000000000051855, 1.248119779622055336, 2.213941609938009591 ) ) ;
#81315 = CARTESIAN_POINT ( 'NONE',  ( 8.920375002787457319, 12.49452237230570084, 1.199719254218450271 ) ) ;
#81316 = CARTESIAN_POINT ( 'NONE',  ( 0.4516242601883875274, 0.6054225165459875546, -1.828971364544299538 ) ) ;
#81317 = CARTESIAN_POINT ( 'NONE',  ( 4.364078322825436729, -1.956782558839207375, 0.1401112987177987601 ) ) ;
#81318 = CARTESIAN_POINT ( 'NONE',  ( -8.015895134177625891, 10.37496362800581018, 1.599625672291295375 ) ) ;
#81319 = CARTESIAN_POINT ( 'NONE',  ( 6.986529229743720926, 7.045372277656132276, -0.7998128361456281477 ) ) ;
#81320 = CARTESIAN_POINT ( 'NONE',  ( 4.124703146219878214, 0.1084699374758208573, 2.189010777610411740 ) ) ;
#81321 = DIRECTION ( 'NONE',  ( 0.000000000000000000, 1.000000000000000000, 0.000000000000000000 ) ) ;
#81322 = CARTESIAN_POINT ( 'NONE',  ( 3.467693386974544545, -0.4085244671708112008, 2.029378838279243258 ) ) ;
#81323 = CARTESIAN_POINT ( 'NONE',  ( -1.402160292154681736E-14, 1.009375000341417916, -1.575800808251659024 ) ) ;
#81324 = ORIENTED_EDGE ( 'NONE', *, *, #98548, .F. ) ;
#81325 = CARTESIAN_POINT ( 'NONE',  ( 3.586856395851648394, -0.6656857563790157251, 2.200217309063193127 ) ) ;
#81326 = CARTESIAN_POINT ( 'NONE',  ( 6.778713617152772208, 10.85232362007950258, -0.7216878364870267237 ) ) ;
#81328 = CARTESIAN_POINT ( 'NONE',  ( 0.000000000000000000, -0.1968749995220437643, -3.793834371823813001 ) ) ;
#81327 = CARTESIAN_POINT ( 'NONE',  ( 6.427974226654860956, 7.632296364919712417, -1.082531754730548412 ) ) ;
#81329 = CARTESIAN_POINT ( 'NONE',  ( 6.720655732516647163, 2.082321177337285167, 2.135279995619132620 ) ) ;
#81330 = CARTESIAN_POINT ( 'NONE',  ( -6.064239847062411926, 10.29697326487330500, 0.000000000000000000 ) ) ;
#81331 = CARTESIAN_POINT ( 'NONE',  ( 3.398316578678576949, 1.530473418458015100, -1.195227296853792920 ) ) ;
#81332 = VERTEX_POINT ( 'NONE', #79573 ) ;
#81334 = CARTESIAN_POINT ( 'NONE',  ( 9.205623113554612047, 12.72334881824701469, 1.082531754730546636 ) ) ;
#81333 = MECHANICAL_DESIGN_GEOMETRIC_PRESENTATION_REPRESENTATION (  '', ( #126407 ), #36316 ) ;
#81335 = CARTESIAN_POINT ( 'NONE',  ( 4.465046277278037934, -1.532637281380120564, 1.143568071694904598 ) ) ;
#81336 = SURFACE_STYLE_USAGE ( .BOTH. , #14175 ) ;
#81337 = CARTESIAN_POINT ( 'NONE',  ( 5.649328262929842914, -1.362134112713381029, -1.057878908126141715 ) ) ;
#81338 = CARTESIAN_POINT ( 'NONE',  ( 4.733611406029458735, 0.6279933214467496860, -1.916352419866963697 ) ) ;
#81339 = CARTESIAN_POINT ( 'NONE',  ( 4.588719013068318198, -0.6136123943910645195, 2.215248572529082693 ) ) ;
#81340 = CARTESIAN_POINT ( 'NONE',  ( 6.385527162356455122, 10.39360608948380538, 1.056142170575426150E-14 ) ) ;
#81341 = CARTESIAN_POINT ( 'NONE',  ( 0.5927436934281338221, -2.190715567557582677, -0.2661302102612560505 ) ) ;
#81343 = CARTESIAN_POINT ( 'NONE',  ( -5.966997003790240228, 6.134120390609613338, -0.7216878364870338292 ) ) ;
#81342 = DIRECTION ( 'NONE',  ( 0.000000000000000000, 1.000000000000000000, 0.000000000000000000 ) ) ;
#81344 = CARTESIAN_POINT ( 'NONE',  ( 5.975818619601467319, 1.055637459841787473, 1.420274316496936917 ) ) ;
#81346 = CARTESIAN_POINT ( 'NONE',  ( 2.168323659614699750, -1.408312831382242614, 1.808550206204377009 ) ) ;
#81345 = CARTESIAN_POINT ( 'NONE',  ( 6.547661840756936691, 6.603636667163397256, 0.7998128361456352531 ) ) ;
#81347 = CARTESIAN_POINT ( 'NONE',  ( 0.8666887897643248406, 1.678224016273874852, -0.4604494717724941233 ) ) ;
#81348 = CARTESIAN_POINT ( 'NONE',  ( 6.369083545433415594, 2.098215621258665564, -0.6323776016037768732 ) ) ;
#81349 = CARTESIAN_POINT ( 'NONE',  ( 1.123892771930210754, 0.3453300891937352568, -1.698893503174392139 ) ) ;
#81350 = CARTESIAN_POINT ( 'NONE',  ( 0.6801582343749744686, 0.3385416670080923507, -1.178068619123886718 ) ) ;
#81351 = CARTESIAN_POINT ( 'NONE',  ( -11.97929049433705551, 13.80000000000000071, -0.7046979865771821894 ) ) ;
#81352 = CARTESIAN_POINT ( 'NONE',  ( 1.381551413260760031, -0.05389312200515179035, 2.170675147484208534 ) ) ;
#81353 = CARTESIAN_POINT ( 'NONE',  ( 2.606657977298726614, 1.900416011228076130, 0.6748465934659984011 ) ) ;
#81354 = CARTESIAN_POINT ( 'NONE',  ( -1.500000000000013101, 0.4520833340161533598, 0.8660254037844403729 ) ) ;
#81355 = CARTESIAN_POINT ( 'NONE',  ( 5.918570133321236604, 1.291915522740747502, -1.429275465086258246 ) ) ;
#81356 = CARTESIAN_POINT ( 'NONE',  ( 1.364683531250000303, 12.50520833367473195, -0.7879004041258355073 ) ) ;
#81357 = CARTESIAN_POINT ( 'NONE',  ( 1.740793075861684303, 1.274151022659695709, -1.819517169034337467 ) ) ;
#81358 = ORIENTED_EDGE ( 'NONE', *, *, #206408, .F. ) ;
#81359 = CARTESIAN_POINT ( 'NONE',  ( 6.439526774796740405, -8.199734048663245289, 6.984891963203204490 ) ) ;
#81360 = CARTESIAN_POINT ( 'NONE',  ( -1.402160292154681736E-14, -0.9124999999999769962, -1.732050807568870754 ) ) ;
#81361 = CARTESIAN_POINT ( 'NONE',  ( 9.738834413317897898, 10.25639499182604730, 0.000000000000000000 ) ) ;
#81362 = DIRECTION ( 'NONE',  ( -0.000000000000000000, -1.000000000000000000, -0.000000000000000000 ) ) ;
#81363 = EDGE_CURVE ( 'NONE', #115330, #24518, #63350, .T. ) ;
#81364 = CARTESIAN_POINT ( 'NONE',  ( 5.442807971621070884, -1.376865196755885146, -1.064510927867247769 ) ) ;
#81365 = CARTESIAN_POINT ( 'NONE',  ( 3.508209890309890167, 1.962046631884439174, 0.002529298861464468473 ) ) ;
#81367 = CARTESIAN_POINT ( 'NONE',  ( -6.019457014787517046, 9.006155036351978893, 1.082531754730548412 ) ) ;
#81366 = CARTESIAN_POINT ( 'NONE',  ( 3.649115900372475796, 7.409052317076538330, 1.040834085586084257E-14 ) ) ;
#81368 = CARTESIAN_POINT ( 'NONE',  ( 5.755082894556171169, 5.678961229929130106, -0.4337107928850430505 ) ) ;
#81369 = CARTESIAN_POINT ( 'NONE',  ( 5.026804934256954738, 2.162974397647707825, 0.6633081500663459140 ) ) ;
#81370 = CARTESIAN_POINT ( 'NONE',  ( 1.152864133210535824, -0.4991712053786099279, -2.001264041248071113 ) ) ;
#81371 = CARTESIAN_POINT ( 'NONE',  ( -7.477485413136760073, 8.682486722536401302, -1.199719254218446718 ) ) ;
#81372 = CARTESIAN_POINT ( 'NONE',  ( 2.571453329723889958, 0.1116048768269807673, -2.259888279461387040 ) ) ;
#81373 = ORIENTED_EDGE ( 'NONE', *, *, #167443, .F. ) ;
#81374 = CARTESIAN_POINT ( 'NONE',  ( -1.201851678989727383E-14, 1.493750000682814383, 1.732050807568877637 ) ) ;
#81375 = CARTESIAN_POINT ( 'NONE',  ( 2.829206387438303327, -1.746784236434804072, 0.6695917499066756928 ) ) ;
#81376 = CARTESIAN_POINT ( 'NONE',  ( 1.459138885926267504, -1.646488293146914472, -0.5446327844310631106 ) ) ;
#81377 = CARTESIAN_POINT ( 'NONE',  ( 4.827760788416924242, 1.126602223531171898, -1.879657820484957664 ) ) ;
#81378 = CARTESIAN_POINT ( 'NONE',  ( 0.3236265600991515834, -0.1057403636935544400, 2.204373366691187108 ) ) ;
#81379 = CARTESIAN_POINT ( 'NONE',  ( 4.241217004700631676, -1.882188537963986219, 1.063020064016991117 ) ) ;
#81380 = CARTESIAN_POINT ( 'NONE',  ( 4.242085645372923430, 0.5190250516928176516, 1.871238508296804604 ) ) ;
#81381 = CARTESIAN_POINT ( 'NONE',  ( -4.568734577680899633, 4.432537883490215158, -0.7216878364870207285 ) ) ;
#81382 = B_SPLINE_SURFACE_WITH_KNOTS ( 'NONE', 1, 3, ( 
 ( #51566, #117691, #85114, #134962, #35289, #167442, #151200, #128272, #95701, #178001, #195314, #196377, #113063, #160675, #77284, #44815, #11203, #193165, #45878, #144470, #112000, #62113, #61037, #12271, #161756, #32806, #210475, #13346, #179069, #79421, #145538, #31753, #147634, #143396, #46945, #14398, #209393, #211536, #64244, #80489, #163890, #30689, #159605, #63171, #129337, #29615, #78347, #28541, #97825, #197424, #96771, #194234, #162822, #180127, #114135, #146588, #65278, #212605, #94632, #48019, #127198, #130387, #15465, #110920, #176925, #81551, #213652, #49066, #131424, #115186, #181181, #19738, #133540, #3471, #100987, #164934, #4528, #66333, #102071, #98881, #99939, #85817, #53317, #167077, #118380, #34914, #2398, #70603, #132478, #69540, #198479, #136717, #184368, #50125, #1338, #263, #182235, #135647, #68477, #134604, #52253, #35991, #116246, #54393, #119450, #149761, #151897, #148693, #185437, #18668, #168136, #16525, #117312, #201670, #86886, #37057, #200606, #83671, #103139, #67399, #33859, #166002, #84748, #169198, #20791, #51189, #17587, #199547, #202743, #152953, #120532, #183308, #150836, #186510, #82608, #105923, #169803, #70145, #88576, #171948, #23537, #201215, #22464, #183917, #151437, #139462, #56063, #205493, #87502, #54997, #187113, #85355, #19273, #204410, #52855, #167672, #86427, #153567, #3008, #73358, #121149, #37676, #203345, #103753, #21392, #5136, #168738, #188181, #152492, #4075, #104827, #117923, #69078, #38746, #155699, #71212, #135198, #35528, #120065, #118989, #20341, #184967, #137328, #39816, #170873, #89646, #101604, #154633, #7281, #6213, #136257, #122220, #202277, #36593, #72284, #102680, #138392, #53928, #186041, #76567, #75509, #208688, #157843, #107001, #90716, #43039, #158898, #123293, #127557, #59248, #159962, #174107, #207630, #189257, #91787, #77637, #173026, #141621, #12626, #57127, #25679, #93922, #161031, #125406, #9439, #156778, #144824, #78697, #24607, #193526, #191372, #209754, #176222, #126476, #109151, #28900, #8365, #45168, #44095, #175164, #26751, #111280, #177285, #40896, #94985, #92852, #10494, #27824 ),
 ( #58192, #142678, #74448, #108078, #60317, #192440, #110215, #11567, #143759, #140552, #206565, #61395, #124351, #190308, #41966, #115530, #65618, #607, #164227, #84025, #64593, #130732, #80848, #149031, #210831, #196725, #146939, #211891, #79768, #82958, #34209, #163172, #113417, #48365, #16877, #165283, #97120, #116592, #212954, #145882, #99234, #62456, #129684, #66674, #128619, #162107, #114478, #194585, #182586, #178360, #213998, #46231, #63530, #197772, #132822, #180476, #15815, #32093, #98179, #100282, #29968, #181525, #96054, #166348, #81900, #13696, #179424, #112348, #195668, #33153, #147988, #131768, #49409, #198826, #47303, #17939, #50471, #31044, #14757, #199898, #104565, #69883, #21130, #1688, #168481, #54732, #138134, #22197, #53668, #134943, #137063, #200949, #19016, #183662, #86168, #170610, #38488, #102413, #51545, #167424, #39550, #88310, #204143, #118726, #152238, #20079, #185778, #169549, #119799, #133892, #120883, #35266, #67742, #101343, #36335, #52598, #3810, #184711, #117669, #151181, #135994, #23276, #202008, #37412, #103488, #87234, #153298, #154374, #55798, #85096, #4874, #70953, #2751, #203088, #186857, #5951, #72021, #121953, #150115, #187919, #105651, #171679, #68821, #89387, #157591, #173850, #90453, #172769, #178905, #130218, #41715, #206311, #144309, #112894, #46780, #190063, #212433, #25426, #24343, #195146, #179961, #8110, #96600, #155436, #40639, #106741, #123045, #196212, #13179, #64075, #7021, #79257, #124099, #211372, #29449, #107825, #139198, #188996, #75257, #194060, #73097, #162652, #91533, #30519, #57935, #9186, #205228, #210307, #14223, #56869, #61943, #47853, #156519, #128102, #129168, #113964, #45713, #111831, #74198, #140292, #177835, #95540, #80318, #161590, #146420, #62998, #145374, #17421, #3302, #65113, #167964, #18501, #83504, #94, #19571, #85645, #163717, #151731, #149586, #198312, #2229, #69371, #135479, #115016, #150668, #97659, #131269, #53147, #184200, #119278, #1170, #183146, #100823, #213491, #147469, #118213, #181012, #81386, #66159, #67236, #197256, #48895, #32634, #98710, #166908, #35823, #199375, #31585 ) ),
 .UNSPECIFIED., .F., .T., .F.,
 ( 2, 2 ),
 ( 4, 2, 2, 2, 2, 2, 2, 2, 2, 2, 2, 2, 2, 2, 2, 2, 2, 2, 2, 2, 2, 2, 2, 2, 2, 2, 2, 2, 2, 2, 2, 2, 2, 2, 2, 2, 2, 2, 2, 2, 2, 2, 2, 2, 2, 2, 2, 2, 2, 2, 2, 2, 2, 2, 2, 2, 2, 2, 2, 2, 2, 2, 2, 2, 2, 2, 2, 2, 2, 2, 2, 2, 2, 2, 2, 2, 2, 2, 2, 2, 2, 2, 2, 2, 2, 2, 2, 2, 2, 2, 2, 2, 2, 2, 2, 2, 2, 2, 2, 2, 2, 2, 2, 2, 2, 2, 2, 2, 2, 2, 2, 2, 2, 2, 2, 2, 2, 2, 2, 2, 2, 2, 2, 4 ),
 ( 0.000000000000000000, 1.000000000000000000 ),
 ( 0.0003308050673979778117, 0.0003990699536394003003, 0.0004673348398808227890, 0.0005355997261222453319, 0.0006038646123636677663, 0.0007403943848465126352, 0.0008769241573293576125, 0.0009110566004500689381, 0.0009451890435707801554, 0.001013453929812202590, 0.001081718816053625024, 0.001149983702295047459, 0.001286513474777892328, 0.001354778361019314762, 0.001388910804140025979, 0.001423043247260737413, 0.001491308133502160065, 0.001559573019743582499, 0.001696102792226427368, 0.001764367678467849802, 0.001832632564709272237, 0.001900897450950694671, 0.001969162337192117106, 0.002037427223433539540, 0.002105692109674961975, 0.002173956995916384409, 0.002242221882157806843, 0.002310486768399229278, 0.002344619211519940495, 0.002378751654640651712, 0.002515281427123497015, 0.002651811199606342317, 0.002720076085847764752, 0.002788340972089187186, 0.002856605858330609621, 0.002924870744572032055, 0.003061400517054876924, 0.003129665403296299359, 0.003197930289537721793, 0.003266195175779144227, 0.003334460062020566662, 0.003402724948261989096, 0.003470989834503411531, 0.003607519606986256400, 0.003675784493227678834, 0.003709916936348390051, 0.003744049379469101269, 0.003812314265710523703, 0.003880579151951946137, 0.004017108924434791006, 0.004085373810676213441, 0.004153638696917635875, 0.004187771140038347092, 0.004221903583159058310, 0.004290168469400480744, 0.004358433355641903179, 0.004426698241883325613, 0.004494963128124748047, 0.004529095571245459265, 0.004563228014366170482, 0.004631492900607592916, 0.004699757786849016218, 0.004836287559331861954, 0.004904552445573284389, 0.004972817331814706823, 0.005041082218056129258, 0.005109347104297551692, 0.005177611990538974127, 0.005245876876780396561, 0.005314141763021818995, 0.005382406649263241430, 0.005450671535504663864, 0.005518936421746086299, 0.005587201307987508733, 0.005655466194228931168, 0.005791995966711776037, 0.005860260852953198471, 0.005928525739194620905, 0.005962658182315332123, 0.005996790625436043340, 0.006065055511677465774, 0.006133320397918888209, 0.006201585284160310643, 0.006269850170401733078, 0.006338115056643155512, 0.006406379942884577947, 0.006440512386005289164, 0.006474644829126000381, 0.006611174601608845250, 0.006747704374091690119, 0.006815969260333112553, 0.006850101703453823770, 0.006884234146574534988, 0.006952499032815957422, 0.007020763919057379857, 0.007157293691540224725, 0.007225558577781647160, 0.007293823464023069594, 0.007327955907143780812, 0.007362088350264492029, 0.007430353236505915331, 0.007498618122747338632, 0.007566883008988761067, 0.007635147895230183501, 0.007703412781471605936, 0.007771677667713028370, 0.007805810110833739587, 0.007839942553954450805, 0.007908207440195873239, 0.007976472326437295673, 0.008113002098920140542, 0.008181266985161562977, 0.008249531871402985411, 0.008317796757644407846, 0.008386061643885830280, 0.008454326530127252715, 0.008522591416368675149, 0.008590856302610097583, 0.008659121188851520018, 0.008727386075092942452, 0.008761518518213653670, 0.008795650961334364887, 0.008932180733817209756, 0.009068710506300054625 ),
 .UNSPECIFIED. ) ;
#81383 = EDGE_CURVE ( 'NONE', #88486, #4353, #212397, .T. ) ;
#81384 = LINE ( 'NONE', #94464, #191503 ) ;
#81385 = CARTESIAN_POINT ( 'NONE',  ( 0.5624999999999944489, -1.451031289061000207, -1.451031289061098795 ) ) ;
#81386 = CARTESIAN_POINT ( 'NONE',  ( 4.050410598061423784, 7.525715715152009544, -0.4746587800704554772 ) ) ;
#81387 = DIRECTION ( 'NONE',  ( -3.330669073875478989E-16, 3.330669073875478989E-16, 1.000000000000000000 ) ) ;
#81388 = CARTESIAN_POINT ( 'NONE',  ( -1.360316468750007779, 2.390625000341400685, -1.734723475976807094E-15 ) ) ;
#81389 = CARTESIAN_POINT ( 'NONE',  ( 5.291638762709002464, 1.525045427759319727, -1.319226660814104335 ) ) ;
#81390 = CARTESIAN_POINT ( 'NONE',  ( -2.453662613948990323, 5.806430783008362795, -0.7216878364870257245 ) ) ;
#81391 = CARTESIAN_POINT ( 'NONE',  ( 7.958799866421889746, 9.244020251369077457, -1.199719254218441611 ) ) ;
#81392 = CARTESIAN_POINT ( 'NONE',  ( 3.379725431556547477, 7.165039780116438273, -1.734723475976807094E-15 ) ) ;
#81394 = DIRECTION ( 'NONE',  ( 1.000000000000000000, 0.000000000000000000, 0.000000000000000000 ) ) ;
#81393 = CARTESIAN_POINT ( 'NONE',  ( 3.615676881913011176, -1.798418494116042821, 0.3134422064149794407 ) ) ;
#81395 = CARTESIAN_POINT ( 'NONE',  ( 11.01135777277262306, 11.00624935217894418, -1.400000000000002132 ) ) ;
#81396 = ORIENTED_EDGE ( 'NONE', *, *, #11376, .F. ) ;
#81397 = CARTESIAN_POINT ( 'NONE',  ( -5.438229012412911345, 5.517224400669388018, -0.7216878364870338292 ) ) ;
#81398 = UNCERTAINTY_MEASURE_WITH_UNIT (LENGTH_MEASURE( 1.000000000000000082E-05 ), #207681, 'distance_accuracy_value', 'NONE');
#81399 = DIRECTION ( 'NONE',  ( 1.000000000000000000, 0.000000000000000000, 0.000000000000000000 ) ) ;
#81400 = CARTESIAN_POINT ( 'NONE',  ( -8.239604668803112375, 10.63595808506888396, -1.599625672291263179 ) ) ;
#81401 = CARTESIAN_POINT ( 'NONE',  ( 0.2287787457191146345, 1.389782569690813929, -1.465877111898945095 ) ) ;
#81402 = CARTESIAN_POINT ( 'NONE',  ( 1.032067064438058068, -2.067986175307830798, 0.4682213744369929098 ) ) ;
#81403 = ORIENTED_EDGE ( 'NONE', *, *, #121519, .T. ) ;
#81404 = CARTESIAN_POINT ( 'NONE',  ( -5.041653019435350380, 6.975290837464928728, -1.599625672291271394 ) ) ;
#81405 = CARTESIAN_POINT ( 'NONE',  ( 2.842405760359353106, 6.467890487061221272, -0.7998128361456291469 ) ) ;
#81406 = CARTESIAN_POINT ( 'NONE',  ( 6.315316842782157991, -0.2547183123318246256, 2.045024454579154938 ) ) ;
#81407 = CARTESIAN_POINT ( 'NONE',  ( 5.608046130584797950, -0.04667949407829304065, 2.016033753796213635 ) ) ;
#81408 = ORIENTED_EDGE ( 'NONE', *, *, #648, .T. ) ;
#81409 = VERTEX_POINT ( 'NONE', #28697 ) ;
#81410 = VERTEX_POINT ( 'NONE', #211690 ) ;
#81411 = CARTESIAN_POINT ( 'NONE',  ( -8.676328237741483207, 12.20980114641871062, -1.199719254218446718 ) ) ;
#81412 = DIRECTION ( 'NONE',  ( 0.7592566023653005702, -0.6507913734559639396, 0.000000000000000000 ) ) ;
#81415 = EDGE_LOOP ( 'NONE', ( #55610, #74940, #2130, #63269 ) ) ;
#81414 = CARTESIAN_POINT ( 'NONE',  ( 10.95308175811721085, 12.29999999999998295, 1.799999999999999600 ) ) ;
#81413 = CARTESIAN_POINT ( 'NONE',  ( -6.089547271193396227, 7.133501900260939443, -1.199719254218453823 ) ) ;
#81416 = CARTESIAN_POINT ( 'NONE',  ( 6.044612043767858545, 7.151903759757407109, 1.166429756139725660 ) ) ;
#81417 = CARTESIAN_POINT ( 'NONE',  ( 5.360703810585087048, -0.7282664037663032497, 1.880147357087233129 ) ) ;
#81418 = CARTESIAN_POINT ( 'NONE',  ( 5.120983416928425846, -1.747193932927636029, 0.5808180576658967809 ) ) ;
#81419 = CARTESIAN_POINT ( 'NONE',  ( 9.860259297219576169, -8.821010173593821335, -0.6081441828345716116 ) ) ;
#81420 = CARTESIAN_POINT ( 'NONE',  ( 2.790017796326722532, 1.632578265707486098, 1.631241332076227346 ) ) ;
#81421 = CARTESIAN_POINT ( 'NONE',  ( 4.993145711582793744, 9.047363440147082159, -0.7998128361456481317 ) ) ;
#81422 = CARTESIAN_POINT ( 'NONE',  ( 6.274726406708529325, -2.050348626090079840, -0.6846857035173321560 ) ) ;
#81423 = CARTESIAN_POINT ( 'NONE',  ( 5.784525094524856748, 9.900363043587685041, 1.040834085586084257E-14 ) ) ;
#81424 = CARTESIAN_POINT ( 'NONE',  ( 1.259210993675137225, 1.913035009642606754, -0.3336937221413670551 ) ) ;
#81425 = CARTESIAN_POINT ( 'NONE',  ( -4.569261463005423352, 5.289558780716470565, -1.199719254218446718 ) ) ;
#81426 = ORIENTED_EDGE ( 'NONE', *, *, #47233, .T. ) ;
#81427 = CARTESIAN_POINT ( 'NONE',  ( 4.851052417537679240, -1.089491736270932432, 2.023782222440795753 ) ) ;
#81428 = CARTESIAN_POINT ( 'NONE',  ( 0.1753634416057497925, 0.0001173177735149660839, -2.144164757042037017 ) ) ;
#81430 =( GEOMETRIC_REPRESENTATION_CONTEXT ( 3 ) GLOBAL_UNCERTAINTY_ASSIGNED_CONTEXT ( ( #59816 ) ) GLOBAL_UNIT_ASSIGNED_CONTEXT ( ( #155137, #138897, #122728 ) ) REPRESENTATION_CONTEXT ( 'NONE', 'WORKASPACE' ) );
#81429 = CARTESIAN_POINT ( 'NONE',  ( -3.793249116773374396, 7.647484079536056356, 0.7998128361456352531 ) ) ;
#81431 = CARTESIAN_POINT ( 'NONE',  ( 3.063207453921251489, 0.2760179531714930246, -1.850060308400132358 ) ) ;
#81432 =( BOUNDED_SURFACE ( )  B_SPLINE_SURFACE ( 3, 2, ( 
 ( #91706, #25592, #9354 ),
 ( #121059, #158814, #204317 ),
 ( #191287, #75428, #88487 ),
 ( #124268, #187026, #40810 ) ),
 .UNSPECIFIED., .F., .F., .T. ) 
 B_SPLINE_SURFACE_WITH_KNOTS ( ( 4, 4 ),
 ( 3, 3 ),
 ( 8.470329472543003391E-22, 3.124390317667046857E-05 ),
 ( 0.000000000000000000, 1.000000000000000000 ),
 .UNSPECIFIED. ) 
 GEOMETRIC_REPRESENTATION_ITEM ( )  RATIONAL_B_SPLINE_SURFACE ( (
 ( 1.000000000000000000, 0.7071067811861172503, 1.000000000000000000),
 ( 1.000000000000000000, 0.7090998123827566557, 1.000000000000000000),
 ( 1.000000000000000000, 0.7100789167762185938, 1.000000000000000000),
 ( 1.000000000000000000, 0.7100530722022274643, 1.000000000000000000) ) ) 
 REPRESENTATION_ITEM ( '' )  SURFACE ( )  );
#81433 = CIRCLE ( 'NONE', #43417, 0.07999999999999993228 ) ;
#81437 = ADVANCED_FACE ( 'NONE', ( #210635 ), #147788, .T. ) ;
#81436 = CARTESIAN_POINT ( 'NONE',  ( -7.273023059088104425, 7.449891421883056530, 0.000000000000000000 ) ) ;
#81435 = CARTESIAN_POINT ( 'NONE',  ( -1.500000000000015099, 0.6604166673494823447, -0.8660254037844313801 ) ) ;
#81434 = CARTESIAN_POINT ( 'NONE',  ( 1.757924209179074770, 0.7287868685415777037, -1.768279316124596878 ) ) ;
#81438 = CARTESIAN_POINT ( 'NONE',  ( 3.334799921508072806, 2.153101868192684343, 0.4835390122766567433 ) ) ;
#81439 = CARTESIAN_POINT ( 'NONE',  ( 6.983263157960380774, 2.077058603031848527, 2.154533585220330227 ) ) ;
#81440 = CYLINDRICAL_SURFACE ( 'NONE', #85740, 1.250000000000000000 ) ;
#81441 = CARTESIAN_POINT ( 'NONE',  ( 6.007671464186823407, 9.062681570643055906, 1.082531754730549967 ) ) ;
#81442 = CARTESIAN_POINT ( 'NONE',  ( -2.788173145904702555, 6.404619103530779789, -0.7998128361456281477 ) ) ;
#81443 = CARTESIAN_POINT ( 'NONE',  ( -6.075462232255183892, 10.10214001435745246, 0.000000000000000000 ) ) ;
#81444 = CARTESIAN_POINT ( 'NONE',  ( 0.6671782056521896598, 0.1977593025605048904, -1.961437444221861837 ) ) ;
#81445 = ADVANCED_FACE ( 'NONE', ( #193321 ), #194748, .T. ) ;
#81446 = CARTESIAN_POINT ( 'NONE',  ( 1.308152564336163115, -0.5581994038030186900, 2.238931160296030232 ) ) ;
#81447 = CARTESIAN_POINT ( 'NONE',  ( 1.346068015636435522, -0.8851805579040676886, 1.750911360861057142 ) ) ;
#81448 = CARTESIAN_POINT ( 'NONE',  ( 5.612196365462351011, 2.060443358388251323, -0.09580443939274756182 ) ) ;
#81449 = CARTESIAN_POINT ( 'NONE',  ( 4.609409038966229666, 6.400729850259146758, -1.443375672974051449 ) ) ;
#81450 = CARTESIAN_POINT ( 'NONE',  ( 4.518610335104485287, 8.493738834255713854, 0.000000000000000000 ) ) ;
#81451 = ORIENTED_EDGE ( 'NONE', *, *, #110186, .T. ) ;
#81452 = CARTESIAN_POINT ( 'NONE',  ( 1.364683531249990311, 4.446875000341417028, 1.214306433183764966E-14 ) ) ;
#81453 = CARTESIAN_POINT ( 'NONE',  ( -3.475000000000000533, -1.429166666666668473, -2.006292185433948827 ) ) ;
#81454 = CARTESIAN_POINT ( 'NONE',  ( 3.023105065722954787, 5.510411095776657220, 1.082531754730546636 ) ) ;
#81455 = CARTESIAN_POINT ( 'NONE',  ( 1.376089442288459752, -2.118726187661602367, 0.4732455120740781673 ) ) ;
#81457 = CARTESIAN_POINT ( 'NONE',  ( 6.620655732516645742, 0.007553340620044741646, 1.826407896915737794 ) ) ;
#81456 = CARTESIAN_POINT ( 'NONE',  ( -11.86687934130374522, 13.60951949616558565, 1.056332641424306606 ) ) ;
#81458 = CYLINDRICAL_SURFACE ( 'NONE', #165305, 1.249999999999999778 ) ;
#81459 = LINE ( 'NONE', #95608, #25450 ) ;
#81460 = CARTESIAN_POINT ( 'NONE',  ( 1.264687732342294701, -1.688641954842164283, -0.8049673154429252131 ) ) ;
#81461 = CARTESIAN_POINT ( 'NONE',  ( 5.975883356200852425, 1.282301362320131588, 1.740048508431484953 ) ) ;
#81462 = CARTESIAN_POINT ( 'NONE',  ( -6.136274411746873270, 5.997031558969919018, 0.08344787587596068368 ) ) ;
#81463 = CARTESIAN_POINT ( 'NONE',  ( 0.07755575628181145265, 7.629137130509078268, -2.788902932953695846 ) ) ;
#81464 = CARTESIAN_POINT ( 'NONE',  ( -1.402160292154681736E-14, -1.178124999658576311, 1.575800808251672791 ) ) ;
#81465 =( BOUNDED_SURFACE ( )  B_SPLINE_SURFACE ( 3, 3, ( 
 ( #19182, #49556, #36505, #102585, #33303, #168644, #99388, #17037, #119970, #107992, #124263, #103663, #53839, #205400, #73265, #121055, #57040, #54902, #106914, #3982, #189167, #156685, #38654, #169711, #104734, #88482, #206475, #171852, #21301, #188088, #39719, #86332, #185947, #190222, #87408, #23447, #72190, #187022, #70050, #105826, #123206, #136164, #153472, #40806, #203259, #58104, #152403, #71121, #6122, #8276, #5046, #170780, #74360, #20247, #155608, #41881, #90626, #22370, #172939, #137237, #89557, #7192, #139370, #24516, #140463, #202182, #37579, #154541, #138299, #204314, #55971, #122124, #142589, #59164, #47215, #63441, #42948, #207544, #144733, #12538, #60229, #174021, #91702, #127466, #112258, #13609, #109057, #175074, #208597, #44006, #46144, #78611, #195579, #160945, #110125, #193437, #162020, #79684, #26661, #210744, #77547, #178272, #9352, #126389, #62368, #129591, #111190, #29882, #45081, #158809, #75424, #10405, #95966, #92764, #145797, #192348, #27737, #125322, #177193, #28809, #176137, #93831, #159872, #61304, #211803, #128530, #94893, #143670, #25590, #141536, #11476, #209663, #194499, #157754, #191282, #76478, #198737, #15731, #113330, #81816, #33069, #148951, #97033, #167337, #147899, #51456, #14668, #130647, #146850, #165197, #98094, #67656, #522, #117576, #116505, #196639, #183571, #48279, #35177, #64504, #181440, #163087, #180387, #100195, #2663, #133802, #1595, #66590, #151099, #166261, #49331, #132734, #199812, #50384, #101254, #131684, #16790, #182496, #18923, #197686, #82873, #34124, #17851, #83936, #150026, #212869, #80761, #114392, #85008, #179337, #68736, #32011, #134857, #164146, #200863, #30958, #213915, #65538, #115450, #99147, #40281, #42433, #159353, #58657, #56527, #124810, #52510, #3723, #152153, #59718, #69798, #102324, #109619, #86078, #26145, #36245, #190771, #108539, #174569, #138855, #106391, #204872, #122687, #118643, #188650, #156170, #125877, #173501, #141018, #74910, #207026, #184628, #92259, #158305, #57594, #143154, #168397, #9896, #19994, #75973, #90105, #172414, #24003, #73838, #41365, #189712, #175624, #93317, #43499, #25076, #142076, #7751, #208090, #139934, #205961, #123751, #107476, #91179, #8833, #157238, #191836, #27211, #10950, #77024, #63989, #81307, #179878, #29363, #46692, #129082, #32549, #12028, #130141, #112810, #82355, #110675, #211289, #30435, #95458, #13087, #160422, #44559, #80235, #111742, #209148, #177748, #195053, #96521, #192903, #48813, #31503, #161507, #147384, #176675, #163634, #131188, #79167, #78099, #145283, #62913, #180928, #146334, #210220, #162569, #14142, #60787, #144226, #98626, #61856, #212348, #178823, #196130, #28287, #47770, #97577, #94382, #128023, #15217, #113883, #164687, #126946, #45625, #213410, #197177, #193977, #65032, #114930, #16270, #69280, #37879, #4274, #150580, #36797, #50935, #19478, #167878, #3212, #151643, #101810, #119188, #49866, #85553, #135393, #1084, #54134, #201415, #117059, #33612, #21585, #103955, #17338, #181981, #185173, #53054, #34670, #148445, #66079, #102882, #86626, #202481, #83420, #149501, #183056, #18414, #20542, #168940, #169998, #152693, #84489, #70345, #136462, #120269, #67148, #186244, #52003, #15, #198230, #100740, #132220, #115992, #99683, #165752, #133283, #199290, #166821, #2142, #68219 ),
 ( #134350, #200353, #118129, #184114, #35735, #155900, #187319, #90911, #156976, #106130, #172153, #23745, #189456, #158045, #124550, #8565, #205693, #175361, #203543, #89850, #123492, #122424, #7487, #38947, #137528, #173230, #204614, #87690, #56265, #73569, #41098, #71416, #141823, #58394, #188381, #174301, #55197, #42165, #9631, #139671, #171068, #57328, #107207, #59454, #24810, #88776, #74646, #140751, #153765, #105030, #191570, #154834, #206762, #190508, #40019, #121344, #108280, #25876, #22665, #6418, #91986, #75708, #125611, #5333, #138591, #207825, #43234, #72490, #109351, #163363, #26942, #162294, #130918, #97304, #29094, #129873, #143952, #112533, #46416, #96243, #30155, #194779, #212076, #142880, #178545, #13881, #94118, #147121, #79960, #209947, #126673, #114669, #196911, #110411, #60512, #63715, #146063, #127755, #93049, #159090, #195856, #179609, #81034, #176414, #28021, #61586, #111474, #113605, #47496, #48551, #31230, #177479, #14939, #213147, #64777, #160159, #10688, #145010, #76758, #208882, #193712, #192636, #44289, #11757, #77831, #45355, #95178, #161227, #12814, #78887, #211016, #62639, #128797, #200097, #168682, #86371, #49598, #85297, #84230, #52796, #16003, #806, #151383, #136203, #117869, #118935, #51746, #165478, #82088, #17074, #184915, #115722, #152440, #133019, #34406, #65810, #183860, #35473, #199018, #50665, #116791, #67944, #36539, #2953, #101551, #150318, #53875, #148181, #182788, #1884, #66874, #100478, #131957, #214182, #167620, #83152, #180663, #149232, #166554, #134089, #164419, #20286, #69024, #18142, #102626, #197967, #135141, #4019, #19219, #181713, #201157, #70088, #202221, #32288, #33342, #98354, #99424, #185984, #71156, #9385, #187059, #123238, #171889, #154581, #169749, #73302, #8311, #21337, #121092, #90658, #88519, #91736, #37618, #170819, #105863, #41914, #38692, #204350, #108025, #120008, #40840, #75456, #190256, #122160, #74396, #22410, #205438, #139404, #189203, #106949, #57074, #156720, #87443, #172972, #24551, #104770, #25624, #140497, #6158, #5081, #207577, #141569, #203293, #153512, #206507, #58138, #72227, #103698, #137273, #124297, #174051, #157789, #54940, #138334, #56008, #188127, #39758, #23486, #89593, #155642, #7226, #128564, #145829, #29915, #93867, #111226, #193472, #97064, #76512, #159905, #211834, #175110, #142623, #92798, #177229, #44040, #13641, #94930, #63471, #62401, #208632, #129626, #60265, #195611, #10440, #127501, #109094, #126422, #46176, #163117, #79713, #162051, #160979, #14699, #112290, #209698, #12570, #47248, #78642, #113362, #77583, #28842, #194529, #179367, #143706, #144768, #178306, #210778, #95997, #30989, #158843, #42984, #192386, #80793, #125353, #146883, #110159, #59197, #176171, #191316, #26697, #27771, #11512, #61342, #45116, #197716, #199841, #102351, #1625, #213945, #67684, #212903, #164176, #98125, #2691, #15761, #48309, #52536, #32038, #183598, #196669, #133830, #51483, #117606, #81846, #49358, #147929, #65566, #64536, #131713, #99173, #68763, #116533, #83964, #17879, #150053, #130680, #35205, #101281, #549, #86108, #114420, #167364, #180420, #18952, #33098, #115477, #181469, #16817, #198764, #132761, #118670, #36274, #200890, #182522, #85036, #165225, #151125, #82902, #148975, #66614, #50414, #34152, #166290, #100222, #134883, #184653 ),
 ( #168423, #20019, #135931, #153238, #74133, #3749, #57874, #37351, #187860, #87168, #90388, #140227, #69823, #23213, #24282, #55736, #137001, #139137, #41652, #155373, #4809, #6958, #152179, #103425, #169487, #156457, #21070, #201949, #206248, #185718, #122977, #53605, #73039, #205166, #56807, #70891, #203029, #54670, #120818, #119739, #186795, #38424, #8043, #121891, #89326, #171619, #188936, #104503, #40575, #106681, #154314, #25368, #170547, #172704, #22131, #124036, #88244, #5887, #71960, #138070, #204083, #39487, #190002, #107766, #173792, #105585, #176970, #192127, #28587, #108832, #91468, #159652, #175916, #92547, #44858, #209437, #93607, #10186, #62156, #157530, #160717, #178043, #128314, #126163, #143440, #11249, #129375, #174858, #43792, #29659, #207323, #26437, #125101, #61081, #76260, #45922, #127241, #95745, #94675, #158586, #161796, #142369, #13387, #42724, #77327, #141311, #208378, #78392, #195354, #112042, #194277, #193211, #46986, #144512, #27507, #110962, #79463, #12311, #145580, #60010, #210520, #211577, #63211, #113102, #179108, #9124, #58944, #75200, #191059, #109905, #150879, #83716, #213694, #130432, #118426, #134643, #114175, #64286, #1380, #149806, #131465, #30730, #162862, #198520, #183355, #84791, #180169, #31795, #65316, #115230, #117357, #67441, #52297, #17630, #181220, #50166, #18708, #2442, #97870, #133586, #148735, #34959, #80531, #197466, #199590, #200648, #182277, #101030, #116287, #15505, #146627, #81592, #167121, #163930, #68516, #49110, #98923, #196418, #33902, #99980, #32847, #164976, #16568, #132522, #96813, #51233, #166046, #303, #14441, #212644, #82651, #66374, #48062, #147677, #135691, #19779, #55496, #86929, #184412, #152996, #104255, #5636, #168180, #24043, #155139, #4572, #56571, #85861, #138899, #106434, #202785, #53357, #54435, #38183, #156215, #121650, #185478, #137830, #203851, #36031, #201716, #73884, #37103, #187617, #21889, #70646, #151936, #39245, #72799, #3510, #103183, #6720, #136756, #7791, #102109, #20831, #170301, #172456, #169243, #120577, #90147, #69580, #105337, #139977, #171374, #22967, #89082, #204918, #122730, #119491, #188693, #40329, #186554, #205999, #57635, #87999, #154071, #71717, #13132, #207067, #157281, #94423, #176714, #9938, #123794, #41404, #77067, #61900, #177790, #58697, #124845, #92300, #208129, #210262, #28327, #145327, #110714, #59758, #143196, #111784, #29406, #190811, #160462, #27249, #128061, #173543, #158344, #12070, #79209, #60827, #194017, #209187, #108581, #25117, #174609, #45667, #42471, #95498, #76013, #191877, #8870, #126988, #192947, #142116, #125918, #43537, #10992, #161545, #78138, #44599, #93356, #211328, #91220, #109660, #159393, #175662, #144269, #74949, #141060, #189752, #107514, #26185, #36577, #100520, #117906, #200136, #103735, #83189, #166594, #4057, #181750, #149272, #99462, #183899, #50704, #20324, #101588, #70127, #69061, #851, #136240, #66916, #202261, #17112, #134127, #115760, #133057, #52836, #169786, #86410, #168721, #167656, #21375, #118972, #1925, #19256, #152477, #85338, #53911, #84269, #35510, #135181, #120047, #150355, #151420, #201196, #2993, #184950, #102663, #165519, #49636, #33381, #186021, #37658, #67984, #199058, #51789, #87483, #153549, #62953, #116828, #129122, #195099, #182830, #34445, #18183, #72266 ),
 ( #71195, #56047, #205479, #141605, #138374, #89631, #207613, #5119, #140534, #109134, #75493, #7265, #108063, #122203, #90699, #24592, #74434, #8349, #173011, #190293, #121133, #156761, #206546, #204392, #125389, #58175, #188165, #104811, #92835, #175147, #88558, #38730, #41951, #124335, #105905, #137311, #203327, #174089, #157827, #59231, #154618, #6197, #39798, #155683, #91770, #25661, #26733, #9423, #73342, #191355, #43020, #54980, #171930, #187096, #123280, #170856, #22446, #23524, #139444, #57111, #189241, #40881, #106986, #143742, #208670, #209736, #31025, #27807, #64573, #111262, #12607, #44077, #162088, #13678, #177265, #28881, #94964, #46212, #14737, #195650, #79749, #62437, #32074, #60301, #161012, #194566, #193509, #78679, #110196, #126459, #144806, #96036, #93905, #158879, #210812, #112328, #142660, #212936, #129663, #45150, #97101, #178342, #29951, #10475, #176206, #48346, #11549, #145865, #128600, #211872, #192423, #63511, #47285, #159945, #77619, #113397, #127537, #130715, #76550, #61380, #179405, #80829, #163153, #146918, #196706, #114457, #180457, #118703, #151158, #50450, #101319, #16857, #1663, #84002, #133870, #67719, #150092, #183638, #147967, #199877, #51520, #33133, #200926, #117645, #82938, #65599, #102390, #184691, #49392, #131748, #35244, #167401, #149011, #98162, #15796, #18991, #2727, #52574, #115511, #181504, #587, #198802, #85073, #68800, #164209, #134919, #116568, #36311, #81882, #213979, #66653, #197753, #99213, #165262, #182562, #132799, #34185, #100259, #166326, #17916, #96743, #62081, #127163, #128239, #163857, #160641, #197396, #29584, #145509, #176895, #80460, #146558, #95672, #161725, #13318, #179039, #147604, #114107, #212578, #195283, #164905, #193135, #79390, #113033, #111967, #211507, #28508, #44783, #63144, #14369, #12241, #77247, #129306, #30658, #61006, #131399, #47992, #177970, #15437, #110889, #31722, #213622, #46915, #78315, #162791, #64217, #49038, #130357, #144439, #94598, #180098, #196349, #97797, #143364, #209361, #81526, #65250, #115158, #210442, #194202, #45848, #181153, #32775, #98854, #86111, #135934, #18955, #213947, #180424, #147932, #552, #118673, #17882, #199844, #133833, #51486, #32042, #117609, #85039, #116536, #201952, #98129, #2694, #164180, #151127, #148978, #16820, #81850, #132764, #100225, #34155, #168426, #152182, #102354, #83967, #183601, #66617, #35209, #131716, #114424, #182526, #198767, #115480, #67687, #150056, #166293, #33102, #197719, #101285, #3752, #68766, #134886, #50417, #1628, #167367, #69826, #49360, #200893, #52539, #15765, #181472, #65569, #184657, #99176, #36277, #20022, #165228, #82905, #137005, #206251, #203032, #57877, #4813, #121894, #103428, #120821, #40578, #157533, #8046, #156460, #89329, #91472, #106684, #204086, #6961, #140230, #73042, #41656, #71963, #171622, #56810, #74137, #138073, #23216, #188939, #155376, #139140, #205169, #87172, #37354, #54673, #190005, #119742, #173795, #153240, #122980, #186798, #124039, #107769, #185721, #172708, #25371, #24285, #38427, #90391, #9128, #75203, #70894, #104506, #105588, #170550, #141314, #53609, #169490, #21072, #22134, #88247, #154317, #5891, #55739, #187863, #39490, #60013, #194281, #96816, #161800, #95748, #28591, #30734, #45926, #143444, #160722, #79467, #12315, #195358, #11252, #110966 ),
 ( #62160, #210524, #78396, #178046, #108835, #144516, #112046, #126166, #113107, #29664, #175919, #92550, #80535, #162865, #76263, #26440, #13390, #145584, #93610, #207326, #125105, #128318, #211581, #46990, #142372, #208382, #27510, #77331, #63215, #129379, #179112, #191062, #14445, #159655, #58947, #42727, #192130, #174861, #176974, #158589, #10189, #209441, #43795, #109908, #61086, #127245, #193215, #44862, #94679, #131469, #18711, #15510, #52301, #98926, #307, #31799, #149810, #1384, #164980, #16572, #82655, #33906, #2446, #183359, #67445, #50171, #19783, #48067, #148739, #182281, #181224, #66378, #97874, #196422, #132526, #83720, #81596, #146631, #198524, #99983, #130435, #200651, #117361, #32852, #84795, #114179, #150883, #133590, #147681, #68520, #213698, #134647, #163934, #116291, #180173, #65321, #199594, #36035, #101035, #34964, #166050, #184417, #51237, #17635, #167125, #118430, #102115, #168184, #212648, #64289, #197471, #49114, #115234, #55500, #6724, #121654, #39249, #105341, #119496, #69584, #86934, #7795, #151940, #206003, #185482, #187621, #20835, #24048, #73888, #3514, #171379, #172461, #203855, #70650, #72802, #189756, #89088, #152999, #155142, #85865, #37108, #103186, #90151, #169247, #135695, #139981, #4576, #56575, #201720, #138903, #204922, #106438, #57638, #107518, #122734, #136761, #53362, #202789, #186558, #156219, #22970, #188697, #40332, #123798, #54439, #41409, #173547, #88003, #120581, #38187, #104258, #170304, #21892, #154074, #5641, #71721, #137834, #10996, #159397, #79213, #62957, #13136, #209191, #110718, #125922, #176718, #42475, #25121, #93361, #109664, #26189, #192951, #143201, #27253, #158348, #108585, #28331, #129126, #194021, #210266, #59762, #77072, #60831, #195103, #174613, #191881, #177794, #141064, #92304, #58701, #126992, #9942, #45671, #44603, #145331, #91225, #94427, #111788, #160467, #76017, #12074, #46739, #78142, #142120, #144273, #157285, #190815, #124850, #29411, #208134, #74953, #211332, #43541, #61904, #8874, #128065, #95502, #161549, #112852, #207071, #175666, #64033, #30478, #212391, #65073, #183100, #82398, #49912, #198269, #116033, #96563, #182020, #83463, #180970, #52046, #162610, #67191, #14186, #149543, #213450, #81346, #146377, #197216, #164724, #98669, #18458, #2186, #166863, #148488, #33650, #131228, #99724, #196172, #178867, #32592, #48856, #179921, #132262, #56, #16313, #97619, #47812, #165796, #68262, #133328, #1129, #114970, #66119, #17380, #134394, #113925, #199332, #117099, #80279, #31543, #130179, #50977, #163676, #34711, #100781, #84535, #150625, #15259, #200397, #147426, #122471, #69325, #186288, #167924, #185217, #105079, #7533, #72540, #6463, #153812, #155948, #171117, #54174, #71461, #204660, #137574, #106176, #136505, #21629, #121391, #138638, #202525, #87737, #38994, #5384, #203592, #55244, #151687, #101856, #119234, #40066, #184159, #23790, #3257, #187364, #53101, #56310, #88825, #19523, #22710, #154880, #36841, #89897, #188431, #86669, #135435, #205740, #73616, #201457, #102923, #172202, #139716, #4318, #118172, #35780, #85599, #168984, #20584, #152736, #70388, #120314, #37926, #104000, #170043, #177527, #41146, #12864, #9678, #45405, #29140, #140795, #176458, #175403, #144003, #107256, #92032, #28070, #78938, #208927, #209995, #76807, #42209 ),
 ( #141864, #207874, #159135, #127804, #94164, #126721, #26987, #145060, #173276, #59496, #93094, #158090, #75754, #8609, #24856, #125653, #60562, #206807, #57373, #191615, #10737, #90958, #111521, #160204, #43277, #61637, #157023, #11806, #193758, #109398, #58440, #142927, #192682, #95227, #44335, #124595, #110457, #77881, #123536, #74692, #161277, #190553, #189501, #108326, #174346, #25924, #167404, #102393, #112587, #212126, #184694, #182565, #185758, #62688, #50453, #199880, #135972, #63764, #84005, #201988, #211063, #134923, #103466, #69863, #1666, #168460, #116571, #85076, #18994, #68803, #2731, #151161, #52577, #34188, #96295, #87212, #169528, #80010, #30208, #36314, #118706, #100262, #128847, #194829, #200929, #152219, #53645, #146115, #132802, #166329, #150095, #86148, #20058, #119778, #46464, #21108, #17919, #37391, #178598, #198805, #3788, #117648, #162347, #13930, #67722, #133873, #51523, #183641, #35247, #101322, #138113, #203068, #204124, #25406, #22173, #58983, #105628, #6998, #38467, #156498, #8088, #171657, #23254, #89367, #40617, #9162, #190041, #74176, #56850, #26475, #54711, #155415, #188973, #187900, #73076, #104543, #120862, #139177, #90429, #88288, #153276, #205208, #106721, #137041, #207363, #124077, #39530, #91509, #186835, #107804, #75238, #123022, #154352, #172748, #24323, #125139, #140268, #5930, #206288, #57912, #4853, #170588, #42765, #72002, #41693, #173829, #157569, #55776, #141348, #191097, #121933, #108872, #174896, #70932, #64323, #158627, #143479, #78429, #14480, #159685, #177007, #80569, #92585, #13425, #196457, #162898, #94712, #195395, #209475, #178081, #112079, #161837, #95780, #45958, #63251, #208414, #29698, #79501, #11286, #212682, #47025, #128350, #130467, #145619, #28624, #211615, #179147, #129412, #146668, #111003, #210559, #113140, #30771, #160754, #62194, #96850, #194317, #48100, #114212, #126203, #76298, #93642, #180210, #10224, #142406, #192165, #60048, #27547, #43826, #109942, #175951, #77365, #61117, #127278, #193249, #44896, #12349, #144551, #32885, #35000, #31833, #197506, #131502, #36070, #49149, #81629, #85903, #65355, #2481, #15544, #167159, #101072, #52338, #3551, #53394, #150920, #115266, #97908, #181258, #132558, #102152, #149849, #117398, #51274, #183395, #163968, #18746, #68557, #33944, #119531, #147714, #134684, #213732, #200687, #66413, #148771, #98962, #50206, #17671, #166083, #151977, #69621, #19818, #1418, #84831, #198558, #118466, #165013, #16608, #100019, #116324, #82689, #199628, #67481, #83757, #340, #182315, #184452, #135731, #168218, #201753, #133626, #23004, #105377, #8909, #202822, #5676, #123832, #86967, #54471, #4610, #89122, #170341, #140015, #6760, #189794, #188731, #120615, #41445, #186593, #107553, #136797, #39282, #20868, #38220, #172498, #74989, #206040, #24084, #91259, #169282, #141097, #137870, #173587, #157318, #104293, #90189, #155176, #57674, #153036, #71754, #156252, #207108, #122771, #25157, #204959, #21926, #70684, #88035, #58735, #154107, #185517, #203890, #171416, #55535, #40369, #106471, #121689, #187656, #72835, #138939, #37141, #7831, #73922, #56607, #103223, #26222, #127025, #160500, #159430, #143231, #76051, #174646, #192983, #61937, #59798, #124887, #44637, #12105, #108618, #178899, #95534, #11029, #211366, #92338, #79249, #46773 ),
 ( #14217, #191911, #128095, #176750, #77107, #158380, #78175, #13170, #9973, #125955, #161583, #93393, #96594, #190851, #175697, #110752, #112887, #43575, #209221, #30513, #42512, #45705, #80312, #195137, #28365, #145367, #27287, #210297, #144303, #194053, #111824, #177826, #62991, #142152, #29443, #129160, #109693, #162644, #146412, #60863, #208167, #212425, #94460, #147461, #97651, #34743, #117135, #164761, #64067, #196204, #17413, #2222, #118207, #213482, #65106, #32625, #148521, #150660, #184194, #16351, #132297, #163710, #67227, #133361, #82431, #87, #66152, #165829, #134430, #100816, #199368, #182055, #151724, #179954, #198304, #99762, #98702, #49944, #15292, #113957, #116065, #1163, #131262, #130211, #33685, #83497, #47846, #35817, #166901, #149579, #68297, #31577, #18494, #200433, #51014, #197249, #183138, #84572, #101893, #52080, #48888, #167958, #19564, #81377, #115008, #85638, #181005, #6502, #55281, #37964, #53141, #171155, #106213, #119271, #4358, #188469, #186330, #189536, #69364, #54215, #203629, #139756, #70427, #87778, #205780, #3296, #138678, #107291, #73656, #5423, #172239, #120353, #88863, #22745, #72577, #204697, #154918, #40101, #185256, #56347, #122509, #136543, #123574, #23827, #104037, #102963, #90998, #173313, #86707, #36880, #89932, #155983, #170083, #135473, #201494, #7571, #57408, #41184, #152776, #202563, #21670, #153852, #24892, #169021, #20619, #71502, #137613, #121429, #187399, #39031, #105115, #61674, #60600, #29179, #206846, #191651, #127842, #112626, #94201, #95268, #176495, #141901, #58478, #207911, #161316, #25963, #158126, #160241, #157061, #108361, #42248, #12900, #174385, #124633, #211103, #190591, #193794, #140833, #77918, #11841, #177566, #128888, #178636, #45443, #92068, #8649, #9717, #43316, #78980, #126759, #28106, #144037, #210034, #74728, #111557, #145099, #159172, #30248, #75793, #62727, #59532, #194869, #109434, #125692, #175440, #27025, #142965, #76846, #46503, #93133, #10772, #192719, #208968, #44373, #110496, #113698, #96332, #164509, #180752, #97395, #49688, #214270, #98445, #15031, #179702, #181803, #134174, #50752, #66971, #131010, #148271, #16093, #200182, #31318, #197002, #34496, #212168, #163451, #129960, #65903, #81123, #116881, #132049, #100570, #99513, #147208, #166643, #213233, #18234, #47584, #82177, #146152, #64865, #83239, #51835, #182880, #199107, #198059, #117953, #149324, #32379, #115816, #84318, #33436, #150404, #114755, #165570, #17165, #1971, #902, #133110, #68034, #183948, #162388, #13965, #195948, #80049, #48637, #63802, #101639, #155731, #135232, #71244, #185003, #188211, #23573, #167705, #121178, #122252, #153599, #20374, #22495, #139497, #38776, #151470, #37709, #137360, #70177, #53959, #201245, #85386, #103785, #187147, #36627, #35558, #169836, #203377, #19307, #89682, #6248, #136289, #39851, #3041, #204442, #171981, #120097, #119021, #186075, #21423, #7316, #104858, #102712, #55030, #170902, #69110, #52886, #205525, #168769, #88607, #87532, #202310, #86459, #154662, #138423, #152523, #4108, #72317, #5171, #73394, #56096, #105957, #57160, #123323, #42002, #59283, #111312, #189286, #110246, #78728, #45199, #191403, #77669, #91820, #60347, #208721, #44126, #192472, #142712, #159994, #90748, #126510, #176255, #108110, #95014, #27856, #157877, #74479 ) ),
 .UNSPECIFIED., .T., .F., .T. ) 
 B_SPLINE_SURFACE_WITH_KNOTS ( ( 4, 3, 4 ),
 ( 4, 1, 1, 1, 1, 1, 1, 1, 1, 1, 1, 1, 1, 1, 1, 1, 1, 1, 1, 1, 1, 1, 1, 1, 1, 1, 1, 1, 1, 1, 1, 1, 1, 1, 1, 1, 1, 1, 1, 1, 1, 1, 1, 1, 1, 1, 1, 1, 1, 1, 1, 1, 1, 1, 1, 1, 1, 1, 1, 1, 1, 1, 1, 1, 1, 1, 1, 1, 1, 1, 1, 1, 1, 1, 1, 1, 1, 1, 1, 1, 1, 1, 1, 1, 1, 1, 1, 1, 1, 1, 1, 1, 1, 1, 1, 1, 1, 1, 1, 1, 1, 1, 1, 1, 1, 1, 1, 1, 1, 1, 1, 1, 1, 1, 1, 1, 1, 1, 1, 1, 1, 1, 1, 1, 1, 1, 1, 1, 1, 1, 1, 1, 1, 1, 1, 1, 1, 1, 1, 1, 1, 1, 1, 1, 1, 1, 1, 1, 1, 1, 1, 1, 1, 1, 1, 1, 1, 1, 1, 1, 1, 1, 1, 1, 1, 1, 1, 1, 1, 1, 1, 1, 1, 1, 1, 1, 1, 1, 1, 1, 1, 1, 1, 1, 1, 1, 1, 1, 1, 1, 1, 1, 1, 1, 1, 1, 1, 1, 1, 1, 1, 1, 1, 1, 1, 1, 1, 1, 1, 1, 1, 1, 1, 1, 1, 1, 1, 1, 1, 1, 1, 1, 1, 1, 1, 1, 1, 1, 1, 1, 1, 1, 1, 1, 1, 1, 1, 1, 1, 1, 1, 1, 1, 1, 1, 1, 1, 1, 1, 1, 1, 1, 1, 1, 1, 1, 1, 1, 1, 1, 1, 1, 1, 1, 1, 1, 1, 1, 1, 1, 1, 1, 1, 1, 1, 1, 1, 1, 1, 1, 1, 1, 1, 1, 1, 1, 1, 1, 1, 1, 1, 1, 1, 1, 1, 1, 1, 1, 1, 1, 1, 1, 1, 1, 1, 1, 1, 1, 1, 1, 1, 1, 1, 1, 1, 1, 1, 1, 1, 1, 1, 1, 1, 1, 1, 1, 1, 1, 1, 1, 1, 1, 1, 1, 1, 1, 1, 1, 1, 1, 1, 1, 1, 1, 1, 1, 1, 1, 1, 1, 1, 1, 1, 1, 1, 1, 1, 1, 1, 1, 1, 1, 1, 1, 1, 1, 1, 1, 1, 1, 1, 1, 1, 1, 1, 1, 1, 1, 1, 1, 1, 1, 1, 1, 4 ),
 ( 0.000000000000000000, 0.5000000000000000000, 1.000000000000000000 ),
 ( 0.000000000000000000, 0.002599888508634240914, 0.005208754120092145765, 0.007813069968323356138, 0.01041690100177071650, 0.01302019566086259385, 0.01562517182793091500, 0.01822893254318404960, 0.02083328139698771564, 0.02343764900838959594, 0.02604139750447371365, 0.02864615928571910553, 0.03124958462592061434, 0.03385442086835698666, 0.03645794792899405279, 0.03906256697173399878, 0.04166661757251870907, 0.04427067912273281725, 0.04687528696281444140, 0.04947881815967773017, 0.05208365228821221909, 0.05468707701066444909, 0.05729184299815447134, 0.05989557646906591704, 0.06249996333325048142, 0.06510433798480201595, 0.06770807906337909798, 0.07031283757201339801, 0.07291626355048291819, 0.07552109983967189577, 0.07812462590386089201, 0.08072924387304455940, 0.08333329402460390445, 0.08593735478041557296, 0.08854196204427712547, 0.09114549249794960672, 0.09375032597506528786, 0.09635375006294695510, 0.09895851527076646170, 0.1015622481948881828, 0.1041666342325376776, 0.1067710083972730206, 0.1093747487337090180, 0.1119795066911244419, 0.1145829320296284648, 0.1171877676425944481, 0.1197912931610935483, 0.1223959103579086161, 0.1249999600491941698, 0.1276040200539713398, 0.1302086268569593308, 0.1328121566649932417, 0.1354169895755736042, 0.1380204131161003600, 0.1406251776355303407, 0.1432289101024236955, 0.1458332954032181272, 0.1484376691708411133, 0.1510414088543486633, 0.1536461663508109643, 0.1562495911381983071, 0.1588544261652600487, 0.1614579512270202244, 0.1640625677415503691, 0.1666666170620310916, 0.1692706764052687440, 0.1718752828374313091, 0.1744788120887783289, 0.1770836445231302458, 0.1796870676051354199, 0.1822918315264069888, 0.1848955636252137269, 0.1874999482789682093, 0.1901043217392619777, 0.1927080608589964439, 0.1953128179847096746, 0.1979162423098047296, 0.2005210768412587219, 0.2031246015352002054, 0.2057292174574958665, 0.2083332664966131842, 0.2109373252677763377, 0.2135419314191336626, 0.2161454602027163274, 0.2187502922511180836, 0.2213537149634070833, 0.2239584783767220588, 0.2265622101965570623, 0.2291665942930569411, 0.2317709675357785548, 0.2343747061808670040, 0.2369794630260087243, 0.2395828869776091552, 0.2421877211037245237, 0.2447912455187418734, 0.2473958609388257068, 0.2499999097859964270, 0.2526039680745227334, 0.2552085740350705789, 0.2578121024397855843, 0.2604169341924902348, 0.2630203566238439872, 0.2656251196193780695, 0.2682288512493328225, 0.2708332348783377697, 0.2734376079932215875, 0.2760413462527663842, 0.2786461029074911444, 0.2812495265743710227, 0.2838543603853929120, 0.2864578846103582599, 0.2890624996182282747, 0.2916665483628478883, 0.2942706062581511572, 0.2968752121178640513, 0.2994787402325856385, 0.3020835717798243114, 0.3046869940190023440, 0.3072917566869088346, 0.3098954882160545599, 0.3124998714673014044, 0.3151042445440625506, 0.3177079825071445485, 0.3203127390615869707, 0.3229161625325003282, 0.3255209961186533163, 0.3281245202424198926, 0.3307291349280532256, 0.3333331836594992104, 0.3359372412509727956, 0.3385418470998076690, 0.3411453750133909280, 0.3437502064453764050, 0.3463536285811206206, 0.3489583910115333087, 0.3515621225289245477, 0.3541665054921307454, 0.3567708786204680238, 0.3593746163761498691, 0.3619793729204284771, 0.3645827962841124981, 0.3671876297356038710, 0.3697911538470093351, 0.3723957683003653041, 0.3749998171080005105, 0.3776038744850206963, 0.3802084804129200468, 0.3828120082142042468, 0.3854168396211344327, 0.3880202617421720235, 0.3906250240252089334, 0.3932287556198868494, 0.3958331383847540352, 0.3984375116543538153, 0.4010412492916836102, 0.4036460059159037717, 0.4062494292610819846, 0.4088542626681055392, 0.4114577868559751161, 0.4140624011669984950, 0.4166664501401745602, 0.4192705073921035863, 0.4218751134889988097, 0.4244786412668108966, 0.4270834727388717056, 0.4296868949339185950, 0.4322916571596854274, 0.4348953889206810253, 0.4374997715768980666, 0.4401041450774376140, 0.4427078826854516369, 0.4453126394797092824, 0.4479160628950952239, 0.4505208963478340434, 0.4531244207009840763, 0.4557290349596088697, 0.4583330841876695483, 0.4609371414038593850, 0.4635417477596745495, 0.4661452756028321986, 0.4687501072302013849, 0.4713535295879656695, 0.4739582918465587991, 0.4765620238628961447, 0.4791664065001429718, 0.4817707803212932793, 0.4843745179890200370, 0.4869792750434049911, 0.4895826986177053142, 0.4921875322063354874, 0.4947910568135764908, 0.4973956711097291539, 0.4999997206820134821, 0.5026037779518089943, 0.5052083846564635605, 0.5078119126537786743, 0.5104167445266291070, 0.5130201671358142201, 0.5156249295173244152, 0.5182286618780244103, 0.5208330445859747915, 0.5234374188174044651, 0.5260411566338674128, 0.5286459140384663913, 0.5312493378603841965, 0.5338541716750782040, 0.5364576966252184720, 0.5390623110488209635, 0.5416663610546670338, 0.5442704184674093115, 0.5468750256108222407, 0.5494785538511040013, 0.5520833860596070508, 0.5546868090089153158, 0.5572915716034309019, 0.5598953043975141153, 0.5624996872658396541, 0.5651040619972180767, 0.5677078000514395040, 0.5703125578963399445, 0.5729159820545779436, 0.5755208161855079885, 0.5781243415673570363, 0.5807289562083304268, 0.5833330067370782190, 0.5859370643821081304, 0.5885416720542003821, 0.5911452006262593040, 0.5937500332605881725, 0.5963534566387238556, 0.5989582195363342132, 0.6015619528528246551, 0.6041663359711972880, 0.6067707112921981727, 0.6093744496732020899, 0.6119792080484952601, 0.6145826326317597177, 0.6171874671691013337, 0.6197909930714722293, 0.6223956080197403651, 0.6249996591607356322, 0.6276037171273963766, 0.6302083254180952387, 0.6328118544107458332, 0.6354166875610788301, 0.6380201114567515264, 0.6406248747475506988, 0.6432286086754787080, 0.6458329921335752566, 0.6484373681338796436, 0.6510411069306952792, 0.6536458659264798854, 0.6562492910234830612, 0.6588541260574176661, 0.6614576525691320263, 0.6640622679146246377, 0.6666663197572214594, 0.6692703781348633418, 0.6718749871341050950, 0.6744785166361690898, 0.6770833503926931840, 0.6796867748946214816, 0.6822915386687108397, 0.6848952732971168578, 0.6874996571846213600, 0.6901040339539210589, 0.6927077732555863010, 0.6953125329619718187, 0.6979159586614360755, 0.7005207942821553013, 0.7031243214920454010, 0.7057289373247008779, 0.7083329899582661016, 0.7109370488362486418, 0.7135416586339821121, 0.7161451887342924483, 0.7187500231872065992, 0.7213534483841206324, 0.7239582127316128712, 0.7265619481495508847, 0.7291663325561579256, 0.7317707101841592898, 0.7343744500797240171, 0.7369792105868335774, 0.7395826369774940456, 0.7421874732752028470, 0.7447910012721150608, 0.7473956176818850050, 0.7499996711958007989, 0.7526037306634962842, 0.7552083413496862851, 0.7578118721370898925, 0.7604167073766084917, 0.7630201333572542710, 0.7656248983682768516, 0.7682286346648167230, 0.7708330196802359868, 0.7734373982566630223, 0.7760411388351919904, 0.7786459002331664880, 0.7812493274037752844, 0.7838541644686951582, 0.7864576933414935134, 0.7890623104183455139, 0.7916663649020125870, 0.7942704250488100692, 0.7968750367134410650, 0.7994785682768023038, 0.8020834043931583945, 0.8046868312463003603, 0.8072915970109983963, 0.8098953342752303053, 0.8124997199891885735, 0.8151040996037859365, 0.8177078409543626636, 0.8203126033333638656, 0.8229160313726919806, 0.8255208692950642968, 0.8281243991326340259, 0.8307290169665545454, 0.8333330725093962554, 0.8359371334247044372, 0.8385417461577832077, 0.8411452785859873105, 0.8437501156694361404, 0.8463535434838604932, 0.8489583100924004144, 0.8515620484134380774, 0.8541664349156833369, 0.8567708156582201084, 0.8593745578699503174, 0.8619793213201638604, 0.8645827503170061545, 0.8671875891870957087, 0.8697911200783463581, 0.8723957387593448409, 0.8749997954508100806, 0.8776038572240605351, 0.8802084711156200614, 0.8828120044975765746, 0.8854168426383988155, 0.8880202715029178462, 0.8906250390454908406, 0.8932287785124739532, 0.8958331658927787267, 0.8984375478530519654, 0.9010412910150662480, 0.9036460556267057465, 0.9062494856698833923, 0.9088543255779816255, 0.9114578576118502751, 0.9140624772299625889, 0.9166665351595286726, 0.9192705978801787303, 0.9218752130202838568, 0.9244787474449313036, 0.9270835867334279445, 0.9296870167368762594, 0.9322917853037333558, 0.9348955260058576799, 0.9374999143539141100, 0.9401042976215825409, 0.9427080418234272674, 0.9453128076877782560, 0.9479162388645026027, 0.9505210798953250828, 0.9531246131693177359, 0.9557292338404025367, 0.9583332930514818493, 0.9609373567081632705, 0.9635419734050364449, 0.9661455093234165847, 0.9687503490003109841, 0.9713537788664922124, 0.9739585512809396661, 0.9765622998769101226, 0.9791666815729623830, 0.9817710277688282972, 0.9843747994658795797, 0.9869797739623470401, 0.9895830763955310028, 0.9921869177308453303, 0.9947912343601759133, 0.9974001139318913189, 1.000000000000000000 ),
 .UNSPECIFIED. ) 
 GEOMETRIC_REPRESENTATION_ITEM ( )  RATIONAL_B_SPLINE_SURFACE ( (
 ( 1.000000000000000222, 1.000000000000000222, 1.000000000000000222, 1.000000000000000000, 1.000000000000000000, 1.000000000000000444, 1.000000000000000000, 0.9999999999999997780, 1.000000000000000444, 0.9999999999999997780, 0.9999999999999997780, 1.000000000000000222, 0.9999999999999997780, 0.9999999999999997780, 1.000000000000000444, 0.9999999999999997780, 1.000000000000000222, 1.000000000000000222, 0.9999999999999996669, 1.000000000000000222, 0.9999999999999996669, 1.000000000000000444, 0.9999999999999994449, 1.000000000000000444, 0.9999999999999996669, 1.000000000000000222, 1.000000000000000000, 0.9999999999999997780, 1.000000000000000222, 0.9999999999999997780, 1.000000000000000000, 0.9999999999999997780, 1.000000000000000000, 1.000000000000000222, 0.9999999999999996669, 1.000000000000000000, 0.9999999999999997780, 1.000000000000000000, 1.000000000000000444, 0.9999999999999996669, 1.000000000000000222, 1.000000000000000000, 1.000000000000000222, 1.000000000000000222, 0.9999999999999997780, 0.9999999999999997780, 1.000000000000000222, 0.9999999999999997780, 1.000000000000000222, 0.9999999999999997780, 0.9999999999999997780, 0.9999999999999997780, 1.000000000000000444, 1.000000000000000000, 0.9999999999999997780, 1.000000000000000222, 1.000000000000000000, 1.000000000000000000, 0.9999999999999997780, 1.000000000000000222, 1.000000000000000000, 1.000000000000000000, 1.000000000000000222, 1.000000000000000000, 1.000000000000000000, 1.000000000000000000, 1.000000000000000222, 1.000000000000000000, 0.9999999999999997780, 1.000000000000000444, 1.000000000000000000, 0.9999999999999997780, 1.000000000000000000, 1.000000000000000222, 0.9999999999999997780, 1.000000000000000222, 0.9999999999999996669, 1.000000000000000222, 1.000000000000000000, 1.000000000000000000, 1.000000000000000000, 1.000000000000000222, 0.9999999999999997780, 1.000000000000000000, 1.000000000000000222, 0.9999999999999997780, 1.000000000000000000, 1.000000000000000000, 0.9999999999999996669, 1.000000000000000000, 1.000000000000000000, 1.000000000000000222, 1.000000000000000000, 0.9999999999999997780, 1.000000000000000222, 0.9999999999999996669, 1.000000000000000222, 0.9999999999999997780, 1.000000000000000000, 1.000000000000000000, 1.000000000000000222, 0.9999999999999996669, 1.000000000000000444, 1.000000000000000000, 0.9999999999999997780, 1.000000000000000000, 1.000000000000000000, 1.000000000000000222, 0.9999999999999997780, 1.000000000000000000, 1.000000000000000222, 1.000000000000000444, 1.000000000000000000, 1.000000000000000000, 1.000000000000000444, 1.000000000000000000, 0.9999999999999997780, 1.000000000000000222, 1.000000000000000000, 1.000000000000000000, 1.000000000000000000, 1.000000000000000000, 1.000000000000000000, 1.000000000000000000, 0.9999999999999996669, 1.000000000000000222, 0.9999999999999997780, 1.000000000000000222, 1.000000000000000000, 0.9999999999999997780, 1.000000000000000222, 0.9999999999999997780, 0.9999999999999997780, 0.9999999999999997780, 1.000000000000000000, 1.000000000000000000, 0.9999999999999996669, 1.000000000000000444, 1.000000000000000222, 1.000000000000000000, 1.000000000000000000, 1.000000000000000222, 1.000000000000000222, 1.000000000000000000, 1.000000000000000222, 0.9999999999999996669, 1.000000000000000444, 0.9999999999999997780, 0.9999999999999997780, 1.000000000000000444, 1.000000000000000000, 1.000000000000000222, 0.9999999999999997780, 1.000000000000000222, 1.000000000000000000, 1.000000000000000222, 1.000000000000000000, 1.000000000000000000, 0.9999999999999996669, 1.000000000000000444, 1.000000000000000000, 1.000000000000000222, 0.9999999999999997780, 1.000000000000000000, 1.000000000000000000, 1.000000000000000000, 1.000000000000000000, 0.9999999999999997780, 1.000000000000000000, 1.000000000000000000, 1.000000000000000000, 1.000000000000000222, 1.000000000000000222, 0.9999999999999997780, 1.000000000000000000, 1.000000000000000000, 0.9999999999999997780, 1.000000000000000000, 1.000000000000000000, 1.000000000000000000, 1.000000000000000000, 1.000000000000000444, 0.9999999999999997780, 1.000000000000000222, 0.9999999999999997780, 1.000000000000000000, 1.000000000000000222, 0.9999999999999997780, 1.000000000000000222, 1.000000000000000000, 1.000000000000000000, 1.000000000000000000, 1.000000000000000000, 0.9999999999999997780, 1.000000000000000000, 1.000000000000000000, 1.000000000000000000, 1.000000000000000000, 1.000000000000000000, 1.000000000000000222, 1.000000000000000000, 1.000000000000000222, 0.9999999999999997780, 1.000000000000000222, 0.9999999999999997780, 1.000000000000000222, 1.000000000000000000, 0.9999999999999997780, 1.000000000000000222, 0.9999999999999996669, 1.000000000000000444, 1.000000000000000000, 0.9999999999999996669, 1.000000000000000222, 1.000000000000000000, 1.000000000000000222, 0.9999999999999997780, 1.000000000000000444, 1.000000000000000000, 1.000000000000000000, 0.9999999999999997780, 1.000000000000000222, 1.000000000000000000, 1.000000000000000000, 1.000000000000000000, 1.000000000000000222, 0.9999999999999997780, 1.000000000000000222, 1.000000000000000000, 0.9999999999999997780, 1.000000000000000000, 0.9999999999999997780, 1.000000000000000222, 0.9999999999999996669, 1.000000000000000000, 1.000000000000000000, 1.000000000000000000, 1.000000000000000444, 1.000000000000000222, 1.000000000000000000, 1.000000000000000000, 0.9999999999999997780, 0.9999999999999997780, 1.000000000000000444, 0.9999999999999996669, 1.000000000000000444, 0.9999999999999997780, 0.9999999999999997780, 1.000000000000000222, 0.9999999999999997780, 0.9999999999999996669, 1.000000000000000444, 0.9999999999999997780, 1.000000000000000222, 1.000000000000000222, 1.000000000000000000, 0.9999999999999997780, 1.000000000000000222, 1.000000000000000000, 1.000000000000000222, 1.000000000000000000, 1.000000000000000000, 0.9999999999999997780, 0.9999999999999997780, 1.000000000000000444, 0.9999999999999997780, 0.9999999999999997780, 1.000000000000000222, 0.9999999999999994449, 1.000000000000000222, 0.9999999999999997780, 1.000000000000000000, 0.9999999999999997780, 1.000000000000000000, 1.000000000000000000, 1.000000000000000000, 1.000000000000000000, 1.000000000000000000, 1.000000000000000000, 1.000000000000000000, 1.000000000000000222, 1.000000000000000000, 1.000000000000000000, 1.000000000000000000, 1.000000000000000000, 1.000000000000000000, 1.000000000000000000, 1.000000000000000000, 1.000000000000000222, 1.000000000000000000, 1.000000000000000222, 0.9999999999999997780, 1.000000000000000000, 1.000000000000000444, 1.000000000000000000, 1.000000000000000000, 1.000000000000000000, 1.000000000000000222, 0.9999999999999997780, 1.000000000000000444, 0.9999999999999997780, 1.000000000000000222, 1.000000000000000000, 1.000000000000000000, 1.000000000000000000, 1.000000000000000222, 0.9999999999999994449, 1.000000000000000222, 1.000000000000000000, 1.000000000000000000, 1.000000000000000000, 0.9999999999999997780, 0.9999999999999997780, 1.000000000000000444, 0.9999999999999996669, 1.000000000000000222, 0.9999999999999997780, 1.000000000000000444, 0.9999999999999997780, 1.000000000000000222, 1.000000000000000222, 0.9999999999999996669, 1.000000000000000222, 1.000000000000000000, 1.000000000000000444, 1.000000000000000000, 1.000000000000000000, 1.000000000000000222, 1.000000000000000000, 1.000000000000000000, 0.9999999999999997780, 0.9999999999999997780, 1.000000000000000000, 0.9999999999999997780, 1.000000000000000222, 1.000000000000000222, 1.000000000000000000, 1.000000000000000222, 1.000000000000000222, 1.000000000000000000, 0.9999999999999997780, 0.9999999999999997780, 1.000000000000000222, 0.9999999999999997780, 1.000000000000000222, 1.000000000000000000, 1.000000000000000000, 1.000000000000000000, 0.9999999999999996669, 1.000000000000000222, 0.9999999999999997780, 1.000000000000000000, 0.9999999999999997780, 1.000000000000000222, 0.9999999999999997780, 1.000000000000000444, 0.9999999999999996669, 1.000000000000000222, 1.000000000000000222, 1.000000000000000000, 1.000000000000000000, 0.9999999999999997780, 1.000000000000000222, 0.9999999999999997780, 1.000000000000000222, 0.9999999999999997780, 0.9999999999999997780, 1.000000000000000000, 1.000000000000000000, 1.000000000000000222, 1.000000000000000000, 1.000000000000000444, 0.9999999999999997780, 1.000000000000000222, 0.9999999999999997780, 0.9999999999999997780, 1.000000000000000222, 1.000000000000000000, 0.9999999999999997780, 1.000000000000000000, 1.000000000000000000, 1.000000000000000000, 0.9999999999999997780, 1.000000000000000444, 0.9999999999999997780, 1.000000000000000000, 1.000000000000000000),
 ( 0.3333333333333334259, 0.3333333333333334259, 0.3333333333333333703, 0.3333333333333334259, 0.3333333333333334259, 0.3333333333333334259, 0.3333333333333334259, 0.3333333333333332593, 0.3333333333333335369, 0.3333333333333332593, 0.3333333333333333703, 0.3333333333333334259, 0.3333333333333333703, 0.3333333333333332593, 0.3333333333333334814, 0.3333333333333332593, 0.3333333333333334259, 0.3333333333333334259, 0.3333333333333332593, 0.3333333333333335369, 0.3333333333333332038, 0.3333333333333335369, 0.3333333333333331483, 0.3333333333333334814, 0.3333333333333333148, 0.3333333333333333703, 0.3333333333333333703, 0.3333333333333333148, 0.3333333333333333703, 0.3333333333333333148, 0.3333333333333333703, 0.3333333333333333703, 0.3333333333333333703, 0.3333333333333333703, 0.3333333333333333703, 0.3333333333333333703, 0.3333333333333333148, 0.3333333333333333148, 0.3333333333333334259, 0.3333333333333332593, 0.3333333333333334259, 0.3333333333333333148, 0.3333333333333334259, 0.3333333333333333703, 0.3333333333333333148, 0.3333333333333334259, 0.3333333333333333703, 0.3333333333333333703, 0.3333333333333334259, 0.3333333333333333148, 0.3333333333333333703, 0.3333333333333332593, 0.3333333333333335369, 0.3333333333333333703, 0.3333333333333333148, 0.3333333333333334259, 0.3333333333333333703, 0.3333333333333333703, 0.3333333333333333148, 0.3333333333333333703, 0.3333333333333333703, 0.3333333333333334259, 0.3333333333333334259, 0.3333333333333334259, 0.3333333333333333703, 0.3333333333333333703, 0.3333333333333334259, 0.3333333333333333148, 0.3333333333333333703, 0.3333333333333334259, 0.3333333333333334259, 0.3333333333333332593, 0.3333333333333333703, 0.3333333333333334259, 0.3333333333333333703, 0.3333333333333334259, 0.3333333333333333148, 0.3333333333333334814, 0.3333333333333333148, 0.3333333333333332593, 0.3333333333333334259, 0.3333333333333333703, 0.3333333333333333148, 0.3333333333333333703, 0.3333333333333334259, 0.3333333333333334259, 0.3333333333333333148, 0.3333333333333333703, 0.3333333333333332593, 0.3333333333333333703, 0.3333333333333333703, 0.3333333333333333703, 0.3333333333333333703, 0.3333333333333333148, 0.3333333333333333703, 0.3333333333333333148, 0.3333333333333334259, 0.3333333333333333703, 0.3333333333333334259, 0.3333333333333333148, 0.3333333333333333703, 0.3333333333333333148, 0.3333333333333334259, 0.3333333333333333703, 0.3333333333333333703, 0.3333333333333333703, 0.3333333333333333703, 0.3333333333333333703, 0.3333333333333332593, 0.3333333333333333703, 0.3333333333333333703, 0.3333333333333335369, 0.3333333333333334259, 0.3333333333333333148, 0.3333333333333335369, 0.3333333333333333148, 0.3333333333333333703, 0.3333333333333333703, 0.3333333333333334259, 0.3333333333333333148, 0.3333333333333333703, 0.3333333333333334259, 0.3333333333333334259, 0.3333333333333333703, 0.3333333333333332593, 0.3333333333333334259, 0.3333333333333333703, 0.3333333333333334814, 0.3333333333333333148, 0.3333333333333333703, 0.3333333333333334259, 0.3333333333333333703, 0.3333333333333333148, 0.3333333333333333703, 0.3333333333333333148, 0.3333333333333334259, 0.3333333333333332593, 0.3333333333333334814, 0.3333333333333333703, 0.3333333333333334259, 0.3333333333333333703, 0.3333333333333333703, 0.3333333333333334259, 0.3333333333333333703, 0.3333333333333333703, 0.3333333333333333148, 0.3333333333333335924, 0.3333333333333333148, 0.3333333333333333703, 0.3333333333333334259, 0.3333333333333333148, 0.3333333333333334259, 0.3333333333333333148, 0.3333333333333334259, 0.3333333333333333703, 0.3333333333333334259, 0.3333333333333333703, 0.3333333333333333703, 0.3333333333333333703, 0.3333333333333334259, 0.3333333333333333703, 0.3333333333333334814, 0.3333333333333333148, 0.3333333333333334814, 0.3333333333333333148, 0.3333333333333333703, 0.3333333333333333148, 0.3333333333333333703, 0.3333333333333333703, 0.3333333333333333703, 0.3333333333333333703, 0.3333333333333333703, 0.3333333333333334259, 0.3333333333333333148, 0.3333333333333334259, 0.3333333333333333703, 0.3333333333333333703, 0.3333333333333333703, 0.3333333333333333703, 0.3333333333333333148, 0.3333333333333333703, 0.3333333333333334259, 0.3333333333333333148, 0.3333333333333334259, 0.3333333333333333148, 0.3333333333333333703, 0.3333333333333333703, 0.3333333333333333148, 0.3333333333333333703, 0.3333333333333334259, 0.3333333333333333148, 0.3333333333333334259, 0.3333333333333333703, 0.3333333333333332593, 0.3333333333333334814, 0.3333333333333332593, 0.3333333333333334259, 0.3333333333333333148, 0.3333333333333333703, 0.3333333333333334814, 0.3333333333333333703, 0.3333333333333333703, 0.3333333333333332593, 0.3333333333333334814, 0.3333333333333333148, 0.3333333333333333703, 0.3333333333333334259, 0.3333333333333333148, 0.3333333333333334259, 0.3333333333333333148, 0.3333333333333333703, 0.3333333333333333703, 0.3333333333333332593, 0.3333333333333333703, 0.3333333333333333703, 0.3333333333333334259, 0.3333333333333333148, 0.3333333333333334814, 0.3333333333333333703, 0.3333333333333334259, 0.3333333333333333148, 0.3333333333333334259, 0.3333333333333333703, 0.3333333333333333703, 0.3333333333333333703, 0.3333333333333333703, 0.3333333333333333148, 0.3333333333333334814, 0.3333333333333333703, 0.3333333333333333703, 0.3333333333333333148, 0.3333333333333334259, 0.3333333333333333703, 0.3333333333333332593, 0.3333333333333333703, 0.3333333333333333703, 0.3333333333333333703, 0.3333333333333334259, 0.3333333333333334259, 0.3333333333333333703, 0.3333333333333333703, 0.3333333333333333703, 0.3333333333333333703, 0.3333333333333334259, 0.3333333333333332593, 0.3333333333333335369, 0.3333333333333332038, 0.3333333333333333148, 0.3333333333333333703, 0.3333333333333333148, 0.3333333333333333148, 0.3333333333333334259, 0.3333333333333333703, 0.3333333333333333703, 0.3333333333333333703, 0.3333333333333334259, 0.3333333333333333148, 0.3333333333333334814, 0.3333333333333333703, 0.3333333333333334259, 0.3333333333333333703, 0.3333333333333333703, 0.3333333333333332593, 0.3333333333333333148, 0.3333333333333334814, 0.3333333333333333148, 0.3333333333333332593, 0.3333333333333334259, 0.3333333333333332038, 0.3333333333333334259, 0.3333333333333333148, 0.3333333333333333148, 0.3333333333333334259, 0.3333333333333333703, 0.3333333333333333703, 0.3333333333333333703, 0.3333333333333333703, 0.3333333333333334259, 0.3333333333333333148, 0.3333333333333333148, 0.3333333333333334259, 0.3333333333333333148, 0.3333333333333334259, 0.3333333333333333148, 0.3333333333333333703, 0.3333333333333334259, 0.3333333333333333148, 0.3333333333333334814, 0.3333333333333333148, 0.3333333333333334259, 0.3333333333333334259, 0.3333333333333333148, 0.3333333333333333148, 0.3333333333333335369, 0.3333333333333333148, 0.3333333333333333148, 0.3333333333333333703, 0.3333333333333335369, 0.3333333333333332593, 0.3333333333333335369, 0.3333333333333333148, 0.3333333333333333148, 0.3333333333333334259, 0.3333333333333333148, 0.3333333333333334259, 0.3333333333333333703, 0.3333333333333332593, 0.3333333333333333703, 0.3333333333333333148, 0.3333333333333334259, 0.3333333333333333148, 0.3333333333333334259, 0.3333333333333332593, 0.3333333333333335369, 0.3333333333333332038, 0.3333333333333334259, 0.3333333333333332593, 0.3333333333333335369, 0.3333333333333333148, 0.3333333333333334259, 0.3333333333333334259, 0.3333333333333333148, 0.3333333333333333148, 0.3333333333333334259, 0.3333333333333334814, 0.3333333333333333148, 0.3333333333333333148, 0.3333333333333334259, 0.3333333333333333703, 0.3333333333333334259, 0.3333333333333333148, 0.3333333333333333148, 0.3333333333333333703, 0.3333333333333333703, 0.3333333333333334814, 0.3333333333333333148, 0.3333333333333334259, 0.3333333333333333703, 0.3333333333333334259, 0.3333333333333334259, 0.3333333333333333148, 0.3333333333333333703, 0.3333333333333334259, 0.3333333333333333148, 0.3333333333333334814, 0.3333333333333333703, 0.3333333333333333148, 0.3333333333333333703, 0.3333333333333333148, 0.3333333333333334259, 0.3333333333333333148, 0.3333333333333333703, 0.3333333333333332593, 0.3333333333333334814, 0.3333333333333333703, 0.3333333333333334814, 0.3333333333333333148, 0.3333333333333334259, 0.3333333333333334814, 0.3333333333333333148, 0.3333333333333334259, 0.3333333333333332593, 0.3333333333333334259, 0.3333333333333333703, 0.3333333333333333703, 0.3333333333333333148, 0.3333333333333333148, 0.3333333333333334259, 0.3333333333333333148, 0.3333333333333334814, 0.3333333333333333148, 0.3333333333333335924, 0.3333333333333333148, 0.3333333333333334259, 0.3333333333333333148, 0.3333333333333333703, 0.3333333333333333703, 0.3333333333333334814, 0.3333333333333332593, 0.3333333333333333703, 0.3333333333333333703, 0.3333333333333334259, 0.3333333333333333148, 0.3333333333333334259, 0.3333333333333333703, 0.3333333333333333703, 0.3333333333333333703),
 ( 0.3333333333333334259, 0.3333333333333334259, 0.3333333333333333703, 0.3333333333333334259, 0.3333333333333334259, 0.3333333333333334259, 0.3333333333333334259, 0.3333333333333332593, 0.3333333333333335369, 0.3333333333333332593, 0.3333333333333333703, 0.3333333333333334259, 0.3333333333333333703, 0.3333333333333332593, 0.3333333333333334814, 0.3333333333333332593, 0.3333333333333334259, 0.3333333333333334259, 0.3333333333333332593, 0.3333333333333335369, 0.3333333333333332038, 0.3333333333333335369, 0.3333333333333331483, 0.3333333333333334814, 0.3333333333333333148, 0.3333333333333333703, 0.3333333333333333703, 0.3333333333333333148, 0.3333333333333333703, 0.3333333333333333148, 0.3333333333333333703, 0.3333333333333333703, 0.3333333333333333703, 0.3333333333333333703, 0.3333333333333333703, 0.3333333333333333703, 0.3333333333333333148, 0.3333333333333333148, 0.3333333333333334259, 0.3333333333333332593, 0.3333333333333334259, 0.3333333333333333148, 0.3333333333333334259, 0.3333333333333333703, 0.3333333333333333148, 0.3333333333333334259, 0.3333333333333333703, 0.3333333333333333703, 0.3333333333333334259, 0.3333333333333333148, 0.3333333333333333703, 0.3333333333333332593, 0.3333333333333335369, 0.3333333333333333703, 0.3333333333333333148, 0.3333333333333334259, 0.3333333333333333703, 0.3333333333333333703, 0.3333333333333333148, 0.3333333333333333703, 0.3333333333333333703, 0.3333333333333334259, 0.3333333333333334259, 0.3333333333333334259, 0.3333333333333333703, 0.3333333333333333703, 0.3333333333333334259, 0.3333333333333333148, 0.3333333333333333703, 0.3333333333333334259, 0.3333333333333334259, 0.3333333333333332593, 0.3333333333333333703, 0.3333333333333334259, 0.3333333333333333703, 0.3333333333333334259, 0.3333333333333333148, 0.3333333333333334814, 0.3333333333333333148, 0.3333333333333332593, 0.3333333333333334259, 0.3333333333333333703, 0.3333333333333333148, 0.3333333333333333703, 0.3333333333333334259, 0.3333333333333334259, 0.3333333333333333148, 0.3333333333333333703, 0.3333333333333332593, 0.3333333333333333703, 0.3333333333333333703, 0.3333333333333333703, 0.3333333333333333703, 0.3333333333333333148, 0.3333333333333333703, 0.3333333333333333148, 0.3333333333333334259, 0.3333333333333333703, 0.3333333333333334259, 0.3333333333333333148, 0.3333333333333333703, 0.3333333333333333148, 0.3333333333333334259, 0.3333333333333333703, 0.3333333333333333703, 0.3333333333333333703, 0.3333333333333333703, 0.3333333333333333703, 0.3333333333333332593, 0.3333333333333333703, 0.3333333333333333703, 0.3333333333333335369, 0.3333333333333334259, 0.3333333333333333148, 0.3333333333333335369, 0.3333333333333333148, 0.3333333333333333703, 0.3333333333333333703, 0.3333333333333334259, 0.3333333333333333148, 0.3333333333333333703, 0.3333333333333334259, 0.3333333333333334259, 0.3333333333333333703, 0.3333333333333332593, 0.3333333333333334259, 0.3333333333333333703, 0.3333333333333334814, 0.3333333333333333148, 0.3333333333333333703, 0.3333333333333334259, 0.3333333333333333703, 0.3333333333333333148, 0.3333333333333333703, 0.3333333333333333148, 0.3333333333333334259, 0.3333333333333332593, 0.3333333333333334814, 0.3333333333333333703, 0.3333333333333334259, 0.3333333333333333703, 0.3333333333333333703, 0.3333333333333334259, 0.3333333333333333703, 0.3333333333333333703, 0.3333333333333333148, 0.3333333333333335924, 0.3333333333333333148, 0.3333333333333333703, 0.3333333333333334259, 0.3333333333333333148, 0.3333333333333334259, 0.3333333333333333148, 0.3333333333333334259, 0.3333333333333333703, 0.3333333333333334259, 0.3333333333333333703, 0.3333333333333333703, 0.3333333333333333703, 0.3333333333333334259, 0.3333333333333333703, 0.3333333333333334814, 0.3333333333333333148, 0.3333333333333334814, 0.3333333333333333148, 0.3333333333333333703, 0.3333333333333333148, 0.3333333333333333703, 0.3333333333333333703, 0.3333333333333333703, 0.3333333333333333703, 0.3333333333333333703, 0.3333333333333334259, 0.3333333333333333148, 0.3333333333333334259, 0.3333333333333333703, 0.3333333333333333703, 0.3333333333333333703, 0.3333333333333333703, 0.3333333333333333148, 0.3333333333333333703, 0.3333333333333334259, 0.3333333333333333148, 0.3333333333333334259, 0.3333333333333333148, 0.3333333333333333703, 0.3333333333333333703, 0.3333333333333333148, 0.3333333333333333703, 0.3333333333333334259, 0.3333333333333333148, 0.3333333333333334259, 0.3333333333333333703, 0.3333333333333332593, 0.3333333333333334814, 0.3333333333333332593, 0.3333333333333334259, 0.3333333333333333148, 0.3333333333333333703, 0.3333333333333334814, 0.3333333333333333703, 0.3333333333333333703, 0.3333333333333332593, 0.3333333333333334814, 0.3333333333333333148, 0.3333333333333333703, 0.3333333333333334259, 0.3333333333333333148, 0.3333333333333334259, 0.3333333333333333148, 0.3333333333333333703, 0.3333333333333333703, 0.3333333333333332593, 0.3333333333333333703, 0.3333333333333333703, 0.3333333333333334259, 0.3333333333333333148, 0.3333333333333334814, 0.3333333333333333703, 0.3333333333333334259, 0.3333333333333333148, 0.3333333333333334259, 0.3333333333333333703, 0.3333333333333333703, 0.3333333333333333703, 0.3333333333333333703, 0.3333333333333333148, 0.3333333333333334814, 0.3333333333333333703, 0.3333333333333333703, 0.3333333333333333148, 0.3333333333333334259, 0.3333333333333333703, 0.3333333333333332593, 0.3333333333333333703, 0.3333333333333333703, 0.3333333333333333703, 0.3333333333333334259, 0.3333333333333334259, 0.3333333333333333703, 0.3333333333333333703, 0.3333333333333333703, 0.3333333333333333703, 0.3333333333333334259, 0.3333333333333332593, 0.3333333333333335369, 0.3333333333333332038, 0.3333333333333333148, 0.3333333333333333703, 0.3333333333333333148, 0.3333333333333333148, 0.3333333333333334259, 0.3333333333333333703, 0.3333333333333333703, 0.3333333333333333703, 0.3333333333333334259, 0.3333333333333333148, 0.3333333333333334814, 0.3333333333333333703, 0.3333333333333334259, 0.3333333333333333703, 0.3333333333333333703, 0.3333333333333332593, 0.3333333333333333148, 0.3333333333333334814, 0.3333333333333333148, 0.3333333333333332593, 0.3333333333333334259, 0.3333333333333332038, 0.3333333333333334259, 0.3333333333333333148, 0.3333333333333333148, 0.3333333333333334259, 0.3333333333333333703, 0.3333333333333333703, 0.3333333333333333703, 0.3333333333333333703, 0.3333333333333334259, 0.3333333333333333148, 0.3333333333333333148, 0.3333333333333334259, 0.3333333333333333148, 0.3333333333333334259, 0.3333333333333333148, 0.3333333333333333703, 0.3333333333333334259, 0.3333333333333333148, 0.3333333333333334814, 0.3333333333333333148, 0.3333333333333334259, 0.3333333333333334259, 0.3333333333333333148, 0.3333333333333333148, 0.3333333333333335369, 0.3333333333333333148, 0.3333333333333333148, 0.3333333333333333703, 0.3333333333333335369, 0.3333333333333332593, 0.3333333333333335369, 0.3333333333333333148, 0.3333333333333333148, 0.3333333333333334259, 0.3333333333333333148, 0.3333333333333334259, 0.3333333333333333703, 0.3333333333333332593, 0.3333333333333333703, 0.3333333333333333148, 0.3333333333333334259, 0.3333333333333333148, 0.3333333333333334259, 0.3333333333333332593, 0.3333333333333335369, 0.3333333333333332038, 0.3333333333333334259, 0.3333333333333332593, 0.3333333333333335369, 0.3333333333333333148, 0.3333333333333334259, 0.3333333333333334259, 0.3333333333333333148, 0.3333333333333333148, 0.3333333333333334259, 0.3333333333333334814, 0.3333333333333333148, 0.3333333333333333148, 0.3333333333333334259, 0.3333333333333333703, 0.3333333333333334259, 0.3333333333333333148, 0.3333333333333333148, 0.3333333333333333703, 0.3333333333333333703, 0.3333333333333334814, 0.3333333333333333148, 0.3333333333333334259, 0.3333333333333333703, 0.3333333333333334259, 0.3333333333333334259, 0.3333333333333333148, 0.3333333333333333703, 0.3333333333333334259, 0.3333333333333333148, 0.3333333333333334814, 0.3333333333333333703, 0.3333333333333333148, 0.3333333333333333703, 0.3333333333333333148, 0.3333333333333334259, 0.3333333333333333148, 0.3333333333333333703, 0.3333333333333332593, 0.3333333333333334814, 0.3333333333333333703, 0.3333333333333334814, 0.3333333333333333148, 0.3333333333333334259, 0.3333333333333334814, 0.3333333333333333148, 0.3333333333333334259, 0.3333333333333332593, 0.3333333333333334259, 0.3333333333333333703, 0.3333333333333333703, 0.3333333333333333148, 0.3333333333333333148, 0.3333333333333334259, 0.3333333333333333148, 0.3333333333333334814, 0.3333333333333333148, 0.3333333333333335924, 0.3333333333333333148, 0.3333333333333334259, 0.3333333333333333148, 0.3333333333333333703, 0.3333333333333333703, 0.3333333333333334814, 0.3333333333333332593, 0.3333333333333333703, 0.3333333333333333703, 0.3333333333333334259, 0.3333333333333333148, 0.3333333333333334259, 0.3333333333333333703, 0.3333333333333333703, 0.3333333333333333703),
 ( 1.000000000000000222, 1.000000000000000222, 1.000000000000000222, 1.000000000000000000, 1.000000000000000000, 1.000000000000000444, 1.000000000000000000, 0.9999999999999997780, 1.000000000000000444, 0.9999999999999997780, 0.9999999999999997780, 1.000000000000000222, 0.9999999999999997780, 0.9999999999999997780, 1.000000000000000444, 0.9999999999999997780, 1.000000000000000222, 1.000000000000000222, 0.9999999999999996669, 1.000000000000000222, 0.9999999999999996669, 1.000000000000000444, 0.9999999999999994449, 1.000000000000000444, 0.9999999999999996669, 1.000000000000000222, 1.000000000000000000, 0.9999999999999997780, 1.000000000000000222, 0.9999999999999997780, 1.000000000000000000, 0.9999999999999997780, 1.000000000000000000, 1.000000000000000222, 0.9999999999999996669, 1.000000000000000000, 0.9999999999999997780, 1.000000000000000000, 1.000000000000000444, 0.9999999999999996669, 1.000000000000000222, 1.000000000000000000, 1.000000000000000222, 1.000000000000000222, 0.9999999999999997780, 0.9999999999999997780, 1.000000000000000222, 0.9999999999999997780, 1.000000000000000222, 0.9999999999999997780, 0.9999999999999997780, 0.9999999999999997780, 1.000000000000000444, 1.000000000000000000, 0.9999999999999997780, 1.000000000000000222, 1.000000000000000000, 1.000000000000000000, 0.9999999999999997780, 1.000000000000000222, 1.000000000000000000, 1.000000000000000000, 1.000000000000000222, 1.000000000000000000, 1.000000000000000000, 1.000000000000000000, 1.000000000000000222, 1.000000000000000000, 0.9999999999999997780, 1.000000000000000444, 1.000000000000000000, 0.9999999999999997780, 1.000000000000000000, 1.000000000000000222, 0.9999999999999997780, 1.000000000000000222, 0.9999999999999996669, 1.000000000000000222, 1.000000000000000000, 1.000000000000000000, 1.000000000000000000, 1.000000000000000222, 0.9999999999999997780, 1.000000000000000000, 1.000000000000000222, 0.9999999999999997780, 1.000000000000000000, 1.000000000000000000, 0.9999999999999996669, 1.000000000000000000, 1.000000000000000000, 1.000000000000000222, 1.000000000000000000, 0.9999999999999997780, 1.000000000000000222, 0.9999999999999996669, 1.000000000000000222, 0.9999999999999997780, 1.000000000000000000, 1.000000000000000000, 1.000000000000000222, 0.9999999999999996669, 1.000000000000000444, 1.000000000000000000, 0.9999999999999997780, 1.000000000000000000, 1.000000000000000000, 1.000000000000000222, 0.9999999999999997780, 1.000000000000000000, 1.000000000000000222, 1.000000000000000444, 1.000000000000000000, 1.000000000000000000, 1.000000000000000444, 1.000000000000000000, 0.9999999999999997780, 1.000000000000000222, 1.000000000000000000, 1.000000000000000000, 1.000000000000000000, 1.000000000000000000, 1.000000000000000000, 1.000000000000000000, 0.9999999999999996669, 1.000000000000000222, 0.9999999999999997780, 1.000000000000000222, 1.000000000000000000, 0.9999999999999997780, 1.000000000000000222, 0.9999999999999997780, 0.9999999999999997780, 0.9999999999999997780, 1.000000000000000000, 1.000000000000000000, 0.9999999999999996669, 1.000000000000000444, 1.000000000000000222, 1.000000000000000000, 1.000000000000000000, 1.000000000000000222, 1.000000000000000222, 1.000000000000000000, 1.000000000000000222, 0.9999999999999996669, 1.000000000000000444, 0.9999999999999997780, 0.9999999999999997780, 1.000000000000000444, 1.000000000000000000, 1.000000000000000222, 0.9999999999999997780, 1.000000000000000222, 1.000000000000000000, 1.000000000000000222, 1.000000000000000000, 1.000000000000000000, 0.9999999999999996669, 1.000000000000000444, 1.000000000000000000, 1.000000000000000222, 0.9999999999999997780, 1.000000000000000000, 1.000000000000000000, 1.000000000000000000, 1.000000000000000000, 0.9999999999999997780, 1.000000000000000000, 1.000000000000000000, 1.000000000000000000, 1.000000000000000222, 1.000000000000000222, 0.9999999999999997780, 1.000000000000000000, 1.000000000000000000, 0.9999999999999997780, 1.000000000000000000, 1.000000000000000000, 1.000000000000000000, 1.000000000000000000, 1.000000000000000444, 0.9999999999999997780, 1.000000000000000222, 0.9999999999999997780, 1.000000000000000000, 1.000000000000000222, 0.9999999999999997780, 1.000000000000000222, 1.000000000000000000, 1.000000000000000000, 1.000000000000000000, 1.000000000000000000, 0.9999999999999997780, 1.000000000000000000, 1.000000000000000000, 1.000000000000000000, 1.000000000000000000, 1.000000000000000000, 1.000000000000000222, 1.000000000000000000, 1.000000000000000222, 0.9999999999999997780, 1.000000000000000222, 0.9999999999999997780, 1.000000000000000222, 1.000000000000000000, 0.9999999999999997780, 1.000000000000000222, 0.9999999999999996669, 1.000000000000000444, 1.000000000000000000, 0.9999999999999996669, 1.000000000000000222, 1.000000000000000000, 1.000000000000000222, 0.9999999999999997780, 1.000000000000000444, 1.000000000000000000, 1.000000000000000000, 0.9999999999999997780, 1.000000000000000222, 1.000000000000000000, 1.000000000000000000, 1.000000000000000000, 1.000000000000000222, 0.9999999999999997780, 1.000000000000000222, 1.000000000000000000, 0.9999999999999997780, 1.000000000000000000, 0.9999999999999997780, 1.000000000000000222, 0.9999999999999996669, 1.000000000000000000, 1.000000000000000000, 1.000000000000000000, 1.000000000000000444, 1.000000000000000222, 1.000000000000000000, 1.000000000000000000, 0.9999999999999997780, 0.9999999999999997780, 1.000000000000000444, 0.9999999999999996669, 1.000000000000000444, 0.9999999999999997780, 0.9999999999999997780, 1.000000000000000222, 0.9999999999999997780, 0.9999999999999996669, 1.000000000000000444, 0.9999999999999997780, 1.000000000000000222, 1.000000000000000222, 1.000000000000000000, 0.9999999999999997780, 1.000000000000000222, 1.000000000000000000, 1.000000000000000222, 1.000000000000000000, 1.000000000000000000, 0.9999999999999997780, 0.9999999999999997780, 1.000000000000000444, 0.9999999999999997780, 0.9999999999999997780, 1.000000000000000222, 0.9999999999999994449, 1.000000000000000222, 0.9999999999999997780, 1.000000000000000000, 0.9999999999999997780, 1.000000000000000000, 1.000000000000000000, 1.000000000000000000, 1.000000000000000000, 1.000000000000000000, 1.000000000000000000, 1.000000000000000000, 1.000000000000000222, 1.000000000000000000, 1.000000000000000000, 1.000000000000000000, 1.000000000000000000, 1.000000000000000000, 1.000000000000000000, 1.000000000000000000, 1.000000000000000222, 1.000000000000000000, 1.000000000000000222, 0.9999999999999997780, 1.000000000000000000, 1.000000000000000444, 1.000000000000000000, 1.000000000000000000, 1.000000000000000000, 1.000000000000000222, 0.9999999999999997780, 1.000000000000000444, 0.9999999999999997780, 1.000000000000000222, 1.000000000000000000, 1.000000000000000000, 1.000000000000000000, 1.000000000000000222, 0.9999999999999994449, 1.000000000000000222, 1.000000000000000000, 1.000000000000000000, 1.000000000000000000, 0.9999999999999997780, 0.9999999999999997780, 1.000000000000000444, 0.9999999999999996669, 1.000000000000000222, 0.9999999999999997780, 1.000000000000000444, 0.9999999999999997780, 1.000000000000000222, 1.000000000000000222, 0.9999999999999996669, 1.000000000000000222, 1.000000000000000000, 1.000000000000000444, 1.000000000000000000, 1.000000000000000000, 1.000000000000000222, 1.000000000000000000, 1.000000000000000000, 0.9999999999999997780, 0.9999999999999997780, 1.000000000000000000, 0.9999999999999997780, 1.000000000000000222, 1.000000000000000222, 1.000000000000000000, 1.000000000000000222, 1.000000000000000222, 1.000000000000000000, 0.9999999999999997780, 0.9999999999999997780, 1.000000000000000222, 0.9999999999999997780, 1.000000000000000222, 1.000000000000000000, 1.000000000000000000, 1.000000000000000000, 0.9999999999999996669, 1.000000000000000222, 0.9999999999999997780, 1.000000000000000000, 0.9999999999999997780, 1.000000000000000222, 0.9999999999999997780, 1.000000000000000444, 0.9999999999999996669, 1.000000000000000222, 1.000000000000000222, 1.000000000000000000, 1.000000000000000000, 0.9999999999999997780, 1.000000000000000222, 0.9999999999999997780, 1.000000000000000222, 0.9999999999999997780, 0.9999999999999997780, 1.000000000000000000, 1.000000000000000000, 1.000000000000000222, 1.000000000000000000, 1.000000000000000444, 0.9999999999999997780, 1.000000000000000222, 0.9999999999999997780, 0.9999999999999997780, 1.000000000000000222, 1.000000000000000000, 0.9999999999999997780, 1.000000000000000000, 1.000000000000000000, 1.000000000000000000, 0.9999999999999997780, 1.000000000000000444, 0.9999999999999997780, 1.000000000000000000, 1.000000000000000000),
 ( 0.3333333333333334259, 0.3333333333333334259, 0.3333333333333333703, 0.3333333333333334259, 0.3333333333333334259, 0.3333333333333334259, 0.3333333333333334259, 0.3333333333333332593, 0.3333333333333335369, 0.3333333333333332593, 0.3333333333333333703, 0.3333333333333334259, 0.3333333333333333703, 0.3333333333333332593, 0.3333333333333334814, 0.3333333333333332593, 0.3333333333333334259, 0.3333333333333334259, 0.3333333333333332593, 0.3333333333333335369, 0.3333333333333332038, 0.3333333333333335369, 0.3333333333333331483, 0.3333333333333334814, 0.3333333333333333148, 0.3333333333333333703, 0.3333333333333333703, 0.3333333333333333148, 0.3333333333333333703, 0.3333333333333333148, 0.3333333333333333703, 0.3333333333333333703, 0.3333333333333333703, 0.3333333333333333703, 0.3333333333333333703, 0.3333333333333333703, 0.3333333333333333148, 0.3333333333333333148, 0.3333333333333334259, 0.3333333333333332593, 0.3333333333333334259, 0.3333333333333333148, 0.3333333333333334259, 0.3333333333333333703, 0.3333333333333333148, 0.3333333333333334259, 0.3333333333333333703, 0.3333333333333333703, 0.3333333333333334259, 0.3333333333333333148, 0.3333333333333333703, 0.3333333333333332593, 0.3333333333333335369, 0.3333333333333333703, 0.3333333333333333148, 0.3333333333333334259, 0.3333333333333333703, 0.3333333333333333703, 0.3333333333333333148, 0.3333333333333333703, 0.3333333333333333703, 0.3333333333333334259, 0.3333333333333334259, 0.3333333333333334259, 0.3333333333333333703, 0.3333333333333333703, 0.3333333333333334259, 0.3333333333333333148, 0.3333333333333333703, 0.3333333333333334259, 0.3333333333333334259, 0.3333333333333332593, 0.3333333333333333703, 0.3333333333333334259, 0.3333333333333333703, 0.3333333333333334259, 0.3333333333333333148, 0.3333333333333334814, 0.3333333333333333148, 0.3333333333333332593, 0.3333333333333334259, 0.3333333333333333703, 0.3333333333333333148, 0.3333333333333333703, 0.3333333333333334259, 0.3333333333333334259, 0.3333333333333333148, 0.3333333333333333703, 0.3333333333333332593, 0.3333333333333333703, 0.3333333333333333703, 0.3333333333333333703, 0.3333333333333333703, 0.3333333333333333148, 0.3333333333333333703, 0.3333333333333333148, 0.3333333333333334259, 0.3333333333333333703, 0.3333333333333334259, 0.3333333333333333148, 0.3333333333333333703, 0.3333333333333333148, 0.3333333333333334259, 0.3333333333333333703, 0.3333333333333333703, 0.3333333333333333703, 0.3333333333333333703, 0.3333333333333333703, 0.3333333333333332593, 0.3333333333333333703, 0.3333333333333333703, 0.3333333333333335369, 0.3333333333333334259, 0.3333333333333333148, 0.3333333333333335369, 0.3333333333333333148, 0.3333333333333333703, 0.3333333333333333703, 0.3333333333333334259, 0.3333333333333333148, 0.3333333333333333703, 0.3333333333333334259, 0.3333333333333334259, 0.3333333333333333703, 0.3333333333333332593, 0.3333333333333334259, 0.3333333333333333703, 0.3333333333333334814, 0.3333333333333333148, 0.3333333333333333703, 0.3333333333333334259, 0.3333333333333333703, 0.3333333333333333148, 0.3333333333333333703, 0.3333333333333333148, 0.3333333333333334259, 0.3333333333333332593, 0.3333333333333334814, 0.3333333333333333703, 0.3333333333333334259, 0.3333333333333333703, 0.3333333333333333703, 0.3333333333333334259, 0.3333333333333333703, 0.3333333333333333703, 0.3333333333333333148, 0.3333333333333335924, 0.3333333333333333148, 0.3333333333333333703, 0.3333333333333334259, 0.3333333333333333148, 0.3333333333333334259, 0.3333333333333333148, 0.3333333333333334259, 0.3333333333333333703, 0.3333333333333334259, 0.3333333333333333703, 0.3333333333333333703, 0.3333333333333333703, 0.3333333333333334259, 0.3333333333333333703, 0.3333333333333334814, 0.3333333333333333148, 0.3333333333333334814, 0.3333333333333333148, 0.3333333333333333703, 0.3333333333333333148, 0.3333333333333333703, 0.3333333333333333703, 0.3333333333333333703, 0.3333333333333333703, 0.3333333333333333703, 0.3333333333333334259, 0.3333333333333333148, 0.3333333333333334259, 0.3333333333333333703, 0.3333333333333333703, 0.3333333333333333703, 0.3333333333333333703, 0.3333333333333333148, 0.3333333333333333703, 0.3333333333333334259, 0.3333333333333333148, 0.3333333333333334259, 0.3333333333333333148, 0.3333333333333333703, 0.3333333333333333703, 0.3333333333333333148, 0.3333333333333333703, 0.3333333333333334259, 0.3333333333333333148, 0.3333333333333334259, 0.3333333333333333703, 0.3333333333333332593, 0.3333333333333334814, 0.3333333333333332593, 0.3333333333333334259, 0.3333333333333333148, 0.3333333333333333703, 0.3333333333333334814, 0.3333333333333333703, 0.3333333333333333703, 0.3333333333333332593, 0.3333333333333334814, 0.3333333333333333148, 0.3333333333333333703, 0.3333333333333334259, 0.3333333333333333148, 0.3333333333333334259, 0.3333333333333333148, 0.3333333333333333703, 0.3333333333333333703, 0.3333333333333332593, 0.3333333333333333703, 0.3333333333333333703, 0.3333333333333334259, 0.3333333333333333148, 0.3333333333333334814, 0.3333333333333333703, 0.3333333333333334259, 0.3333333333333333148, 0.3333333333333334259, 0.3333333333333333703, 0.3333333333333333703, 0.3333333333333333703, 0.3333333333333333703, 0.3333333333333333148, 0.3333333333333334814, 0.3333333333333333703, 0.3333333333333333703, 0.3333333333333333148, 0.3333333333333334259, 0.3333333333333333703, 0.3333333333333332593, 0.3333333333333333703, 0.3333333333333333703, 0.3333333333333333703, 0.3333333333333334259, 0.3333333333333334259, 0.3333333333333333703, 0.3333333333333333703, 0.3333333333333333703, 0.3333333333333333703, 0.3333333333333334259, 0.3333333333333332593, 0.3333333333333335369, 0.3333333333333332038, 0.3333333333333333148, 0.3333333333333333703, 0.3333333333333333148, 0.3333333333333333148, 0.3333333333333334259, 0.3333333333333333703, 0.3333333333333333703, 0.3333333333333333703, 0.3333333333333334259, 0.3333333333333333148, 0.3333333333333334814, 0.3333333333333333703, 0.3333333333333334259, 0.3333333333333333703, 0.3333333333333333703, 0.3333333333333332593, 0.3333333333333333148, 0.3333333333333334814, 0.3333333333333333148, 0.3333333333333332593, 0.3333333333333334259, 0.3333333333333332038, 0.3333333333333334259, 0.3333333333333333148, 0.3333333333333333148, 0.3333333333333334259, 0.3333333333333333703, 0.3333333333333333703, 0.3333333333333333703, 0.3333333333333333703, 0.3333333333333334259, 0.3333333333333333148, 0.3333333333333333148, 0.3333333333333334259, 0.3333333333333333148, 0.3333333333333334259, 0.3333333333333333148, 0.3333333333333333703, 0.3333333333333334259, 0.3333333333333333148, 0.3333333333333334814, 0.3333333333333333148, 0.3333333333333334259, 0.3333333333333334259, 0.3333333333333333148, 0.3333333333333333148, 0.3333333333333335369, 0.3333333333333333148, 0.3333333333333333148, 0.3333333333333333703, 0.3333333333333335369, 0.3333333333333332593, 0.3333333333333335369, 0.3333333333333333148, 0.3333333333333333148, 0.3333333333333334259, 0.3333333333333333148, 0.3333333333333334259, 0.3333333333333333703, 0.3333333333333332593, 0.3333333333333333703, 0.3333333333333333148, 0.3333333333333334259, 0.3333333333333333148, 0.3333333333333334259, 0.3333333333333332593, 0.3333333333333335369, 0.3333333333333332038, 0.3333333333333334259, 0.3333333333333332593, 0.3333333333333335369, 0.3333333333333333148, 0.3333333333333334259, 0.3333333333333334259, 0.3333333333333333148, 0.3333333333333333148, 0.3333333333333334259, 0.3333333333333334814, 0.3333333333333333148, 0.3333333333333333148, 0.3333333333333334259, 0.3333333333333333703, 0.3333333333333334259, 0.3333333333333333148, 0.3333333333333333148, 0.3333333333333333703, 0.3333333333333333703, 0.3333333333333334814, 0.3333333333333333148, 0.3333333333333334259, 0.3333333333333333703, 0.3333333333333334259, 0.3333333333333334259, 0.3333333333333333148, 0.3333333333333333703, 0.3333333333333334259, 0.3333333333333333148, 0.3333333333333334814, 0.3333333333333333703, 0.3333333333333333148, 0.3333333333333333703, 0.3333333333333333148, 0.3333333333333334259, 0.3333333333333333148, 0.3333333333333333703, 0.3333333333333332593, 0.3333333333333334814, 0.3333333333333333703, 0.3333333333333334814, 0.3333333333333333148, 0.3333333333333334259, 0.3333333333333334814, 0.3333333333333333148, 0.3333333333333334259, 0.3333333333333332593, 0.3333333333333334259, 0.3333333333333333703, 0.3333333333333333703, 0.3333333333333333148, 0.3333333333333333148, 0.3333333333333334259, 0.3333333333333333148, 0.3333333333333334814, 0.3333333333333333148, 0.3333333333333335924, 0.3333333333333333148, 0.3333333333333334259, 0.3333333333333333148, 0.3333333333333333703, 0.3333333333333333703, 0.3333333333333334814, 0.3333333333333332593, 0.3333333333333333703, 0.3333333333333333703, 0.3333333333333334259, 0.3333333333333333148, 0.3333333333333334259, 0.3333333333333333703, 0.3333333333333333703, 0.3333333333333333703),
 ( 0.3333333333333334259, 0.3333333333333334259, 0.3333333333333333703, 0.3333333333333334259, 0.3333333333333334259, 0.3333333333333334259, 0.3333333333333334259, 0.3333333333333332593, 0.3333333333333335369, 0.3333333333333332593, 0.3333333333333333703, 0.3333333333333334259, 0.3333333333333333703, 0.3333333333333332593, 0.3333333333333334814, 0.3333333333333332593, 0.3333333333333334259, 0.3333333333333334259, 0.3333333333333332593, 0.3333333333333335369, 0.3333333333333332038, 0.3333333333333335369, 0.3333333333333331483, 0.3333333333333334814, 0.3333333333333333148, 0.3333333333333333703, 0.3333333333333333703, 0.3333333333333333148, 0.3333333333333333703, 0.3333333333333333148, 0.3333333333333333703, 0.3333333333333333703, 0.3333333333333333703, 0.3333333333333333703, 0.3333333333333333703, 0.3333333333333333703, 0.3333333333333333148, 0.3333333333333333148, 0.3333333333333334259, 0.3333333333333332593, 0.3333333333333334259, 0.3333333333333333148, 0.3333333333333334259, 0.3333333333333333703, 0.3333333333333333148, 0.3333333333333334259, 0.3333333333333333703, 0.3333333333333333703, 0.3333333333333334259, 0.3333333333333333148, 0.3333333333333333703, 0.3333333333333332593, 0.3333333333333335369, 0.3333333333333333703, 0.3333333333333333148, 0.3333333333333334259, 0.3333333333333333703, 0.3333333333333333703, 0.3333333333333333148, 0.3333333333333333703, 0.3333333333333333703, 0.3333333333333334259, 0.3333333333333334259, 0.3333333333333334259, 0.3333333333333333703, 0.3333333333333333703, 0.3333333333333334259, 0.3333333333333333148, 0.3333333333333333703, 0.3333333333333334259, 0.3333333333333334259, 0.3333333333333332593, 0.3333333333333333703, 0.3333333333333334259, 0.3333333333333333703, 0.3333333333333334259, 0.3333333333333333148, 0.3333333333333334814, 0.3333333333333333148, 0.3333333333333332593, 0.3333333333333334259, 0.3333333333333333703, 0.3333333333333333148, 0.3333333333333333703, 0.3333333333333334259, 0.3333333333333334259, 0.3333333333333333148, 0.3333333333333333703, 0.3333333333333332593, 0.3333333333333333703, 0.3333333333333333703, 0.3333333333333333703, 0.3333333333333333703, 0.3333333333333333148, 0.3333333333333333703, 0.3333333333333333148, 0.3333333333333334259, 0.3333333333333333703, 0.3333333333333334259, 0.3333333333333333148, 0.3333333333333333703, 0.3333333333333333148, 0.3333333333333334259, 0.3333333333333333703, 0.3333333333333333703, 0.3333333333333333703, 0.3333333333333333703, 0.3333333333333333703, 0.3333333333333332593, 0.3333333333333333703, 0.3333333333333333703, 0.3333333333333335369, 0.3333333333333334259, 0.3333333333333333148, 0.3333333333333335369, 0.3333333333333333148, 0.3333333333333333703, 0.3333333333333333703, 0.3333333333333334259, 0.3333333333333333148, 0.3333333333333333703, 0.3333333333333334259, 0.3333333333333334259, 0.3333333333333333703, 0.3333333333333332593, 0.3333333333333334259, 0.3333333333333333703, 0.3333333333333334814, 0.3333333333333333148, 0.3333333333333333703, 0.3333333333333334259, 0.3333333333333333703, 0.3333333333333333148, 0.3333333333333333703, 0.3333333333333333148, 0.3333333333333334259, 0.3333333333333332593, 0.3333333333333334814, 0.3333333333333333703, 0.3333333333333334259, 0.3333333333333333703, 0.3333333333333333703, 0.3333333333333334259, 0.3333333333333333703, 0.3333333333333333703, 0.3333333333333333148, 0.3333333333333335924, 0.3333333333333333148, 0.3333333333333333703, 0.3333333333333334259, 0.3333333333333333148, 0.3333333333333334259, 0.3333333333333333148, 0.3333333333333334259, 0.3333333333333333703, 0.3333333333333334259, 0.3333333333333333703, 0.3333333333333333703, 0.3333333333333333703, 0.3333333333333334259, 0.3333333333333333703, 0.3333333333333334814, 0.3333333333333333148, 0.3333333333333334814, 0.3333333333333333148, 0.3333333333333333703, 0.3333333333333333148, 0.3333333333333333703, 0.3333333333333333703, 0.3333333333333333703, 0.3333333333333333703, 0.3333333333333333703, 0.3333333333333334259, 0.3333333333333333148, 0.3333333333333334259, 0.3333333333333333703, 0.3333333333333333703, 0.3333333333333333703, 0.3333333333333333703, 0.3333333333333333148, 0.3333333333333333703, 0.3333333333333334259, 0.3333333333333333148, 0.3333333333333334259, 0.3333333333333333148, 0.3333333333333333703, 0.3333333333333333703, 0.3333333333333333148, 0.3333333333333333703, 0.3333333333333334259, 0.3333333333333333148, 0.3333333333333334259, 0.3333333333333333703, 0.3333333333333332593, 0.3333333333333334814, 0.3333333333333332593, 0.3333333333333334259, 0.3333333333333333148, 0.3333333333333333703, 0.3333333333333334814, 0.3333333333333333703, 0.3333333333333333703, 0.3333333333333332593, 0.3333333333333334814, 0.3333333333333333148, 0.3333333333333333703, 0.3333333333333334259, 0.3333333333333333148, 0.3333333333333334259, 0.3333333333333333148, 0.3333333333333333703, 0.3333333333333333703, 0.3333333333333332593, 0.3333333333333333703, 0.3333333333333333703, 0.3333333333333334259, 0.3333333333333333148, 0.3333333333333334814, 0.3333333333333333703, 0.3333333333333334259, 0.3333333333333333148, 0.3333333333333334259, 0.3333333333333333703, 0.3333333333333333703, 0.3333333333333333703, 0.3333333333333333703, 0.3333333333333333148, 0.3333333333333334814, 0.3333333333333333703, 0.3333333333333333703, 0.3333333333333333148, 0.3333333333333334259, 0.3333333333333333703, 0.3333333333333332593, 0.3333333333333333703, 0.3333333333333333703, 0.3333333333333333703, 0.3333333333333334259, 0.3333333333333334259, 0.3333333333333333703, 0.3333333333333333703, 0.3333333333333333703, 0.3333333333333333703, 0.3333333333333334259, 0.3333333333333332593, 0.3333333333333335369, 0.3333333333333332038, 0.3333333333333333148, 0.3333333333333333703, 0.3333333333333333148, 0.3333333333333333148, 0.3333333333333334259, 0.3333333333333333703, 0.3333333333333333703, 0.3333333333333333703, 0.3333333333333334259, 0.3333333333333333148, 0.3333333333333334814, 0.3333333333333333703, 0.3333333333333334259, 0.3333333333333333703, 0.3333333333333333703, 0.3333333333333332593, 0.3333333333333333148, 0.3333333333333334814, 0.3333333333333333148, 0.3333333333333332593, 0.3333333333333334259, 0.3333333333333332038, 0.3333333333333334259, 0.3333333333333333148, 0.3333333333333333148, 0.3333333333333334259, 0.3333333333333333703, 0.3333333333333333703, 0.3333333333333333703, 0.3333333333333333703, 0.3333333333333334259, 0.3333333333333333148, 0.3333333333333333148, 0.3333333333333334259, 0.3333333333333333148, 0.3333333333333334259, 0.3333333333333333148, 0.3333333333333333703, 0.3333333333333334259, 0.3333333333333333148, 0.3333333333333334814, 0.3333333333333333148, 0.3333333333333334259, 0.3333333333333334259, 0.3333333333333333148, 0.3333333333333333148, 0.3333333333333335369, 0.3333333333333333148, 0.3333333333333333148, 0.3333333333333333703, 0.3333333333333335369, 0.3333333333333332593, 0.3333333333333335369, 0.3333333333333333148, 0.3333333333333333148, 0.3333333333333334259, 0.3333333333333333148, 0.3333333333333334259, 0.3333333333333333703, 0.3333333333333332593, 0.3333333333333333703, 0.3333333333333333148, 0.3333333333333334259, 0.3333333333333333148, 0.3333333333333334259, 0.3333333333333332593, 0.3333333333333335369, 0.3333333333333332038, 0.3333333333333334259, 0.3333333333333332593, 0.3333333333333335369, 0.3333333333333333148, 0.3333333333333334259, 0.3333333333333334259, 0.3333333333333333148, 0.3333333333333333148, 0.3333333333333334259, 0.3333333333333334814, 0.3333333333333333148, 0.3333333333333333148, 0.3333333333333334259, 0.3333333333333333703, 0.3333333333333334259, 0.3333333333333333148, 0.3333333333333333148, 0.3333333333333333703, 0.3333333333333333703, 0.3333333333333334814, 0.3333333333333333148, 0.3333333333333334259, 0.3333333333333333703, 0.3333333333333334259, 0.3333333333333334259, 0.3333333333333333148, 0.3333333333333333703, 0.3333333333333334259, 0.3333333333333333148, 0.3333333333333334814, 0.3333333333333333703, 0.3333333333333333148, 0.3333333333333333703, 0.3333333333333333148, 0.3333333333333334259, 0.3333333333333333148, 0.3333333333333333703, 0.3333333333333332593, 0.3333333333333334814, 0.3333333333333333703, 0.3333333333333334814, 0.3333333333333333148, 0.3333333333333334259, 0.3333333333333334814, 0.3333333333333333148, 0.3333333333333334259, 0.3333333333333332593, 0.3333333333333334259, 0.3333333333333333703, 0.3333333333333333703, 0.3333333333333333148, 0.3333333333333333148, 0.3333333333333334259, 0.3333333333333333148, 0.3333333333333334814, 0.3333333333333333148, 0.3333333333333335924, 0.3333333333333333148, 0.3333333333333334259, 0.3333333333333333148, 0.3333333333333333703, 0.3333333333333333703, 0.3333333333333334814, 0.3333333333333332593, 0.3333333333333333703, 0.3333333333333333703, 0.3333333333333334259, 0.3333333333333333148, 0.3333333333333334259, 0.3333333333333333703, 0.3333333333333333703, 0.3333333333333333703),
 ( 1.000000000000000222, 1.000000000000000222, 1.000000000000000222, 1.000000000000000000, 1.000000000000000000, 1.000000000000000444, 1.000000000000000000, 0.9999999999999997780, 1.000000000000000444, 0.9999999999999997780, 0.9999999999999997780, 1.000000000000000222, 0.9999999999999997780, 0.9999999999999997780, 1.000000000000000444, 0.9999999999999997780, 1.000000000000000222, 1.000000000000000222, 0.9999999999999996669, 1.000000000000000222, 0.9999999999999996669, 1.000000000000000444, 0.9999999999999994449, 1.000000000000000444, 0.9999999999999996669, 1.000000000000000222, 1.000000000000000000, 0.9999999999999997780, 1.000000000000000222, 0.9999999999999997780, 1.000000000000000000, 0.9999999999999997780, 1.000000000000000000, 1.000000000000000222, 0.9999999999999996669, 1.000000000000000000, 0.9999999999999997780, 1.000000000000000000, 1.000000000000000444, 0.9999999999999996669, 1.000000000000000222, 1.000000000000000000, 1.000000000000000222, 1.000000000000000222, 0.9999999999999997780, 0.9999999999999997780, 1.000000000000000222, 0.9999999999999997780, 1.000000000000000222, 0.9999999999999997780, 0.9999999999999997780, 0.9999999999999997780, 1.000000000000000444, 1.000000000000000000, 0.9999999999999997780, 1.000000000000000222, 1.000000000000000000, 1.000000000000000000, 0.9999999999999997780, 1.000000000000000222, 1.000000000000000000, 1.000000000000000000, 1.000000000000000222, 1.000000000000000000, 1.000000000000000000, 1.000000000000000000, 1.000000000000000222, 1.000000000000000000, 0.9999999999999997780, 1.000000000000000444, 1.000000000000000000, 0.9999999999999997780, 1.000000000000000000, 1.000000000000000222, 0.9999999999999997780, 1.000000000000000222, 0.9999999999999996669, 1.000000000000000222, 1.000000000000000000, 1.000000000000000000, 1.000000000000000000, 1.000000000000000222, 0.9999999999999997780, 1.000000000000000000, 1.000000000000000222, 0.9999999999999997780, 1.000000000000000000, 1.000000000000000000, 0.9999999999999996669, 1.000000000000000000, 1.000000000000000000, 1.000000000000000222, 1.000000000000000000, 0.9999999999999997780, 1.000000000000000222, 0.9999999999999996669, 1.000000000000000222, 0.9999999999999997780, 1.000000000000000000, 1.000000000000000000, 1.000000000000000222, 0.9999999999999996669, 1.000000000000000444, 1.000000000000000000, 0.9999999999999997780, 1.000000000000000000, 1.000000000000000000, 1.000000000000000222, 0.9999999999999997780, 1.000000000000000000, 1.000000000000000222, 1.000000000000000444, 1.000000000000000000, 1.000000000000000000, 1.000000000000000444, 1.000000000000000000, 0.9999999999999997780, 1.000000000000000222, 1.000000000000000000, 1.000000000000000000, 1.000000000000000000, 1.000000000000000000, 1.000000000000000000, 1.000000000000000000, 0.9999999999999996669, 1.000000000000000222, 0.9999999999999997780, 1.000000000000000222, 1.000000000000000000, 0.9999999999999997780, 1.000000000000000222, 0.9999999999999997780, 0.9999999999999997780, 0.9999999999999997780, 1.000000000000000000, 1.000000000000000000, 0.9999999999999996669, 1.000000000000000444, 1.000000000000000222, 1.000000000000000000, 1.000000000000000000, 1.000000000000000222, 1.000000000000000222, 1.000000000000000000, 1.000000000000000222, 0.9999999999999996669, 1.000000000000000444, 0.9999999999999997780, 0.9999999999999997780, 1.000000000000000444, 1.000000000000000000, 1.000000000000000222, 0.9999999999999997780, 1.000000000000000222, 1.000000000000000000, 1.000000000000000222, 1.000000000000000000, 1.000000000000000000, 0.9999999999999996669, 1.000000000000000444, 1.000000000000000000, 1.000000000000000222, 0.9999999999999997780, 1.000000000000000000, 1.000000000000000000, 1.000000000000000000, 1.000000000000000000, 0.9999999999999997780, 1.000000000000000000, 1.000000000000000000, 1.000000000000000000, 1.000000000000000222, 1.000000000000000222, 0.9999999999999997780, 1.000000000000000000, 1.000000000000000000, 0.9999999999999997780, 1.000000000000000000, 1.000000000000000000, 1.000000000000000000, 1.000000000000000000, 1.000000000000000444, 0.9999999999999997780, 1.000000000000000222, 0.9999999999999997780, 1.000000000000000000, 1.000000000000000222, 0.9999999999999997780, 1.000000000000000222, 1.000000000000000000, 1.000000000000000000, 1.000000000000000000, 1.000000000000000000, 0.9999999999999997780, 1.000000000000000000, 1.000000000000000000, 1.000000000000000000, 1.000000000000000000, 1.000000000000000000, 1.000000000000000222, 1.000000000000000000, 1.000000000000000222, 0.9999999999999997780, 1.000000000000000222, 0.9999999999999997780, 1.000000000000000222, 1.000000000000000000, 0.9999999999999997780, 1.000000000000000222, 0.9999999999999996669, 1.000000000000000444, 1.000000000000000000, 0.9999999999999996669, 1.000000000000000222, 1.000000000000000000, 1.000000000000000222, 0.9999999999999997780, 1.000000000000000444, 1.000000000000000000, 1.000000000000000000, 0.9999999999999997780, 1.000000000000000222, 1.000000000000000000, 1.000000000000000000, 1.000000000000000000, 1.000000000000000222, 0.9999999999999997780, 1.000000000000000222, 1.000000000000000000, 0.9999999999999997780, 1.000000000000000000, 0.9999999999999997780, 1.000000000000000222, 0.9999999999999996669, 1.000000000000000000, 1.000000000000000000, 1.000000000000000000, 1.000000000000000444, 1.000000000000000222, 1.000000000000000000, 1.000000000000000000, 0.9999999999999997780, 0.9999999999999997780, 1.000000000000000444, 0.9999999999999996669, 1.000000000000000444, 0.9999999999999997780, 0.9999999999999997780, 1.000000000000000222, 0.9999999999999997780, 0.9999999999999996669, 1.000000000000000444, 0.9999999999999997780, 1.000000000000000222, 1.000000000000000222, 1.000000000000000000, 0.9999999999999997780, 1.000000000000000222, 1.000000000000000000, 1.000000000000000222, 1.000000000000000000, 1.000000000000000000, 0.9999999999999997780, 0.9999999999999997780, 1.000000000000000444, 0.9999999999999997780, 0.9999999999999997780, 1.000000000000000222, 0.9999999999999994449, 1.000000000000000222, 0.9999999999999997780, 1.000000000000000000, 0.9999999999999997780, 1.000000000000000000, 1.000000000000000000, 1.000000000000000000, 1.000000000000000000, 1.000000000000000000, 1.000000000000000000, 1.000000000000000000, 1.000000000000000222, 1.000000000000000000, 1.000000000000000000, 1.000000000000000000, 1.000000000000000000, 1.000000000000000000, 1.000000000000000000, 1.000000000000000000, 1.000000000000000222, 1.000000000000000000, 1.000000000000000222, 0.9999999999999997780, 1.000000000000000000, 1.000000000000000444, 1.000000000000000000, 1.000000000000000000, 1.000000000000000000, 1.000000000000000222, 0.9999999999999997780, 1.000000000000000444, 0.9999999999999997780, 1.000000000000000222, 1.000000000000000000, 1.000000000000000000, 1.000000000000000000, 1.000000000000000222, 0.9999999999999994449, 1.000000000000000222, 1.000000000000000000, 1.000000000000000000, 1.000000000000000000, 0.9999999999999997780, 0.9999999999999997780, 1.000000000000000444, 0.9999999999999996669, 1.000000000000000222, 0.9999999999999997780, 1.000000000000000444, 0.9999999999999997780, 1.000000000000000222, 1.000000000000000222, 0.9999999999999996669, 1.000000000000000222, 1.000000000000000000, 1.000000000000000444, 1.000000000000000000, 1.000000000000000000, 1.000000000000000222, 1.000000000000000000, 1.000000000000000000, 0.9999999999999997780, 0.9999999999999997780, 1.000000000000000000, 0.9999999999999997780, 1.000000000000000222, 1.000000000000000222, 1.000000000000000000, 1.000000000000000222, 1.000000000000000222, 1.000000000000000000, 0.9999999999999997780, 0.9999999999999997780, 1.000000000000000222, 0.9999999999999997780, 1.000000000000000222, 1.000000000000000000, 1.000000000000000000, 1.000000000000000000, 0.9999999999999996669, 1.000000000000000222, 0.9999999999999997780, 1.000000000000000000, 0.9999999999999997780, 1.000000000000000222, 0.9999999999999997780, 1.000000000000000444, 0.9999999999999996669, 1.000000000000000222, 1.000000000000000222, 1.000000000000000000, 1.000000000000000000, 0.9999999999999997780, 1.000000000000000222, 0.9999999999999997780, 1.000000000000000222, 0.9999999999999997780, 0.9999999999999997780, 1.000000000000000000, 1.000000000000000000, 1.000000000000000222, 1.000000000000000000, 1.000000000000000444, 0.9999999999999997780, 1.000000000000000222, 0.9999999999999997780, 0.9999999999999997780, 1.000000000000000222, 1.000000000000000000, 0.9999999999999997780, 1.000000000000000000, 1.000000000000000000, 1.000000000000000000, 0.9999999999999997780, 1.000000000000000444, 0.9999999999999997780, 1.000000000000000000, 1.000000000000000000) ) ) 
 REPRESENTATION_ITEM ( '' )  SURFACE ( )  );
#81466 = CARTESIAN_POINT ( 'NONE',  ( 2.596233987490266681, -0.9813665562012074961, 1.641104690102652919 ) ) ;
#81467 = CARTESIAN_POINT ( 'NONE',  ( 3.326767387183640956, 0.04228616847017605679, 1.769505212706389941 ) ) ;
#81468 = CARTESIAN_POINT ( 'NONE',  ( 1.102048709075389654, -0.8591247869965330519, 1.708478583560539166 ) ) ;
#81470 = CARTESIAN_POINT ( 'NONE',  ( 5.571877068885287443, -0.8567909204831600789, 1.713377365699362054 ) ) ;
#81469 = CARTESIAN_POINT ( 'NONE',  ( 7.137427359598738086, -7.616807914308158622, -7.137427359597695364 ) ) ;
#81471 = CARTESIAN_POINT ( 'NONE',  ( 6.338338845641732888, -1.054863691225367939, 1.663055945198953278 ) ) ;
#81472 = CARTESIAN_POINT ( 'NONE',  ( 1.499999999999989120, 4.254166666666687746, 0.8660254037844524744 ) ) ;
#81473 = CARTESIAN_POINT ( 'NONE',  ( 1.512141599020993432, -0.7094941370262074498, 1.998545949238240027 ) ) ;
#81474 = CARTESIAN_POINT ( 'NONE',  ( 3.177206141917496840, 8.963489737286222336, -2.500000000000001332 ) ) ;
#81475 = CARTESIAN_POINT ( 'NONE',  ( 5.260568668178753349, -1.354309965608934352, 1.290672426560689035 ) ) ;
#81477 = ORIENTED_EDGE ( 'NONE', *, *, #34501, .F. ) ;
#81476 = CARTESIAN_POINT ( 'NONE',  ( 0.3986991128735201673, 1.519733473351183362, -1.011397189243423700 ) ) ;
#81479 = CARTESIAN_POINT ( 'NONE',  ( 3.834746474454188013E-15, 12.31250000000000178, 1.500000000000001554 ) ) ;
#81478 = CARTESIAN_POINT ( 'NONE',  ( 4.776106669258010307, 1.268914099295117781, 1.805409367619143390 ) ) ;
#81480 = CARTESIAN_POINT ( 'NONE',  ( 0.6823417656249917140, 4.405208333674755394, 1.181850606188765695 ) ) ;
#81481 = CARTESIAN_POINT ( 'NONE',  ( 2.066913078360913314, 1.530046405743747506, -1.383527225477628297 ) ) ;
#81482 = CARTESIAN_POINT ( 'NONE',  ( 5.124091990960999432, 8.065525525174782828, -1.199719254218452047 ) ) ;
#81483 = CARTESIAN_POINT ( 'NONE',  ( -7.557780564614042795, 10.90482886110335414, -1.199719254218446718 ) ) ;
#81484 = SURFACE_STYLE_FILL_AREA ( #212532 ) ;
#81485 = CARTESIAN_POINT ( 'NONE',  ( 11.96535697748089078, 11.25262667064446198, -0.9148528286454237213 ) ) ;
#81486 = CARTESIAN_POINT ( 'NONE',  ( 7.343676480457483002, 8.596652644402405841, -1.199719254218452047 ) ) ;
#81487 = VERTEX_POINT ( 'NONE', #148839 ) ;
#81488 = CARTESIAN_POINT ( 'NONE',  ( 4.334477209444560053, -1.194628513295314942, 1.690740121169509447 ) ) ;
#81489 = CARTESIAN_POINT ( 'NONE',  ( -0.7499999999999972244, 5.608333333333353821, -1.299038105676652011 ) ) ;
#81490 = CARTESIAN_POINT ( 'NONE',  ( 1.845224345143604561, -1.827161268409679407, 1.154667503900350223 ) ) ;
#81491 = CARTESIAN_POINT ( 'NONE',  ( -6.087706144486034532, 7.033779493390481363, -0.9955609822858858537 ) ) ;
#81492 = CARTESIAN_POINT ( 'NONE',  ( 1.910812834059022469, -0.5409473409442880909, -1.945794739053583466 ) ) ;
#81493 = CARTESIAN_POINT ( 'NONE',  ( 4.292412370785825715, 7.263935575258185118, -1.002239974148201762 ) ) ;
#81494 = EDGE_LOOP ( 'NONE', ( #164201, #34516, #98211, #113989 ) ) ;
#81495 = AXIS2_PLACEMENT_3D ( 'NONE', #50660, #116786, #182783 ) ;
#81497 = CARTESIAN_POINT ( 'NONE',  ( 7.700668062882064291, 10.00719871149432549, -1.443375672974057666 ) ) ;
#81496 = CARTESIAN_POINT ( 'NONE',  ( 3.475000000000000533, -2.624999999999998668, 0.000000000000000000 ) ) ;
#81498 = CARTESIAN_POINT ( 'NONE',  ( -1.063873381751401226E-14, -5.907420853759270507, 11.00029519899100094 ) ) ;
#81499 = CARTESIAN_POINT ( 'NONE',  ( 0.6906390985809904848, 1.523792322931913468, -1.320830384837400118 ) ) ;
#81500 = CARTESIAN_POINT ( 'NONE',  ( 5.460537066722415567, -1.980877156148381335, -0.9378266216248376530 ) ) ;
#81501 = CARTESIAN_POINT ( 'NONE',  ( 0.7499999999999920064, 4.764583334016150751, 1.299038105676669330 ) ) ;
#81502 = CARTESIAN_POINT ( 'NONE',  ( 3.041163856788456687, 0.05134138945498378792, 1.911883771832747048 ) ) ;
#81503 = CARTESIAN_POINT ( 'NONE',  ( -3.846762897975357198, 5.510976019103107859, -1.599625672291256295 ) ) ;
#81504 = CARTESIAN_POINT ( 'NONE',  ( 5.788968402910805722, 7.776882441527838807, 1.443375672974062551 ) ) ;
#81506 = CARTESIAN_POINT ( 'NONE',  ( 2.021111450618333194, -1.799914642762674433, 0.9091633978678403949 ) ) ;
#81505 = CARTESIAN_POINT ( 'NONE',  ( -8.609064354553318310, 12.98773281371349775, 0.7216878364870317197 ) ) ;
#81507 = CARTESIAN_POINT ( 'NONE',  ( -1.364683531250000748, 11.92187500034139980, 0.000000000000000000 ) ) ;
#81509 = CARTESIAN_POINT ( 'NONE',  ( -5.354544322754380303, 5.211666229493680191, 0.7998128361456281477 ) ) ;
#81508 = CARTESIAN_POINT ( 'NONE',  ( -0.05846771364293941453, -1.777572824190313261, -1.447063799157372044 ) ) ;
#81510 = CARTESIAN_POINT ( 'NONE',  ( 4.155083606764530479, -1.434382041474260516, -0.9574503856549732017 ) ) ;
#81511 = CARTESIAN_POINT ( 'NONE',  ( 6.016786309414542622, 10.24161080428416426, 0.7998128361456341429 ) ) ;
#81512 = CARTESIAN_POINT ( 'NONE',  ( 3.822509244049070887, 6.547012320444182798, -1.199719254218452047 ) ) ;
#81513 = DIRECTION ( 'NONE',  ( 0.000000000000000000, 0.000000000000000000, 1.000000000000000000 ) ) ;
#81514 = CARTESIAN_POINT ( 'NONE',  ( 3.785751206713845018, 5.439795712631356750, 1.599625672291267398 ) ) ;
#81515 = CARTESIAN_POINT ( 'NONE',  ( 0.1753634416057497647, 0.2329791690731698173, -2.177930625204091086 ) ) ;
#81516 =( BOUNDED_SURFACE ( )  B_SPLINE_SURFACE ( 3, 2, ( 
 ( #89746, #155795, #24704 ),
 ( #191468, #61484, #10587 ),
 ( #209845, #76662, #11658 ),
 ( #90806, #77731, #74544 ),
 ( #43133, #109249, #188274 ),
 ( #192533, #44187, #7379 ),
 ( #110307, #73458, #176315 ),
 ( #27919, #94015, #139560 ) ),
 .UNSPECIFIED., .F., .F., .T. ) 
 B_SPLINE_SURFACE_WITH_KNOTS ( ( 4, 2, 2, 4 ),
 ( 3, 3 ),
 ( 0.000000000000000000, 0.0002469787127373868161, 0.0004939574254747736322, 0.0009879148509495472644 ),
 ( 0.000000000000000000, 1.000000000000000000 ),
 .UNSPECIFIED. ) 
 GEOMETRIC_REPRESENTATION_ITEM ( )  RATIONAL_B_SPLINE_SURFACE ( (
 ( 1.000000000000000000, 0.3826834323650766811, 1.000000000000000000),
 ( 1.000000000000000000, 0.3798541548343959406, 1.000000000000000000),
 ( 1.000000000000000000, 0.3995981355978913130, 1.000000000000000000),
 ( 1.000000000000000000, 0.4556299950042939639, 1.000000000000000000),
 ( 1.000000000000000000, 0.4903550589607226229, 1.000000000000000000),
 ( 1.000000000000000000, 0.5915489574623006286, 1.000000000000000000),
 ( 1.000000000000000000, 0.6554239218402544420, 1.000000000000000000),
 ( 1.000000000000000000, 0.7100530722070637069, 1.000000000000000000) ) ) 
 REPRESENTATION_ITEM ( '' )  SURFACE ( )  );
#81517 = ORIENTED_EDGE ( 'NONE', *, *, #125041, .T. ) ;
#81518 = CARTESIAN_POINT ( 'NONE',  ( 5.584552742667589165, -1.144318741887658586, 1.404276898221923364 ) ) ;
#81519 = VERTEX_POINT ( 'NONE', #63326 ) ;
#81520 = CARTESIAN_POINT ( 'NONE',  ( 8.269583629331492602, 11.73526576994040482, 1.199719254218450271 ) ) ;
#81521 = CARTESIAN_POINT ( 'NONE',  ( 5.448397627845284141, 7.449826213943242514, 1.599625672291268286 ) ) ;
#81522 = DIRECTION ( 'NONE',  ( 0.000000000000000000, 0.000000000000000000, -1.000000000000000000 ) ) ;
#81523 = CARTESIAN_POINT ( 'NONE',  ( 6.270143006926431006, 1.806086713848788161, -0.1406222877055433862 ) ) ;
#81524 = CARTESIAN_POINT ( 'NONE',  ( 5.017926250389229459, 8.868348035513836436, 0.000000000000000000 ) ) ;
#81525 = FACE_OUTER_BOUND ( 'NONE', #79154, .T. ) ;
#81526 = CARTESIAN_POINT ( 'NONE',  ( 2.607599380506659514, -2.167453834138896696, 0.3226137089109848421 ) ) ;
#81528 = CARTESIAN_POINT ( 'NONE',  ( 8.971744963941056028, 11.49012176272984931, 1.599625672291281386 ) ) ;
#81527 = CARTESIAN_POINT ( 'NONE',  ( 6.232830220009587308, -1.767433141015135822, -0.5829711297899267120 ) ) ;
#81529 = CARTESIAN_POINT ( 'NONE',  ( 3.743669890235715947, 1.900728030520698830, -0.2378226680747745625 ) ) ;
#81530 = DIRECTION ( 'NONE',  ( -2.126226658603517140E-31, 1.665334536937738015E-16, 1.000000000000000000 ) ) ;
#81531 = CARTESIAN_POINT ( 'NONE',  ( 0.000000000000000000, 8.980740528189222971, 0.000000000000000000 ) ) ;
#81532 = CARTESIAN_POINT ( 'NONE',  ( 0.6823417656249882723, -0.07395833299191079124, -1.181850606188749264 ) ) ;
#81533 = CARTESIAN_POINT ( 'NONE',  ( 6.046573322014824114, 7.117052299514516456, -1.082531754730543083 ) ) ;
#81534 = CARTESIAN_POINT ( 'NONE',  ( -8.649738815838677652, 13.03518635187974262, 0.7216878364870357165 ) ) ;
#81535 = CARTESIAN_POINT ( 'NONE',  ( 0.7433210806352362754, -1.853469564684958382, 1.112228649290482263 ) ) ;
#81536 = CARTESIAN_POINT ( 'NONE',  ( -5.123001941117347080, 7.070197912760590064, 1.599625672291263179 ) ) ;
#81537 = CARTESIAN_POINT ( 'NONE',  ( 3.230585741806197841, 6.991043475407723307, 0.7998128361456271485 ) ) ;
#81538 = CARTESIAN_POINT ( 'NONE',  ( 0.2877648253245302379, -0.8656086203641421006, 1.607325130595547602 ) ) ;
#81539 = CARTESIAN_POINT ( 'NONE',  ( -4.115063316947640715, 4.759660943649018705, 1.199719254218462483 ) ) ;
#81540 = CARTESIAN_POINT ( 'NONE',  ( 3.504746488097260748, 1.439749907568649068, -1.122338611188322455 ) ) ;
#81541 = CARTESIAN_POINT ( 'NONE',  ( 9.010018398950542462, 11.11739593148128158, 8.024259704181407216 ) ) ;
#81542 = ORIENTED_EDGE ( 'NONE', *, *, #6348, .F. ) ;
#81543 = CARTESIAN_POINT ( 'NONE',  ( 3.051173608728700248, 1.690664904776484789, -1.010063219348409813 ) ) ;
#81544 = ORIENTED_EDGE ( 'NONE', *, *, #143656, .F. ) ;
#81545 = CARTESIAN_POINT ( 'NONE',  ( 5.056170473960743372, -1.404048225252243265, 1.341958350743667205 ) ) ;
#81546 = CARTESIAN_POINT ( 'NONE',  ( -6.064239847062411926, 10.29697326487330500, 0.000000000000000000 ) ) ;
#81548 = CARTESIAN_POINT ( 'NONE',  ( 5.431924468521282634, -2.068440459917933794, 0.4666711972392265650 ) ) ;
#81547 = CARTESIAN_POINT ( 'NONE',  ( 4.830447868218803897, 8.857549289555754157, -0.7998128361456481317 ) ) ;
#81549 = DIRECTION ( 'NONE',  ( 0.000000000000000000, 0.000000000000000000, -1.000000000000000000 ) ) ;
#81550 = CARTESIAN_POINT ( 'NONE',  ( 3.299369280271017946, 1.727720890571235124, -0.8199460011262191816 ) ) ;
#81551 = CARTESIAN_POINT ( 'NONE',  ( 5.803731464950218744, 6.215061796778338810, -0.9591748237987550718 ) ) ;
#81552 = CARTESIAN_POINT ( 'NONE',  ( -4.480905194642735623, 5.440750306600657282, -1.194628488029887414 ) ) ;
#81553 = CARTESIAN_POINT ( 'NONE',  ( 3.770049233051776749, 6.556085317605844232, 1.199719254218451159 ) ) ;
#81554 = CARTESIAN_POINT ( 'NONE',  ( 4.477201648280199286, -1.799136850145161892, -0.9032412251695760563 ) ) ;
#81555 = FACE_OUTER_BOUND ( 'NONE', #2164, .T. ) ;
#81556 = CARTESIAN_POINT ( 'NONE',  ( 5.180226163740526246, -1.011166736308216629, 1.519887457628710248 ) ) ;
#81557 = CARTESIAN_POINT ( 'NONE',  ( 0.9771079587245214970, 1.912259438035465386, 0.7939916666956441382 ) ) ;
#81558 = CARTESIAN_POINT ( 'NONE',  ( -8.351459436338041442, 9.806086099558291025, -1.082531754730543971 ) ) ;
#81559 = CARTESIAN_POINT ( 'NONE',  ( -6.592485395868785680, 6.772832640907240354, 0.2792626473412176957 ) ) ;
#81560 = CARTESIAN_POINT ( 'NONE',  ( -0.4000000000000200617, 3.963633530850230180, -0.9046180958551521822 ) ) ;
#81561 = CARTESIAN_POINT ( 'NONE',  ( 5.366025703835962446, 0.9229158262306772498, 1.627043297953718382 ) ) ;
#81562 = CARTESIAN_POINT ( 'NONE',  ( 5.750629710490689384, 9.860818428881154674, -0.7998128361456291469 ) ) ;
#81563 = CARTESIAN_POINT ( 'NONE',  ( -5.922214171070950606, 5.803671375871217286, -0.7998128361456291469 ) ) ;
#81564 = CARTESIAN_POINT ( 'NONE',  ( 2.367870383881045981, 5.914265881169853856, 0.000000000000000000 ) ) ;
#81565 = CARTESIAN_POINT ( 'NONE',  ( 1.364683531249996529, 10.02604166700806587, 0.7879004041258405033 ) ) ;
#81566 = CARTESIAN_POINT ( 'NONE',  ( -4.252453736180621391, 8.112946458852704268, -0.7998128361456281477 ) ) ;
#81568 = CARTESIAN_POINT ( 'NONE',  ( -5.745623237141265882, 9.925253886631958622, 0.7998128361456291469 ) ) ;
#81567 = CARTESIAN_POINT ( 'NONE',  ( 4.871457266011829823, 4.577788319968905562, -0.7998128361456221525 ) ) ;
#81569 = EDGE_CURVE ( 'NONE', #49308, #145598, #18315, .T. ) ;
#81570 = CARTESIAN_POINT ( 'NONE',  ( -4.380693030546956912, 6.204170850428461392, 1.443375672974065660 ) ) ;
#81571 = CIRCLE ( 'NONE', #29793, 2.000000000000000000 ) ;
#81572 = CARTESIAN_POINT ( 'NONE',  ( -6.067437437315529536, 7.037430750744921859, 1.199719254218450271 ) ) ;
#81573 = CARTESIAN_POINT ( 'NONE',  ( 1.446235060908855008, -0.9343481645287862181, 1.847524432027500385 ) ) ;
#81574 = CARTESIAN_POINT ( 'NONE',  ( 2.671616206378808478, 1.499349897650571695, 1.495110359788552223 ) ) ;
#81575 = VECTOR ( 'NONE', #109488, 1000.000000000000000 ) ;
#81576 = CARTESIAN_POINT ( 'NONE',  ( 9.134442807305049428, 11.67993591332117376, 1.599625672291281386 ) ) ;
#81577 = CARTESIAN_POINT ( 'NONE',  ( 5.484430959185962351, 6.043327615839653610, 0.8208683321978844649 ) ) ;
#81578 = CARTESIAN_POINT ( 'NONE',  ( 0.3562224712859492493, -1.968894089644295686, -0.05400687454796929826 ) ) ;
#81579 = CARTESIAN_POINT ( 'NONE',  ( 4.441740843186996912, 7.307116142998927977, 1.228109861675081849 ) ) ;
#81580 = CARTESIAN_POINT ( 'NONE',  ( 3.863710590214593399, 7.451486755318259547, 1.040834085586084257E-14 ) ) ;
#81582 = DIRECTION ( 'NONE',  ( -1.000000000000000000, 1.014813233446432150E-15, 1.972152263052529514E-31 ) ) ;
#81581 = CARTESIAN_POINT ( 'NONE',  ( 1.001543065824772753E-15, -3.412500000000000977, 4.012584370867899430 ) ) ;
#81583 = CARTESIAN_POINT ( 'NONE',  ( 3.012002838297692886, -1.130384021687063534, -1.994099915080405294 ) ) ;
#81584 = CARTESIAN_POINT ( 'NONE',  ( 0.04711308451243316486, -1.408776630263553375, -1.161003007932148501 ) ) ;
#81585 = CARTESIAN_POINT ( 'NONE',  ( 2.601700882821424976, 1.355260107747566334, 1.349524769375435973 ) ) ;
#81586 = CARTESIAN_POINT ( 'NONE',  ( 8.392133896734671694, 8.893170422386358354, 0.7216878364870458196 ) ) ;
#81587 = CARTESIAN_POINT ( 'NONE',  ( 0.3518148739534024960, -1.426620726115679361, -1.420723246562720421 ) ) ;
#81588 = CARTESIAN_POINT ( 'NONE',  ( 1.551531708069888715, 1.481957716508151890, 1.285475804911541120 ) ) ;
#81589 = CARTESIAN_POINT ( 'NONE',  ( -10.45741655484220267, 11.09474082360439873, -0.7998128361456221525 ) ) ;
#81590 = CARTESIAN_POINT ( 'NONE',  ( -6.795661308947694934, 8.951357498570873261, -1.599625672291263179 ) ) ;
#81591 = CARTESIAN_POINT ( 'NONE',  ( -7.698131257602420341, -5.543994141378503215, -7.787098537122147945 ) ) ;
#81593 = CARTESIAN_POINT ( 'NONE',  ( 2.219294626563913297, -1.717429429511443173, 0.4269959701016200482 ) ) ;
#81592 = CARTESIAN_POINT ( 'NONE',  ( 3.732441334599644556, 0.3067963083541249691, 2.067875747930392638 ) ) ;
#81594 = CARTESIAN_POINT ( 'NONE',  ( 0.000000000000000000, 5.999999999999998224, 0.000000000000000000 ) ) ;
#81596 = CARTESIAN_POINT ( 'NONE',  ( 5.402359069383361856, 1.738778441700383315, -1.493778605308769603 ) ) ;
#81595 = CARTESIAN_POINT ( 'NONE',  ( -11.51301453142883346, 6.867562542198304421, 3.390093443801430073 ) ) ;
#81597 = CARTESIAN_POINT ( 'NONE',  ( 4.822041096100106117, 1.666637052750892911, 0.5010418475075908429 ) ) ;
#81598 = CARTESIAN_POINT ( 'NONE',  ( 8.215351014876830504, 11.67199438640995801, -1.199719254218446718 ) ) ;
#81599 = FILL_AREA_STYLE_COLOUR ( '', #28867 ) ;
#81600 = CARTESIAN_POINT ( 'NONE',  ( 4.692597494581693063, -1.067344209891357032, -1.366281018423552762 ) ) ;
#81601 = CARTESIAN_POINT ( 'NONE',  ( 4.580651514471745678, 1.339088007528920210, -1.708959110978137019 ) ) ;
#81602 = CARTESIAN_POINT ( 'NONE',  ( 4.090809663021327758, 5.795697244990093644, 1.599625672291267398 ) ) ;
#81603 = CARTESIAN_POINT ( 'NONE',  ( 5.964077395145578109, -1.074666730956087335, 1.706109649615504154 ) ) ;
#81605 = TOROIDAL_SURFACE ( 'NONE', #140407, 11.92000000000000348, 0.08000000000000000167 ) ;
#81604 = CARTESIAN_POINT ( 'NONE',  ( 0.2499999969303341174, 7.552774431159578439E-08, 2.052068128417954274 ) ) ;
#81606 = CARTESIAN_POINT ( 'NONE',  ( -1.001543065824772872E-14, 4.493750000682820378, 1.732050807568877637 ) ) ;
#81607 = CARTESIAN_POINT ( 'NONE',  ( 3.153258193586833347, -1.574033464040735408, -1.110325110657943481 ) ) ;
#81608 = CARTESIAN_POINT ( 'NONE',  ( 0.7500000000000006661, 10.44791666734946212, -1.299038105676657340 ) ) ;
#81609 = CARTESIAN_POINT ( 'NONE',  ( 6.012022869640524014, -0.7491050530544652863, 2.091446645375413027 ) ) ;
#81610 = ORIENTED_EDGE ( 'NONE', *, *, #79549, .T. ) ;
#81611 = CARTESIAN_POINT ( 'NONE',  ( 6.883263157960401557, 2.461427291499204362, 2.229941283862615808 ) ) ;
#81612 = CARTESIAN_POINT ( 'NONE',  ( -1.499999999999997780, 2.900000000000020783, 1.214306433183764966E-14 ) ) ;
#81613 = CARTESIAN_POINT ( 'NONE',  ( 4.611744806942754238, 8.532119374741881757, -0.7998128361456231517 ) ) ;
#81614 = CARTESIAN_POINT ( 'NONE',  ( 1.208037074693757651, 1.685330760668615646, 1.447128815913247379 ) ) ;
#81615 = CARTESIAN_POINT ( 'NONE',  ( 1.499999999999990896, 4.775000000000022560, 1.214306433183764966E-14 ) ) ;
#81616 = CARTESIAN_POINT ( 'NONE',  ( 6.466876084038451822, 10.48851316477946582, 1.040834085586084257E-14 ) ) ;
#81617 = FACE_OUTER_BOUND ( 'NONE', #90107, .T. ) ;
#81618 = CARTESIAN_POINT ( 'NONE',  ( 4.065465959251388206, 5.836405933916976707, -1.599625672291269396 ) ) ;
#81619 = CARTESIAN_POINT ( 'NONE',  ( -5.004368097219957789, 5.011053332944274352, 0.000000000000000000 ) ) ;
#81621 = CARTESIAN_POINT ( 'NONE',  ( 4.791499389596598490, -1.887151845835168817, 0.8330235203531827226 ) ) ;
#81620 = CARTESIAN_POINT ( 'NONE',  ( -5.608633734226008194, 5.643391804966442216, 0.4859901473732997079 ) ) ;
#81622 = CARTESIAN_POINT ( 'NONE',  ( -5.264643720808155791, 5.036505850564608089, 0.000000000000000000 ) ) ;
#81623 = CARTESIAN_POINT ( 'NONE',  ( -0.7499999999999972244, 5.639583334016151639, -1.299038105676652899 ) ) ;
#81624 = CARTESIAN_POINT ( 'NONE',  ( 1.364683531249986537, -0.8864583329919110133, 0.7879004041258500513 ) ) ;
#81625 = CARTESIAN_POINT ( 'NONE',  ( 5.624238404463478780, 1.114819804898508515, -1.501858222471161408 ) ) ;
#81626 = CARTESIAN_POINT ( 'NONE',  ( 5.133366751340045830, 0.5111148723837605212, 1.657103328152222055 ) ) ;
#81627 = CARTESIAN_POINT ( 'NONE',  ( 4.212277857634297185, 1.593487861523819271, 0.7003764074154511521 ) ) ;
#81628 = CARTESIAN_POINT ( 'NONE',  ( 3.323720213644492993, 7.029424015893889433, 1.040834085586084257E-14 ) ) ;
#81629 = CARTESIAN_POINT ( 'NONE',  ( 2.331904285594294191, 1.077338530963572127, -2.023425408739158105 ) ) ;
#81630 = CARTESIAN_POINT ( 'NONE',  ( -0.6823417656249969321, 5.030208333674755394, -1.181850606188749264 ) ) ;
#81631 = CARTESIAN_POINT ( 'NONE',  ( 0.7613493127172387132, 0.9053670157611827252, 1.603083849714491027 ) ) ;
#81632 = CIRCLE ( 'NONE', #175043, 0.1000000000000001027 ) ;
#81633 = EDGE_CURVE ( 'NONE', #121309, #23505, #113936, .T. ) ;
#81634 = DIRECTION ( 'NONE',  ( -5.578564026256490882E-16, -1.000000000000000000, -9.066213480720158442E-32 ) ) ;
#81635 = CARTESIAN_POINT ( 'NONE',  ( 1.781981981289095796, -0.9795585948506604357, 1.540336029244721461 ) ) ;
#81636 = CARTESIAN_POINT ( 'NONE',  ( 2.426407915648312930, -1.496052118593782065, -1.352154011671408362 ) ) ;
#81637 = CARTESIAN_POINT ( 'NONE',  ( 1.640847625397081844, -1.850035366842089024, 1.174371965539475093 ) ) ;
#81638 = CARTESIAN_POINT ( 'NONE',  ( 9.634427881463707877, 13.63015724552533037, -8.222364378050974310 ) ) ;
#81639 = CARTESIAN_POINT ( 'NONE',  ( -7.562750758324527922, 7.717630727667075696, 1.040834085586084257E-14 ) ) ;
#81640 = CARTESIAN_POINT ( 'NONE',  ( 1.188034388246852480, -1.312013912954514971, -1.601590607232979524 ) ) ;
#81641 = CARTESIAN_POINT ( 'NONE',  ( 4.843287188579786573, 6.673587691474970107, -1.599625672291256295 ) ) ;
#81642 = CARTESIAN_POINT ( 'NONE',  ( 0.6801582343749674742, -0.2447916663252461267, 1.178068619123796568 ) ) ;
#81643 = CARTESIAN_POINT ( 'NONE',  ( 3.528090983593739516, -2.088826311502915090, 0.3641918842257965139 ) ) ;
#81644 = CARTESIAN_POINT ( 'NONE',  ( -1.402160292154681736E-14, 0.07187500034142156602, 1.575800808251672791 ) ) ;
#81645 = CARTESIAN_POINT ( 'NONE',  ( 6.516225534515442952, -0.8655890497146904172, -1.607451055071248636 ) ) ;
#81646 = ORIENTED_EDGE ( 'NONE', *, *, #111378, .F. ) ;
#81647 = CARTESIAN_POINT ( 'NONE',  ( -4.281342646865346602, 8.216926531310035031, 0.7998128361456352531 ) ) ;
#81648 = CARTESIAN_POINT ( 'NONE',  ( 10.42352117080803708, 11.05519620889787724, -0.7998128361456281477 ) ) ;
#81649 = CARTESIAN_POINT ( 'NONE',  ( 5.519577934094840543, 9.453608333170423705, 0.7216878364870317197 ) ) ;
#81650 = CARTESIAN_POINT ( 'NONE',  ( -1.737500000000000266, -2.464583332377416447, -3.009438278150923907 ) ) ;
#81651 = CARTESIAN_POINT ( 'NONE',  ( -5.032047568966410367, 9.022472597102808578, 1.214306433183764966E-14 ) ) ;
#81652 = CARTESIAN_POINT ( 'NONE',  ( 3.340107562988120726, -1.206563586372558561, -1.619613960689977761 ) ) ;
#81653 = CARTESIAN_POINT ( 'NONE',  ( 1.149603698739794400, -1.659950780972534012, -1.295870271070469260 ) ) ;
#81654 = CARTESIAN_POINT ( 'NONE',  ( -4.959250327548641479, 9.007818825440551791, -0.7998128361456362523 ) ) ;
#81655 = CARTESIAN_POINT ( 'NONE',  ( 9.023114925094663619, 10.48572115315399245, 1.199719254218453823 ) ) ;
#81656 = CARTESIAN_POINT ( 'NONE',  ( 5.576953945496859966, 1.718729505308995931, 0.7139912403442708611 ) ) ;
#81657 = CARTESIAN_POINT ( 'NONE',  ( 7.944187942603509356, 11.35563746875774882, 1.199719254218460707 ) ) ;
#81658 = EDGE_CURVE ( 'NONE', #115330, #70402, #77792, .T. ) ;
#81659 = DIRECTION ( 'NONE',  ( 0.1674078377056216482, 0.000000000000000000, 0.9858877298530133171 ) ) ;
#81660 = CARTESIAN_POINT ( 'NONE',  ( -3.578462479003122976, 6.262291094557191684, 1.199719254218464037 ) ) ;
#81661 = CARTESIAN_POINT ( 'NONE',  ( -5.506582945444718824, 9.576097202994168001, 0.7998128361456481317 ) ) ;
#81662 = CARTESIAN_POINT ( 'NONE',  ( 0.3566080023540801336, 0.8287714912002723811, 1.996717379258300840 ) ) ;
#81664 = CARTESIAN_POINT ( 'NONE',  ( -5.029856876702963220, 6.770753873564038017, 1.447965164949674310 ) ) ;
#81663 = CARTESIAN_POINT ( 'NONE',  ( -6.473091995881817162, 6.516638514809040217, 0.7998128361456281477 ) ) ;
#81665 = CARTESIAN_POINT ( 'NONE',  ( -1.402160292154681736E-14, 0.07187500034142156602, 1.575800808251672791 ) ) ;
#81666 = CARTESIAN_POINT ( 'NONE',  ( 2.336848640490073237, -1.070562806433389857, 1.363724479458855443 ) ) ;
#81667 = CARTESIAN_POINT ( 'NONE',  ( 1.815945235625218590, 1.623157326234461628, 0.6282625412417954802 ) ) ;
#81669 = CARTESIAN_POINT ( 'NONE',  ( 5.802526556968819804, 9.713438716531550554, -0.7216878364870267237 ) ) ;
#81668 = CARTESIAN_POINT ( 'NONE',  ( 0.1480895125635858234, -1.786911571543071675, -1.459641600669525197 ) ) ;
#81670 = CARTESIAN_POINT ( 'NONE',  ( -10.94029418865078362, 4.766281873824294024, -4.419956640179717233 ) ) ;
#81671 = CARTESIAN_POINT ( 'NONE',  ( 2.987629706096385895, 1.454891456164056462, 1.459756821352270473 ) ) ;
#81672 = CARTESIAN_POINT ( 'NONE',  ( 5.626797444871351139, 6.523350759560078593, 1.199719254218462483 ) ) ;
#81673 = CARTESIAN_POINT ( 'NONE',  ( 1.352888501574830205, -0.9090079681693465918, 1.799646022210943386 ) ) ;
#81674 = CARTESIAN_POINT ( 'NONE',  ( 6.825078400183574701, 2.043583509370741069, 2.350167621585138367 ) ) ;
#81675 = CARTESIAN_POINT ( 'NONE',  ( -6.231907884136888676, 7.299589282028351001, -1.199719254218453823 ) ) ;
#81676 = CARTESIAN_POINT ( 'NONE',  ( 1.270321628189803542, -1.252206795699914332, 1.522702518494284396 ) ) ;
#81679 = ADVANCED_FACE ( 'NONE', ( #21998 ), #175119, .T. ) ;
#81678 = CARTESIAN_POINT ( 'NONE',  ( -7.322812365156824654, 8.676274193172000437, 1.082531754730549078 ) ) ;
#81677 = CARTESIAN_POINT ( 'NONE',  ( 4.465046277278037934, -1.532637281380120564, 1.143568071694904598 ) ) ;
#81680 = CARTESIAN_POINT ( 'NONE',  ( 6.270183524512255246, 1.130759168108757873, 1.895055401287759178 ) ) ;
#81681 = CARTESIAN_POINT ( 'NONE',  ( -5.750066545527201534, 9.722511713174800008, 0.000000000000000000 ) ) ;
#81682 = CARTESIAN_POINT ( 'NONE',  ( 7.686546744304875389, 7.932335721302671949, 0.7998128361456291469 ) ) ;
#81683 = CARTESIAN_POINT ( 'NONE',  ( -3.160459205317013076, 6.701303149596211206, -0.7216878364870458196 ) ) ;
#81684 = CARTESIAN_POINT ( 'NONE',  ( 0.3463606850301796380, 1.036194208456611809, -1.733443346147050868 ) ) ;
#81685 = ORIENTED_EDGE ( 'NONE', *, *, #29276, .F. ) ;
#81686 = DIRECTION ( 'NONE',  ( -0.7592566023652990159, 0.6507913734559659380, -1.175982368226361624E-15 ) ) ;
#81687 = EDGE_CURVE ( 'NONE', #140589, #133576, #36353, .T. ) ;
#81688 = CARTESIAN_POINT ( 'NONE',  ( 4.665214083390394784, -2.058938813511351551, -1.042142520334616185 ) ) ;
#81689 = CARTESIAN_POINT ( 'NONE',  ( 5.266048140081638351, -1.952571265509401854, 0.1905133553196102503 ) ) ;
#81690 = CARTESIAN_POINT ( 'NONE',  ( 2.061309051315598051, 1.628117514333087934, 1.094105149622534467 ) ) ;
#81691 = CARTESIAN_POINT ( 'NONE',  ( 8.224992744984721327, 12.74757530245756243, 1.040834085586084257E-14 ) ) ;
#81692 = CARTESIAN_POINT ( 'NONE',  ( -0.1341500063891595818, -0.1486117279969369209, -1.983907055413631992 ) ) ;
#81693 = VERTEX_POINT ( 'NONE', #19886 ) ;
#81694 = CARTESIAN_POINT ( 'NONE',  ( 6.509000000000012776, 0.004788705324892602276, 2.000274819378269342 ) ) ;
#81695 =( BOUNDED_SURFACE ( )  B_SPLINE_SURFACE ( 3, 2, ( 
 ( #202551, #201484, #2211 ),
 ( #99750, #119259, #185245 ),
 ( #36867, #102951, #37952 ),
 ( #7559, #74717, #204686 ) ),
 .UNSPECIFIED., .F., .F., .F. ) 
 B_SPLINE_SURFACE_WITH_KNOTS ( ( 4, 4 ),
 ( 3, 3 ),
 ( 0.01133669335851671296, 0.01377857026255084431 ),
 ( 0.000000000000000000, 1.000000000000000000 ),
 .UNSPECIFIED. ) 
 GEOMETRIC_REPRESENTATION_ITEM ( )  RATIONAL_B_SPLINE_SURFACE ( (
 ( 1.000000000000000000, 0.7169883299103946284, 1.000000000000000000),
 ( 1.000000000000000000, 0.7174882367753905310, 1.000000000000000000),
 ( 1.000000000000000000, 0.7180609655871069696, 1.000000000000000000),
 ( 1.000000000000000000, 0.7187540731122941118, 1.000000000000000000) ) ) 
 REPRESENTATION_ITEM ( '' )  SURFACE ( )  );
#81697 = CARTESIAN_POINT ( 'NONE',  ( -8.128276786592724790, 9.441743324901704426, -1.199719254218446718 ) ) ;
#81696 = CARTESIAN_POINT ( 'NONE',  ( -4.062639585589296942, 7.891496616496157301, 0.7998128361456341429 ) ) ;
#81698 = CARTESIAN_POINT ( 'NONE',  ( 0.7086343398283838635, -0.2726298849291541870, 1.820711063333625646 ) ) ;
#81699 = ORIENTED_EDGE ( 'NONE', *, *, #32385, .F. ) ;
#81701 = COLOUR_RGB ( '', 0.08235294, 0.09019608, 0.10196078) ;
#81700 = CARTESIAN_POINT ( 'NONE',  ( 3.713894982949633050, 0.5324762967815239723, -2.104625409411722270 ) ) ;
#81702 = CARTESIAN_POINT ( 'NONE',  ( -0.3979845002021665801, 2.888372890405577209, 2.025450573642260554 ) ) ;
#81703 = CARTESIAN_POINT ( 'NONE',  ( 2.338272602237463360, -1.224740070204191289, -1.730971256048131401 ) ) ;
#81704 = B_SPLINE_CURVE_WITH_KNOTS ( 'NONE', 3,
 ( #202292, #181781, #199087, #102695 ),
 .UNSPECIFIED., .F., .F.,
 ( 4, 4 ),
 ( 0.000000000000000000, 0.002006560693247981270 ),
 .UNSPECIFIED. ) ;
#81705 = CARTESIAN_POINT ( 'NONE',  ( -1.500000000000013101, 2.702083334016155636, 0.8660254037844403729 ) ) ;
#81706 = CARTESIAN_POINT ( 'NONE',  ( 8.215351014876830504, 11.67199438640995801, -1.199719254218446718 ) ) ;
#81707 = CARTESIAN_POINT ( 'NONE',  ( -1.837596251593757390, 2.507245085144842012, -2.496647680644803025 ) ) ;
#81708 = CARTESIAN_POINT ( 'NONE',  ( 6.606300428615679898, 6.765996464729716386, -0.04887194053871009303 ) ) ;
#81709 = CARTESIAN_POINT ( 'NONE',  ( 2.354824746187761164, -1.594966302183076667, 1.304983254080711808 ) ) ;
#81711 = CARTESIAN_POINT ( 'NONE',  ( 1.499999999999990896, 4.775000000000022560, 1.214306433183764966E-14 ) ) ;
#81710 = CARTESIAN_POINT ( 'NONE',  ( -9.515124878692420296, 9.995400534762978850, 1.040834085586084257E-14 ) ) ;
#81712 = CARTESIAN_POINT ( 'NONE',  ( 1.364683531249988535, 3.113541667008083991, 0.7879004041258500513 ) ) ;
#81713 = CARTESIAN_POINT ( 'NONE',  ( -0.02264175331117677936, 7.629137130509094256, -2.689100833419917347 ) ) ;
#81714 = CARTESIAN_POINT ( 'NONE',  ( -6.520158902582637417, 5.290451655907114414, 2.438235897557452958 ) ) ;
#81715 = CARTESIAN_POINT ( 'NONE',  ( 5.426388453851806126, -0.8635988772061551355, -1.706256623820540108 ) ) ;
#81716 = CARTESIAN_POINT ( 'NONE',  ( 11.81900460097218186, 9.842428651258618544, -1.592493057836596337 ) ) ;
#81717 = CARTESIAN_POINT ( 'NONE',  ( 1.722331603166191050, -1.256259422768091216, -1.881381621351454037 ) ) ;
#81718 = CARTESIAN_POINT ( 'NONE',  ( -8.676855123066012254, 12.10645282934361866, -1.082531754730543971 ) ) ;
#81719 = CARTESIAN_POINT ( 'NONE',  ( 1.406221933027915982, -1.803026290124358555, -0.1754379831288860880 ) ) ;
#81720 = CARTESIAN_POINT ( 'NONE',  ( 2.465921856196826134, -0.9807800477944830231, 1.645437157327357180 ) ) ;
#81721 = CARTESIAN_POINT ( 'NONE',  ( 3.209495720308676248, -1.691010085789945716, -1.194244797349801157 ) ) ;
#81722 = CARTESIAN_POINT ( 'NONE',  ( -1.364683531250014514, 1.551041667008084435, -0.7879004041258289570 ) ) ;
#81723 = CARTESIAN_POINT ( 'NONE',  ( 1.182427310604698079, -1.922956083944601158, -0.4339701177692931178 ) ) ;
#81724 = CARTESIAN_POINT ( 'NONE',  ( 5.760362637647353345, 0.7829873311157690141, 1.760386188003287611 ) ) ;
#81726 = CARTESIAN_POINT ( 'NONE',  ( 6.492781079782697695, 6.747302000852300807, 0.03582484399037785816 ) ) ;
#81725 = CARTESIAN_POINT ( 'NONE',  ( 0.7159568421808035765, -0.3331041906398305441, 2.283425790780469811 ) ) ;
#81727 = CARTESIAN_POINT ( 'NONE',  ( -1.201851678989727383E-14, 2.571875000341417472, 1.575800808251672791 ) ) ;
#81728 = AXIS2_PLACEMENT_3D ( 'NONE', #79351, #15391, #145468 ) ;
#81729 = CARTESIAN_POINT ( 'NONE',  ( 5.195784910611107144, -1.456250996468626768, -1.461061404345398440 ) ) ;
#81730 = CARTESIAN_POINT ( 'NONE',  ( -4.401593425930945713, 8.286942763561420122, 1.040834085586084257E-14 ) ) ;
#81731 = CARTESIAN_POINT ( 'NONE',  ( 8.260995669428309540, 8.532249790621511565, 0.7998128361456481317 ) ) ;
#81732 = CARTESIAN_POINT ( 'NONE',  ( 1.000000000000001554, 5.868705557303652398, -4.125226524755055024 ) ) ;
#81734 = CARTESIAN_POINT ( 'NONE',  ( 0.7499999999999920064, 4.483333333333352932, 1.299038105676669330 ) ) ;
#81733 = CARTESIAN_POINT ( 'NONE',  ( 6.774446309029529267, -1.298820955785205955, 1.658247839749617869 ) ) ;
#81735 = AXIS2_PLACEMENT_3D ( 'NONE', #51232, #50165, #135690 ) ;
#81736 = CARTESIAN_POINT ( 'NONE',  ( -0.6823417656250003738, 2.780208333674753618, -1.181850606188749264 ) ) ;
#81737 = CARTESIAN_POINT ( 'NONE',  ( 5.325516461952284786, -2.054413220456321909, 0.6725034809518318779 ) ) ;
#81738 = CARTESIAN_POINT ( 'NONE',  ( 5.918619479961092722, -0.7289874232782632690, -1.883701229315833059 ) ) ;
#81739 = DIRECTION ( 'NONE',  ( 1.000000000000000000, -0.000000000000000000, -0.000000000000000000 ) ) ;
#81740 = CARTESIAN_POINT ( 'NONE',  ( -5.748293942514189681, 5.808690475795744490, -0.7216878364870207285 ) ) ;
#81743 = CARTESIAN_POINT ( 'NONE',  ( 3.863710590214593399, 7.451486755318259547, 1.040834085586084257E-14 ) ) ;
#81742 = CARTESIAN_POINT ( 'NONE',  ( -3.285556943749998737, -1.130208332855377140, 1.896917185911908499 ) ) ;
#81741 = CARTESIAN_POINT ( 'NONE',  ( 5.677832469072920496, 9.846164657218904992, 0.000000000000000000 ) ) ;
#81744 = CARTESIAN_POINT ( 'NONE',  ( -3.969505113751027547, 7.853116076009993840, 1.214306433183764966E-14 ) ) ;
#81745 = CARTESIAN_POINT ( 'NONE',  ( 3.520720487665735643, 0.3006478860226591276, 1.993893439002386581 ) ) ;
#81746 = CARTESIAN_POINT ( 'NONE',  ( -6.503107236049161521, 10.73870887536603291, 0.7998128361456481317 ) ) ;
#81747 = CARTESIAN_POINT ( 'NONE',  ( -2.764973262183167968, 5.313220341600567664, 1.199719254218462483 ) ) ;
#81748 = EDGE_CURVE ( 'NONE', #61771, #197229, #15629, .T. ) ;
#81749 = CARTESIAN_POINT ( 'NONE',  ( 1.364683531249988535, 5.155208333674749177, -0.7879004041258300672 ) ) ;
#81751 = CARTESIAN_POINT ( 'NONE',  ( -8.012344526598182026E-15, 8.796875000341403350, -1.575800808251669460 ) ) ;
#81750 = CARTESIAN_POINT ( 'NONE',  ( 5.137646372127643524, -1.526005641499485810, -1.531359247741073570 ) ) ;
#81752 = DIRECTION ( 'NONE',  ( -3.347138415753902517E-16, -0.6000000000000018652, -0.7999999999999984901 ) ) ;
#81753 = CARTESIAN_POINT ( 'NONE',  ( -11.73415479055029209, 7.419463409362142770, -2.523393346103949053 ) ) ;
#81755 = CARTESIAN_POINT ( 'NONE',  ( 5.237907724141787291, 2.013986247903374327, -0.1017665992488273330 ) ) ;
#81754 = CARTESIAN_POINT ( 'NONE',  ( -6.765155463094763455, 8.915767345075790828, 1.443375672974078761 ) ) ;
#81756 = CARTESIAN_POINT ( 'NONE',  ( -0.6823417656250246877, -0.6364583329919113464, 1.181850606188755259 ) ) ;
#81757 = CARTESIAN_POINT ( 'NONE',  ( 0.7501351305400367764, 0.4964161116564491660, 1.651887862327553691 ) ) ;
#81758 = CARTESIAN_POINT ( 'NONE',  ( 4.278479993564246797, 7.149254538203735798, 1.199719254218452047 ) ) ;
#81760 = CARTESIAN_POINT ( 'NONE',  ( 7.343676480457483002, 8.596652644402405841, -1.199719254218452047 ) ) ;
#81759 = CARTESIAN_POINT ( 'NONE',  ( 6.914295153289432783, 10.05013286460426691, -1.082531754730537976 ) ) ;
#81761 = CARTESIAN_POINT ( 'NONE',  ( -11.37622529897019952, 7.826419360496526423, -3.683600133736221416 ) ) ;
#81762 = CARTESIAN_POINT ( 'NONE',  ( 6.292256349370360269, -1.861554482619768525, -0.1834065582871149958 ) ) ;
#81763 = CARTESIAN_POINT ( 'NONE',  ( 1.365886254406587064, 0.5821385057369383720, -1.927099543440218499 ) ) ;
#81764 = FACE_OUTER_BOUND ( 'NONE', #35165, .T. ) ;
#81766 =( GEOMETRIC_REPRESENTATION_CONTEXT ( 3 ) GLOBAL_UNCERTAINTY_ASSIGNED_CONTEXT ( ( #181028 ) ) GLOBAL_UNIT_ASSIGNED_CONTEXT ( ( #179827, #112759, #195002 ) ) REPRESENTATION_CONTEXT ( 'NONE', 'WORKASPACE' ) );
#81765 = CARTESIAN_POINT ( 'NONE',  ( 3.469938103458301892, 2.153457811087633011, -0.4814610123115290463 ) ) ;
#81767 = CARTESIAN_POINT ( 'NONE',  ( -6.034787771414192648, 9.094317262408276648, 1.082531754730549967 ) ) ;
#81768 = ORIENTED_EDGE ( 'NONE', *, *, #139653, .F. ) ;
#81769 = CARTESIAN_POINT ( 'NONE',  ( 9.097157884645296733, 10.67606762258344055, -1.082531754730543083 ) ) ;
#81771 = CARTESIAN_POINT ( 'NONE',  ( 1.757435634535610136, 1.928746520693159550, -0.5880414618760835266 ) ) ;
#81770 = CARTESIAN_POINT ( 'NONE',  ( 2.491022521637117570, -2.029929026191950481, -0.6131127883793398015 ) ) ;
#81773 = EDGE_LOOP ( 'NONE', ( #157483, #154545, #29394, #157806 ) ) ;
#81772 = CARTESIAN_POINT ( 'NONE',  ( 2.091809026493749890, 1.116998374171035424, 1.426102431979922702 ) ) ;
#81774 = CARTESIAN_POINT ( 'NONE',  ( 5.664274315459256748, 9.830346811336296398, -0.7998128361456481317 ) ) ;
#81775 =( GEOMETRIC_REPRESENTATION_CONTEXT ( 3 ) GLOBAL_UNCERTAINTY_ASSIGNED_CONTEXT ( ( #53163 ) ) GLOBAL_UNIT_ASSIGNED_CONTEXT ( ( #207917, #194875, #162395 ) ) REPRESENTATION_CONTEXT ( 'NONE', 'WORKASPACE' ) );
#81776 = CARTESIAN_POINT ( 'NONE',  ( 7.311924916471702396, 7.425000578838787391, -0.7998128361456281477 ) ) ;
#81778 = CARTESIAN_POINT ( 'NONE',  ( -0.2353475280464593089, -0.1482846297235005661, -1.883952934485186415 ) ) ;
#81777 = CARTESIAN_POINT ( 'NONE',  ( -4.253507506385335368, 5.985511395581417204, 1.599625672291267398 ) ) ;
#81779 = CARTESIAN_POINT ( 'NONE',  ( -0.7500000000000215383, 3.441666666666689967, 1.299038105676671107 ) ) ;
#81780 = CARTESIAN_POINT ( 'NONE',  ( -2.324088772396477673E-16, 1.562500000000000666, 1.224999999999980549 ) ) ;
#81781 = CARTESIAN_POINT ( 'NONE',  ( 5.138177029454841893, 7.017625839162543677, 1.443375672974062551 ) ) ;
#81782 = CARTESIAN_POINT ( 'NONE',  ( 0.6823417656249882723, 0.4052083336747516751, 1.181850606188755259 ) ) ;
#81783 = CARTESIAN_POINT ( 'NONE',  ( 2.550000000000000266, 2.499999999999998668, -1.849324200890695824 ) ) ;
#81784 = CARTESIAN_POINT ( 'NONE',  ( -10.45741655484220267, 11.09474082360439873, -0.7998128361456221525 ) ) ;
#81785 = AXIS2_PLACEMENT_3D ( 'NONE', #127533, #94960, #93901 ) ;
#81786 = CARTESIAN_POINT ( 'NONE',  ( 4.118171802502921253, -1.108985364570359566, -1.855417305202881506 ) ) ;
#81787 = CARTESIAN_POINT ( 'NONE',  ( -5.966997003790228682, 8.054858819212300958, -1.443375672974066548 ) ) ;
#81788 = CARTESIAN_POINT ( 'NONE',  ( 5.899206235721897507, 6.055031161196562373, 0.000000000000000000 ) ) ;
#81789 = CARTESIAN_POINT ( 'NONE',  ( 1.371502371489873751, -1.821557607348308405, -1.085495857948336251 ) ) ;
#81790 = CARTESIAN_POINT ( 'NONE',  ( 4.177814833343409084, 3.976464848429826393, 1.040551764647542070E-14 ) ) ;
#81791 = CARTESIAN_POINT ( 'NONE',  ( 3.321511454083085457, -1.900871985879136528, 0.5222822307265824193 ) ) ;
#81792 = CARTESIAN_POINT ( 'NONE',  ( 5.607647405131535479, 1.452367144367059826, 1.244281684088064166 ) ) ;
#81793 = VERTEX_POINT ( 'NONE', #3615 ) ;
#81794 = CARTESIAN_POINT ( 'NONE',  ( -0.7499999999999972244, 4.608333333333352932, -1.299038105676652011 ) ) ;
#81795 = CARTESIAN_POINT ( 'NONE',  ( 6.865690646733241032, -0.4297541067138924697, 1.928966555396218752 ) ) ;
#81796 = CARTESIAN_POINT ( 'NONE',  ( 1.886567394283003907, 1.689560458097194795, -0.9572515956587694941 ) ) ;
#81797 = VERTEX_POINT ( 'NONE', #1485 ) ;
#81798 = CARTESIAN_POINT ( 'NONE',  ( -4.995253251992230581, 4.792493313604505367, 0.000000000000000000 ) ) ;
#81800 = CARTESIAN_POINT ( 'NONE',  ( -2.303929616531696922E-15, -8.198316280121936472, 9.513083155459831630 ) ) ;
#81799 = CARTESIAN_POINT ( 'NONE',  ( -5.628043163448566588, 9.580151100749725757, 0.000000000000000000 ) ) ;
#81802 = CARTESIAN_POINT ( 'NONE',  ( 6.120616281565444794, 9.228137197546649517, -1.199719254218440723 ) ) ;
#81801 = CARTESIAN_POINT ( 'NONE',  ( 2.695356974763486679, -0.6552250210129506591, 1.985377264055338209 ) ) ;
#81804 = CARTESIAN_POINT ( 'NONE',  ( 4.516274566683592617, 8.283087737857252719, -0.7216878364870357165 ) ) ;
#81803 = CARTESIAN_POINT ( 'NONE',  ( 5.798083248138522272, 9.916180889470295412, 0.7998128361456462443 ) ) ;
#81806 = ORIENTED_EDGE ( 'NONE', *, *, #85855, .T. ) ;
#81805 = CARTESIAN_POINT ( 'NONE',  ( 5.637344576021464881, -0.04253375892994575719, 1.911971901805488816 ) ) ;
#81807 = CARTESIAN_POINT ( 'NONE',  ( 4.776106669258010307, 1.268914099295117781, 1.805409367619143390 ) ) ;
#81808 = EDGE_CURVE ( 'NONE', #113990, #82462, #173350, .T. ) ;
#81809 = CARTESIAN_POINT ( 'NONE',  ( 1.659489206604364941, -1.893029981318217647, -1.133929415002648655 ) ) ;
#81810 = CARTESIAN_POINT ( 'NONE',  ( 1.119614361207950548, -0.4638517909370845071, 1.855054000551699778 ) ) ;
#81811 = CARTESIAN_POINT ( 'NONE',  ( -2.285154342840974184, 5.536993397787091098, 0.3900462783498563901 ) ) ;
#81812 = CARTESIAN_POINT ( 'NONE',  ( -1.500000000000022204, 6.280000000000042881, 2.580000000000011173 ) ) ;
#81813 = CARTESIAN_POINT ( 'NONE',  ( 4.229010956685672618, -1.930657356216297860, -0.7480826485904976675 ) ) ;
#81815 = CARTESIAN_POINT ( 'NONE',  ( 1.657319961134783748, -1.854130675604428902, -1.111159678259740602 ) ) ;
#81814 = CARTESIAN_POINT ( 'NONE',  ( -2.442440228756222353, 6.001264033524212671, -0.7998128361456281477 ) ) ;
#81816 = CARTESIAN_POINT ( 'NONE',  ( 4.195009555701286530, 1.760677850468267414, 1.304791629949946019 ) ) ;
#81817 = DIRECTION ( 'NONE',  ( 1.000000000000000000, 0.000000000000000000, 0.000000000000000000 ) ) ;
#81818 = EDGE_CURVE ( 'NONE', #81410, #187130, #67550, .T. ) ;
#81819 = PLANE ( 'NONE',  #193876 ) ;
#81820 = CARTESIAN_POINT ( 'NONE',  ( -3.449547071718257030, -1.000000000000000888, 2.025000000000002576 ) ) ;
#81821 = CARTESIAN_POINT ( 'NONE',  ( -1.364683531250000748, 14.67187500034139447, 0.000000000000000000 ) ) ;
#81822 = CARTESIAN_POINT ( 'NONE',  ( -4.655245641445871385, 6.524482229810530498, 1.599625672291263179 ) ) ;
#81823 = ADVANCED_FACE ( 'NONE', ( #5747 ), #14911, .T. ) ;
#81824 = CARTESIAN_POINT ( 'NONE',  ( -0.1224325501351306023, -0.4448023855274513272, -1.973852191825019364 ) ) ;
#81825 = CARTESIAN_POINT ( 'NONE',  ( -9.083599731475995753, 11.62061899152058686, 1.443375672974064550 ) ) ;
#81826 = CARTESIAN_POINT ( 'NONE',  ( 4.733297664174529906, 0.005294743050891088411, -2.070434559870132585 ) ) ;
#81827 = CARTESIAN_POINT ( 'NONE',  ( 6.151990787553828888, 1.088749021807510431, 1.815729776765177661 ) ) ;
#81828 = CARTESIAN_POINT ( 'NONE',  ( 5.099838337034727331, 9.101561826515851550, -0.7998128361456281477 ) ) ;
#81829 = CARTESIAN_POINT ( 'NONE',  ( 4.647606103345025552, 8.407977806742819027, 0.6343139517084724899 ) ) ;
#81830 = CARTESIAN_POINT ( 'NONE',  ( 3.784006971647640327, -1.169605039944806357, -1.584395421511639812 ) ) ;
#81831 = CARTESIAN_POINT ( 'NONE',  ( 5.947306879541199187, 0.6707566017311801243, -2.191947003353618584 ) ) ;
#81832 = CARTESIAN_POINT ( 'NONE',  ( 3.756323439517950558, 0.6585720284536450420, 1.702948436616057881 ) ) ;
#81833 = CARTESIAN_POINT ( 'NONE',  ( 4.634908411025333130, 6.500755460986618495, 1.599625672291268286 ) ) ;
#81834 = CARTESIAN_POINT ( 'NONE',  ( 5.639828713160493834, 5.682147708216442439, 1.040834085586084257E-14 ) ) ;
#81835 = CARTESIAN_POINT ( 'NONE',  ( -7.456058132872594335, 7.663432341298296535, 0.000000000000000000 ) ) ;
#81836 = CARTESIAN_POINT ( 'NONE',  ( 5.773793314573267388, 7.829454515125894964, 1.599625672291268286 ) ) ;
#81837 = ORIENTED_EDGE ( 'NONE', *, *, #87216, .F. ) ;
#81838 = CARTESIAN_POINT ( 'NONE',  ( 4.693612458567416823, 1.876924737948972188, -0.7285200738881071336 ) ) ;
#81839 = CARTESIAN_POINT ( 'NONE',  ( 6.346320258841911865, 0.3977546830747305528, -2.263887401186816639 ) ) ;
#81840 = CARTESIAN_POINT ( 'NONE',  ( 4.768382384511014038, -0.8351381170168621360, -1.775225883709200980 ) ) ;
#81841 = CARTESIAN_POINT ( 'NONE',  ( -7.379715684540041565, 7.504089808251839244, 1.040834085586084257E-14 ) ) ;
#81842 = VECTOR ( 'NONE', #139063, 1000.000000000000000 ) ;
#81843 = CARTESIAN_POINT ( 'NONE',  ( -5.284980951228653190, 5.060232619388524533, 0.000000000000000000 ) ) ;
#81844 = CARTESIAN_POINT ( 'NONE',  ( -7.765925996254661179, -5.615420858948581895, 7.710915694720366531 ) ) ;
#81845 = CARTESIAN_POINT ( 'NONE',  ( -6.310394152517827315, 6.326824364217716656, 0.7998128361456281477 ) ) ;
#81847 = CARTESIAN_POINT ( 'NONE',  ( 5.700005536890629720, -1.770032025875327042, 0.003423177859356376761 ) ) ;
#81846 = CARTESIAN_POINT ( 'NONE',  ( 0.5914941650546343688, -0.7489122546765265565, 1.952206342558031160 ) ) ;
#81848 = CARTESIAN_POINT ( 'NONE',  ( 11.00023563321887643, -5.575210796978345762, 0.04341786867414096363 ) ) ;
#81849 = CARTESIAN_POINT ( 'NONE',  ( 6.246037776718591061, 0.6113502166280659900, 1.843275756764614082 ) ) ;
#81850 = CARTESIAN_POINT ( 'NONE',  ( 2.045129345224237394, -1.761195505111545989, -1.303888621850733509 ) ) ;
#81851 = CARTESIAN_POINT ( 'NONE',  ( 1.118268200169919568, -0.04383651085794643132, 1.740047355671838547 ) ) ;
#81852 = CARTESIAN_POINT ( 'NONE',  ( 7.149227073107712549, 7.235186428247455837, -0.7998128361456281477 ) ) ;
#81853 = CARTESIAN_POINT ( 'NONE',  ( 0.2333690889706717397, 6.947499272388762748, -2.648434294982876303 ) ) ;
#81854 = CARTESIAN_POINT ( 'NONE',  ( 1.224769985559545304, -0.04580521419573525821, 1.724442238450181186 ) ) ;
#81855 = CARTESIAN_POINT ( 'NONE',  ( 1.189316404147572337, 1.662717542896676504, 1.427817766309902314 ) ) ;
#81856 = CARTESIAN_POINT ( 'NONE',  ( 3.598431038176507002, -2.204323482753521635, -0.1086902067785888437 ) ) ;
#81858 = CARTESIAN_POINT ( 'NONE',  ( 0.9190777403676134716, -1.573854924298900615, 1.495750265368815946 ) ) ;
#81857 = B_SPLINE_CURVE_WITH_KNOTS ( 'NONE', 3,
 ( #127528, #90689, #207603, #208661, #27798, #75485, #143733, #209726, #11540, #171919, #74425 ),
 .UNSPECIFIED., .F., .F.,
 ( 4, 1, 1, 1, 1, 1, 1, 1, 4 ),
 ( 0.000000000000000000, 0.2254179815473072723, 0.3971144120416517653, 0.5241699701252212629, 0.6156743509408303394, 0.6807935377546089351, 0.7289379548928518471, 0.7696256121123346006, 1.000000000000000000 ),
 .UNSPECIFIED. ) ;
#81859 = CARTESIAN_POINT ( 'NONE',  ( 0.3635304476994546952, 1.806310985241452949, -0.2645042207462811046 ) ) ;
#81860 = CARTESIAN_POINT ( 'NONE',  ( 2.220046512049120846, 0.9935532346000598425, -1.869724544471425665 ) ) ;
#81861 = CARTESIAN_POINT ( 'NONE',  ( 3.999292125906899198, 6.649295999324608353, 1.082531754730558626 ) ) ;
#81862 = ORIENTED_EDGE ( 'NONE', *, *, #69515, .T. ) ;
#81864 = CARTESIAN_POINT ( 'NONE',  ( 0.6823417656249882723, -0.3447916663252489911, 1.181850606188755259 ) ) ;
#81863 = CARTESIAN_POINT ( 'NONE',  ( 2.437429393347473994, -1.701094670537067755, -1.536833775788006173 ) ) ;
#81865 = CARTESIAN_POINT ( 'NONE',  ( 3.832150974156964818, 7.622593236491780999, 1.040834085586084257E-14 ) ) ;
#81866 = CARTESIAN_POINT ( 'NONE',  ( 4.934350062338543452, -1.187533444586796438, -1.877053939226761115 ) ) ;
#81867 = CARTESIAN_POINT ( 'NONE',  ( -6.046573322014817897, 9.998159942418544333, 0.7216878364870458196 ) ) ;
#81868 = CARTESIAN_POINT ( 'NONE',  ( -1.152833933277347844, 3.300000000000025135, -0.7331020405358537051 ) ) ;
#81869 = VECTOR ( 'NONE', #109423, 1000.000000000000000 ) ;
#81870 = CARTESIAN_POINT ( 'NONE',  ( 5.178851490740205676, 6.104710163027444736, 1.082531754730558626 ) ) ;
#81871 = CARTESIAN_POINT ( 'NONE',  ( -6.954969613686107444, 10.09758640173367894, 1.082531754730549967 ) ) ;
#81872 = CARTESIAN_POINT ( 'NONE',  ( 3.445180431648313224, 7.033477913649446300, 0.7216878364870257245 ) ) ;
#81874 = ORIENTED_EDGE ( 'NONE', *, *, #112471, .T. ) ;
#81873 =( GEOMETRIC_REPRESENTATION_CONTEXT ( 3 ) GLOBAL_UNCERTAINTY_ASSIGNED_CONTEXT ( ( #100553 ) ) GLOBAL_UNIT_ASSIGNED_CONTEXT ( ( #108866, #24318, #11281 ) ) REPRESENTATION_CONTEXT ( 'NONE', 'WORKASPACE' ) );
#81875 = CARTESIAN_POINT ( 'NONE',  ( 3.217422812353257555, 1.967887761762876941, 0.4390297752325384995 ) ) ;
#81877 = CARTESIAN_POINT ( 'NONE',  ( 0.8485701241471826917, -2.046539366587364572, -0.2563945212397024109 ) ) ;
#81876 = CARTESIAN_POINT ( 'NONE',  ( 5.615048174354031474, 9.702639970055050966, 0.7998128361456462443 ) ) ;
#81878 = CARTESIAN_POINT ( 'NONE',  ( 5.736508391913541338, 6.825586224388162648, -1.082531754730548412 ) ) ;
#81879 = B_SPLINE_CURVE_WITH_KNOTS ( 'NONE', 3,
 ( #172190, #108315, #155936, #139705, #207862, #92022 ),
 .UNSPECIFIED., .F., .F.,
 ( 4, 2, 4 ),
 ( 0.001496030744711065140, 0.002086206484339691788, 0.002676382223968318437 ),
 .UNSPECIFIED. ) ;
#81880 = CARTESIAN_POINT ( 'NONE',  ( -9.611344009005486910, -6.731960136058444455, 0.1523027874135076676 ) ) ;
#81881 = CARTESIAN_POINT ( 'NONE',  ( -1.364683531249997417, 3.509375000341423245, 1.214306433183764966E-14 ) ) ;
#81882 = CARTESIAN_POINT ( 'NONE',  ( 3.785266741157941262, 1.586943040539133154, 1.511552532079393885 ) ) ;
#81883 = CARTESIAN_POINT ( 'NONE',  ( 2.197888892816081796, 1.802417619043535701, 0.9041091288993635677 ) ) ;
#81884 = CARTESIAN_POINT ( 'NONE',  ( 1.417261839328866513, -1.023339270300478221, -1.530466495063505628 ) ) ;
#81885 = EDGE_CURVE ( 'NONE', #94238, #44666, #208659, .T. ) ;
#81886 = CARTESIAN_POINT ( 'NONE',  ( 6.421758314367153275, 10.64380180007036891, -0.7998128361456291469 ) ) ;
#81887 = CARTESIAN_POINT ( 'NONE',  ( 4.788025880137685597, -0.8597811773201522456, 1.610451283527076116 ) ) ;
#81888 = CARTESIAN_POINT ( 'NONE',  ( 6.100232455412330168, -0.2440331339308223768, 2.001510902166554473 ) ) ;
#81889 = CARTESIAN_POINT ( 'NONE',  ( -6.842061076390810292, 11.13415502243129218, 0.000000000000000000 ) ) ;
#81891 = CARTESIAN_POINT ( 'NONE',  ( -6.631873415740034083, 7.766215735565355160, 1.199719254218452047 ) ) ;
#81890 = CARTESIAN_POINT ( 'NONE',  ( 4.294006694993548479, -0.8693707907260415091, 2.089011835857216948 ) ) ;
#81892 = CARTESIAN_POINT ( 'NONE',  ( 1.313257463657933055, 1.858222661572891621, 0.9912184023134795741 ) ) ;
#81893 = CARTESIAN_POINT ( 'NONE',  ( -7.923814432544069142, 8.209148024248356990, 0.000000000000000000 ) ) ;
#81894 = CARTESIAN_POINT ( 'NONE',  ( 5.178213324540339002, -1.104578422852561914, -1.750899486206449751 ) ) ;
#81895 = CARTESIAN_POINT ( 'NONE',  ( 9.511208455186636712, 11.05516360492796935, 1.199719254218453823 ) ) ;
#81896 =( LENGTH_UNIT ( ) NAMED_UNIT ( * ) SI_UNIT ( .MILLI., .METRE. ) );
#81897 = CARTESIAN_POINT ( 'NONE',  ( -7.991641480251377772, 11.41099992934688956, 1.199719254218453823 ) ) ;
#81898 = UNCERTAINTY_MEASURE_WITH_UNIT (LENGTH_MEASURE( 1.000000000000000082E-05 ), #108750, 'distance_accuracy_value', 'NONE');
#81899 = CARTESIAN_POINT ( 'NONE',  ( 6.339319342841494453, 9.553567112360518365, -1.199719254218452047 ) ) ;
#81900 = CARTESIAN_POINT ( 'NONE',  ( 5.587453275722374713, 6.167276584799368244, -0.8733612469495740660 ) ) ;
#81901 = CARTESIAN_POINT ( 'NONE',  ( -4.776550190716183586, 4.467063398790632966, 1.214306433183764966E-14 ) ) ;
#81903 = CARTESIAN_POINT ( 'NONE',  ( 2.250487404410873804, 1.042729518208513007, -1.961448655418545739 ) ) ;
#81902 = CARTESIAN_POINT ( 'NONE',  ( 0.4223351350958382544, -2.109807164369668087, 0.2139620856976830743 ) ) ;
#81904 = CARTESIAN_POINT ( 'NONE',  ( -1.484314741415495353, 7.334687650741205545, 4.257443109328100661 ) ) ;
#81905 = CARTESIAN_POINT ( 'NONE',  ( -5.576146316970437944, 9.727530813099326323, 0.000000000000000000 ) ) ;
#81906 = CARTESIAN_POINT ( 'NONE',  ( 7.149227073107712549, 7.235186428247455837, -0.7998128361456281477 ) ) ;
#81907 = CARTESIAN_POINT ( 'NONE',  ( 3.613678190204441254, 0.4790664972640528152, -1.902336835828049244 ) ) ;
#81908 = CARTESIAN_POINT ( 'NONE',  ( 6.471319392424407901, 6.444294134116939077, 0.7998128361456341429 ) ) ;
#81909 = CARTESIAN_POINT ( 'NONE',  ( -4.018125071768071876, 7.621166010707856486, 0.1319346992594405132 ) ) ;
#81910 = CARTESIAN_POINT ( 'NONE',  ( 4.844340958784499662, 4.546152628203684820, 0.7998128361456341429 ) ) ;
#81911 = CARTESIAN_POINT ( 'NONE',  ( -6.455090533882213322, 6.703562842383589349, -0.7216878364870338292 ) ) ;
#81913 = CARTESIAN_POINT ( 'NONE',  ( -8.039621903223732602, 8.481906429956900695, 1.040834085586084257E-14 ) ) ;
#81912 = AXIS2_PLACEMENT_3D ( 'NONE', #127703, #60467, #175310 ) ;
#81914 = CARTESIAN_POINT ( 'NONE',  ( 2.566775492539817627, 0.7186216927172992541, 1.995234744298620910 ) ) ;
#81915 = CARTESIAN_POINT ( 'NONE',  ( -5.074494633264801990, 9.142270515442742607, 0.7998128361456291469 ) ) ;
#81916 = CARTESIAN_POINT ( 'NONE',  ( 5.863715402168388380, -0.4781514528688200483, 1.902565108626976809 ) ) ;
#81917 = CARTESIAN_POINT ( 'NONE',  ( 3.819328725847204620, -0.1613130240520690706, 2.155748724213396361 ) ) ;
#81918 = CARTESIAN_POINT ( 'NONE',  ( 2.471991059931688106, -1.762569054296094340, -0.5325411743367300943 ) ) ;
#81919 = CARTESIAN_POINT ( 'NONE',  ( -4.016961781477323079, 7.622873323794868483, 0.1115696107641880874 ) ) ;
#81920 = CARTESIAN_POINT ( 'NONE',  ( 0.6823417656249864960, -0.7614583329919113464, -1.181850606188749264 ) ) ;
#81921 = CARTESIAN_POINT ( 'NONE',  ( 4.575936575705426890, -1.688975870839603655, -0.4190883748532001629 ) ) ;
#81922 = CARTESIAN_POINT ( 'NONE',  ( 11.41381675112453387, 10.19999999999999929, -3.704697986577184299 ) ) ;
#81923 = CARTESIAN_POINT ( 'NONE',  ( 5.233084105194869551, 6.167981546557892436, -1.082531754730548412 ) ) ;
#81924 = CARTESIAN_POINT ( 'NONE',  ( 6.720655732516647163, 0.005566325962592238996, 1.826293863978686982 ) ) ;
#81925 = AXIS2_PLACEMENT_3D ( 'NONE', #75587, #63599, #44166 ) ;
#81926 = CARTESIAN_POINT ( 'NONE',  ( 1.657319961134783748, -1.854130675604428902, -1.111159678259740602 ) ) ;
#81927 = CARTESIAN_POINT ( 'NONE',  ( 4.692732413458527319, -1.238132498367884082, -1.591073831703953445 ) ) ;
#81928 = CARTESIAN_POINT ( 'NONE',  ( -9.124274191872636663, 11.66807252865000244, -1.443375672974058777 ) ) ;
#81929 = CARTESIAN_POINT ( 'NONE',  ( 1.674925575805393585, -2.052671086741376882, -0.6780288057936025847 ) ) ;
#81930 = CARTESIAN_POINT ( 'NONE',  ( 2.319545460040703500, -1.913138470506670075, 0.4751570986292509846 ) ) ;
#81931 = CARTESIAN_POINT ( 'NONE',  ( -6.529133882450190107, 6.806989898173073428, 0.6212416517149940143 ) ) ;
#81932 = CARTESIAN_POINT ( 'NONE',  ( 3.456523497251274168, -1.714022962016878759, -0.9130526778427237033 ) ) ;
#81936 = VERTEX_POINT ( 'NONE', #24149 ) ;
#81935 = EDGE_CURVE ( 'NONE', #132208, #142386, #115363, .T. ) ;
#81934 = CARTESIAN_POINT ( 'NONE',  ( -4.258669648468323743, 6.061810238003387141, 1.443375672974065660 ) ) ;
#81933 = CARTESIAN_POINT ( 'NONE',  ( -8.907343734053998929, 12.37535620882957588, 1.082531754730558626 ) ) ;
#81937 = CIRCLE ( 'NONE', #192614, 0.07999999999999946043 ) ;
#81938 = CARTESIAN_POINT ( 'NONE',  ( -6.257970421159510188, 9.458660037064859694, 1.199719254218452047 ) ) ;
#81939 = CARTESIAN_POINT ( 'NONE',  ( 5.598591087800349086, 5.496387455380669529, -0.7998128361456481317 ) ) ;
#81941 = ORIENTED_EDGE ( 'NONE', *, *, #46655, .T. ) ;
#81940 = CARTESIAN_POINT ( 'NONE',  ( -5.444481204339554736, 8.509589284108232121, 1.199719254218454489 ) ) ;
#81942 = CARTESIAN_POINT ( 'NONE',  ( -8.581948047326017459, 11.99572790764693409, 1.082531754730558626 ) ) ;
#81943 = EDGE_CURVE ( 'NONE', #8852, #14053, #189867, .T. ) ;
#81944 = CARTESIAN_POINT ( 'NONE',  ( 1.026743138268666922, 1.313310656681260680, -1.773271738842125300 ) ) ;
#81945 = CARTESIAN_POINT ( 'NONE',  ( -1.642778471874998480, -2.501041666188707158, 2.845375778867863303 ) ) ;
#81946 = CARTESIAN_POINT ( 'NONE',  ( 5.489096970993415425, 0.1405823987245969631, 1.956747174436481274 ) ) ;
#81947 = CARTESIAN_POINT ( 'NONE',  ( 3.854788253679425125, -1.977088355604763148, -0.7582873983895296321 ) ) ;
#81948 = CARTESIAN_POINT ( 'NONE',  ( 0.7499999999999902300, 2.514583334016148974, 1.299038105676669330 ) ) ;
#81949 = CARTESIAN_POINT ( 'NONE',  ( 0.1745949693968146810, 5.726316517925682525, -2.349368801211670021 ) ) ;
#81950 = CARTESIAN_POINT ( 'NONE',  ( 4.452959842461719830, 0.4008590389125502029, -1.796806262838637647 ) ) ;
#81951 = VERTEX_POINT ( 'NONE', #75058 ) ;
#81952 = CARTESIAN_POINT ( 'NONE',  ( -7.483210719738908168, 10.81783070874899799, 1.199719254218453823 ) ) ;
#81953 = CARTESIAN_POINT ( 'NONE',  ( 6.938893903907228378E-15, 10.64264068711930733, 1.214306433183764966E-14 ) ) ;
#81954 = CARTESIAN_POINT ( 'NONE',  ( 5.379186226027963258, -1.918017450862268714, -0.9047448674902383026 ) ) ;
#81955 = CARTESIAN_POINT ( 'NONE',  ( 7.135668919494039031, 7.219368582364847242, 1.040834085586084257E-14 ) ) ;
#81956 = ORIENTED_EDGE ( 'NONE', *, *, #37910, .F. ) ;
#81957 = CARTESIAN_POINT ( 'NONE',  ( 6.802032647988246694, -2.060431444914239130, 0.04577141437269586360 ) ) ;
#81960 = CARTESIAN_POINT ( 'NONE',  ( 3.368544699895597461, 0.04196216268675251326, -1.840931771443871101 ) ) ;
#81959 = CARTESIAN_POINT ( 'NONE',  ( 0.9415990247386073486, 1.246032235168346380, 1.382555731526733611 ) ) ;
#81958 = CARTESIAN_POINT ( 'NONE',  ( 9.499700864329909678, -7.154544010627095219, 0.07538891330675402680 ) ) ;
#81961 = CARTESIAN_POINT ( 'NONE',  ( 7.853197290813620945, 10.18514947741448573, 1.599625672291281386 ) ) ;
#81962 = CARTESIAN_POINT ( 'NONE',  ( -11.01272219801457375, 3.870433085555834651, 3.737564583532713591 ) ) ;
#81963 = CARTESIAN_POINT ( 'NONE',  ( -5.447343857640614573, 9.577261277214532242, -0.7998128361456362523 ) ) ;
#81964 = DIRECTION ( 'NONE',  ( -5.578564026256490882E-16, -1.000000000000000000, -9.066213480720158442E-32 ) ) ;
#81965 = CARTESIAN_POINT ( 'NONE',  ( 3.264504910713565078, 0.9923201075644829672, 1.971275125648555449 ) ) ;
#81966 = CARTESIAN_POINT ( 'NONE',  ( 5.167352989974902222, 0.2290589858122368538, -2.250810084452478765 ) ) ;
#81967 = CARTESIAN_POINT ( 'NONE',  ( -5.083944415444539899, 8.875092884753202682, 0.000000000000000000 ) ) ;
#81968 = CARTESIAN_POINT ( 'NONE',  ( 4.500164564109310206, -0.8477707339301239209, 1.600948808527142386 ) ) ;
#81969 = CARTESIAN_POINT ( 'NONE',  ( 5.507027455500737467, -0.04000985115821522470, 1.915467925163343965 ) ) ;
#81970 = CARTESIAN_POINT ( 'NONE',  ( 0.6823417656249917140, 4.905208333674755394, 1.181850606188765695 ) ) ;
#81971 = CARTESIAN_POINT ( 'NONE',  ( 5.735183426005796115, -1.690533149647139410, 0.8011652756413772947 ) ) ;
#81972 = CARTESIAN_POINT ( 'NONE',  ( 6.285601362909060796, -1.752004058920811902, 0.6281230767469258014 ) ) ;
#81973 = DIRECTION ( 'NONE',  ( 0.6507913734559640506, -0.7592566023653004592, 0.000000000000000000 ) ) ;
#81974 = EDGE_CURVE ( 'NONE', #14088, #154674, #64735, .T. ) ;
#81975 = CARTESIAN_POINT ( 'NONE',  ( 6.069200897874186040, 0.1259568369440123015, -1.765440829579780990 ) ) ;
#81976 = CARTESIAN_POINT ( 'NONE',  ( 1.692592581891849912, 1.490968054865527304, -1.357870634957742961 ) ) ;
#81978 = CARTESIAN_POINT ( 'NONE',  ( 2.561271001754578780, -1.832848164261296597, -1.037248627104673249 ) ) ;
#81977 = CARTESIAN_POINT ( 'NONE',  ( -8.618179199781044630, 13.20629283305325963, 0.7998128361456341429 ) ) ;
#81979 = CARTESIAN_POINT ( 'NONE',  ( 10.09812548408005384, 10.67556790771522124, -0.7998128361456281477 ) ) ;
#81981 = CARTESIAN_POINT ( 'NONE',  ( -8.208571938070008400, 11.66408546346865016, -1.199719254218446718 ) ) ;
#81980 = DIRECTION ( 'NONE',  ( 1.000000000000000000, -5.578564026256490882E-16, -5.570868214615546318E-48 ) ) ;
#81982 = CARTESIAN_POINT ( 'NONE',  ( 4.101444922696781070, 3.685019076479660427, 2.420000000000010587 ) ) ;
#81983 = CARTESIAN_POINT ( 'NONE',  ( 1.758075477673838982, 0.7690763710625804217, -1.867840884567156357 ) ) ;
#81984 = CARTESIAN_POINT ( 'NONE',  ( -1.402160292154681736E-14, 2.196875000341423689, -1.575800808251660134 ) ) ;
#81985 = CARTESIAN_POINT ( 'NONE',  ( 3.659811400685081040, 6.357198169852855685, -1.199719254218446718 ) ) ;
#81986 = CARTESIAN_POINT ( 'NONE',  ( 2.829541668879275829, -2.018026287816252040, 0.7751260729957698548 ) ) ;
#81987 = CARTESIAN_POINT ( 'NONE',  ( 6.620655732516645742, 3.706282450693793695, 2.340867613974298767 ) ) ;
#81990 =( LENGTH_UNIT ( ) NAMED_UNIT ( * ) SI_UNIT ( .MILLI., .METRE. ) );
#81989 = CARTESIAN_POINT ( 'NONE',  ( 11.96533679318060095, 9.847539888129947627, -0.9151144679398871551 ) ) ;
#81988 = CARTESIAN_POINT ( 'NONE',  ( 5.422335090822693715, 5.290755458906732933, 0.000000000000000000 ) ) ;
#81991 = CARTESIAN_POINT ( 'NONE',  ( 8.337901282279995385, 11.71100668175994386, -1.082531754730543083 ) ) ;
#81992 = CARTESIAN_POINT ( 'NONE',  ( 11.86145016429273369, 10.09412591486744226, -1.100000000000002087 ) ) ;
#81993 = CARTESIAN_POINT ( 'NONE',  ( -6.060131475628484310, 10.01397778830115470, 0.000000000000000000 ) ) ;
#81994 = CIRCLE ( 'NONE', #168578, 0.08000000000000025147 ) ;
#81995 = CARTESIAN_POINT ( 'NONE',  ( -1.364683531250000748, 0.2593750003414205252, 0.000000000000000000 ) ) ;
#81996 = CARTESIAN_POINT ( 'NONE',  ( 1.329895901633147748, 1.076045675571284166, -1.909117696414885934 ) ) ;
#81997 = CARTESIAN_POINT ( 'NONE',  ( 0.3088250840612624115, 7.211283896344578004, 2.083830622148073353 ) ) ;
#81998 = CARTESIAN_POINT ( 'NONE',  ( 0.9368240258568013568, 2.229511284875786536, 0.3842425355367936057 ) ) ;
#81999 = CARTESIAN_POINT ( 'NONE',  ( -8.076906825439122528, 10.44614393447756129, -1.599625672291263179 ) ) ;
#82000 = CARTESIAN_POINT ( 'NONE',  ( -2.440104460335327463, 5.790612937125752424, 1.040834085586084257E-14 ) ) ;
#82001 = CARTESIAN_POINT ( 'NONE',  ( -0.6823417656249969321, 3.530208333674754506, -1.181850606188749264 ) ) ;
#82002 = CARTESIAN_POINT ( 'NONE',  ( 4.716601407767927689, 8.224641112169805979, 0.6639617910879731522 ) ) ;
#82003 = CARTESIAN_POINT ( 'NONE',  ( -0.7500000000000179856, 11.29166666666666430, 1.299038105676658228 ) ) ;
#82004 = CARTESIAN_POINT ( 'NONE',  ( 8.000720045840086669, 8.506797273001177828, 0.7216878364870267237 ) ) ;
#82005 = CARTESIAN_POINT ( 'NONE',  ( 3.374023350818358580, -1.056766630983814625, 1.419390967538982418 ) ) ;
#82006 = CARTESIAN_POINT ( 'NONE',  ( 6.282275147445602670, -1.185768659569720329, 1.860957768143455038 ) ) ;
#82007 = CARTESIAN_POINT ( 'NONE',  ( -1.402160292154681736E-14, 9.921875000341401574, 1.575800808251682339 ) ) ;
#82008 = VERTEX_POINT ( 'NONE', #7902 ) ;
#82009 = CARTESIAN_POINT ( 'NONE',  ( -6.123442655227560927, 7.173046514967467147, 1.199719254218452047 ) ) ;
#82010 = CARTESIAN_POINT ( 'NONE',  ( 5.026970340808907700, -1.727993218758390404, 1.039010492973009514 ) ) ;
#82011 = ORIENTED_EDGE ( 'NONE', *, *, #56772, .F. ) ;
#82012 = B_SPLINE_CURVE_WITH_KNOTS ( 'NONE', 3,
 ( #160981, #29917, #12572, #78644, #13643, #47250, #144770, #46178, #210780, #194531 ),
 .UNSPECIFIED., .F., .F.,
 ( 4, 2, 2, 2, 4 ),
 ( 0.000000000000000000, 0.0002503535593264583385, 0.0005007071186529166770, 0.0007510606779793750154, 0.001001414237305833354 ),
 .UNSPECIFIED. ) ;
#82013 = CARTESIAN_POINT ( 'NONE',  ( 2.483090063216564669, 1.711211315118581711, -0.7561169667836544761 ) ) ;
#82014 = CARTESIAN_POINT ( 'NONE',  ( 2.799741537105740363, -1.531010120401912200, -1.393694001666223814 ) ) ;
#82015 = CARTESIAN_POINT ( 'NONE',  ( -7.227905289416804102, 8.565549271475310533, -1.082531754730549967 ) ) ;
#82016 = CARTESIAN_POINT ( 'NONE',  ( 1.828231037913151447, -0.9045423626323212396, -1.684975973026317408 ) ) ;
#82017 = CARTESIAN_POINT ( 'NONE',  ( -0.5998553420608248032, 3.416832205580481840, 0.2583637543479647691 ) ) ;
#82018 = AXIS2_PLACEMENT_3D ( 'NONE', #113421, #33157, #179427 ) ;
#82019 = CARTESIAN_POINT ( 'NONE',  ( -10.33433454857960321, 4.766519530047388820, -5.444264161973041638 ) ) ;
#82020 = CARTESIAN_POINT ( 'NONE',  ( -0.6823417656250212460, 4.863541667008086655, 1.181850606188767472 ) ) ;
#82021 = CARTESIAN_POINT ( 'NONE',  ( 0.9317291061951762376, -1.865162313430932750, 0.4216105838140621342 ) ) ;
#82022 = CARTESIAN_POINT ( 'NONE',  ( 2.822649888979886335, -1.354935067541668259, 1.419045635080482093 ) ) ;
#82023 = DIRECTION ( 'NONE',  ( 0.000000000000000000, 0.000000000000000000, -1.000000000000000000 ) ) ;
#82024 = CARTESIAN_POINT ( 'NONE',  ( -5.795184315198522285, 5.725746220678519904, -0.7998128361456362523 ) ) ;
#82026 = DIRECTION ( 'NONE',  ( -0.6507913734559640506, -0.7592566023653004592, 0.000000000000000000 ) ) ;
#82025 = CARTESIAN_POINT ( 'NONE',  ( 8.072990401933337168, 11.50590700464255356, -1.199719254218446718 ) ) ;
#82027 = CARTESIAN_POINT ( 'NONE',  ( 6.520779640719153392, 1.838571040693348646, 0.7116797190419403840 ) ) ;
#82028 = CARTESIAN_POINT ( 'NONE',  ( 0.6823417656249882723, 2.176041667008084435, -1.181850606188749264 ) ) ;
#82029 = CARTESIAN_POINT ( 'NONE',  ( 1.599859548348059324, 1.391279381849828800, 1.455310581225319311 ) ) ;
#82031 = CARTESIAN_POINT ( 'NONE',  ( 1.669685637109643794, 1.462710821638053105, 1.530943346549427320 ) ) ;
#82030 = CARTESIAN_POINT ( 'NONE',  ( -6.236387472606141458, 10.21960978477508952, -0.7216878364870278340 ) ) ;
#82032 = CARTESIAN_POINT ( 'NONE',  ( 8.776573235218648961, 13.27486625357122563, -8.183627694784485485 ) ) ;
#82033 = CARTESIAN_POINT ( 'NONE',  ( 3.613788337741298040, 0.5058112091442801272, -2.007490274132675445 ) ) ;
#82034 = CARTESIAN_POINT ( 'NONE',  ( 5.571474780572990504, 5.464751763615448787, 0.7998128361456352531 ) ) ;
#82036 = CARTESIAN_POINT ( 'NONE',  ( 5.030238685870051185, 5.827365540725222282, -1.199719254218452047 ) ) ;
#82035 = CARTESIAN_POINT ( 'NONE',  ( 5.964805764622640005, 0.1547682761293242837, -2.084958343724970131 ) ) ;
#82038 = ORIENTED_EDGE ( 'NONE', *, *, #57301, .F. ) ;
#82037 = CARTESIAN_POINT ( 'NONE',  ( 3.909063277197013520, 1.565549990038747952, 0.9388121169797561949 ) ) ;
#82039 = CARTESIAN_POINT ( 'NONE',  ( 10.56588178375152864, 11.22128359066528169, -0.7998128361456281477 ) ) ;
#82040 = LINE ( 'NONE', #31183, #88895 ) ;
#82041 = CARTESIAN_POINT ( 'NONE',  ( 9.312415520145556513, 13.13417835526394306, 6.702754826033684665 ) ) ;
#82042 = CARTESIAN_POINT ( 'NONE',  ( 5.104599427727727345, -0.7392731805347592111, -2.079399364341961487 ) ) ;
#82043 = CARTESIAN_POINT ( 'NONE',  ( -0.6823417656250003738, 10.96354166700806765, 1.181850606188754593 ) ) ;
#82044 = ORIENTED_EDGE ( 'NONE', *, *, #93974, .F. ) ;
#82045 = CARTESIAN_POINT ( 'NONE',  ( 3.527896108305649037, -1.883508717751972705, 0.3295761852530054159 ) ) ;
#82047 = CARTESIAN_POINT ( 'NONE',  ( -7.960608749518247151, 12.43912730774665576, 0.000000000000000000 ) ) ;
#82046 = CIRCLE ( 'NONE', #140866, 0.2000000000000000111 ) ;
#82048 = CARTESIAN_POINT ( 'NONE',  ( 6.958359152311676787, 9.141171649162195934, -1.599625672291262513 ) ) ;
#82049 = CARTESIAN_POINT ( 'NONE',  ( 0.6801582343749883464, 1.505208333674713739, 1.178068619123805227 ) ) ;
#82050 = CARTESIAN_POINT ( 'NONE',  ( 4.812781342726858647, 6.637997537979888563, 1.443375672974062551 ) ) ;
#82051 = CARTESIAN_POINT ( 'NONE',  ( 5.764883781430363285, 7.068005876895862016, -2.440105357730324886 ) ) ;
#82052 = CARTESIAN_POINT ( 'NONE',  ( 6.928203230275523872, 14.53091781611523814, -9.797958971132697314 ) ) ;
#82053 = CARTESIAN_POINT ( 'NONE',  ( 0.1867156058280825814, 1.363667594142993877, 1.237386390646778578 ) ) ;
#82054 = ORIENTED_EDGE ( 'NONE', *, *, #110293, .T. ) ;
#82056 = EDGE_CURVE ( 'NONE', #169163, #210464, #108555, .T. ) ;
#82055 = MECHANICAL_DESIGN_GEOMETRIC_PRESENTATION_REPRESENTATION (  '', ( #120187 ), #137447 ) ;
#82057 = CARTESIAN_POINT ( 'NONE',  ( -6.064239847062411926, 10.29697326487330500, 0.000000000000000000 ) ) ;
#82058 = CARTESIAN_POINT ( 'NONE',  ( 4.639837347815604751, 0.8015432297804045980, -1.690266223530467293 ) ) ;
#82059 = CARTESIAN_POINT ( 'NONE',  ( 1.499999999999996891, 10.89583333333333215, -0.8660254037844378194 ) ) ;
#82060 = CARTESIAN_POINT ( 'NONE',  ( 0.03257971700928394970, 14.52926532189213127, 11.98509109043141940 ) ) ;
#82061 = CARTESIAN_POINT ( 'NONE',  ( -7.375272376154101472, 7.706831981708990753, -0.7216878364870278340 ) ) ;
#82062 = CARTESIAN_POINT ( 'NONE',  ( 3.486418057008484617, 7.219238166485217434, 1.040834085586084257E-14 ) ) ;
#82063 = CARTESIAN_POINT ( 'NONE',  ( 1.498812192398508270, 0.3789717401675870567, 1.932455098789982895 ) ) ;
#82064 = CARTESIAN_POINT ( 'NONE',  ( 2.460564738353550496, -1.930424690641812768, -0.5826366834433827080 ) ) ;
#82065 = CARTESIAN_POINT ( 'NONE',  ( -9.481229494658258261, 9.955855920056455588, -0.7998128361456291469 ) ) ;
#82066 = CARTESIAN_POINT ( 'NONE',  ( 7.354371980770088690, 7.544798497178720531, 0.000000000000000000 ) ) ;
#82067 = PLANE ( 'NONE',  #59764 ) ;
#82068 = AXIS2_PLACEMENT_3D ( 'NONE', #121376, #187350, #203578 ) ;
#82069 = CARTESIAN_POINT ( 'NONE',  ( 2.695491272475036837, -0.6865090956127660737, 2.081212476921667776 ) ) ;
#82070 = CARTESIAN_POINT ( 'NONE',  ( -10.29471871147821282, 10.90492667301307605, -0.7998128361456291469 ) ) ;
#82071 = CARTESIAN_POINT ( 'NONE',  ( -1.201851678989727383E-14, 3.071875000341419248, 1.575800808251672791 ) ) ;
#82072 = CARTESIAN_POINT ( 'NONE',  ( -0.08058608058609216529, -8.407420853759283830, -10.99970480893080271 ) ) ;
#82073 = CARTESIAN_POINT ( 'NONE',  ( 5.153507786970260796, 7.105788066255672497, -1.443375672974078761 ) ) ;
#82074 = CARTESIAN_POINT ( 'NONE',  ( 8.772289083241844310, 10.19309100432570148, -1.199719254218446718 ) ) ;
#82075 = EDGE_CURVE ( 'NONE', #92250, #201176, #31400, .T. ) ;
#82076 = CARTESIAN_POINT ( 'NONE',  ( 6.590672070018850803, 7.822110515511036866, -1.082531754730548412 ) ) ;
#82077 = ORIENTED_EDGE ( 'NONE', *, *, #180435, .F. ) ;
#82079 = CARTESIAN_POINT ( 'NONE',  ( 1.418609115998151982, -0.7265329536030593616, -1.877579518606347531 ) ) ;
#82078 = CARTESIAN_POINT ( 'NONE',  ( 5.407694413872749628, -0.8332299576223768378, -1.642021276980778932 ) ) ;
#82080 = VERTEX_POINT ( 'NONE', #206109 ) ;
#82081 = CARTESIAN_POINT ( 'NONE',  ( 3.444923099841538772, 1.455166840473320233, 1.779090439993118888 ) ) ;
#82082 = CARTESIAN_POINT ( 'NONE',  ( 1.410758858885716061, -1.471193852737593843, 1.139540799010074323 ) ) ;
#82083 = CARTESIAN_POINT ( 'NONE',  ( -3.285556943750000514, -2.588541666188707513, -1.896917185911906500 ) ) ;
#82084 = CARTESIAN_POINT ( 'NONE',  ( -4.092446641025072829, 3.979529022206003575, 0.4031905389056175126 ) ) ;
#82085 = CARTESIAN_POINT ( 'NONE',  ( 5.801015586618943232, -0.2871438832755985326, -1.890612906794430614 ) ) ;
#82086 = CARTESIAN_POINT ( 'NONE',  ( -7.635213062790267458, 12.05949900656400686, 0.000000000000000000 ) ) ;
#82087 = CARTESIAN_POINT ( 'NONE',  ( -7.444835747679825033, 7.858265591814152629, 0.000000000000000000 ) ) ;
#82089 = CARTESIAN_POINT ( 'NONE',  ( 1.920565142479381038, 1.744437793965779582, 0.6759427408406930571 ) ) ;
#82088 = CARTESIAN_POINT ( 'NONE',  ( 4.036730150552261698, -1.818196258471163729, 1.032062162679239892 ) ) ;
#82090 = CARTESIAN_POINT ( 'NONE',  ( 6.968527767744098433, 9.153035033833367251, 1.443375672974076540 ) ) ;
#82091 = CARTESIAN_POINT ( 'NONE',  ( -0.6823417656249969321, 5.780208333674756283, -1.181850606188749264 ) ) ;
#82092 = CARTESIAN_POINT ( 'NONE',  ( 5.829618728418341611, 0.9018330327132916269, -1.605192750430362025 ) ) ;
#82093 = CARTESIAN_POINT ( 'NONE',  ( 3.334415713957098681, 5.977569868670206787, -1.199719254218446718 ) ) ;
#82094 = CARTESIAN_POINT ( 'NONE',  ( -7.245729715095584389, -5.507058666270985725, -7.863746947443975621 ) ) ;
#82095 = CARTESIAN_POINT ( 'NONE',  ( 5.109832884134172026, -1.716065896558026216, 0.1740927981267632318 ) ) ;
#82096 = CARTESIAN_POINT ( 'NONE',  ( -6.551614543901706611, 8.666636272683888365, 1.599625672291283607 ) ) ;
#82097 =( BOUNDED_CURVE ( )  B_SPLINE_CURVE ( 3, ( #142220, #156313, #188797, #72899 ),
 .UNSPECIFIED., .F., .T. ) 
 B_SPLINE_CURVE_WITH_KNOTS ( ( 4, 4 ),
 ( 0.000000000000000000, 0.5000000000000008882 ),
 .UNSPECIFIED. ) 
 CURVE ( )  GEOMETRIC_REPRESENTATION_ITEM ( )  RATIONAL_B_SPLINE_CURVE ( ( 1.000000000000000222, 0.3333333333333322601, 0.3333333333333334259, 1.000000000000001332 ) ) 
 REPRESENTATION_ITEM ( '' )  );
#82098 = CARTESIAN_POINT ( 'NONE',  ( 0.4571073982213811893, -1.631979074848688205, -0.5868837268243607408 ) ) ;
#82099 = PLANE ( 'NONE',  #123725 ) ;
#82100 = SURFACE_STYLE_FILL_AREA ( #81045 ) ;
#82101 = DIRECTION ( 'NONE',  ( 5.578564026256491869E-16, 1.000000000000000000, 9.066213480720160632E-32 ) ) ;
#82102 = CARTESIAN_POINT ( 'NONE',  ( 5.067309307786254102, 1.885564733447910646, 1.076134493607887155 ) ) ;
#82103 = CARTESIAN_POINT ( 'NONE',  ( 3.053144290054691901, -1.492835736363471888, -1.050712463094093385 ) ) ;
#82104 = CARTESIAN_POINT ( 'NONE',  ( 0.6198768371072010952, 1.941228818809427104, -0.2821078022595123747 ) ) ;
#82105 = CARTESIAN_POINT ( 'NONE',  ( 5.805892041792804825, -1.178307743425134335, -1.758994673012766574 ) ) ;
#82107 = CARTESIAN_POINT ( 'NONE',  ( 0.6823417656249917140, 3.405208333674754506, 1.181850606188765695 ) ) ;
#82106 = CARTESIAN_POINT ( 'NONE',  ( 5.601222333718593127, -0.5599829797399961118, 2.222829207915150374 ) ) ;
#82108 = CARTESIAN_POINT ( 'NONE',  ( 4.812781342726866640, 5.677628323678546529, 1.082531754730560403 ) ) ;
#82109 = CARTESIAN_POINT ( 'NONE',  ( 8.402302512167096893, 10.82577223566020841, -1.599625672291268286 ) ) ;
#82110 = CARTESIAN_POINT ( 'NONE',  ( 1.787894333202539654, 2.028250040683087008, -0.6185522307536188702 ) ) ;
#82111 = CARTESIAN_POINT ( 'NONE',  ( -3.416291520963659512, 5.969128626890772615, 1.082531754730560403 ) ) ;
#82112 = CARTESIAN_POINT ( 'NONE',  ( -3.811250579217344558, 5.539821323877241355, 0.000000000000000000 ) ) ;
#82113 = CARTESIAN_POINT ( 'NONE',  ( -5.056828107772866510, 5.962349549565537643, -1.082531754730543971 ) ) ;
#82114 = CARTESIAN_POINT ( 'NONE',  ( 6.702019227905350540, 0.8390156466466727192, -2.002601388009570549 ) ) ;
#82116 = CARTESIAN_POINT ( 'NONE',  ( 1.499999999999997113, 11.92708333401613174, -0.8660254037844378194 ) ) ;
#82115 = CARTESIAN_POINT ( 'NONE',  ( 6.983263157960365675, 7.629137130509066722, 2.753810918356710769 ) ) ;
#82118 = VERTEX_POINT ( 'NONE', #105450 ) ;
#82117 = CARTESIAN_POINT ( 'NONE',  ( 1.875925780897500950, 0.3759573520328520768, -2.189106109952672519 ) ) ;
#82119 = CARTESIAN_POINT ( 'NONE',  ( 5.783827325522512552, 1.646840809264274119, -1.163266671679111353 ) ) ;
#82121 = CARTESIAN_POINT ( 'NONE',  ( 5.453991371731997440, -0.7473993133914544895, 1.922551457666883401 ) ) ;
#82120 = CARTESIAN_POINT ( 'NONE',  ( 5.196852952739813070, 4.957416621151553571, -0.7998128361456221525 ) ) ;
#82123 = CARTESIAN_POINT ( 'NONE',  ( -1.737500000000000266, -3.908333333333333215, -3.009438278150923907 ) ) ;
#82122 = CARTESIAN_POINT ( 'NONE',  ( 4.960304097753311936, 6.880383762169266504, 1.599625672291268286 ) ) ;
#82124 = CARTESIAN_POINT ( 'NONE',  ( 6.008198349511364000, 7.038594824965278995, 1.199719254218453823 ) ) ;
#82125 = CARTESIAN_POINT ( 'NONE',  ( 1.642778471875000035, -2.763541666188709556, -2.845375778867859751 ) ) ;
#82126 = CARTESIAN_POINT ( 'NONE',  ( -4.903732577545095950, 4.837283930932079201, 0.1501914610188368471 ) ) ;
#82127 = CARTESIAN_POINT ( 'NONE',  ( 4.950658015114751009, -1.558304906039936988, -0.9804572199803849308 ) ) ;
#82128 = EDGE_CURVE ( 'NONE', #1110, #10129, #4701, .T. ) ;
#82129 = CARTESIAN_POINT ( 'NONE',  ( 4.924636110261782385, 6.768494766770632332, 1.599625672291267398 ) ) ;
#82130 = CARTESIAN_POINT ( 'NONE',  ( -4.942274067367465662, 4.660407921550463684, 0.1785095769484911221 ) ) ;
#82131 = CARTESIAN_POINT ( 'NONE',  ( 1.940065037515970037, 1.705369652917272383, 0.2570983470618106170 ) ) ;
#82132 = CARTESIAN_POINT ( 'NONE',  ( 0.3039231887648624619, -1.082844287645868375, -1.700959134490941160 ) ) ;
#82133 = CARTESIAN_POINT ( 'NONE',  ( 2.163060705912169812, 1.417378650759585357, 1.809622876518288681 ) ) ;
#82134 = CARTESIAN_POINT ( 'NONE',  ( -1.364683531250012516, 4.051041667008088432, -0.7879004041258300672 ) ) ;
#82135 = CARTESIAN_POINT ( 'NONE',  ( 1.581717252844972998, 2.090516975186909487, -0.8654489506779092789 ) ) ;
#82136 = CARTESIAN_POINT ( 'NONE',  ( 3.914754834457169874, 1.489469167258972382, -1.489228550157334574 ) ) ;
#82137 = CARTESIAN_POINT ( 'NONE',  ( -2.972980823146582186, 6.690504403638126263, 0.000000000000000000 ) ) ;
#82138 = CARTESIAN_POINT ( 'NONE',  ( 3.040057762974816224, 1.755912757559551007, 0.2203070401886226548 ) ) ;
#82139 = CARTESIAN_POINT ( 'NONE',  ( 6.972971076130050072, 7.029554431773520129, 1.040834085586084257E-14 ) ) ;
#82140 = CARTESIAN_POINT ( 'NONE',  ( 6.346625304528514810, 6.577020074804287297, 0.000000000000000000 ) ) ;
#82141 = CARTESIAN_POINT ( 'NONE',  ( -5.870844209917351009, 6.808071985447069707, -1.199719254218446718 ) ) ;
#82142 = UNCERTAINTY_MEASURE_WITH_UNIT (LENGTH_MEASURE( 1.000000000000000082E-05 ), #47430, 'distance_accuracy_value', 'NONE');
#82143 = CARTESIAN_POINT ( 'NONE',  ( 0.7499999999999885647, 2.066666666666688634, -1.299038105676652899 ) ) ;
#82144 = CARTESIAN_POINT ( 'NONE',  ( 4.816739660502834752, -0.7493216981008001820, -2.091313736985983773 ) ) ;
#82145 = CARTESIAN_POINT ( 'NONE',  ( 3.785266741157941262, 1.586943040539133154, 1.511552532079393885 ) ) ;
#82146 = CARTESIAN_POINT ( 'NONE',  ( -6.423865854776591000, 6.388931673527803667, 1.040834085586084257E-14 ) ) ;
#82147 = CARTESIAN_POINT ( 'NONE',  ( -4.065465959251405081, 5.836405933916976707, -1.599625672291271394 ) ) ;
#82148 = CARTESIAN_POINT ( 'NONE',  ( -2.113655003624821838, 5.617681270870908072, 1.040834085586084257E-14 ) ) ;
#82149 = CARTESIAN_POINT ( 'NONE',  ( -0.6823417656250212460, 3.301041667008085323, 1.181850606188767472 ) ) ;
#82150 = CARTESIAN_POINT ( 'NONE',  ( 6.890000000000047642, 4.686644152421160392, 2.842524626796953946 ) ) ;
#82151 = CARTESIAN_POINT ( 'NONE',  ( -3.958617665510272943, 6.601842462195195438, -1.082531754730549967 ) ) ;
#82152 = CARTESIAN_POINT ( 'NONE',  ( 5.678019686890188211, 2.088907387943875982, -0.3644037002746222664 ) ) ;
#82153 = CARTESIAN_POINT ( 'NONE',  ( -7.431277594066152403, 8.802816960232885179, -1.082531754730549967 ) ) ;
#82154 = ORIENTED_EDGE ( 'NONE', *, *, #204535, .T. ) ;
#82156 = CARTESIAN_POINT ( 'NONE',  ( 6.596550757224428629, -0.5713381284546023009, -2.084776384472402100 ) ) ;
#82155 = CARTESIAN_POINT ( 'NONE',  ( -3.499413046103020175, 7.096749297179887783, 0.7216878364870338292 ) ) ;
#82157 = CARTESIAN_POINT ( 'NONE',  ( 4.819033534653518025, 7.709623992816043270, -1.199719254218452047 ) ) ;
#82158 = CARTESIAN_POINT ( 'NONE',  ( 6.444863656277017405, -1.483217659742747996, -1.090817886357238198 ) ) ;
#82159 = CARTESIAN_POINT ( 'NONE',  ( 1.217358635584784965, 3.264784080462327154, -0.7749999999999840350 ) ) ;
#82160 = CARTESIAN_POINT ( 'NONE',  ( 0.6823417656249917140, 4.655208333674755394, 1.181850606188765695 ) ) ;
#82161 = CARTESIAN_POINT ( 'NONE',  ( 1.469815953039468326, -1.652492729624547962, -0.5465173985150991731 ) ) ;
#82162 = CARTESIAN_POINT ( 'NONE',  ( 4.518945272056516416, 4.166524327021037699, 0.7998128361456341429 ) ) ;
#82163 = CARTESIAN_POINT ( 'NONE',  ( -9.499606459999013097, -9.910930816046743530, 0.08647025586260563557 ) ) ;
#82164 = CARTESIAN_POINT ( 'NONE',  ( -1.402160292154681736E-14, 0.6343750003414162508, 1.575800808251672791 ) ) ;
#82165 = CARTESIAN_POINT ( 'NONE',  ( -4.255544820792433569, 7.363048058395826878, -0.9459158008643682169 ) ) ;
#82166 = CARTESIAN_POINT ( 'NONE',  ( 5.963787895669664607, 2.130530397400759668, -0.3648857593604309391 ) ) ;
#82167 = CARTESIAN_POINT ( 'NONE',  ( -5.122283107864663343, 4.870418468797203637, 0.000000000000000000 ) ) ;
#82168 = CARTESIAN_POINT ( 'NONE',  ( -4.880572110795192486, 8.637825195995631589, 1.214306433183764966E-14 ) ) ;
#82169 = AXIS2_PLACEMENT_3D ( 'NONE', #136132, #167550, #19151 ) ;
#82170 = CARTESIAN_POINT ( 'NONE',  ( 4.680646922328831394, -2.095996545452833981, -0.5284188670612932626 ) ) ;
#82172 = ORIENTED_EDGE ( 'NONE', *, *, #68597, .F. ) ;
#82171 = CARTESIAN_POINT ( 'NONE',  ( -3.688700311369816909, 6.461178242310183784, -1.199719254218450271 ) ) ;
#82173 = CARTESIAN_POINT ( 'NONE',  ( -0.6823417656250212460, 3.551041667008085323, 1.181850606188767472 ) ) ;
#82174 = CARTESIAN_POINT ( 'NONE',  ( 5.764905551123544747, -1.781034818069273884, -0.8454043039353341671 ) ) ;
#82175 = CARTESIAN_POINT ( 'NONE',  ( 4.710095198716817144, -1.340344737836828282, -1.099787012688882015 ) ) ;
#82177 = CARTESIAN_POINT ( 'NONE',  ( 1.892365914234435120, -0.5883382831698009685, -2.111031122750434808 ) ) ;
#82176 = CARTESIAN_POINT ( 'NONE',  ( 0.6801582343749674742, -0.4427083329919187515, -1.178068619123886718 ) ) ;
#82178 = CARTESIAN_POINT ( 'NONE',  ( 3.874305460179793048, 1.279221729648010175, 1.920377363040247420 ) ) ;
#82179 = CARTESIAN_POINT ( 'NONE',  ( 5.044241359090890775, 2.054987069614383266, 0.1556004420267612098 ) ) ;
#82180 = CARTESIAN_POINT ( 'NONE',  ( 0.09355730106928944467, -1.941490229121365374, -0.04880333718709597285 ) ) ;
#82182 = EDGE_CURVE ( 'NONE', #29604, #144257, #131917, .T. ) ;
#82181 = CARTESIAN_POINT ( 'NONE',  ( -5.544921637864820951, 9.412899644243539754, -0.7216878364870207285 ) ) ;
#82183 = CARTESIAN_POINT ( 'NONE',  ( -5.829079699232685208, 5.765290835385048496, 0.000000000000000000 ) ) ;
#82184 = CARTESIAN_POINT ( 'NONE',  ( -9.523271316415712562, 15.37774589682084247, 7.301265812912605568 ) ) ;
#82185 = CARTESIAN_POINT ( 'NONE',  ( 3.797228045176269440, -0.2112621354826669517, -2.110076569278092062 ) ) ;
#82186 = FACE_OUTER_BOUND ( 'NONE', #185021, .T. ) ;
#82187 = CARTESIAN_POINT ( 'NONE',  ( 1.125625214514534900, 0.3961039030971893471, 1.976955501819408711 ) ) ;
#82188 = CARTESIAN_POINT ( 'NONE',  ( -4.717874267431199087, 8.448011045404303587, 1.040834085586084257E-14 ) ) ;
#82189 = CARTESIAN_POINT ( 'NONE',  ( 4.067547972739316897, 0.2730280005818259137, -2.189760481282684967 ) ) ;
#82190 = FACE_OUTER_BOUND ( 'NONE', #10105, .T. ) ;
#82191 = CARTESIAN_POINT ( 'NONE',  ( -1.201851678989727383E-14, 4.868750000682822154, -1.732050807568863648 ) ) ;
#82192 = CARTESIAN_POINT ( 'NONE',  ( -6.050681693448748177, 10.28115541899069463, 0.7998128361456291469 ) ) ;
#82194 = CARTESIAN_POINT ( 'NONE',  ( 6.825078400183551608, 0.5660753733540256905, 2.196387875007102419 ) ) ;
#82193 = CARTESIAN_POINT ( 'NONE',  ( -4.818718062179155659, 8.223694781438435797, -0.9201054579500017594 ) ) ;
#82195 = DIRECTION ( 'NONE',  ( 0.6507913734559641616, -0.7592566023653004592, 0.000000000000000000 ) ) ;
#82196 = EDGE_LOOP ( 'NONE', ( #88741, #170770, #40429, #118480 ) ) ;
#82197 = CARTESIAN_POINT ( 'NONE',  ( 4.522374016017603360, 1.269557654445327532, -1.623317902228790910 ) ) ;
#82198 = CARTESIAN_POINT ( 'NONE',  ( -1.360316468750008667, 2.369791667008076974, -0.7853790794159001276 ) ) ;
#82199 = ADVANCED_FACE ( 'NONE', ( #171486 ), #25789, .F. ) ;
#82200 = CARTESIAN_POINT ( 'NONE',  ( -5.253948220495577637, 6.088359997788290734, 1.199719254218450271 ) ) ;
#82201 = CARTESIAN_POINT ( 'NONE',  ( 3.791669620513484773, 1.900943035724310448, -0.6826196560621737852 ) ) ;
#82202 = CARTESIAN_POINT ( 'NONE',  ( -0.7500000000000249800, -0.8083333333333136972, 1.299038105676659116 ) ) ;
#82203 = CARTESIAN_POINT ( 'NONE',  ( 4.383363735919856730, 4.008345868194933104, -0.7998128361456211532 ) ) ;
#82204 = CARTESIAN_POINT ( 'NONE',  ( 8.308449207076147758, 8.587612251210650527, -0.7998128361456281477 ) ) ;
#82205 = CARTESIAN_POINT ( 'NONE',  ( 2.659116476608857305, -1.792500920499852546, -1.016832356063899656 ) ) ;
#82206 = CARTESIAN_POINT ( 'NONE',  ( -9.495238110454899072, 14.82843120887656951, -7.231499654889533169 ) ) ;
#82207 = CARTESIAN_POINT ( 'NONE',  ( 5.626797444871351139, 6.523350759560078593, 1.199719254218462483 ) ) ;
#82208 = VECTOR ( 'NONE', #35574, 1000.000000000000114 ) ;
#82209 = CARTESIAN_POINT ( 'NONE',  ( -0.2408018239683913930, 0.6935112996086059134, -2.180753846165773169 ) ) ;
#82210 = CARTESIAN_POINT ( 'NONE',  ( 1.165666007907351309, -1.169451938622353859, 1.422036577929463030 ) ) ;
#82211 = CARTESIAN_POINT ( 'NONE',  ( 0.2765547061623524483, 1.334074794448695034, 1.882843260577294009 ) ) ;
#82212 = CARTESIAN_POINT ( 'NONE',  ( 5.580062740476173566, 8.667767742934335828, 1.199719254218451159 ) ) ;
#82213 = CARTESIAN_POINT ( 'NONE',  ( 1.722176697685766200, -1.199285583244277253, -1.798187405066300038 ) ) ;
#82214 = CARTESIAN_POINT ( 'NONE',  ( -3.145128448690317935, 5.652771709238564313, -1.082531754730549967 ) ) ;
#82215 = CARTESIAN_POINT ( 'NONE',  ( 2.378138974734815392, -2.011451771401792321, -0.1435188914247695346 ) ) ;
#82216 = AXIS2_PLACEMENT_3D ( 'NONE', #164603, #112729, #1002 ) ;
#82217 = CARTESIAN_POINT ( 'NONE',  ( 1.757567914286566335, -2.287329856776819881, -0.2253975434684113155 ) ) ;
#82218 = CARTESIAN_POINT ( 'NONE',  ( -4.702146809683723561, 5.356480858934594025, -2.500000000000000444 ) ) ;
#82219 = CARTESIAN_POINT ( 'NONE',  ( 0.3384655940862451029, 0.3152513238553408814, 1.843739016257638141 ) ) ;
#82220 = EDGE_CURVE ( 'NONE', #73245, #195702, #160571, .T. ) ;
#82221 = CARTESIAN_POINT ( 'NONE',  ( 4.627780688875618331, -1.211982541104269062, -1.554853849032981072 ) ) ;
#82222 = CARTESIAN_POINT ( 'NONE',  ( 4.188685576152741064, 1.555700494002542067, -1.282988152656767911 ) ) ;
#82224 = CARTESIAN_POINT ( 'NONE',  ( 8.500599125643985232, 11.90082083235127008, -1.082531754730543083 ) ) ;
#82223 = CARTESIAN_POINT ( 'NONE',  ( -1.402160292154681736E-14, 1.946875000341422579, -1.575800808251660134 ) ) ;
#82226 = CARTESIAN_POINT ( 'NONE',  ( 6.094376849853386346, -2.095768364502542003, -0.2079484218287275255 ) ) ;
#82225 = CARTESIAN_POINT ( 'NONE',  ( -7.039708073993679704, 9.236078724457858158, 1.599625672291283607 ) ) ;
#82227 = CARTESIAN_POINT ( 'NONE',  ( 5.266107318980479235, -2.060723932065291031, 0.1993833602659672022 ) ) ;
#82228 = CARTESIAN_POINT ( 'NONE',  ( 6.667912619822566000, 6.673652899414787676, 1.040834085586084257E-14 ) ) ;
#82229 = CARTESIAN_POINT ( 'NONE',  ( -6.413170354464012846, 7.440785820751486312, 1.199719254218450271 ) ) ;
#82230 = CARTESIAN_POINT ( 'NONE',  ( 6.539320575229223387, 6.036367980355456631, 2.598156967962389263 ) ) ;
#82231 = CARTESIAN_POINT ( 'NONE',  ( 5.765880396963712684, 0.5824918586248282182, -1.933996001582516611 ) ) ;
#82232 = CARTESIAN_POINT ( 'NONE',  ( -1.500000000000001332, -0.5687499993171779566, 0.000000000000000000 ) ) ;
#82233 = CARTESIAN_POINT ( 'NONE',  ( 3.071242857908276669, -2.132312958082840826, -0.8828933859421483898 ) ) ;
#82234 = CARTESIAN_POINT ( 'NONE',  ( 1.411062195701995980, -1.628543573593312921, 1.265665014175233916 ) ) ;
#82235 = CARTESIAN_POINT ( 'NONE',  ( 8.120970824905713314, 8.576813505252564696, 1.040834085586084257E-14 ) ) ;
#82236 = CARTESIAN_POINT ( 'NONE',  ( 6.852720297064418986, 6.959538199522133262, 0.7998128361456331437 ) ) ;
#82237 = CARTESIAN_POINT ( 'NONE',  ( 6.384963997392946844, 6.413822516572072807, 0.7998128361456352531 ) ) ;
#82238 = CARTESIAN_POINT ( 'NONE',  ( 1.364683531249986537, 0.9260416670080896528, 0.7879004041258500513 ) ) ;
#82239 = CARTESIAN_POINT ( 'NONE',  ( 5.716698046817569434, 6.698511138489155137, -1.199719254218452047 ) ) ;
#82240 = CARTESIAN_POINT ( 'NONE',  ( 5.273758565591489145, 9.096542726591325234, -0.7216878364870267237 ) ) ;
#82242 = CARTESIAN_POINT ( 'NONE',  ( 11.33772463945037146, 12.59088423488572062, 3.599999999999998757 ) ) ;
#82241 = CARTESIAN_POINT ( 'NONE',  ( 4.035715546050927749, 2.045666111725014780, -0.7279006231073074096 ) ) ;
#82243 = CARTESIAN_POINT ( 'NONE',  ( -2.365690013115477441, -0.8887487162373138849, -2.290443095882321423 ) ) ;
#82245 = CARTESIAN_POINT ( 'NONE',  ( 2.718100415690410721, 1.734538518968967935, 0.6181264464550640936 ) ) ;
#82244 = CARTESIAN_POINT ( 'NONE',  ( -3.443407828190963915, 6.961133532957338943, 0.7216878364870317197 ) ) ;
#82246 = CARTESIAN_POINT ( 'NONE',  ( -1.201851678989727383E-14, 4.946875000341420581, -1.575800808251660134 ) ) ;
#82247 = CARTESIAN_POINT ( 'NONE',  ( 3.808297599986898430, 1.548825491099754315, -1.550762550882843094 ) ) ;
#82248 = CARTESIAN_POINT ( 'NONE',  ( 8.435195442881084915, 13.95515841652898281, 8.535564829755013960 ) ) ;
#82249 = CARTESIAN_POINT ( 'NONE',  ( 5.981380223923965289, 2.093118249296622491, -0.8594570314751952544 ) ) ;
#82250 = CARTESIAN_POINT ( 'NONE',  ( -5.285102783734889620, 6.572932445422958736, -1.390504041276509062 ) ) ;
#82251 = CARTESIAN_POINT ( 'NONE',  ( 4.669458948634179762, 8.398658883068243597, -0.5498995856093937817 ) ) ;
#82252 = CARTESIAN_POINT ( 'NONE',  ( -6.590672069574513792, 6.861741300691274859, 0.000000000000000000 ) ) ;
#82253 = CARTESIAN_POINT ( 'NONE',  ( 4.638297949650961982, 5.544340708415133712, -1.082531754730548412 ) ) ;
#82254 = CARTESIAN_POINT ( 'NONE',  ( 0.07459516483346910476, 0.007201286963451345932, -1.755573347271717655 ) ) ;
#82255 = CARTESIAN_POINT ( 'NONE',  ( 3.686192936682455734, 1.120187844794858556, 1.672449120617898410 ) ) ;
#82256 = CARTESIAN_POINT ( 'NONE',  ( 7.283754839039659146, 9.520799950344851936, -1.599625672291262513 ) ) ;
#82257 = CARTESIAN_POINT ( 'NONE',  ( 2.678859613419749763, -2.014854250346362008, -0.6126693332187698182 ) ) ;
#82258 = CARTESIAN_POINT ( 'NONE',  ( 1.669406806874464300, 1.322410700044797327, 1.386144426805105523 ) ) ;
#82259 = CARTESIAN_POINT ( 'NONE',  ( 3.659811400685081040, 6.357198169852855685, -1.199719254218446718 ) ) ;
#82260 = CARTESIAN_POINT ( 'NONE',  ( 3.174220446822792141, -0.9683065041741106826, -1.714983525329449421 ) ) ;
#82261 = CARTESIAN_POINT ( 'NONE',  ( 4.816668504955663899, -0.6845142050268312461, -1.900371106210005712 ) ) ;
#82262 = CARTESIAN_POINT ( 'NONE',  ( 0.1099206271272800961, -0.7955684105149689600, -1.691499381818922343 ) ) ;
#82263 = CARTESIAN_POINT ( 'NONE',  ( 0.6429252097494702056, -0.2364460082661112295, -1.947484529462916836 ) ) ;
#82265 = ORIENTED_EDGE ( 'NONE', *, *, #206395, .F. ) ;
#82264 = CARTESIAN_POINT ( 'NONE',  ( 0.3692113334803036606, -1.616751421056546789, -1.021125667832627260 ) ) ;
#82266 = CARTESIAN_POINT ( 'NONE',  ( 4.026408433578586354, 7.641300905909586660, 1.040834085586084257E-14 ) ) ;
#82267 = CARTESIAN_POINT ( 'NONE',  ( -0.6823417656250212460, 0.8635416670080899859, 1.181850606188755259 ) ) ;
#82268 = CARTESIAN_POINT ( 'NONE',  ( 6.455916552660014851, 1.865467424361374249, -0.1398750677365916961 ) ) ;
#82269 = CARTESIAN_POINT ( 'NONE',  ( -0.7158994178059416846, 2.800000000000024691, 1.161830092591057184 ) ) ;
#82270 = EDGE_LOOP ( 'NONE', ( #135087, #206688, #93389, #43519 ) ) ;
#82271 = CARTESIAN_POINT ( 'NONE',  ( 6.280147189154119403, -1.145143509460907039, -1.724508502191648862 ) ) ;
#82272 = CARTESIAN_POINT ( 'NONE',  ( 0.5200892513525963157, 2.048054262204841880, -0.3022008342252607838 ) ) ;
#82273 = CARTESIAN_POINT ( 'NONE',  ( 1.499999999999989120, 1.275000000000019229, 0.000000000000000000 ) ) ;
#82274 = CARTESIAN_POINT ( 'NONE',  ( 5.438792177376376991, 9.497007973581119700, 1.040834085586084257E-14 ) ) ;
#82275 = CARTESIAN_POINT ( 'NONE',  ( -8.015895134177625891, 10.37496362800581018, 1.599625672291295375 ) ) ;
#82276 = CARTESIAN_POINT ( 'NONE',  ( 4.366607992053101128, 7.252070536440704096, -1.199719254218448494 ) ) ;
#82277 = CARTESIAN_POINT ( 'NONE',  ( 5.092489908381383934, -1.177591669451777179, 1.763244422785560150 ) ) ;
#82278 = CARTESIAN_POINT ( 'NONE',  ( 5.585032934186686226, 5.480569609498057382, 0.000000000000000000 ) ) ;
#82279 = CARTESIAN_POINT ( 'NONE',  ( -1.364683531250014514, 1.488541667008084435, -0.7879004041258289570 ) ) ;
#82280 = ORIENTED_EDGE ( 'NONE', *, *, #117967, .F. ) ;
#82281 = CARTESIAN_POINT ( 'NONE',  ( -0.7499999999999972244, 3.108333333333358706, -1.299038105676652011 ) ) ;
#82283 = CARTESIAN_POINT ( 'NONE',  ( 4.792970997630896512, 5.550553237779539018, 1.199719254218464037 ) ) ;
#82282 = CARTESIAN_POINT ( 'NONE',  ( 6.707479306934847507, -1.574971382793718178, -1.169550641929931079 ) ) ;
#82284 = CARTESIAN_POINT ( 'NONE',  ( 4.481795959180916888, 1.842165523724150544, 0.8196470798618460396 ) ) ;
#82285 = CARTESIAN_POINT ( 'NONE',  ( 3.204202018521628226, 1.211454676919420326, -1.484069150048252350 ) ) ;
#82286 = CARTESIAN_POINT ( 'NONE',  ( 11.89317557362582711, 9.837241561624077590, -1.599935658896034729 ) ) ;
#82287 = CARTESIAN_POINT ( 'NONE',  ( 1.945129482973105839, -1.762486321751283835, -1.302348873264857820 ) ) ;
#82288 =( BOUNDED_CURVE ( )  B_SPLINE_CURVE ( 2, ( #130119, #31479, #147360, #213387, #175078, #206478, #70323 ),
 .UNSPECIFIED., .F., .T. ) 
 B_SPLINE_CURVE_WITH_KNOTS ( ( 3, 2, 2, 3 ),
 ( 0.1375000000000000666, 0.1416666666666667740, 0.1458333333333335091, 0.1500000000000002165 ),
 .UNSPECIFIED. ) 
 CURVE ( )  GEOMETRIC_REPRESENTATION_ITEM ( )  RATIONAL_B_SPLINE_CURVE ( ( 0.9999999999999982236, 0.8660254037844404840, 1.000000000000000000, 0.8660254037844387076, 1.000000000000000000, 0.8660254037844316022, 1.000000000000007105 ) ) 
 REPRESENTATION_ITEM ( '' )  );
#82289 = CARTESIAN_POINT ( 'NONE',  ( 0.2026985623078847998, -4.140708350189159503, -0.9999999999999991118 ) ) ;
#82290 = CARTESIAN_POINT ( 'NONE',  ( 3.303821147848403861, -1.868562489643767144, 0.08839296284299941187 ) ) ;
#82291 = CARTESIAN_POINT ( 'NONE',  ( -1.500000000000013101, -0.04791666598384902026, 0.8660254037844403729 ) ) ;
#82292 = APPLICATION_CONTEXT ( 'automotive_design' ) ;
#82293 = CARTESIAN_POINT ( 'NONE',  ( -7.426115451983156923, 9.686887332112256388, -1.599625672291263179 ) ) ;
#82295 = CARTESIAN_POINT ( 'NONE',  ( 5.817987567751313982, 1.043164272916985214, -1.842315021624504778 ) ) ;
#82294 = CARTESIAN_POINT ( 'NONE',  ( -3.958617665510272943, 6.601842462195195438, -1.082531754730549967 ) ) ;
#82296 = CARTESIAN_POINT ( 'NONE',  ( -1.364683531250010295, 8.692708333674730170, 0.7879004041258445001 ) ) ;
#82297 = CARTESIAN_POINT ( 'NONE',  ( -11.41381675112453387, 12.69999999999998153, 3.704697986577180746 ) ) ;
#82299 = CARTESIAN_POINT ( 'NONE',  ( -6.077442586152565163, 6.376797013798398694, -0.4802106596381822134 ) ) ;
#82298 = CARTESIAN_POINT ( 'NONE',  ( 2.331682703721962291, 0.9828498176551370147, -1.845303212725694975 ) ) ;
#82301 = ORIENTED_EDGE ( 'NONE', *, *, #83013, .T. ) ;
#82300 = CARTESIAN_POINT ( 'NONE',  ( 0.9731894095723004900, 1.663878915475509812, -0.4539961392346722469 ) ) ;
#82302 = CARTESIAN_POINT ( 'NONE',  ( 5.764187864104357573, 9.876636274763768597, 1.040834085586084257E-14 ) ) ;
#82303 = SPHERICAL_SURFACE ( 'NONE', #93115, 0.08000000000000000167 ) ;
#82304 = CARTESIAN_POINT ( 'NONE',  ( -6.773846765307993678, -7.473374494058229622, -6.773846765307958151 ) ) ;
#82306 = CARTESIAN_POINT ( 'NONE',  ( 8.554831740098654436, 11.00372300158037042, 1.443375672974076540 ) ) ;
#82305 = CARTESIAN_POINT ( 'NONE',  ( 7.644099680006512187, 7.812537802962739697, 1.040834085586084257E-14 ) ) ;
#82307 = CARTESIAN_POINT ( 'NONE',  ( 0.000000000000000000, -6.054403199333757257, 10.91970695577495931 ) ) ;
#82309 = CARTESIAN_POINT ( 'NONE',  ( 1.752323211514599688, 1.791785093909546323, 0.2653131528348381396 ) ) ;
#82308 = CARTESIAN_POINT ( 'NONE',  ( 4.908934136599710563, 7.884784371745123366, 1.199719254218451159 ) ) ;
#82310 = CARTESIAN_POINT ( 'NONE',  ( -7.206322340863467346, 8.366129804884193888, 1.199719254218450271 ) ) ;
#82311 = CIRCLE ( 'NONE', #158405, 1.500000000000000222 ) ;
#82312 = CARTESIAN_POINT ( 'NONE',  ( 5.854423403002611437, 5.724582146458163656, 1.040834085586084257E-14 ) ) ;
#82313 = CARTESIAN_POINT ( 'NONE',  ( -6.265474751258844677, 6.912123529488261475, 0.7890932636151950508 ) ) ;
#82314 = CARTESIAN_POINT ( 'NONE',  ( 4.766573523656222555, 7.718696989977711809, 1.199719254218452047 ) ) ;
#82315 = CARTESIAN_POINT ( 'NONE',  ( 1.445103857048098739, 8.688264192037886247, -2.625611233228243968 ) ) ;
#82316 = SURFACE_STYLE_USAGE ( .BOTH. , #162533 ) ;
#82317 = CARTESIAN_POINT ( 'NONE',  ( -4.000000000000000000, 2.800000000000026912, 1.214306433183764966E-14 ) ) ;
#82318 = CARTESIAN_POINT ( 'NONE',  ( 8.256552361042350796, 12.57646882128404187, 1.040834085586084257E-14 ) ) ;
#82319 = ORIENTED_EDGE ( 'NONE', *, *, #65507, .T. ) ;
#82320 = ADVANCED_FACE ( 'NONE', ( #212506 ), #30589, .F. ) ;
#82321 = CARTESIAN_POINT ( 'NONE',  ( 3.279601929513912939, -1.794223665640673593, 0.4940275889762090200 ) ) ;
#82322 = CARTESIAN_POINT ( 'NONE',  ( -0.0005723727212556676321, -1.878494010790388913, 0.3742560964640674892 ) ) ;
#82323 = CARTESIAN_POINT ( 'NONE',  ( 6.211935731971203190, -1.911736917912661537, 0.2365620046330171311 ) ) ;
#82324 = CARTESIAN_POINT ( 'NONE',  ( 4.897706171852771462, 4.871974472535213430, 0.6676900015689657408 ) ) ;
#82325 = AXIS2_PLACEMENT_3D ( 'NONE', #108560, #173523, #141040 ) ;
#82326 = CARTESIAN_POINT ( 'NONE',  ( 4.768187943840554333, 8.164982483533503199, -0.7738548252242994918 ) ) ;
#82327 = SURFACE_SIDE_STYLE ('',( #176651 ) ) ;
#82328 = CARTESIAN_POINT ( 'NONE',  ( -3.795919822146283540, 6.412028311603867436, -1.082531754730549967 ) ) ;
#82329 = CARTESIAN_POINT ( 'NONE',  ( 7.619319141200051604, 11.83303006480134911, 0.7216878364870438212 ) ) ;
#82330 = CARTESIAN_POINT ( 'NONE',  ( 4.153143631030720151, 1.666095859335927187, -1.049822023992821984 ) ) ;
#82331 = CARTESIAN_POINT ( 'NONE',  ( 1.541811043186253061, -1.995513645039903361, 0.7175487213698439337 ) ) ;
#82332 = CARTESIAN_POINT ( 'NONE',  ( -5.259673527097670664, 8.223703984000886535, -1.199719254218446718 ) ) ;
#82333 = CARTESIAN_POINT ( 'NONE',  ( -11.89630347798379972, 8.889736554344878527, 1.217639561629326517 ) ) ;
#82334 = CARTESIAN_POINT ( 'NONE',  ( 6.048345925472209395, 6.229027465905260463, 0.7216878364870190632 ) ) ;
#82335 = CARTESIAN_POINT ( 'NONE',  ( 5.384801694919699067, 1.933943663793664225, -1.030698541907522081 ) ) ;
#82336 =( NAMED_UNIT ( * ) SI_UNIT ( $, .STERADIAN. ) SOLID_ANGLE_UNIT ( ) );
#82337 = CARTESIAN_POINT ( 'NONE',  ( 3.944294614955777600, 1.917013643722576433, 0.1899554498810165082 ) ) ;
#82338 = CARTESIAN_POINT ( 'NONE',  ( -7.555971681517696936, 7.709721804725773175, 0.7998128361456462443 ) ) ;
#82339 = CARTESIAN_POINT ( 'NONE',  ( 0.1471128783409255958, -1.407412912164500263, -1.162481699956314785 ) ) ;
#82340 = CARTESIAN_POINT ( 'NONE',  ( 1.366164030173491195, 2.173753390890633685, -0.3800739277931909355 ) ) ;
#82341 = CARTESIAN_POINT ( 'NONE',  ( -6.168302983024037900, 6.978022005381355974, 0.9131412519865607091 ) ) ;
#82342 = ORIENTED_EDGE ( 'NONE', *, *, #195841, .T. ) ;
#82343 = DIRECTION ( 'NONE',  ( 1.276756478318932585E-15, -1.000000000000000000, 1.665334536937738262E-16 ) ) ;
#82344 = ORIENTED_EDGE ( 'NONE', *, *, #51928, .F. ) ;
#82345 = CARTESIAN_POINT ( 'NONE',  ( 6.631706394207740551, 1.885626601332585306, -0.5685293109318545479 ) ) ;
#82346 = CARTESIAN_POINT ( 'NONE',  ( 2.050241756059832721, -1.499988152044306133, 1.233518166440790598 ) ) ;
#82347 = CARTESIAN_POINT ( 'NONE',  ( 6.591202130252849400, 1.331619970128885777, -1.873199602832905430 ) ) ;
#82349 = CARTESIAN_POINT ( 'NONE',  ( 4.610102165239228889, 1.860615736367857265, -0.04253844368732987574 ) ) ;
#82348 = CARTESIAN_POINT ( 'NONE',  ( -6.200875153403786477, 8.327716660428123419, -1.599625672291271394 ) ) ;
#82350 = CARTESIAN_POINT ( 'NONE',  ( 5.468734858265785093, 7.473552982767158070, 1.599625672291269396 ) ) ;
#82351 = CARTESIAN_POINT ( 'NONE',  ( 8.014278199453780616, 8.522615118883788199, 0.000000000000000000 ) ) ;
#82352 = CARTESIAN_POINT ( 'NONE',  ( 6.509000000000020769, 1.267728212239338736, 2.115804336118334295 ) ) ;
#82353 = CARTESIAN_POINT ( 'NONE',  ( -5.799137018343247796, 7.788745826199009237, -1.599625672291256295 ) ) ;
#82354 = CARTESIAN_POINT ( 'NONE',  ( -3.387811967423835835, -0.9606458502256096654, 0.3526910777686760312 ) ) ;
#82355 = CARTESIAN_POINT ( 'NONE',  ( 1.822082775007987543, 1.258534617508931586, -1.793986466278547853 ) ) ;
#82356 = CARTESIAN_POINT ( 'NONE',  ( 4.202664430556254160, 5.926194473780837413, 1.443375672974062551 ) ) ;
#82357 = EDGE_LOOP ( 'NONE', ( #120079, #95798, #118310 ) ) ;
#82358 = CARTESIAN_POINT ( 'NONE',  ( 0.000000000000000000, 5.999999999999998224, -1.500000000000000222 ) ) ;
#82359 = CARTESIAN_POINT ( 'NONE',  ( 0.1263921868141488214, 7.050106634747087320, 4.033475512996062662 ) ) ;
#82360 = CARTESIAN_POINT ( 'NONE',  ( 2.139018802738294589, -1.631172329757241801, 0.8201644002571031322 ) ) ;
#82361 = CARTESIAN_POINT ( 'NONE',  ( -3.113568832632681360, 6.784247404713427798, -0.7998128361456281477 ) ) ;
#82362 = VECTOR ( 'NONE', #89818, 1000.000000000000000 ) ;
#82363 = CARTESIAN_POINT ( 'NONE',  ( 3.744493841719060967, 1.720499418279351822, -0.2165549783500023973 ) ) ;
#82364 = CARTESIAN_POINT ( 'NONE',  ( -6.258858270227934284, 6.997355405945988593, -0.9884160956115575214 ) ) ;
#82365 = CARTESIAN_POINT ( 'NONE',  ( 6.609000000000053276, 0.5717736360873815205, 2.152148306911850995 ) ) ;
#82366 = CARTESIAN_POINT ( 'NONE',  ( -0.6125000000000226930, 0.2083333333333242665, -1.060881119635965764 ) ) ;
#82367 = CARTESIAN_POINT ( 'NONE',  ( 6.692070433991195166, -0.7751425012093198230, 1.651373049820707317 ) ) ;
#82368 = CARTESIAN_POINT ( 'NONE',  ( 4.153139481255548660, 1.659551801668930793, -1.045809187271130591 ) ) ;
#82369 = VECTOR ( 'NONE', #76472, 1000.000000000000000 ) ;
#82370 = CARTESIAN_POINT ( 'NONE',  ( -7.771848369131641121, 10.09024240211882351, -1.599625672291263179 ) ) ;
#82371 = CARTESIAN_POINT ( 'NONE',  ( 6.908042961362778733, 8.018137195466769285, 1.199719254218462483 ) ) ;
#82372 = CARTESIAN_POINT ( 'NONE',  ( 5.338584462458719315, 1.262900380722062454, -1.703257760751579530 ) ) ;
#82373 = CARTESIAN_POINT ( 'NONE',  ( -8.779068160048691283, 10.20099992726700933, -1.199719254218446718 ) ) ;
#82374 = CARTESIAN_POINT ( 'NONE',  ( 5.996784015946103885, 5.890669528225568996, 1.040834085586084257E-14 ) ) ;
#82375 = CARTESIAN_POINT ( 'NONE',  ( 2.975506508543227291, -0.2074491501150333705, 2.059866449969804503 ) ) ;
#82377 = CARTESIAN_POINT ( 'NONE',  ( -1.364683531250000748, 0.5718750003414208027, 0.000000000000000000 ) ) ;
#82376 = CARTESIAN_POINT ( 'NONE',  ( -0.3387883092347166447, -5.166862915010296042, -10.99523224158953383 ) ) ;
#82378 = ORIENTED_EDGE ( 'NONE', *, *, #150147, .F. ) ;
#82379 = CARTESIAN_POINT ( 'NONE',  ( 3.094664012895144367, -0.4461126415513679833, 2.254854857015383462 ) ) ;
#82380 = CARTESIAN_POINT ( 'NONE',  ( 8.595506201384013778, 10.09080732544527592, 1.082531754730558626 ) ) ;
#82382 = CARTESIAN_POINT ( 'NONE',  ( -3.285556943750000070, -1.859374999522041882, 0.000000000000000000 ) ) ;
#82381 = CARTESIAN_POINT ( 'NONE',  ( 6.048345925472191631, 7.189396680206621149, 1.082531754730549967 ) ) ;
#82383 = CARTESIAN_POINT ( 'NONE',  ( 6.720655732516650716, 2.467238681591706673, 2.210725262702870175 ) ) ;
#82384 = CARTESIAN_POINT ( 'NONE',  ( 1.224999999999979661, 1.624999999999987566, -3.989863994746656317E-14 ) ) ;
#82385 =( NAMED_UNIT ( * ) SI_UNIT ( $, .STERADIAN. ) SOLID_ANGLE_UNIT ( ) );
#82386 = ORIENTED_EDGE ( 'NONE', *, *, #106610, .T. ) ;
#82387 = CARTESIAN_POINT ( 'NONE',  ( 10.07334494482924292, 11.81495252613139257, -1.082531754730537088 ) ) ;
#82388 = CARTESIAN_POINT ( 'NONE',  ( 3.902528505893249733, -1.892296425594198750, -0.2755589300712790735 ) ) ;
#82389 = CARTESIAN_POINT ( 'NONE',  ( -0.4000000000000114575, 2.999999999999999112, 2.023857702507764422 ) ) ;
#82390 = CARTESIAN_POINT ( 'NONE',  ( 5.157137038817142916, -1.458691705945897032, -0.9200343150467110709 ) ) ;
#82391 = CARTESIAN_POINT ( 'NONE',  ( 3.678922940808615483, 1.700962499606586853, -1.082838980105811366 ) ) ;
#82392 = CARTESIAN_POINT ( 'NONE',  ( 5.449893634413335519, -2.076765696135183248, -0.9856196477224605790 ) ) ;
#82393 = CARTESIAN_POINT ( 'NONE',  ( 11.41381675112453564, 11.03005666089991799, 3.704697986577179858 ) ) ;
#82394 = CARTESIAN_POINT ( 'NONE',  ( 0.2412292383832773390, 0.3817025157030576321, 2.173470055567463088 ) ) ;
#82395 = CARTESIAN_POINT ( 'NONE',  ( -5.533136088152923904, 6.588318536667425285, 1.082531754730549078 ) ) ;
#82396 = CARTESIAN_POINT ( 'NONE',  ( 5.694547528447587048, -0.4312477495709844399, -1.716266690248748672 ) ) ;
#82398 = CARTESIAN_POINT ( 'NONE',  ( 2.414399183035727425, 1.495821068830467615, -1.737032439462746325 ) ) ;
#82397 = CARTESIAN_POINT ( 'NONE',  ( 5.794130544993763898, 7.853181283949808744, 1.599625672291269396 ) ) ;
#82399 = CARTESIAN_POINT ( 'NONE',  ( 6.615202361034350886, -1.784545987531281019, 0.4526050685512914007 ) ) ;
#82400 = CARTESIAN_POINT ( 'NONE',  ( 0.4499999999999834133, 3.949999999999995293, 0.8338124244295450627 ) ) ;
#82401 = CIRCLE ( 'NONE', #213806, 11.95586206894151005 ) ;
#82402 = CARTESIAN_POINT ( 'NONE',  ( -3.169574050544739841, 6.919863168935977527, -0.7998128361456481317 ) ) ;
#82403 = CARTESIAN_POINT ( 'NONE',  ( -5.558564015327489343E-14, 0.4843750003414603600, 1.570758158831762286 ) ) ;
#82404 = CARTESIAN_POINT ( 'NONE',  ( 0.000000000000000000, 0.000000000000000000, 8.300000000000000711 ) ) ;
#82405 = CARTESIAN_POINT ( 'NONE',  ( 0.3972422249299937258, 0.3718246657071262451, 2.138946393809169511 ) ) ;
#82406 = CARTESIAN_POINT ( 'NONE',  ( 2.852750215419812108, -1.865046845876184189, -0.7672916333427428626 ) ) ;
#82407 = CARTESIAN_POINT ( 'NONE',  ( -1.500000000000001332, 0.1812500006828157706, 0.000000000000000000 ) ) ;
#82408 = CARTESIAN_POINT ( 'NONE',  ( 5.461526653864938297, 0.3736970969714300539, -1.889748759083320406 ) ) ;
#82409 = CARTESIAN_POINT ( 'NONE',  ( 0.6823417656249934904, 11.19270833367473550, 1.181850606188764807 ) ) ;
#82410 = CARTESIAN_POINT ( 'NONE',  ( 2.039591900818237491, 0.005460781979979567602, 2.221583674558536892 ) ) ;
#82411 = VERTEX_POINT ( 'NONE', #196278 ) ;
#82412 = CARTESIAN_POINT ( 'NONE',  ( -9.578539647746888264, -9.962495449538964820, 0.1460552299441092994 ) ) ;
#82413 = CARTESIAN_POINT ( 'NONE',  ( -1.298432343300637860E-14, 2.519999999999999130, -2.000000000000000000 ) ) ;
#82414 = CARTESIAN_POINT ( 'NONE',  ( 9.215791728987056786, 11.77484298861683598, -1.599625672291262513 ) ) ;
#82415 = CARTESIAN_POINT ( 'NONE',  ( -1.500000000000021316, 5.202083334016151639, 0.8660254037844343777 ) ) ;
#82416 = AXIS2_PLACEMENT_3D ( 'NONE', #195783, #212007, #144939 ) ;
#82417 = CARTESIAN_POINT ( 'NONE',  ( 4.933026880143430049, -1.235701381803285148, -1.225916536586797667 ) ) ;
#82418 = CARTESIAN_POINT ( 'NONE',  ( 3.420314466093795414, 0.8798059112791326575, 1.753580237611163994 ) ) ;
#82420 = CARTESIAN_POINT ( 'NONE',  ( -6.236387472606141458, 10.21960978477508952, -0.7216878364870278340 ) ) ;
#82419 = CARTESIAN_POINT ( 'NONE',  ( 5.671388329218120639, 5.511041227042920099, 1.040834085586084257E-14 ) ) ;
#82421 = CARTESIAN_POINT ( 'NONE',  ( -5.911556925646939575, 6.000462466000660022, -0.05029327469607651480 ) ) ;
#82422 = CARTESIAN_POINT ( 'NONE',  ( 5.061948053633171796, 2.238818834584723749, -0.3250485201948364877 ) ) ;
#82423 = CARTESIAN_POINT ( 'NONE',  ( 0.9595213787957155294, 1.685235279958563037, 1.189114231603551675 ) ) ;
#82424 = CARTESIAN_POINT ( 'NONE',  ( -8.182509401047415309, 9.505014708432145909, 1.199719254218462483 ) ) ;
#82425 = CARTESIAN_POINT ( 'NONE',  ( -3.917943204224921150, 5.594019709727598766, -1.443375672974051449 ) ) ;
#82426 = CARTESIAN_POINT ( 'NONE',  ( 2.378104638162964246, 1.391771292293322082, 1.783738300129237508 ) ) ;
#82427 = ORIENTED_EDGE ( 'NONE', *, *, #108367, .T. ) ;
#82428 = CARTESIAN_POINT ( 'NONE',  ( 1.499999999999987121, -0.2145833326505137972, 0.8660254037844524744 ) ) ;
#82429 = CARTESIAN_POINT ( 'NONE',  ( 2.934663490303309530, 0.2251962677765201870, 1.856852477824536329 ) ) ;
#82430 = CARTESIAN_POINT ( 'NONE',  ( 1.722904486866124962, 1.715286564835089456, 0.2538950934896730405 ) ) ;
#82431 = CARTESIAN_POINT ( 'NONE',  ( 5.513277522340928272, -2.138352208816508782, 0.4792397250529822905 ) ) ;
#82432 = CARTESIAN_POINT ( 'NONE',  ( 6.405331179067034419, 1.913585160600343782, 1.289386977092843889 ) ) ;
#82433 = CARTESIAN_POINT ( 'NONE',  ( 1.745067373267340960, -1.741593738584124695, 1.101550882630119244 ) ) ;
#82434 = CARTESIAN_POINT ( 'NONE',  ( 4.048723784538146298, -1.615201170136868924, -1.077811959465636571 ) ) ;
#82435 = CARTESIAN_POINT ( 'NONE',  ( -4.785665035499573783, 5.645992631913323123, 1.082531754730558626 ) ) ;
#82436 = CARTESIAN_POINT ( 'NONE',  ( 6.837182164354378422, -1.670574593475544489, 0.8415915117672703172 ) ) ;
#82437 = CARTESIAN_POINT ( 'NONE',  ( 1.437500000000001110, 1.451031289061064156, -1.451031289061176288 ) ) ;
#82438 = CARTESIAN_POINT ( 'NONE',  ( 0.8610211112611746431, 13.30206454917688497, 1.155895390264894518 ) ) ;
#82439 = CARTESIAN_POINT ( 'NONE',  ( 6.485703859413265882, 1.880147802650249611, 0.7282652505391642439 ) ) ;
#82440 = CARTESIAN_POINT ( 'NONE',  ( -3.555477883677943599E-14, 1.578125000341449535, -1.570758158831814466 ) ) ;
#82441 = CARTESIAN_POINT ( 'NONE',  ( 4.887342357109405455, -0.6819942819097268849, -1.897698409216505233 ) ) ;
#82442 = CARTESIAN_POINT ( 'NONE',  ( -10.17947440576205054, 10.77047498301088346, 0.7998128361456462443 ) ) ;
#82443 = CARTESIAN_POINT ( 'NONE',  ( 6.934105498385400246, 10.17720795050327354, -1.199719254218441611 ) ) ;
#82444 = CARTESIAN_POINT ( 'NONE',  ( 5.551137550152489553, 5.441024994791534120, 0.7998128361456352531 ) ) ;
#82446 = CARTESIAN_POINT ( 'NONE',  ( 11.33772463945037146, 10.19999999999998153, 3.599999999999999201 ) ) ;
#82445 = CARTESIAN_POINT ( 'NONE',  ( 2.613660848560446226, -1.805822647967849193, 0.2677728182119283318 ) ) ;
#82447 = CARTESIAN_POINT ( 'NONE',  ( 6.979380938965668690, -8.233137084989705201, -6.445605026751793254 ) ) ;
#82448 = CARTESIAN_POINT ( 'NONE',  ( -10.41980074470002648, 5.020554563858687480, 5.279403930596816785 ) ) ;
#82449 = ORIENTED_EDGE ( 'NONE', *, *, #29537, .F. ) ;
#82450 = CARTESIAN_POINT ( 'NONE',  ( -5.926322542504877333, 7.047036066744706950, -1.082531754730549967 ) ) ;
#82451 = EDGE_CURVE ( 'NONE', #153088, #202349, #209292, .T. ) ;
#82452 = CARTESIAN_POINT ( 'NONE',  ( 3.285556943749998737, -3.842708332855377051, -1.896917185911906500 ) ) ;
#82454 = CARTESIAN_POINT ( 'NONE',  ( -9.321394304595349567, 10.83371376257142416, 1.199719254218462483 ) ) ;
#82453 = B_SPLINE_CURVE_WITH_KNOTS ( 'NONE', 3,
 ( #32469, #16188, #62833, #211208, #33530, #178740, #145202, #63902, #64953, #128994, #147302, #182975, #199205, #83333, #15133, #131104, #197093, #146254, #17257, #130058, #47684, #95373, #163549, #179798, #96439, #50852, #46608, #14063, #180845, #148365, #81221, #48733, #80149, #31417, #67065, #97493, #212268, #198150, #161424, #114846, #99601, #82271, #214364, #133202, #65994, #132144, #149418, #79083, #49782, #116978, #13007, #38868, #101731, #37800, #104953, #70268, #169924, #72413, #86549, #184036, #121267, #187242, #85479, #56187, #166739, #36718, #134268, #118051, #22592, #103875, #120190, #35652, #2063, #122347, #102805, #54054, #185092, #152614, #135321, #69202, #21509, #100662, #52975, #186166, #201336, #84413, #68135, #20464, #136383, #18332, #170993, #168861, #137452, #151565, #4198, #150503, #119112, #55121, #200275, #202401, #204538, #51926, #87618, #153690, #88698, #154757, #5259, #19398, #71335, #6341, #203466, #138514, #3132, #34592, #167801, #107131, #192561, #205615, #77757, #76689, #176340, #156900, #110337, #27946, #106052, #8488, #143879, #140674, #208808, #94042, #160081, #57255, #92974, #39945, #7409, #209872, #126598, #61511, #157970, #125536, #43163, #89778, #60439, #123415, #23668, #74572, #9561, #155825, #25803, #188303, #172076, #11683, #108206, #91912, #75637, #24736, #44216, #206689, #58318, #175285, #73491, #124475, #189379, #139591, #41022, #173154, #59380, #26871, #174228, #141745, #90837, #190432, #42091, #207753, #191496, #142804, #109276, #159019, #10613, #729, #46344, #197891, #163284, #48478, #165400, #179538, #62567, #214108, #111399, #30081, #130844, #128731, #131882, #194703, #196838, #144937, #33265, #148105, #114595, #180586, #115641, #129800, #147048, #63643, #31158, #13811, #162224, #32209, #96173, #99348, #213070, #95103, #79882, #29018, #210942, #98283, #97230, #14867, #80956, #64701, #161151, #195780, #193636, #145992, #65735, #12739, #212004, #83072, #127676, #47417, #164342, #16996, #113532, #15930, #78813, #45278, #149149, #112461, #177403, #82014, #178471, #49520, #181637, #74052, #84150, #173712, #172627, #57797, #38345, #5808, #88166, #105507, #91389, #139064, #104422, #25289, #166469, #132934, #100402, #170470, #54596, #18062, #157449, #7960, #66795, #39412, #6883, #205091, #34327, #182708, #156376, #150236, #116708, #22056, #171539, #1806, #121814, #198941, #50585, #123957, #204011, #23132, #67864, #137993, #55658, #154236, #140143, #136926, #187782, #71884, #202954, #120744, #186718, #89249, #155300, #122900, #72962, #56732, #188859, #40496, #189925, #90307, #206167, #106600, #24204, #41570, #107684, #58861, #42642, #209351, #110880, #75119, #79382, #11160, #111957, #126080, #159564, #141229, #43704, #29575, #125019, #143355, #94589, #207238, #27423, #128230, #211499, #95665, #127153, #208292, #210432, #195273, #176886, #60999, #59925, #192041, #76176, #142282, #13309, #26350, #113023, #62073, #193125, #109822, #145501, #63134, #190975, #175833, #179031, #93522, #161717, #129298, #46907, #92466, #194193, #108751, #174775, #30649, #96733, #9044, #44773, #77238, #28497, #160631, #12232, #78306, #158503, #10102, #144430, #45837, #177960, #47982, #97786, #163848, #17549, #167038, #116211, #35955, #16489, #82570, #32766, #149721, #162783, #64207, #164896, #198443, #99904 ),
 .UNSPECIFIED., .F., .F.,
 ( 4, 1, 1, 1, 1, 1, 1, 1, 1, 1, 1, 1, 1, 1, 1, 1, 1, 1, 1, 1, 1, 1, 1, 1, 1, 1, 1, 1, 1, 1, 1, 1, 1, 1, 1, 1, 1, 1, 1, 1, 1, 1, 1, 1, 1, 1, 1, 1, 1, 1, 1, 1, 1, 1, 1, 1, 1, 1, 1, 1, 1, 1, 1, 1, 1, 1, 1, 1, 1, 1, 1, 1, 1, 1, 1, 1, 1, 1, 1, 1, 1, 1, 1, 1, 1, 1, 1, 1, 1, 1, 1, 1, 1, 1, 1, 1, 1, 1, 1, 1, 1, 1, 1, 1, 1, 1, 1, 1, 1, 1, 1, 1, 1, 1, 1, 1, 1, 1, 1, 1, 1, 1, 1, 1, 1, 1, 1, 1, 1, 1, 1, 1, 1, 1, 1, 1, 1, 1, 1, 1, 1, 1, 1, 1, 1, 1, 1, 1, 1, 1, 1, 1, 1, 1, 1, 1, 1, 1, 1, 1, 1, 1, 1, 1, 1, 1, 1, 1, 1, 1, 1, 1, 1, 1, 1, 1, 1, 1, 1, 1, 1, 1, 1, 1, 1, 1, 1, 1, 1, 1, 1, 1, 1, 1, 1, 1, 1, 1, 1, 1, 1, 1, 1, 1, 1, 1, 1, 1, 1, 1, 1, 1, 1, 1, 1, 1, 1, 1, 1, 1, 1, 1, 1, 1, 1, 1, 1, 1, 1, 1, 1, 1, 1, 1, 1, 1, 1, 1, 1, 1, 1, 1, 1, 1, 1, 1, 1, 1, 1, 1, 1, 1, 1, 1, 1, 1, 1, 1, 1, 1, 1, 1, 1, 1, 1, 1, 1, 1, 1, 1, 1, 1, 1, 1, 1, 1, 1, 1, 1, 1, 1, 1, 1, 1, 1, 1, 1, 1, 1, 1, 1, 1, 1, 1, 1, 1, 1, 1, 1, 1, 1, 1, 1, 1, 1, 1, 1, 1, 1, 1, 1, 1, 1, 1, 1, 1, 1, 1, 1, 1, 1, 1, 1, 1, 1, 1, 1, 1, 1, 1, 1, 1, 1, 1, 1, 1, 1, 1, 1, 1, 1, 1, 1, 1, 1, 1, 1, 1, 1, 1, 1, 1, 1, 1, 1, 1, 1, 1, 1, 1, 1, 1, 1, 1, 1, 1, 1, 1, 1, 1, 1, 1, 1, 1, 1, 1, 1, 1, 1, 1, 1, 1, 1, 1, 4 ),
 ( 0.000000000000000000, 0.002599974731368114196, 0.005208790931971673047, 0.007813145979665977320, 0.01041652777592116073, 0.01302061325022423749, 0.01562498222773845216, 0.01822909327250534645, 0.02083329118620782031, 0.02343750764584028035, 0.02604160881127103033, 0.02864587273906003470, 0.03124992668191499748, 0.03385418289307650513, 0.03645825757725845717, 0.03906249379052053466, 0.04166666320740203266, 0.04427081823557592333, 0.04687506849204003262, 0.04947913642841410276, 0.05208339700068515682, 0.05468745344639398126, 0.05729170333903113588, 0.05989581325979084075, 0.06250002080062810883, 0.06510424464624173235, 0.06770834408375023261, 0.07031260355790951155, 0.07291665769283758869, 0.07552091454841564078, 0.07812498837240108851, 0.08072922377910608793, 0.08333339284475561881, 0.08593754734057650058, 0.08854179710653446722, 0.09114586450482109470, 0.09375012458370637902, 0.09635418052565795921, 0.09895842987840544613, 0.1015625393267825388, 0.1041667463075427041, 0.1067709697059155277, 0.1093750686050062593, 0.1119793276133541904, 0.1145833812402851093, 0.1171876375884709082, 0.1197917109360151500, 0.1223959458003068407, 0.1250001144218755300, 0.1276042683764700425, 0.1302085177025434359, 0.1328125845892443313, 0.1354168441945610146, 0.1380208996559441903, 0.1406251484930516882, 0.1432292574929059925, 0.1458334639374244401, 0.1484376869122458475, 0.1510417852965526830, 0.1536460438630466996, 0.1562500970055218374, 0.1588543528702505148, 0.1614584257649260002, 0.1640626601106844606, 0.1666668283118819260, 0.1692709817489688462, 0.1718752306590244638, 0.1744792970577103974, 0.1770835562133957763, 0.1796876112177483997, 0.1822918595631332073, 0.1848959681380851483, 0.1875001740701665309, 0.1901043966452301559, 0.1927084945383780445, 0.1953127526869259389, 0.1979168053684795814, 0.2005210607736844508, 0.2031251332390507092, 0.2057293670901427229, 0.2083335348946688259, 0.2109376878379560227, 0.2135419363558502259, 0.2161460022900811573, 0.2187502610200618980, 0.2213543155909112325, 0.2239585634684796434, 0.2265626716421396125, 0.2291668770855771753, 0.2317710992846666596, 0.2343751967102698508, 0.2369794544647692847, 0.2395835067089256143, 0.2421877616785296505, 0.2447918337381362330, 0.2473960671184182170, 0.2500002345499632850, 0.2526043870231480248, 0.2552086351727278490, 0.2578127006660536624, 0.2604169589942467167, 0.2630210131551104502, 0.2656252605887587936, 0.2682293683847277177, 0.2708335733633049913, 0.2734377952101950116, 0.2760418921918580404, 0.2786461495761977103, 0.2812502014064713896, 0.2838544559643880194, 0.2864585276417753179, 0.2890627605750938911, 0.2916669276573394809, 0.2942710796841097043, 0.2968753274892133587, 0.2994793925651746958, 0.3020836505154881335, 0.3046877042898750165, 0.3072919513034905736, 0.3098960587453611915, 0.3125002632828523530, 0.3151044848013095923, 0.3177085813626279731, 0.3203128384006882490, 0.3229168898405855304, 0.3255211440107198539, 0.3281252153294201834, 0.3307294478396133885, 0.3333336145962333963, 0.3359377662002681064, 0.3385420136847264727, 0.3411460783668558427, 0.3437503359631899347, 0.3463543893746011126, 0.3489586359920627823, 0.3515627431034201722, 0.3541669472235909888, 0.3567711684373747749, 0.3593752646019360286, 0.3619795213175900916, 0.3645835723906095116, 0.3671878261968588575, 0.3697918971803975663, 0.3723961292912953969, 0.3750002957459567798, 0.3776044469509276524, 0.3802086941385645069, 0.3828127584503868142, 0.3854170157166348365, 0.3880210687885642384, 0.3906253150337437030, 0.3932294218381663375, 0.3958336255647753599, 0.3984378464976386924, 0.4010419422890235119, 0.4036461987061379930, 0.4062502494357712601, 0.4088545029020263510, 0.4114585735739221262, 0.4140628053093475813, 0.4166669714857112461, 0.4192711223152827404, 0.4218753692299160307, 0.4244794331949501842, 0.4270836901549991405, 0.4296877429109347002, 0.4322919888076972583, 0.4348960953287579478, 0.4375002986855570652, 0.4401045193612476147, 0.4427086148030301427, 0.4453128709454660106, 0.4479169213551993378, 0.4505211745053449013, 0.4531252448891109341, 0.4557294762728811288, 0.4583336421946030970, 0.4609377926724337327, 0.4635420393378766879, 0.4661461029796354349, 0.4687503596573671660, 0.4713544121207915438, 0.4739586576929967765, 0.4765627639542633909, 0.4791669669649988861, 0.4817711874072597711, 0.4843752825230089321, 0.4869795384146229367, 0.4895835885279371524, 0.4921878413858530310, 0.4947919115049980165, 0.4973961425609249032, 0.5000003082516567554, 0.5026044584014001115, 0.5052087048414615200, 0.5078127681834534446, 0.5104170246027455171, 0.5130210767971369323, 0.5156253220686399796, 0.5182294280936764475, 0.5208336307820899957, 0.5234378510146604491, 0.5260419458279406157, 0.5286462014925853437, 0.5312502513329574461, 0.5338545039225196520, 0.5364585738005485105, 0.5390628045524396006, 0.5416669700358295314, 0.5442711198811350792, 0.5468753661196208427, 0.5494794291853500878, 0.5520836853700766822, 0.5546877373189100791, 0.5572919823135623618, 0.5598960881259297251, 0.5625002905157588939, 0.5651045105623757614, 0.5677086050967478092, 0.5703128605582734600, 0.5729169101491768945, 0.5755211624942581095, 0.5781252321546730411, 0.5807294626263322934, 0.5833336279260263879, 0.5859377774905402125, 0.5885420235512536236, 0.5911460863642216124, 0.5937503423382545220, 0.5963543940650019026, 0.5989586388066517886, 0.6015627444299086468, 0.6041669465448881171, 0.6067711664292861906, 0.6093752607083083861, 0.6119795159905627724, 0.6145835653554690969, 0.6171878174799397820, 0.6197918869462408775, 0.6223961171614702526, 0.6250002823011129305, 0.6276044316084782304, 0.6302086775152213605, 0.6328127400989277396, 0.6354169958861367595, 0.6380210474142689048, 0.6406252919267632073, 0.6432293973844667168, 0.6458335992483292820, 0.6484378189942425763, 0.6510419130414711875, 0.6536461681683013447, 0.6562502173306804520, 0.6588544692584096252, 0.6614585385540960871, 0.6640627685366956579, 0.6666669335399304508, 0.6692710826137896474, 0.6718753283903641238, 0.6744793907683068745, 0.6770836463925611337, 0.6796876977455479363, 0.6822919420527318035, 0.6848960473684391204, 0.6875002490049163528, 0.6901044686360783276, 0.6927085624750688453, 0.6953128174703216979, 0.6979168664536427036, 0.7005211182084990496, 0.7031251873570698585, 0.7057294171308388098, 0.7083335820213095824, 0.7109377308853042088, 0.7135419765555117699, 0.7161460387511890957, 0.7187502942363581671, 0.7213543454376690756, 0.7239585895633880996, 0.7265626947606567132, 0.7291668961934797411, 0.7317711157336249661, 0.7343752093879328813, 0.7369794642754557978, 0.7395835131031885945, 0.7421877647090413532, 0.7447918337339959338, 0.7473960633227341166, 0.7500002281240860658, 0.7526043768018576552, 0.7552086223895014827, 0.7578126844264116979, 0.7604169397963658206, 0.7630209908694718379, 0.7656252348375721661, 0.7682293399399604539, 0.7708335411928610714, 0.7734377606657260040, 0.7760418541589074737, 0.7786461089625497101, 0.7812501576581653007, 0.7838544091388848223, 0.7864584780637244865, 0.7890627074912324179, 0.7916668722271122949, 0.7942710207423038238, 0.7968752662711893198, 0.7994793281728324041, 0.8020835834514440377, 0.8046876344198176101, 0.8072918782541467220, 0.8098959832852158369, 0.8125001843819276148, 0.8151044038112509327, 0.8177084971668638902, 0.8203127519104773668, 0.8229168004974481976, 0.8255210518769072747, 0.8281251207251358881, 0.8307293500152160837, 0.8333335147092740813, 0.8359376630855301915, 0.8385419085794658667, 0.8411459703693440204, 0.8437502255804886220, 0.8463542764676049712, 0.8489585201920134550, 0.8515626251753276588, 0.8541668261395859441, 0.8567710455491102106, 0.8593751387907155870, 0.8619793934981552219, 0.8645834419999574028, 0.8671876933020320477, 0.8697917620971562513, 0.8723959912736143352, 0.8750001559495040881, 0.8776043042104727521, 0.8802085496932706699, 0.8828126113948897569, 0.8854168665624462253, 0.8880209173917842369, 0.8906251610301256783, 0.8932292659892527853, 0.8958334668447968108, 0.8984376862582688084, 0.9010417794094305322, 0.9036460341045560174, 0.9062500825446693220, 0.9088543337932389887, 0.9114584025587700866, 0.9140626316454156797, 0.9166667963267953745, 0.9192709444961273402, 0.9218751899916067805, 0.9244792516284782158, 0.9270835067763207871, 0.9296875575713596795, 0.9322918011475309630, 0.9348959061060417852, 0.9375001068764983181, 0.9401043263176916964, 0.9427084194022110619, 0.9453126741091559815, 0.9479167225106870376, 0.9505209737258253355, 0.9531250424882484751, 0.9557292715345466760, 0.9583334362123939743, 0.9609375841976093291, 0.9635418299546441023, 0.9661458919105455623, 0.9687501459642621215, 0.9713541960184646218, 0.9739584433044384815, 0.9765625494917742344, 0.9791667425299969141, 0.9817709508269629737, 0.9843750450459556323, 0.9869794226472197174, 0.9895834977571079660, 0.9921868632736227100, 0.9947912224625704569, 0.9974000159472320437, 1.000000000000000000 ),
 .UNSPECIFIED. ) ;
#82455 = CARTESIAN_POINT ( 'NONE',  ( 0.0002682147194760230472, -0.9481790448457677600, 1.783359508359374512 ) ) ;
#82456 = CARTESIAN_POINT ( 'NONE',  ( 0.1883438084668061507, 1.224518555304452416, 1.730999496979759300 ) ) ;
#82457 = EDGE_LOOP ( 'NONE', ( #33681, #191866, #26945, #205378 ) ) ;
#82458 = CARTESIAN_POINT ( 'NONE',  ( -5.936491157937300756, 8.019268665717216749, 1.599625672291263179 ) ) ;
#82459 = CARTESIAN_POINT ( 'NONE',  ( 4.222474775652216294, 7.013638773981186958, 1.199719254218462483 ) ) ;
#82460 = CARTESIAN_POINT ( 'NONE',  ( 6.104382415481349966, -0.7394567487006579176, -1.923849829731038019 ) ) ;
#82461 = CARTESIAN_POINT ( 'NONE',  ( 4.570935502227962743, -0.9480417383296577682, 1.779625852769653127 ) ) ;
#82462 = VERTEX_POINT ( 'NONE', #162724 ) ;
#82463 = VERTEX_POINT ( 'NONE', #11103 ) ;
#82464 = CARTESIAN_POINT ( 'NONE',  ( 10.50000000000000178, 10.90000000000000036, -3.600000000000002309 ) ) ;
#82465 = CYLINDRICAL_SURFACE ( 'NONE', #54817, 1.250000000000000000 ) ;
#82466 = AXIS2_PLACEMENT_3D ( 'NONE', #6165, #187067, #38699 ) ;
#82468 = DIRECTION ( 'NONE',  ( 0.000000000000000000, 0.000000000000000000, 1.000000000000000000 ) ) ;
#82467 = CARTESIAN_POINT ( 'NONE',  ( -6.306477729012051725, 7.386587434382707151, 1.199719254218452047 ) ) ;
#82469 = CARTESIAN_POINT ( 'NONE',  ( 5.669760509565840323, 7.437725440679550992, 1.325564871123290356 ) ) ;
#82470 = CARTESIAN_POINT ( 'NONE',  ( 5.220077296912079667, -1.701688162634030999, -1.080898591909580597 ) ) ;
#82471 = CARTESIAN_POINT ( 'NONE',  ( 4.382634408885896171, 1.643497958660003144, -0.8300281608688080404 ) ) ;
#82472 = CARTESIAN_POINT ( 'NONE',  ( 10.95855051086948251, -7.723431457505092190, -0.6286713519883923018 ) ) ;
#82473 = CARTESIAN_POINT ( 'NONE',  ( 3.334905300413065543, 2.251431139208215804, 0.5058342958955232005 ) ) ;
#82474 = CARTESIAN_POINT ( 'NONE',  ( 6.210516883511641772, 9.403297576475722508, 1.199719254218452047 ) ) ;
#82475 = CARTESIAN_POINT ( 'NONE',  ( 5.624359561864977763, 1.292596479719224645, -1.732379065785584871 ) ) ;
#82476 = CARTESIAN_POINT ( 'NONE',  ( 6.272618624616828953, 10.46980549536166016, 1.040834085586084257E-14 ) ) ;
#82477 = CARTESIAN_POINT ( 'NONE',  ( 1.434995430731567101, -1.407912642168735573, -1.337921467293776923 ) ) ;
#82478 = CARTESIAN_POINT ( 'NONE',  ( -3.276266675996675204, 6.974061555304760240, -0.7998128361456281477 ) ) ;
#82479 = CARTESIAN_POINT ( 'NONE',  ( 4.938965133657190698, 1.317805461337580697, 1.882938791714399374 ) ) ;
#82480 = CARTESIAN_POINT ( 'NONE',  ( -9.494322902919321905, 15.33478604102567999, -7.339005329679038070 ) ) ;
#82481 = CARTESIAN_POINT ( 'NONE',  ( -5.842637852846353397, 5.781108681267656202, 0.7998128361456281477 ) ) ;
#82482 = CARTESIAN_POINT ( 'NONE',  ( 3.731198135974967300, -1.728734619261709904, 0.7151963084984153118 ) ) ;
#82483 = VECTOR ( 'NONE', #204727, 1000.000000000000114 ) ;
#82484 = EDGE_CURVE ( 'NONE', #145929, #9969, #41005, .T. ) ;
#82487 = CARTESIAN_POINT ( 'NONE',  ( -4.762657100150483380, 8.778460060142702304, 0.000000000000000000 ) ) ;
#82486 = CARTESIAN_POINT ( 'NONE',  ( -1.402160292154681736E-14, -0.8812499993171809543, -1.732050807568870754 ) ) ;
#82485 = CARTESIAN_POINT ( 'NONE',  ( 1.283307755816986528, 0.1377011610334301639, -1.907463248872851569 ) ) ;
#82488 = CARTESIAN_POINT ( 'NONE',  ( 2.702037527177497012, -0.6914408288211832954, 2.095836555436859872 ) ) ;
#82489 = CARTESIAN_POINT ( 'NONE',  ( 6.883263157960371359, 7.052674735402435502, 2.544342468817725855 ) ) ;
#82490 = CARTESIAN_POINT ( 'NONE',  ( 2.544126380858701797, 6.119897877643793116, 0.7998128361456462443 ) ) ;
#82491 = CARTESIAN_POINT ( 'NONE',  ( 7.499068361690118145, 7.921536974826172361, -0.7216878364870317197 ) ) ;
#82492 = CARTESIAN_POINT ( 'NONE',  ( -3.948449050077848632, 5.629609863222681199, 1.599625672291267398 ) ) ;
#82493 = CARTESIAN_POINT ( 'NONE',  ( -5.926322542504864899, 8.967774495347393682, -1.082531754730549967 ) ) ;
#82494 = CARTESIAN_POINT ( 'NONE',  ( 0.6144489392437714192, 1.362578290646492718, -1.424861684082868063 ) ) ;
#82495 = CARTESIAN_POINT ( 'NONE',  ( 6.721333375000203780, -0.1674226297891309168, 2.271100132491596479 ) ) ;
#82496 = CARTESIAN_POINT ( 'NONE',  ( 1.592165322863370980, 0.9698756732311950568, -1.705302290208744687 ) ) ;
#82497 = CARTESIAN_POINT ( 'NONE',  ( 5.155161738035724639, 1.717805270433828246, -1.141362358335789251 ) ) ;
#82498 = CARTESIAN_POINT ( 'NONE',  ( 3.823036129373602154, 6.443664003369091731, -1.082531754730548412 ) ) ;
#82499 = CARTESIAN_POINT ( 'NONE',  ( 5.692444392891300886, 7.734547439830227411, -1.599625672291281386 ) ) ;
#82500 = ORIENTED_EDGE ( 'NONE', *, *, #33740, .F. ) ;
#82501 = CARTESIAN_POINT ( 'NONE',  ( -1.364683531249997417, 4.821875000341417916, 1.214306433183764966E-14 ) ) ;
#82502 = CARTESIAN_POINT ( 'NONE',  ( -1.737500000000000266, -1.458333333333332371, -3.009438278150923907 ) ) ;
#82503 = CARTESIAN_POINT ( 'NONE',  ( 3.511198595814932766, 5.119484333249288532, 1.443375672974066548 ) ) ;
#82504 = CARTESIAN_POINT ( 'NONE',  ( 0.6378409936122396706, 2.026330576540099404, -0.7799181171992456418 ) ) ;
#82505 = CARTESIAN_POINT ( 'NONE',  ( 1.369155121446740960E-15, 18.91999999999999815, -11.18000000000000149 ) ) ;
#82506 = FACE_OUTER_BOUND ( 'NONE', #142539, .T. ) ;
#82508 = CARTESIAN_POINT ( 'NONE',  ( -11.84668729035104384, 12.59481419982588690, -1.400000000000001688 ) ) ;
#82507 = B_SPLINE_CURVE_WITH_KNOTS ( 'NONE', 3,
 ( #82472, #134471, #2263, #133404, #15329, #81419, #68339 ),
 .UNSPECIFIED., .F., .F.,
 ( 4, 3, 4 ),
 ( 3.314949680324038239E-05, 0.0009000000012044577329, 0.001928999666871126280 ),
 .UNSPECIFIED. ) ;
#82509 = CARTESIAN_POINT ( 'NONE',  ( 1.581098268704693055, 1.730367963306264301, -0.7109649657882493035 ) ) ;
#82510 = CARTESIAN_POINT ( 'NONE',  ( 5.624359561864977763, 1.292596479719224645, -1.732379065785584871 ) ) ;
#82511 = CARTESIAN_POINT ( 'NONE',  ( -6.127725819454865608, 6.002332559294505820, -0.1884722350499398735 ) ) ;
#82512 = PRESENTATION_STYLE_ASSIGNMENT (( #13255 ) ) ;
#82513 = CARTESIAN_POINT ( 'NONE',  ( 6.246047416222394233, 7.008439898793222156, -0.9866338212708870570 ) ) ;
#82514 = CARTESIAN_POINT ( 'NONE',  ( 0.6823417656249917140, 5.655208333674749177, 1.181850606188765695 ) ) ;
#82515 = CARTESIAN_POINT ( 'NONE',  ( 1.102048709075389876, -0.8591247869965330519, 1.708478583560539166 ) ) ;
#82516 = CARTESIAN_POINT ( 'NONE',  ( 2.781836775232096048, -0.9115585761545975663, 1.516887842838773759 ) ) ;
#82517 = CARTESIAN_POINT ( 'NONE',  ( 0.2758376730330712734, 1.891454726169951250, -0.2806862973558504892 ) ) ;
#82519 = CARTESIAN_POINT ( 'NONE',  ( 5.097249261280999200, -0.2764669589378037085, 1.895409748447648202 ) ) ;
#82518 = CARTESIAN_POINT ( 'NONE',  ( 7.709579522695849008, -6.700642373080283321, 7.846302513400023493 ) ) ;
#82520 = CARTESIAN_POINT ( 'NONE',  ( 6.883263157960362477, -0.001323150302089473379, 1.953658984494692330 ) ) ;
#82521 = CARTESIAN_POINT ( 'NONE',  ( 0.7499999999999902300, 4.316666666666691299, -1.299038105676658228 ) ) ;
#82523 = CARTESIAN_POINT ( 'NONE',  ( 1.143014088299774578, 2.045220145331683614, 0.5602274146137007360 ) ) ;
#82522 = AXIS2_PLACEMENT_3D ( 'NONE', #147372, #149489, #84479 ) ;
#82524 = CARTESIAN_POINT ( 'NONE',  ( 2.325000000000005063, 0.000000000000000000, -0.5000000000000004441 ) ) ;
#82525 = CARTESIAN_POINT ( 'NONE',  ( 3.625732356982212412, -1.113523340526129335, -1.502988901547596567 ) ) ;
#82527 = VERTEX_POINT ( 'NONE', #94532 ) ;
#82526 = CARTESIAN_POINT ( 'NONE',  ( 0.6447967512687136082, -1.567379569643694515, 0.9359695128687425258 ) ) ;
#82529 = DIRECTION ( 'NONE',  ( 0.000000000000000000, -1.000000000000000000, 0.000000000000000000 ) ) ;
#82528 = CARTESIAN_POINT ( 'NONE',  ( 4.565167970240332274, -1.970479184476851886, -0.9938812724585781577 ) ) ;
#82530 = CARTESIAN_POINT ( 'NONE',  ( 1.364683531249990311, 4.946875000341417916, 1.214306433183764966E-14 ) ) ;
#82531 = EDGE_CURVE ( 'NONE', #135108, #128654, #53128, .T. ) ;
#82532 = CARTESIAN_POINT ( 'NONE',  ( 2.137244103193221889, -0.09901990427806567352, -2.060404765751827405 ) ) ;
#82533 = CARTESIAN_POINT ( 'NONE',  ( 5.503720292143644777, 8.508425209887878538, 1.199719254218462483 ) ) ;
#82534 = CARTESIAN_POINT ( 'NONE',  ( -8.202846631467911820, 9.528741477256060577, 1.199719254218462483 ) ) ;
#82535 = SURFACE_STYLE_USAGE ( .BOTH. , #193089 ) ;
#82536 = CARTESIAN_POINT ( 'NONE',  ( -3.427332196402439468, -0.01934385360880741186, -0.4151528345443494805 ) ) ;
#82537 = CARTESIAN_POINT ( 'NONE',  ( 1.499999999999822586, 10.00000000000000178, 4.154462424328221104 ) ) ;
#82538 = EDGE_LOOP ( 'NONE', ( #55416, #146322, #152733, #161467 ) ) ;
#82539 = CARTESIAN_POINT ( 'NONE',  ( 4.422371208857902580, 0.9731212702417373350, 1.827393648576709717 ) ) ;
#82540 = CARTESIAN_POINT ( 'NONE',  ( -0.7500000000000215383, 5.191666666666685082, 1.299038105676671107 ) ) ;
#82541 = CARTESIAN_POINT ( 'NONE',  ( 2.020999711022552159, 2.016103727727487804, 0.7800470891412072394 ) ) ;
#82542 = CARTESIAN_POINT ( 'NONE',  ( -4.981341760169012645, 7.953289812593539843, -1.047584607753747399 ) ) ;
#82543 = CARTESIAN_POINT ( 'NONE',  ( 2.315108654539797861, 1.620709295712051246, -1.204917113890991320 ) ) ;
#82544 = FACE_OUTER_BOUND ( 'NONE', #189193, .T. ) ;
#82545 = B_SPLINE_CURVE_WITH_KNOTS ( 'NONE', 3,
 ( #167378, #183615, #198779, #36290 ),
 .UNSPECIFIED., .F., .F.,
 ( 4, 4 ),
 ( 0.000000000000000000, 1.930757672285080358E-06 ),
 .UNSPECIFIED. ) ;
#82546 = ORIENTED_EDGE ( 'NONE', *, *, #72791, .F. ) ;
#82548 = CARTESIAN_POINT ( 'NONE',  ( 7.727784370109387346, 10.99920361756089093, -1.082531754730543083 ) ) ;
#82547 = CARTESIAN_POINT ( 'NONE',  ( -3.475000000000000533, -3.179166666666664476, -2.006292185433948827 ) ) ;
#82549 = CARTESIAN_POINT ( 'NONE',  ( 6.883263157960362477, -0.004191378316371896506, 2.053658919477070910 ) ) ;
#82550 = CARTESIAN_POINT ( 'NONE',  ( 0.4621254960020632074, -1.116205757145168231, 1.679226196708947239 ) ) ;
#82551 = CARTESIAN_POINT ( 'NONE',  ( 6.539320575229274901, 4.692178491785949923, 2.665866134390063813 ) ) ;
#82552 = CARTESIAN_POINT ( 'NONE',  ( 5.232042516939362287, 2.159042084939459816, 0.3751777721049884273 ) ) ;
#82553 = CARTESIAN_POINT ( 'NONE',  ( -1.201851678989727383E-14, 3.118750000682814161, -1.732050807568863648 ) ) ;
#82554 = CARTESIAN_POINT ( 'NONE',  ( 3.322422747544371280, -0.7792853099402965444, -1.746611395919236642 ) ) ;
#82555 = CARTESIAN_POINT ( 'NONE',  ( -4.283486466913726254, 7.084819080452935403, -1.199719254218452047 ) ) ;
#82556 = CARTESIAN_POINT ( 'NONE',  ( 4.812781342726866640, 5.677628323678546529, 1.082531754730560403 ) ) ;
#82558 = CARTESIAN_POINT ( 'NONE',  ( 1.985954055300429566, -2.015913623055834325, 0.05231662700833779323 ) ) ;
#82557 = DIRECTION ( 'NONE',  ( -0.9982742078614211811, 0.000000000000000000, -0.05872483221476467591 ) ) ;
#82559 = CARTESIAN_POINT ( 'NONE',  ( 0.6823417656249934904, 12.50520833367473017, 1.181850606188764807 ) ) ;
#82560 = CIRCLE ( 'NONE', #134555, 2.600000000000000533 ) ;
#82562 = CARTESIAN_POINT ( 'NONE',  ( -3.481411583659053566, 7.283673624236017830, 0.000000000000000000 ) ) ;
#82561 = CARTESIAN_POINT ( 'NONE',  ( 0.1699995558098127968, 1.326729642492694872, 1.869266897796989291 ) ) ;
#82563 = CARTESIAN_POINT ( 'NONE',  ( 3.979312383816283383, 1.623897443016858011, -0.5815980338331677713 ) ) ;
#82564 = CARTESIAN_POINT ( 'NONE',  ( 0.1405533004714799583, 4.081756738537394291, -2.834601852798774413 ) ) ;
#82565 = CARTESIAN_POINT ( 'NONE',  ( 5.020596955762157698, 4.751784624677624080, 1.040834085586084257E-14 ) ) ;
#82566 = CARTESIAN_POINT ( 'NONE',  ( 0.3736316133628529434, 1.073300769168658686, 1.531925686032776124 ) ) ;
#82567 = CARTESIAN_POINT ( 'NONE',  ( 4.325214697959421706, 5.004837554829479451, 1.199719254218462483 ) ) ;
#82568 = CARTESIAN_POINT ( 'NONE',  ( 0.1751657365761703222, 0.2353161675953834020, -2.077853038718394885 ) ) ;
#82569 = ORIENTED_EDGE ( 'NONE', *, *, #149088, .F. ) ;
#82570 = CARTESIAN_POINT ( 'NONE',  ( 0.3388458784313007066, -2.007247006727829852, -0.5063607812752639603 ) ) ;
#82571 = ORIENTED_EDGE ( 'NONE', *, *, #87621, .F. ) ;
#82572 = CARTESIAN_POINT ( 'NONE',  ( 5.549399115596888699, -1.634990982212698230, 0.7802194360074166113 ) ) ;
#82573 = ORIENTED_EDGE ( 'NONE', *, *, #73148, .T. ) ;
#82574 = CARTESIAN_POINT ( 'NONE',  ( 5.017399365509065845, 8.011327138806002779, -1.199719254218450271 ) ) ;
#82575 = FACE_OUTER_BOUND ( 'NONE', #27243, .T. ) ;
#82576 = CARTESIAN_POINT ( 'NONE',  ( 5.549399115596888699, -1.634990982212698230, 0.7802194360074166113 ) ) ;
#82577 = CARTESIAN_POINT ( 'NONE',  ( 6.251718229232841928, 8.387033582228703210, -1.443375672974078761 ) ) ;
#82578 = CARTESIAN_POINT ( 'NONE',  ( 4.030162213014739869, 7.767662802593035209, -0.3896624696924297360 ) ) ;
#82579 = CARTESIAN_POINT ( 'NONE',  ( 4.685856777024981490, 6.842343872427582241, -1.228950205364977899 ) ) ;
#82580 = EDGE_LOOP ( 'NONE', ( #58895, #174142, #46497, #18700 ) ) ;
#82581 = EDGE_CURVE ( 'NONE', #68331, #71979, #174227, .T. ) ;
#82583 = CARTESIAN_POINT ( 'NONE',  ( 9.836604141914616406, 11.43479190611061647, 1.199719254218452047 ) ) ;
#82582 = CARTESIAN_POINT ( 'NONE',  ( 6.637149568644561626, -0.09269223384644230401, -1.858852300295941395 ) ) ;
#82584 = CARTESIAN_POINT ( 'NONE',  ( 3.690956203553748427, 1.644769065816154008, 0.9816995294186120491 ) ) ;
#82585 = DIRECTION ( 'NONE',  ( 0.000000000000000000, 0.000000000000000000, -1.000000000000000000 ) ) ;
#82586 = CARTESIAN_POINT ( 'NONE',  ( -0.4019237886466871523, 11.94866454968463110, -1.499999999999998668 ) ) ;
#82587 =( LENGTH_UNIT ( ) NAMED_UNIT ( * ) SI_UNIT ( .MILLI., .METRE. ) );
#82588 = CARTESIAN_POINT ( 'NONE',  ( 5.341549334104184865, 8.215262742221458581, 1.082531754730558626 ) ) ;
#82590 = CARTESIAN_POINT ( 'NONE',  ( 5.735599800244862045, 0.6120854273203913953, -2.026975329707622731 ) ) ;
#82589 = CARTESIAN_POINT ( 'NONE',  ( -8.839552966430002101, 12.29626697993494666, -1.082531754730543971 ) ) ;
#82591 = CARTESIAN_POINT ( 'NONE',  ( 0.4444780689869810564, 2.156031605563761833, 0.1575401717312311101 ) ) ;
#82592 = CARTESIAN_POINT ( 'NONE',  ( -5.285699784481336927, 7.260012063351913625, 1.599625672291263179 ) ) ;
#82593 = EDGE_CURVE ( 'NONE', #16465, #120494, #70103, .T. ) ;
#82594 = CARTESIAN_POINT ( 'NONE',  ( 3.393283585170187688, 7.180857625999046867, 0.7998128361456271485 ) ) ;
#82595 = CARTESIAN_POINT ( 'NONE',  ( 0.9557436305893592943, 1.823730570757615022, -0.08488363409227267509 ) ) ;
#82596 = CARTESIAN_POINT ( 'NONE',  ( -4.386226389220933441, 5.076017861301227008, -1.199719254218446718 ) ) ;
#82597 = CARTESIAN_POINT ( 'NONE',  ( 3.117977517195897441, -0.8984765085307615529, -1.589086709143338272 ) ) ;
#82598 = CARTESIAN_POINT ( 'NONE',  ( 9.224544533040768712, 13.18315223404452574, 9.019998505197962757 ) ) ;
#82599 = CARTESIAN_POINT ( 'NONE',  ( 2.795058504854182946, -0.1448928079688660830, -1.906987441340234568 ) ) ;
#82600 = ORIENTED_EDGE ( 'NONE', *, *, #60090, .T. ) ;
#82601 = CARTESIAN_POINT ( 'NONE',  ( 2.892966452247947906, 0.2382023302623069438, 1.955005545544076240 ) ) ;
#82602 = CARTESIAN_POINT ( 'NONE',  ( 4.704598389810739079, 1.691404259434112767, 0.9541841752371772456 ) ) ;
#82603 = CARTESIAN_POINT ( 'NONE',  ( -4.516801452008150086, 5.298631777878131111, 1.199719254218452935 ) ) ;
#82605 = CARTESIAN_POINT ( 'NONE',  ( 5.220985865760717992, 1.604251394084664550, -1.386888226476624242 ) ) ;
#82604 = CARTESIAN_POINT ( 'NONE',  ( 6.475954649182838807, 7.584310507915338562, 1.199719254218452047 ) ) ;
#82606 = CARTESIAN_POINT ( 'NONE',  ( -1.868950538045364596, 2.288804294181979298E-16, -0.4856446947087145194 ) ) ;
#82607 = CARTESIAN_POINT ( 'NONE',  ( 2.719282321824310511, 1.616554633311767297, 1.021241153818429614 ) ) ;
#82608 = CARTESIAN_POINT ( 'NONE',  ( 5.577782935947014131, 6.368007920784547693, 1.193350709755973682 ) ) ;
#82609 = DIRECTION ( 'NONE',  ( 0.000000000000000000, -1.000000000000000000, 0.000000000000000000 ) ) ;
#82610 = ORIENTED_EDGE ( 'NONE', *, *, #182079, .F. ) ;
#82611 = CARTESIAN_POINT ( 'NONE',  ( 5.564695703766185275, 5.456842840674144490, 0.000000000000000000 ) ) ;
#82612 = CARTESIAN_POINT ( 'NONE',  ( 4.336591701909254581, 1.236597081578957757, -1.588450131361287987 ) ) ;
#82613 = CARTESIAN_POINT ( 'NONE',  ( -4.600947939797212172, 7.141072520302401472, -1.375236645198579799 ) ) ;
#82614 = CARTESIAN_POINT ( 'NONE',  ( 4.652862234063231739, -1.464609733205827879, 1.089778014065109657 ) ) ;
#82615 = CARTESIAN_POINT ( 'NONE',  ( 0.4146172280090759665, 0.7909515328246279342, 1.913518691844050323 ) ) ;
#82616 = CARTESIAN_POINT ( 'NONE',  ( -8.351459436338030784, 11.72682452816096976, -1.082531754730543971 ) ) ;
#82617 = CARTESIAN_POINT ( 'NONE',  ( -6.569648045741773856, 6.787758985223060648, 0.3860807628459517749 ) ) ;
#82618 = CARTESIAN_POINT ( 'NONE',  ( 0.000000000000000000, 11.29999999999998117, 0.000000000000000000 ) ) ;
#82619 = CARTESIAN_POINT ( 'NONE',  ( 5.330866702616011921, 0.1386157390740362649, 1.865562100978317206 ) ) ;
#82620 = CARTESIAN_POINT ( 'NONE',  ( 6.401421083946654100, 10.62007503124645957, -0.7998128361456291469 ) ) ;
#82621 = EDGE_CURVE ( 'NONE', #145598, #53161, #46752, .T. ) ;
#82622 = CARTESIAN_POINT ( 'NONE',  ( -4.599240423533815125, 6.388866465587985211, 1.599625672291267175 ) ) ;
#82623 = CARTESIAN_POINT ( 'NONE',  ( -1.364683531250010295, 10.69270833367473372, 0.7879004041258445001 ) ) ;
#82624 = CARTESIAN_POINT ( 'NONE',  ( -4.954615070790188369, 7.867802451642154082, -1.199719254218452047 ) ) ;
#82625 = CARTESIAN_POINT ( 'NONE',  ( 3.063252641683779753, 5.661212951017999373, 1.199719254218450271 ) ) ;
#82626 = CARTESIAN_POINT ( 'NONE',  ( -8.120407659942227241, 8.438506789546210030, 0.7998128361456341429 ) ) ;
#82627 = CARTESIAN_POINT ( 'NONE',  ( -5.799137018343247796, 7.788745826199009237, -1.599625672291256295 ) ) ;
#82628 = AXIS2_PLACEMENT_3D ( 'NONE', #212180, #47597, #78994 ) ;
#82629 = CARTESIAN_POINT ( 'NONE',  ( 0.3739936534635743270, -2.030981289472892026, 0.4004457479018645460 ) ) ;
#82630 = CARTESIAN_POINT ( 'NONE',  ( 1.775175926465226039, 1.840253878465339055, -1.046873989079605050 ) ) ;
#82631 = CARTESIAN_POINT ( 'NONE',  ( 7.553864141108259211, 11.96459193126834464, 1.040834085586084257E-14 ) ) ;
#82633 = EDGE_CURVE ( 'NONE', #7968, #45206, #81459, .T. ) ;
#82632 = CARTESIAN_POINT ( 'NONE',  ( -2.278321918429671467, 2.687264847271879198, 2.500000000000000444 ) ) ;
#82634 = CARTESIAN_POINT ( 'NONE',  ( 6.244996659533327943, -0.2978818936431072983, -2.048576297084458098 ) ) ;
#82635 = CARTESIAN_POINT ( 'NONE',  ( 4.554780495368041748, 6.962214942802684270, -1.182099088617315497 ) ) ;
#82636 = CARTESIAN_POINT ( 'NONE',  ( 4.663641653420880218, 8.384739662392275861, -0.7216878364870207285 ) ) ;
#82638 = DIRECTION ( 'NONE',  ( -0.000000000000000000, 1.000000000000000000, -0.000000000000000000 ) ) ;
#82637 = CARTESIAN_POINT ( 'NONE',  ( 1.737500000000001155, -3.383333333333331971, 3.009438278150922130 ) ) ;
#82639 = CARTESIAN_POINT ( 'NONE',  ( 3.047136720273002641, -1.874302040764055599, -1.319397901421492714 ) ) ;
#82641 = CARTESIAN_POINT ( 'NONE',  ( -0.1409997244346088141, -0.002808977843308038680, -2.000147647483838220 ) ) ;
#82640 = CARTESIAN_POINT ( 'NONE',  ( 0.08226035653636187828, -1.769965142718381124, -0.4472663993063328847 ) ) ;
#82642 = CARTESIAN_POINT ( 'NONE',  ( 2.707167837304753633, 1.638089068140319071, -0.9866689735503200165 ) ) ;
#82643 = EDGE_CURVE ( 'NONE', #68330, #127411, #59777, .T. ) ;
#82644 = ORIENTED_EDGE ( 'NONE', *, *, #134567, .F. ) ;
#82645 = CARTESIAN_POINT ( 'NONE',  ( 7.497295758232718654, 9.769931022736756177, -1.443375672974058777 ) ) ;
#82646 = CARTESIAN_POINT ( 'NONE',  ( 0.2111898618733127897, 1.671471951565723035, -1.121848769376234234 ) ) ;
#82647 = CARTESIAN_POINT ( 'NONE',  ( 1.182386158793121256, 1.172985831986381955, -1.572276950389992933 ) ) ;
#82648 = CARTESIAN_POINT ( 'NONE',  ( 0.2335667940002684739, 0.001055507091213010252, -2.153566573614831281 ) ) ;
#82649 = CARTESIAN_POINT ( 'NONE',  ( -6.201965203247477909, 9.323044272842313518, 1.199719254218452047 ) ) ;
#82650 = CARTESIAN_POINT ( 'NONE',  ( -1.642778471874998480, -0.4885416661887104217, 2.845375778867863303 ) ) ;
#82652 = CARTESIAN_POINT ( 'NONE',  ( 2.430210232679584248, 1.715968397599322737, 0.4327865170333042300 ) ) ;
#82651 = CARTESIAN_POINT ( 'NONE',  ( 3.398458197991469643, 1.647775209707361466, -1.286576258924768235 ) ) ;
#82653 = LINE ( 'NONE', #150881, #98966 ) ;
#82655 = CARTESIAN_POINT ( 'NONE',  ( 5.683585447934278001, -1.035311694948486183, 2.045203486727443121 ) ) ;
#82654 = CARTESIAN_POINT ( 'NONE',  ( 2.179377205606497281, 5.694357173182881482, -0.3219805702579285889 ) ) ;
#82656 = CARTESIAN_POINT ( 'NONE',  ( 3.978220273661048356, -0.1731065449946489199, -1.731690827559639878 ) ) ;
#82657 = CARTESIAN_POINT ( 'NONE',  ( 8.971744963941056028, 11.49012176272984931, 1.599625672291281386 ) ) ;
#82658 = CARTESIAN_POINT ( 'NONE',  ( 3.901714345682657292, 7.774026846596938434, 0.7998128361456271485 ) ) ;
#82659 = CARTESIAN_POINT ( 'NONE',  ( 2.969770354771487320, 1.463018481607085475, 0.9301108516524180247 ) ) ;
#82660 = CARTESIAN_POINT ( 'NONE',  ( 5.195835581519938629, -1.531768914234220347, -1.538983792029069209 ) ) ;
#82661 = CARTESIAN_POINT ( 'NONE',  ( 3.497113557321089861, 6.167384019261527683, -1.199719254218446718 ) ) ;
#82662 = CARTESIAN_POINT ( 'NONE',  ( 6.104703911763087909, 1.883310800321544409, 0.7212973825745233603 ) ) ;
#82663 = CARTESIAN_POINT ( 'NONE',  ( 6.656247777566118629, -1.895918425136842833, 0.7852924748303453661 ) ) ;
#82664 = CARTESIAN_POINT ( 'NONE',  ( -0.7499999999999972244, 4.139583334016149863, -1.299038105676652899 ) ) ;
#82665 = CARTESIAN_POINT ( 'NONE',  ( 1.729391032145210394, -1.814785505609041838, 0.6465514451386763506 ) ) ;
#82666 = CARTESIAN_POINT ( 'NONE',  ( -0.7500000000000179856, 9.322916667349467446, 1.299038105676658228 ) ) ;
#82667 = CARTESIAN_POINT ( 'NONE',  ( 5.519863322019965324, -0.5397129975505778887, 2.154757917147765323 ) ) ;
#82668 = EDGE_LOOP ( 'NONE', ( #75883, #148517, #43741, #3765 ) ) ;
#82669 = CARTESIAN_POINT ( 'NONE',  ( 6.883263157960368694, 4.693146704925188040, 2.608790034323371643 ) ) ;
#82670 = CARTESIAN_POINT ( 'NONE',  ( 0.7499999999999885647, 2.066666666666688634, -1.299038105676652899 ) ) ;
#82671 = CARTESIAN_POINT ( 'NONE',  ( 5.829115978871627135, 8.888053511070525659, 1.199719254218462483 ) ) ;
#82672 = CARTESIAN_POINT ( 'NONE',  ( 4.324687812634887329, 6.068555086205916105, 1.443375672974062551 ) ) ;
#82673 = CARTESIAN_POINT ( 'NONE',  ( 1.911064425300706526, -0.5960121562160587416, -2.139774337300159424 ) ) ;
#82674 = CARTESIAN_POINT ( 'NONE',  ( 6.391066755906244623, 0.1909826923555627554, 1.952524381009380861 ) ) ;
#82675 = CARTESIAN_POINT ( 'NONE',  ( 8.487040972474689582, 9.964264558384387627, -1.082531754730543083 ) ) ;
#82676 = AXIS2_PLACEMENT_3D ( 'NONE', #101166, #183486, #68651 ) ;
#82677 =( NAMED_UNIT ( * ) SI_UNIT ( $, .STERADIAN. ) SOLID_ANGLE_UNIT ( ) );
#82678 = CARTESIAN_POINT ( 'NONE',  ( 3.691562964670865199, 7.528850235416478576, -0.7998128361456362523 ) ) ;
#82679 = CARTESIAN_POINT ( 'NONE',  ( -5.343321937561608337, 5.406499480009534508, 0.7216878364870257245 ) ) ;
#82680 = CARTESIAN_POINT ( 'NONE',  ( 4.229007335028351910, -1.923526752047514110, -0.7451934795693700986 ) ) ;
#82681 = CARTESIAN_POINT ( 'NONE',  ( -5.440899717785814715, 5.242137847038546461, 0.7998128361456341429 ) ) ;
#82682 =( BOUNDED_CURVE ( )  B_SPLINE_CURVE ( 2, ( #108988, #143598, #27664 ),
 .UNSPECIFIED., .F., .T. ) 
 B_SPLINE_CURVE_WITH_KNOTS ( ( 3, 3 ),
 ( 0.000000000000000000, 0.004569332664469506929 ),
 .UNSPECIFIED. ) 
 CURVE ( )  GEOMETRIC_REPRESENTATION_ITEM ( )  RATIONAL_B_SPLINE_CURVE ( ( 1.000000000000000000, 0.9265390601563747719, 0.9336383135903749686 ) ) 
 REPRESENTATION_ITEM ( '' )  );
#82683 = CARTESIAN_POINT ( 'NONE',  ( -1.499999999999997780, 5.681250000682820378, 1.214306433183764966E-14 ) ) ;
#82684 = CARTESIAN_POINT ( 'NONE',  ( 0.6823417656249882723, 0.3427083336747516196, 1.181850606188755259 ) ) ;
#82685 = CARTESIAN_POINT ( 'NONE',  ( 5.712129104542990277, -0.8404194184173617854, -1.671158263034502767 ) ) ;
#82686 = CARTESIAN_POINT ( 'NONE',  ( 4.641094080744356809, 0.6698209448141523303, 1.599790421982680400 ) ) ;
#82687 = CARTESIAN_POINT ( 'NONE',  ( 4.159493969870859509, 0.8249727819007621754, 1.532509256507504025 ) ) ;
#82688 = CARTESIAN_POINT ( 'NONE',  ( 5.034155109375821446, 4.767602470560229122, -0.7998128361456221525 ) ) ;
#82689 = CARTESIAN_POINT ( 'NONE',  ( 1.523386150502318737, -2.156637510313658801, 0.7774349738483375960 ) ) ;
#82690 = CARTESIAN_POINT ( 'NONE',  ( -1.364683531250010295, 5.592708333674750953, 0.7879004041258379498 ) ) ;
#82691 = CARTESIAN_POINT ( 'NONE',  ( 5.196857871947656804, 1.709930586799845553, 1.202785367055765775 ) ) ;
#82692 = CARTESIAN_POINT ( 'NONE',  ( 0.8492453639068753279, 1.839163117542693904, -0.08803940487626948919 ) ) ;
#82693 = DIRECTION ( 'NONE',  ( 0.000000000000000000, 0.000000000000000000, 1.000000000000000000 ) ) ;
#82694 = SURFACE_STYLE_USAGE ( .BOTH. , #131507 ) ;
#82695 = CARTESIAN_POINT ( 'NONE',  ( 1.740861508391436274, 2.010826320759526720, -0.1511413081683593562 ) ) ;
#82696 = CARTESIAN_POINT ( 'NONE',  ( -5.707619481228860536, 5.761236937629468535, -0.7216878364870003004 ) ) ;
#82697 = CARTESIAN_POINT ( 'NONE',  ( 7.019708803244085082, 15.99401525430995186, -9.337312011067078643 ) ) ;
#82698 = CARTESIAN_POINT ( 'NONE',  ( -8.037286134802835491, 8.271255333558444889, -0.7998128361456291469 ) ) ;
#82699 =( BOUNDED_CURVE ( )  B_SPLINE_CURVE ( 2, ( #143216, #156235, #122751, #175680, #25137, #93376, #7812, #188713, #207087 ),
 .UNSPECIFIED., .F., .T. ) 
 B_SPLINE_CURVE_WITH_KNOTS ( ( 3, 2, 2, 2, 3 ),
 ( 0.07812500000000022204, 0.08333333333333332871, 0.09375000000000000000, 0.1041666666666666713, 0.1093749999999998473 ),
 .UNSPECIFIED. ) 
 CURVE ( )  GEOMETRIC_REPRESENTATION_ITEM ( )  RATIONAL_B_SPLINE_CURVE ( ( 0.9330127018922194093, 0.9330127018922221849, 1.000000000000000000, 0.8660254037844387076, 1.000000000000000000, 0.8660254037844387076, 1.000000000000000000, 0.9330127018922212967, 0.9330127018922194093 ) ) 
 REPRESENTATION_ITEM ( '' )  );
#82700 = CARTESIAN_POINT ( 'NONE',  ( 1.346235217667652417, -0.9325981557438846048, 1.848514419461377845 ) ) ;
#82701 = CARTESIAN_POINT ( 'NONE',  ( 5.464099601507359516, 6.333536608968757697, 1.199719254218462483 ) ) ;
#82702 = CARTESIAN_POINT ( 'NONE',  ( -1.360316468750024876, -0.8072916663252578395, 0.7853790794158560518 ) ) ;
#82703 = CARTESIAN_POINT ( 'NONE',  ( 3.071057173463411338, -1.604308532545582366, 1.386676294644908936 ) ) ;
#82704 = CARTESIAN_POINT ( 'NONE',  ( 0.6823417656249864960, -0.8239583329919114574, -1.181850606188749264 ) ) ;
#82705 = CARTESIAN_POINT ( 'NONE',  ( 5.373610676068619973, 1.758448663713826132, -0.4906839848310071139 ) ) ;
#82706 = EDGE_LOOP ( 'NONE', ( #56489, #9931, #202598, #184102, #127164 ) ) ;
#82707 = CARTESIAN_POINT ( 'NONE',  ( -6.154475385960665790, 6.144919136567696505, 0.000000000000000000 ) ) ;
#82708 = EDGE_CURVE ( 'NONE', #92493, #96092, #98524, .T. ) ;
#82709 = CARTESIAN_POINT ( 'NONE',  ( 10.23370702021670020, 10.83374636654133383, 0.7998128361456462443 ) ) ;
#82710 = CARTESIAN_POINT ( 'NONE',  ( 6.875393295461478260, 8.154285278527437342, -1.082531754730548412 ) ) ;
#82711 = CARTESIAN_POINT ( 'NONE',  ( 3.475000000000000533, -2.931249999044084120, 0.000000000000000000 ) ) ;
#82712 = STYLED_ITEM ( 'NONE', ( #65683 ), #43581 ) ;
#82713 = CARTESIAN_POINT ( 'NONE',  ( -6.555530967407501741, 7.606873202518897870, 1.199719254218450271 ) ) ;
#82714 = CARTESIAN_POINT ( 'NONE',  ( 3.445573674754712545, -1.864599547292019155, 0.7769016540176328922 ) ) ;
#82715 = CARTESIAN_POINT ( 'NONE',  ( 6.686557766011572923, -2.162873314485185272, -0.4371622687903350957 ) ) ;
#82716 = CARTESIAN_POINT ( 'NONE',  ( -5.794130544993808307, 7.853181283949808744, 1.599625672291263179 ) ) ;
#82717 = CARTESIAN_POINT ( 'NONE',  ( 10.70146331988817323, 11.37946204949139251, 0.7998128361456341429 ) ) ;
#82718 = CARTESIAN_POINT ( 'NONE',  ( 4.733164070488131259, 0.002922519798398153738, -1.861131630917359336 ) ) ;
#82719 = CARTESIAN_POINT ( 'NONE',  ( 6.726816770674637347, 10.99970333242910669, -0.7998128361456291469 ) ) ;
#82720 =( BOUNDED_SURFACE ( )  B_SPLINE_SURFACE ( 3, 2, ( 
 ( #55150, #139623, #54086 ),
 ( #205646, #124502, #22621 ),
 ( #123446, #120222, #186196 ),
 ( #121297, #190461, #189408 ),
 ( #41050, #37829, #103907 ),
 ( #38898, #44242, #129825 ),
 ( #144960, #63671, #43188 ),
 ( #111425, #194729, #178497 ) ),
 .UNSPECIFIED., .F., .F., .T. ) 
 B_SPLINE_SURFACE_WITH_KNOTS ( ( 4, 2, 2, 4 ),
 ( 3, 3 ),
 ( 0.000000000000000000, 0.0002568729646053799498, 0.0005137459292107598996, 0.001027491858421519799 ),
 ( 0.000000000000000000, 1.000000000000000000 ),
 .UNSPECIFIED. ) 
 GEOMETRIC_REPRESENTATION_ITEM ( )  RATIONAL_B_SPLINE_SURFACE ( (
 ( 1.000000000000000000, 0.3826834323651039926, 1.000000000000000000),
 ( 1.000000000000000000, 0.3847114443833997699, 1.000000000000000000),
 ( 1.000000000000000000, 0.4039255759075961461, 1.000000000000000000),
 ( 1.000000000000000000, 0.4557194474495045444, 1.000000000000000000),
 ( 1.000000000000000000, 0.4874388927523756743, 1.000000000000000000),
 ( 1.000000000000000000, 0.5833547384516969414, 1.000000000000000000),
 ( 1.000000000000000000, 0.6470545345836524742, 1.000000000000000000),
 ( 1.000000000000000000, 0.7045118851637717228, 1.000000000000000000) ) ) 
 REPRESENTATION_ITEM ( '' )  SURFACE ( )  );
#82721 = CARTESIAN_POINT ( 'NONE',  ( -10.95308175811721085, 13.79999999999998295, 1.799999999999999600 ) ) ;
#82722 = CARTESIAN_POINT ( 'NONE',  ( -4.776550190716183586, 4.467063398790632966, 1.214306433183764966E-14 ) ) ;
#82723 = CARTESIAN_POINT ( 'NONE',  ( -7.426115451983156923, 9.686887332112256388, -1.599625672291263179 ) ) ;
#82724 = CARTESIAN_POINT ( 'NONE',  ( 0.1280963075596490419, -1.331634228802502928, -1.703589906866372017 ) ) ;
#82726 = CARTESIAN_POINT ( 'NONE',  ( -4.277165953568806245, 7.474871692096041187, 1.085114461911325101 ) ) ;
#82725 = CARTESIAN_POINT ( 'NONE',  ( -5.250750630242457362, 9.347902511916677426, 0.000000000000000000 ) ) ;
#82727 = CARTESIAN_POINT ( 'NONE',  ( -1.201851678989727383E-14, 0.8218750003414171390, 1.575800808251672791 ) ) ;
#82728 = CARTESIAN_POINT ( 'NONE',  ( 1.791952614948258304, -1.634470817638247642, 0.5789770405969245637 ) ) ;
#82729 = CARTESIAN_POINT ( 'NONE',  ( 1.394060603838151779, 1.424319145653055507, -0.9997159833949519347 ) ) ;
#82730 = MECHANICAL_DESIGN_GEOMETRIC_PRESENTATION_REPRESENTATION (  '', ( #30811 ), #138089 ) ;
#82732 = CARTESIAN_POINT ( 'NONE',  ( 8.758204044748010730, 9.320252261735261001, 0.7216878364870438212 ) ) ;
#82731 = CARTESIAN_POINT ( 'NONE',  ( 6.393248246410252911, 2.011339380631727458, -1.131280203180404342 ) ) ;
#82733 = CARTESIAN_POINT ( 'NONE',  ( 3.040771591214902259, 6.769593633051179005, -0.7998128361456362523 ) ) ;
#82734 = CARTESIAN_POINT ( 'NONE',  ( 2.108734400483037952, 1.529077776457531401, -1.381789073784354560 ) ) ;
#82735 = CARTESIAN_POINT ( 'NONE',  ( 4.873266149108180123, 7.772895376346490970, 1.199719254218462483 ) ) ;
#82736 = COLOUR_RGB ( '', 0.40784314, 0.44705882, 0.49803922) ;
#82737 = EDGE_CURVE ( 'NONE', #90728, #175932, #84199, .T. ) ;
#82738 = CARTESIAN_POINT ( 'NONE',  ( 1.669295836627190610, -0.7230268306642473330, -1.882186858670406693 ) ) ;
#82739 = CARTESIAN_POINT ( 'NONE',  ( 0.005132432257108309609, 7.078226584369340380, -2.121329534126251470 ) ) ;
#82740 = CARTESIAN_POINT ( 'NONE',  ( -6.608673532018475960, 6.674816973635147477, -0.7998128361456362523 ) ) ;
#82741 = CARTESIAN_POINT ( 'NONE',  ( 0.5496082175940236736, 0.6205544711120424273, -1.871312427623121000 ) ) ;
#82743 = CARTESIAN_POINT ( 'NONE',  ( -6.292392690518202159, 9.394856334696294553, -1.082531754730549967 ) ) ;
#82742 = CARTESIAN_POINT ( 'NONE',  ( 5.062724140118719518, 0.5608846916410530348, 1.828269531156314853 ) ) ;
#82744 = CARTESIAN_POINT ( 'NONE',  ( 6.674453038267287752, -1.361800985140369402, 1.737325302230605883 ) ) ;
#82745 = CARTESIAN_POINT ( 'NONE',  ( -7.417719440008134768, 7.826629899530511025, 0.7216878364870317197 ) ) ;
#82746 = CARTESIAN_POINT ( 'NONE',  ( 5.989670002187236442, 10.20997511251894529, -0.7998128361456481317 ) ) ;
#82747 = CARTESIAN_POINT ( 'NONE',  ( -4.462041952228957165, 5.338708711422782471, -1.082531754730549967 ) ) ;
#82748 = CARTESIAN_POINT ( 'NONE',  ( 0.1002680356884171620, -0.9499045104094726577, 1.782327323349098602 ) ) ;
#82749 = DIRECTION ( 'NONE',  ( 1.000000000000000000, 0.000000000000000000, -6.695352868347765393E-17 ) ) ;
#82750 = CARTESIAN_POINT ( 'NONE',  ( 4.805897800482852311, -0.6205396350037055697, 2.222522205952178975 ) ) ;
#82751 = CARTESIAN_POINT ( 'NONE',  ( 5.019951445752288244, 1.940773837913706057, -0.2859759768028962146 ) ) ;
#82752 = CARTESIAN_POINT ( 'NONE',  ( 1.551531708069888715, 1.481957716508151890, 1.285475804911541120 ) ) ;
#82753 = CARTESIAN_POINT ( 'NONE',  ( 8.778014389843965759, 12.32843499053828928, 1.199719254218450271 ) ) ;
#82754 = DIRECTION ( 'NONE',  ( 1.000000000000000000, 0.000000000000000000, -4.440892098500751393E-16 ) ) ;
#82755 = ORIENTED_EDGE ( 'NONE', *, *, #170444, .F. ) ;
#82756 = CARTESIAN_POINT ( 'NONE',  ( 0.4974488191052604535, -0.3042024069639309158, 2.095249342460514086 ) ) ;
#82758 = CARTESIAN_POINT ( 'NONE',  ( -9.155833807930273238, 9.576227618873799585, -0.7998128361456291469 ) ) ;
#82757 = CARTESIAN_POINT ( 'NONE',  ( -5.599681137644054729, 6.491715067794862293, 1.199719254218450271 ) ) ;
#82759 = CARTESIAN_POINT ( 'NONE',  ( 0.8844010234979463592, 1.624802019249080853, -0.8659260420235401767 ) ) ;
#82760 = EDGE_LOOP ( 'NONE', ( #107712, #20127, #47101, #41425 ) ) ;
#82761 = CARTESIAN_POINT ( 'NONE',  ( 4.434556658511819016, -1.254960995779637045, 1.771429847731820661 ) ) ;
#82762 = CARTESIAN_POINT ( 'NONE',  ( 11.33772463945036790, 10.19999999999999929, -3.600000000000000977 ) ) ;
#82763 = CARTESIAN_POINT ( 'NONE',  ( 1.371502371489873751, -1.821557607348308405, -1.085495857948336251 ) ) ;
#82764 = CARTESIAN_POINT ( 'NONE',  ( -1.201851678989727383E-14, 3.243750000682814161, 1.732050807568877637 ) ) ;
#82765 = CARTESIAN_POINT ( 'NONE',  ( 7.995557903757111617, 10.35123685918189729, 1.599625672291281386 ) ) ;
#82766 = CARTESIAN_POINT ( 'NONE',  ( 6.231590709102786008, 7.018523052454695765, 1.002697108273574500 ) ) ;
#82767 = CARTESIAN_POINT ( 'NONE',  ( 2.636070936407476584, 0.9742463255392861399, -1.815968889038493073 ) ) ;
#82769 = CARTESIAN_POINT ( 'NONE',  ( 7.874165004059028306, 14.38583653512666416, -8.999470220878452054 ) ) ;
#82768 = CARTESIAN_POINT ( 'NONE',  ( -8.154339323615371171, 11.60081407993821045, 1.199719254218453823 ) ) ;
#82770 = CARTESIAN_POINT ( 'NONE',  ( 1.364683531249988535, 3.905208333674751842, -0.7879004041258239610 ) ) ;
#82771 = LINE ( 'NONE', #196536, #63592 ) ;
#82772 = CARTESIAN_POINT ( 'NONE',  ( 5.591026288145455325, 7.491806139540827303, -1.383104942081718969 ) ) ;
#82773 = CARTESIAN_POINT ( 'NONE',  ( 4.758414378865199801, 1.907420806491459064, 0.1369992607160031295 ) ) ;
#82774 = B_SPLINE_CURVE_WITH_KNOTS ( 'NONE', 3,
 ( #155756, #43095, #76622, #104881, #156832, #7341 ),
 .UNSPECIFIED., .F., .F.,
 ( 4, 2, 4 ),
 ( 0.000000000000000000, 0.0003132070624402877746, 0.0006264141248805755492 ),
 .UNSPECIFIED. ) ;
#82775 =( BOUNDED_CURVE ( )  B_SPLINE_CURVE ( 2, ( #214283, #135245, #119032, #50766, #181816, #200195, #116895, #150420, #36641 ),
 .UNSPECIFIED., .F., .T. ) 
 B_SPLINE_CURVE_WITH_KNOTS ( ( 3, 2, 2, 2, 3 ),
 ( 0.3541666666666666852, 0.3611111111111111049, 0.3750000000000000000, 0.3888888888888888951, 0.3958333333333333703 ),
 .UNSPECIFIED. ) 
 CURVE ( )  GEOMETRIC_REPRESENTATION_ITEM ( )  RATIONAL_B_SPLINE_CURVE ( ( 0.9330127018922194093, 0.9330127018922196314, 1.000000000000000000, 0.8660254037844387076, 1.000000000000000000, 0.8660254037844387076, 1.000000000000000000, 0.9330127018922190762, 0.9330127018922194093 ) ) 
 REPRESENTATION_ITEM ( '' )  );
#82776 = CARTESIAN_POINT ( 'NONE',  ( -3.022498986271247023, 2.800000000000024691, -2.500000000000000444 ) ) ;
#82777 = CARTESIAN_POINT ( 'NONE',  ( 1.810245590833154283, -2.245401999695510575, 0.2761584955175334644 ) ) ;
#82778 = CARTESIAN_POINT ( 'NONE',  ( -2.767835915484202047, 6.380892334706859792, -0.7998128361456281477 ) ) ;
#82779 = CARTESIAN_POINT ( 'NONE',  ( 1.001899194773261170, -0.8131845483106721062, 1.618847804792804324 ) ) ;
#82780 = CARTESIAN_POINT ( 'NONE',  ( 1.569406966088880084, 1.323937531303821968, 1.384834552875470415 ) ) ;
#82781 = CARTESIAN_POINT ( 'NONE',  ( 3.561042923925850978, 1.633862107263984065, -1.271492733312264090 ) ) ;
#82782 = CARTESIAN_POINT ( 'NONE',  ( 1.364683531249988757, 1.196875000341421469, 0.000000000000000000 ) ) ;
#82783 = CARTESIAN_POINT ( 'NONE',  ( 0.8660190917160478508, 0.9698478150794390684, 1.716334202883246229 ) ) ;
#82784 = CARTESIAN_POINT ( 'NONE',  ( 6.006463946069247939, -0.6956954824784820079, -1.796673741800159707 ) ) ;
#82785 = EDGE_CURVE ( 'NONE', #130236, #69840, #165906, .T. ) ;
#82787 = CARTESIAN_POINT ( 'NONE',  ( 6.080034374691865473, 7.023743017405461586, -0.9950221519831742301 ) ) ;
#82786 = CARTESIAN_POINT ( 'NONE',  ( 1.260874316716424470, 0.9392902264234997967, 2.108064829403846208 ) ) ;
#82788 = CARTESIAN_POINT ( 'NONE',  ( 1.364683531249988757, 1.884375000341421913, 0.000000000000000000 ) ) ;
#82789 = CARTESIAN_POINT ( 'NONE',  ( 4.914538883754228316, 0.7863694667932183968, 1.907089347224044884 ) ) ;
#82790 = CARTESIAN_POINT ( 'NONE',  ( -6.247609857798938293, 6.183299677053865295, -0.7998128361456291469 ) ) ;
#82791 = CARTESIAN_POINT ( 'NONE',  ( -1.123270288250342919, 2.846052654332832610, 0.7749999999993751887 ) ) ;
#82793 = CARTESIAN_POINT ( 'NONE',  ( 1.499999999999990896, 4.775000000000022560, 1.214306433183764966E-14 ) ) ;
#82792 = CARTESIAN_POINT ( 'NONE',  ( 6.229533133763371922, -1.984190613765562494, 0.7061325270490863559 ) ) ;
#82794 = CARTESIAN_POINT ( 'NONE',  ( -1.364683531250012516, 2.342708333674752286, 0.7879004041258379498 ) ) ;
#82795 = CARTESIAN_POINT ( 'NONE',  ( 4.780646861661003832, -2.095393720161139228, -0.5303334973314683953 ) ) ;
#82796 = CARTESIAN_POINT ( 'NONE',  ( 5.022131231807676066, -2.009760515157756444, 0.1999713455246488469 ) ) ;
#82797 = DIRECTION ( 'NONE',  ( 0.000000000000000000, 1.000000000000000000, 0.000000000000000000 ) ) ;
#82798 = CARTESIAN_POINT ( 'NONE',  ( -6.412643469583822586, 6.583764924043652655, 1.040834085586084257E-14 ) ) ;
#82801 = CARTESIAN_POINT ( 'NONE',  ( 6.168596704537822717, 6.299043698156668647, 1.040834085586084257E-14 ) ) ;
#82800 = CARTESIAN_POINT ( 'NONE',  ( -1.642778471875000035, -1.917708332855375897, -2.845375778867859751 ) ) ;
#82799 = CARTESIAN_POINT ( 'NONE',  ( 6.176621499477501054, 9.363752961769195693, -1.199719254218452047 ) ) ;
#82802 = CARTESIAN_POINT ( 'NONE',  ( -4.034433228518296666, 6.864533312316751790, -1.199719254218450271 ) ) ;
#82803 = CARTESIAN_POINT ( 'NONE',  ( 3.485564796978508184, -0.5807542032013839339, 1.931124776463407189 ) ) ;
#82804 = CARTESIAN_POINT ( 'NONE',  ( -7.506410603460441422, 11.90922947067921278, -0.7998128361456291469 ) ) ;
#82806 =( NAMED_UNIT ( * ) SI_UNIT ( $, .STERADIAN. ) SOLID_ANGLE_UNIT ( ) );
#82805 = CARTESIAN_POINT ( 'NONE',  ( -3.735435015764967837, 4.316761258935923884, -1.199719254218452047 ) ) ;
#82807 = CARTESIAN_POINT ( 'NONE',  ( -0.6823417656250212460, 4.801041667008086655, 1.181850606188767472 ) ) ;
#82809 = CARTESIAN_POINT ( 'NONE',  ( -11.86145016429273014, 12.69999999999999929, -1.100000000000000533 ) ) ;
#82808 = CARTESIAN_POINT ( 'NONE',  ( 5.102478102407745908, -0.7247817745383768884, -2.036717088958202471 ) ) ;
#82810 = CARTESIAN_POINT ( 'NONE',  ( -11.51166771951771217, 6.864275254849497188, -3.394607536566083272 ) ) ;
#82812 = CARTESIAN_POINT ( 'NONE',  ( 5.624625116526842383, 0.3961212581503182339, 1.976953148079656719 ) ) ;
#82811 = CARTESIAN_POINT ( 'NONE',  ( -6.195713011320783892, 10.17215624660883577, -0.7216878364870267237 ) ) ;
#82813 = CARTESIAN_POINT ( 'NONE',  ( -0.6823417656250246877, -0.1364583329919108468, 1.181850606188755259 ) ) ;
#82814 = ADVANCED_FACE ( 'NONE', ( #4431 ), #164838, .T. ) ;
#82815 = CARTESIAN_POINT ( 'NONE',  ( 0.5742808809356505506, -1.622453496466894407, -0.5859570326207633739 ) ) ;
#82816 = CARTESIAN_POINT ( 'NONE',  ( 5.061990249855835344, 6.999017606288844284, -1.599625672291273171 ) ) ;
#82818 = CARTESIAN_POINT ( 'NONE',  ( 6.505933609711257226, 8.683618192786854095, -1.599625672291281386 ) ) ;
#82817 = CARTESIAN_POINT ( 'NONE',  ( 8.161645285746708112, 9.584636257201740506, -1.082531754730543083 ) ) ;
#82819 = AXIS2_PLACEMENT_3D ( 'NONE', #186657, #23073, #140082 ) ;
#82820 = CARTESIAN_POINT ( 'NONE',  ( -3.416291520519271874, 6.929497840673697340, 1.040834085586084257E-14 ) ) ;
#82821 = CARTESIAN_POINT ( 'NONE',  ( 6.889956934492897034, -0.7990643998789861424, 1.689675875712663755 ) ) ;
#82822 = CARTESIAN_POINT ( 'NONE',  ( 0.3111896917125516748, 1.672494819392616128, -1.120119447130196288 ) ) ;
#82823 = CARTESIAN_POINT ( 'NONE',  ( 6.539320575229250920, 2.072231551265828475, 2.205269387046896679 ) ) ;
#82824 = CARTESIAN_POINT ( 'NONE',  ( -5.736508391913536897, 9.706693867292189637, 0.7216878364870267237 ) ) ;
#82825 = ORIENTED_EDGE ( 'NONE', *, *, #79256, .F. ) ;
#82826 = CARTESIAN_POINT ( 'NONE',  ( 8.066738210006668908, 12.35501897840907581, 0.7216878364870438212 ) ) ;
#82828 = CARTESIAN_POINT ( 'NONE',  ( 1.950796209937825321, -1.844718841590715863, -0.8146091914792084054 ) ) ;
#82827 = CARTESIAN_POINT ( 'NONE',  ( 2.403126630736720948, -0.3650820022202577175, -2.088671427859823293 ) ) ;
#82829 = CARTESIAN_POINT ( 'NONE',  ( 2.109342631017618874, 1.402271653390272377, 1.146968571259598058 ) ) ;
#82830 = CARTESIAN_POINT ( 'NONE',  ( 7.523848900940885542, 7.742521570711348389, 0.7998128361456291469 ) ) ;
#82831 = CARTESIAN_POINT ( 'NONE',  ( 6.350466702034289312, 0.6732396885240909956, 2.054270918568662729 ) ) ;
#82832 = ORIENTED_EDGE ( 'NONE', *, *, #12404, .T. ) ;
#82833 = AXIS2_PLACEMENT_3D ( 'NONE', #159438, #60872, #28373 ) ;
#82834 = CARTESIAN_POINT ( 'NONE',  ( 6.368579470117202490, 8.453095353268645695, 1.599625672291281386 ) ) ;
#82836 = CARTESIAN_POINT ( 'NONE',  ( 0.7080363470168028472, 1.138615994813133359, -1.540489816406021673 ) ) ;
#82835 = CARTESIAN_POINT ( 'NONE',  ( -3.716906668440817185, 7.488141546489591072, 0.7998128361456341429 ) ) ;
#82837 = PLANE ( 'NONE',  #138706 ) ;
#82838 = CARTESIAN_POINT ( 'NONE',  ( 6.290620086616457662, 6.441404310581745563, 1.040834085586084257E-14 ) ) ;
#82839 = CARTESIAN_POINT ( 'NONE',  ( -1.402160292154681736E-14, 0.5093750003414236893, -1.575800808251659024 ) ) ;
#82840 = CARTESIAN_POINT ( 'NONE',  ( 2.548569689688999329, 5.917155704705049146, -0.7216878364870267237 ) ) ;
#82841 = CARTESIAN_POINT ( 'NONE',  ( -8.622095623286845978, 12.14652976288826913, 1.199719254218462483 ) ) ;
#82842 = CARTESIAN_POINT ( 'NONE',  ( 4.364260218091946975, 1.016419123106377276, 1.907829002176252953 ) ) ;
#82843 = CARTESIAN_POINT ( 'NONE',  ( -6.346625304972878467, 7.537389289624049304, 1.082531754730548412 ) ) ;
#82844 = EDGE_CURVE ( 'NONE', #47983, #171576, #177615, .T. ) ;
#82845 = CARTESIAN_POINT ( 'NONE',  ( 3.906157654512984134, 7.571284673658201569, -0.7216878364870338292 ) ) ;
#82846 = CARTESIAN_POINT ( 'NONE',  ( 1.933984528066152953, -2.055706711753771287, 0.5200354980386610038 ) ) ;
#82847 = CARTESIAN_POINT ( 'NONE',  ( -0.6125000000000175859, 2.541666666666664298, 1.060881119635903147 ) ) ;
#82848 = CARTESIAN_POINT ( 'NONE',  ( 3.725814648419359720, -1.171505211990100159, -1.585385422309880887 ) ) ;
#82849 = CARTESIAN_POINT ( 'NONE',  ( 5.713130151434068438, 1.559639147136464343, -1.106415316399149473 ) ) ;
#82850 = ORIENTED_EDGE ( 'NONE', *, *, #185099, .F. ) ;
#82851 = CARTESIAN_POINT ( 'NONE',  ( 9.609247538824295276, -6.583727468837977881, -0.3728355200474618991 ) ) ;
#82852 = CARTESIAN_POINT ( 'NONE',  ( 5.600048008112708864, 0.7998006467024108002, -1.800045223161725660 ) ) ;
#82853 = CARTESIAN_POINT ( 'NONE',  ( 1.921723552510564259, 1.118073055411296313, -1.587613466820477992 ) ) ;
#82854 = ORIENTED_EDGE ( 'NONE', *, *, #60154, .F. ) ;
#82855 = CARTESIAN_POINT ( 'NONE',  ( -4.309512724297390740, 6.121127159803966933, 1.599625672291270506 ) ) ;
#82857 = CARTESIAN_POINT ( 'NONE',  ( 1.843539612419922813, 2.497715572767779335, -2.492262248206851272 ) ) ;
#82856 = CARTESIAN_POINT ( 'NONE',  ( -6.970300371201519241, 7.304640985922785212, 0.7216878364870317197 ) ) ;
#82859 = CARTESIAN_POINT ( 'NONE',  ( 8.132193210098487057, 8.381980254736715708, 1.040834085586084257E-14 ) ) ;
#82858 = CARTESIAN_POINT ( 'NONE',  ( 2.431682593473180276, 0.9845738105917539729, -1.844271946693208708 ) ) ;
#82861 = CARTESIAN_POINT ( 'NONE',  ( 5.709392084686216506, 5.833581318321598985, -0.7216878364870458196 ) ) ;
#82860 = CARTESIAN_POINT ( 'NONE',  ( 6.283314124929436417, 9.417951348137970413, -1.199719254218440723 ) ) ;
#82863 = VERTEX_POINT ( 'NONE', #182133 ) ;
#82862 = CARTESIAN_POINT ( 'NONE',  ( 6.551426578739074635, -1.705833205818767295, 0.8644478841580638395 ) ) ;
#82864 = CARTESIAN_POINT ( 'NONE',  ( 4.916741810085081710, 1.523553907054091328, -1.596827639139485777 ) ) ;
#82865 = CARTESIAN_POINT ( 'NONE',  ( 1.466163881440044836, 2.173982691173735216, -0.3780781022180225159 ) ) ;
#82866 =( NAMED_UNIT ( * ) PLANE_ANGLE_UNIT ( ) SI_UNIT ( $, .RADIAN. ) );
#82867 = CARTESIAN_POINT ( 'NONE',  ( 0.5395309102857149819, -1.815710607404594557, 0.6001554849531522962 ) ) ;
#82868 = CARTESIAN_POINT ( 'NONE',  ( 11.44779963594995564, 13.40000000000000924, -3.600000000000078693 ) ) ;
#82869 = CARTESIAN_POINT ( 'NONE',  ( 3.719242722441223226, -1.824546119899137731, -0.9785211796824041519 ) ) ;
#82870 = CARTESIAN_POINT ( 'NONE',  ( -5.005985031943793295, 6.863401842066301661, -1.599625672291256295 ) ) ;
#82872 = CARTESIAN_POINT ( 'NONE',  ( 1.587033755777764510, -0.3173376132806354222, -2.138153673666403964 ) ) ;
#82871 = CARTESIAN_POINT ( 'NONE',  ( 3.619250341048967812, 3.172667246362768534, 2.500000000000000444 ) ) ;
#82873 = CARTESIAN_POINT ( 'NONE',  ( 3.474349307649237328, -2.112600797985896950, -0.5827812199917583591 ) ) ;
#82874 = DIRECTION ( 'NONE',  ( 1.000000000000000000, 0.000000000000000000, 0.000000000000000000 ) ) ;
#82875 = CARTESIAN_POINT ( 'NONE',  ( -0.7500000000000215383, 4.722916667349482012, 1.299038105676671107 ) ) ;
#82876 = COLOUR_RGB ( '', 0.40784314, 0.44705882, 0.49803922) ;
#82877 = CARTESIAN_POINT ( 'NONE',  ( 1.364683531250000303, 14.06770833367473550, -0.7879004041258355073 ) ) ;
#82878 = CARTESIAN_POINT ( 'NONE',  ( -5.842637852846353397, 5.781108681267656202, 0.7998128361456281477 ) ) ;
#82879 = PRODUCT_DEFINITION_CONTEXT ( 'detailed design', #173739, 'design' ) ;
#82880 = CARTESIAN_POINT ( 'NONE',  ( 5.766190679352209969, 1.598854145598350929, -0.6720813200297001133 ) ) ;
#82881 = CARTESIAN_POINT ( 'NONE',  ( -9.571693261567968847, 12.19006144329456731, 1.443375672974076540 ) ) ;
#82882 = CARTESIAN_POINT ( 'NONE',  ( 4.293848342403890683, -1.423947089648310849, -1.503027170334819029 ) ) ;
#82883 = CARTESIAN_POINT ( 'NONE',  ( 5.835599761872579450, 0.6139674163637841575, -2.026275392342128612 ) ) ;
#82884 = CARTESIAN_POINT ( 'NONE',  ( 5.289652487626049115, 9.323011668872403845, 0.7998128361456462443 ) ) ;
#82886 = EDGE_CURVE ( 'NONE', #210405, #68973, #67300, .T. ) ;
#82885 = CARTESIAN_POINT ( 'NONE',  ( -1.364683531249997417, 5.509375000341417916, 1.214306433183764966E-14 ) ) ;
#82887 = CARTESIAN_POINT ( 'NONE',  ( 3.221498965751792731, 0.2935017643310656177, -1.947342446911073610 ) ) ;
#82888 = CARTESIAN_POINT ( 'NONE',  ( 6.474598600699414064, -0.1057723710937721190, -2.289958182497778161 ) ) ;
#82889 = CARTESIAN_POINT ( 'NONE',  ( 2.736711336054332921, 0.2235625380298221498, 1.811883384933578256 ) ) ;
#82890 = EDGE_CURVE ( 'NONE', #111999, #66325, #101969, .T. ) ;
#82891 = CARTESIAN_POINT ( 'NONE',  ( 4.523580528814945545, 5.306540700819438960, 1.199719254218452047 ) ) ;
#82892 = CARTESIAN_POINT ( 'NONE',  ( 3.999292125906899198, 6.649295999324608353, 1.082531754730558626 ) ) ;
#82893 = CARTESIAN_POINT ( 'NONE',  ( -6.826694039680798021, 7.923230120171105284, -1.199719254218446718 ) ) ;
#82894 = CARTESIAN_POINT ( 'NONE',  ( 4.532168488718122390, 8.509556680138327778, 0.7998128361456271485 ) ) ;
#82895 = VERTEX_POINT ( 'NONE', #70500 ) ;
#82896 = ORIENTED_EDGE ( 'NONE', *, *, #105557, .F. ) ;
#82897 = CARTESIAN_POINT ( 'NONE',  ( 3.674091251731440355, 1.997487462777279621, -0.2507888908306437625 ) ) ;
#82898 = CARTESIAN_POINT ( 'NONE',  ( 4.293769791895286403, -1.349757117914761384, -1.423854091114319598 ) ) ;
#82899 = CARTESIAN_POINT ( 'NONE',  ( -5.208303565944065738, 9.228104593576741621, -0.7998128361456231517 ) ) ;
#82900 = CARTESIAN_POINT ( 'NONE',  ( -4.623494077460110319, 5.352830164246910272, 1.199719254218462483 ) ) ;
#82901 = CARTESIAN_POINT ( 'NONE',  ( -10.33323920393396200, 4.021557182957058885, -5.965898435992030180 ) ) ;
#82903 = CARTESIAN_POINT ( 'NONE',  ( 6.051566426668148146, 0.5099629880620482059, -1.694758430261036564 ) ) ;
#82902 = CARTESIAN_POINT ( 'NONE',  ( -0.006154234300160406693, -2.090381218474619995, -0.04699178559822854429 ) ) ;
#82904 = CARTESIAN_POINT ( 'NONE',  ( 10.99976946526262900, -5.360092950639649523, -0.08269815893117112016 ) ) ;
#82905 = CARTESIAN_POINT ( 'NONE',  ( 1.342011898504836820, 2.189069585219292957, 0.1046993245200772138 ) ) ;
#82906 = CARTESIAN_POINT ( 'NONE',  ( 0.8193799409778947940, 1.038239828973979373, -1.396697621350863505 ) ) ;
#82907 = CARTESIAN_POINT ( 'NONE',  ( 6.582647274634798151, 7.638508894284114170, 1.199719254218462483 ) ) ;
#82908 = DIRECTION ( 'NONE',  ( -0.000000000000000000, 0.000000000000000000, -1.000000000000000000 ) ) ;
#82909 = CARTESIAN_POINT ( 'NONE',  ( 1.048929499675733235, -1.357256335890437926, -1.064349854222715885 ) ) ;
#82910 = CARTESIAN_POINT ( 'NONE',  ( 1.072081722297711259, 1.739511735661619429, -1.502347287396257114 ) ) ;
#82911 = CARTESIAN_POINT ( 'NONE',  ( 0.2928600448571066495, 1.818678932476354149, -1.222557900829209121 ) ) ;
#82912 = CARTESIAN_POINT ( 'NONE',  ( 2.614145488985010424, -2.182733025630137824, 0.3247920039054427721 ) ) ;
#82913 = CARTESIAN_POINT ( 'NONE',  ( 1.604584692665763423, 2.168457688117795712, 0.1093331725631509210 ) ) ;
#82914 = CARTESIAN_POINT ( 'NONE',  ( 1.150196859685074235, 3.145291321728038714, -0.7750000000000022427 ) ) ;
#82915 = CARTESIAN_POINT ( 'NONE',  ( 1.833370464255643206, -1.703966518588348578, -1.256690760101538240 ) ) ;
#82916 = CARTESIAN_POINT ( 'NONE',  ( 6.727182134110236689, 0.5535242275785922095, 2.340336476220133743 ) ) ;
#82917 = CARTESIAN_POINT ( 'NONE',  ( 5.649420354817641154, -1.518837414639911065, -1.184835060848010713 ) ) ;
#82918 = VERTEX_POINT ( 'NONE', #33763 ) ;
#82920 = CARTESIAN_POINT ( 'NONE',  ( -1.364683531250012516, 0.5927083336747520637, 0.7879004041258379498 ) ) ;
#82919 = CARTESIAN_POINT ( 'NONE',  ( 2.261634143469380742, 2.247403939606710477, -0.4510662058269006569 ) ) ;
#82921 = CARTESIAN_POINT ( 'NONE',  ( 4.033714395265605823, 4.664753868353354704, -1.199719254218446718 ) ) ;
#82922 = CARTESIAN_POINT ( 'NONE',  ( 5.678167406024951624, 5.518950149984223508, 0.7998128361456341429 ) ) ;
#82923 = CARTESIAN_POINT ( 'NONE',  ( 4.811300260135710438, 1.847242992945047568, -1.233362022257722845 ) ) ;
#82924 = CARTESIAN_POINT ( 'NONE',  ( -6.724481002698115439, 10.78905223654906109, -0.7216878364870267237 ) ) ;
#82925 = CARTESIAN_POINT ( 'NONE',  ( -0.02903434592766130848, -5.609732095436329224, -10.94445979172680694 ) ) ;
#82926 = CARTESIAN_POINT ( 'NONE',  ( 6.155038550924155416, 6.283225852274053835, 0.7216878364870317197 ) ) ;
#82927 = B_SPLINE_CURVE_WITH_KNOTS ( 'NONE', 3,
 ( #7959, #154235, #75116, #39411 ),
 .UNSPECIFIED., .F., .F.,
 ( 4, 4 ),
 ( 0.000000000000000000, 0.0003462261082409072736 ),
 .UNSPECIFIED. ) ;
#82928 = CARTESIAN_POINT ( 'NONE',  ( -7.836249598574384301, 8.244638741199329601, 1.040834085586084257E-14 ) ) ;
#82929 = CARTESIAN_POINT ( 'NONE',  ( 5.234856708652233515, 6.240325927249993576, 1.082531754730549078 ) ) ;
#82930 = ORIENTED_EDGE ( 'NONE', *, *, #155535, .T. ) ;
#82931 = CARTESIAN_POINT ( 'NONE',  ( 2.936172824561166905, -1.650081981912490336, -1.158688413653415239 ) ) ;
#82933 = CARTESIAN_POINT ( 'NONE',  ( 1.586864402838471522, 1.986712475098152408, 0.5538950855334312529 ) ) ;
#82932 = CARTESIAN_POINT ( 'NONE',  ( 5.991813822235618758, 9.077867661661846554, 1.199719254218462483 ) ) ;
#82934 = CARTESIAN_POINT ( 'NONE',  ( 6.883263157960400669, 0.001763689368145522022, 1.846037217754382009 ) ) ;
#82935 = CARTESIAN_POINT ( 'NONE',  ( 4.787437638956922648, 6.678706226906775179, -1.443375672974068769 ) ) ;
#82936 = CARTESIAN_POINT ( 'NONE',  ( -7.626074735689159390, -6.442483420751607959, -8.280982046698074583 ) ) ;
#82937 = CARTESIAN_POINT ( 'NONE',  ( -0.6823417656250212460, 4.051041667008085767, 1.181850606188767472 ) ) ;
#82938 = CARTESIAN_POINT ( 'NONE',  ( 4.207102436150745639, -0.3756362130699179014, 2.158856393654845274 ) ) ;
#82939 = CARTESIAN_POINT ( 'NONE',  ( 1.670546294658280084, 1.392546765991018454, 1.458555661489918442 ) ) ;
#82940 = CARTESIAN_POINT ( 'NONE',  ( 1.012948470060770934, -1.796336717620912626, 0.4034172393945419377 ) ) ;
#82941 = CARTESIAN_POINT ( 'NONE',  ( 4.136529068399773301, -1.600833271991594531, 0.9093273525555561898 ) ) ;
#82942 = CARTESIAN_POINT ( 'NONE',  ( 6.259060471003163428, 10.45398764947904624, -0.7998128361456291469 ) ) ;
#82943 =( NAMED_UNIT ( * ) SI_UNIT ( $, .STERADIAN. ) SOLID_ANGLE_UNIT ( ) );
#82944 = CARTESIAN_POINT ( 'NONE',  ( 5.315394819225006451, -0.2661953434012730435, 1.805952802178517613 ) ) ;
#82945 = CARTESIAN_POINT ( 'NONE',  ( 5.959611329766300258, -1.915599147091971544, -0.6298778581111733610 ) ) ;
#82946 = CARTESIAN_POINT ( 'NONE',  ( -9.840520565420403543, 10.37502883594562597, 1.040834085586084257E-14 ) ) ;
#82948 = CARTESIAN_POINT ( 'NONE',  ( -5.769876891067536206, 8.889217585290882795, 1.199719254218454489 ) ) ;
#82947 = CARTESIAN_POINT ( 'NONE',  ( 4.206154751832458238, -2.256696944984788011, 0.1629611055770207317 ) ) ;
#82949 = CARTESIAN_POINT ( 'NONE',  ( 0.3289212212809545788, 2.016005455721520345, 0.6092940615431781115 ) ) ;
#82950 = CARTESIAN_POINT ( 'NONE',  ( 0.4634916963840206017, 7.369626292149110469, -4.459501722865408802 ) ) ;
#82951 = CARTESIAN_POINT ( 'NONE',  ( 5.213363469605923228, -1.747142239327776903, -1.110534646669825376 ) ) ;
#82952 = CARTESIAN_POINT ( 'NONE',  ( 9.565441069641300587, 11.11843498845840905, -1.199719254218440723 ) ) ;
#82953 = CARTESIAN_POINT ( 'NONE',  ( 4.542476715900265916, 4.951051008190067826, -0.8264431066547142102 ) ) ;
#82954 = PRODUCT_CONTEXT ( 'NONE', #201209, 'mechanical' ) ;
#82955 = CARTESIAN_POINT ( 'NONE',  ( -7.232384877886063990, 10.52520055992070525, -1.199719254218446718 ) ) ;
#82956 =( NAMED_UNIT ( * ) SI_UNIT ( $, .STERADIAN. ) SOLID_ANGLE_UNIT ( ) );
#82957 = CARTESIAN_POINT ( 'NONE',  ( 6.176621499477501054, 9.363752961769195693, -1.199719254218452047 ) ) ;
#82958 = CARTESIAN_POINT ( 'NONE',  ( 4.731797659388218946, 6.802130194288283249, -1.238660871931380303 ) ) ;
#82959 = CARTESIAN_POINT ( 'NONE',  ( -3.789667630219657912, 4.380032642466370696, 1.199719254218462483 ) ) ;
#82961 = CARTESIAN_POINT ( 'NONE',  ( 1.916566064170255324, -2.220770990188126959, 0.06023022952456217466 ) ) ;
#82960 = CARTESIAN_POINT ( 'NONE',  ( 1.125412309253082332, 1.872817075645373697, 0.9946839901537674056 ) ) ;
#82962 = CYLINDRICAL_SURFACE ( 'NONE', #75086, 0.08000000000000020983 ) ;
#82964 = AXIS2_PLACEMENT_3D ( 'NONE', #190403, #75606, #108174 ) ;
#82963 = CARTESIAN_POINT ( 'NONE',  ( -8.100070429521727178, 8.414780020722290033, 0.7998128361456341429 ) ) ;
#82965 = CARTESIAN_POINT ( 'NONE',  ( 5.262536180398716290, 9.291375977107183104, -0.7998128361456291469 ) ) ;
#82966 = CARTESIAN_POINT ( 'NONE',  ( 3.420314466093795414, 0.8798059112791326575, 1.753580237611163994 ) ) ;
#82967 = CARTESIAN_POINT ( 'NONE',  ( 5.178324605415663306, 8.128796908705222535, 1.199719254218462483 ) ) ;
#82968 = CARTESIAN_POINT ( 'NONE',  ( -4.137838753588869878, 7.456630865025390520, 0.6858938789830407723 ) ) ;
#82969 = CARTESIAN_POINT ( 'NONE',  ( 5.118366684358879759, 5.930181538962194132, 1.199719254218462483 ) ) ;
#82970 = CARTESIAN_POINT ( 'NONE',  ( -5.966997003790228682, 8.054858819212300958, -1.443375672974066548 ) ) ;
#82971 = CARTESIAN_POINT ( 'NONE',  ( -8.242994207428740339, 9.679543332497402730, 1.082531754730558626 ) ) ;
#82972 = CARTESIAN_POINT ( 'NONE',  ( 2.707414796094851361, 1.816601298730673220, -1.093838055662835096 ) ) ;
#82973 = CARTESIAN_POINT ( 'NONE',  ( -5.641074431737709283, 8.738948049406083385, -1.199719254218452047 ) ) ;
#82974 = CARTESIAN_POINT ( 'NONE',  ( 4.123457186961496213, 0.2424046295769199388, -1.946780420294342617 ) ) ;
#82975 = CARTESIAN_POINT ( 'NONE',  ( 3.221700144506876917, -2.083771231579465866, 0.5749860669421112958 ) ) ;
#82976 = CARTESIAN_POINT ( 'NONE',  ( 2.577489280727011334, -0.9446877197298313433, 1.580272903027237552 ) ) ;
#82977 = CARTESIAN_POINT ( 'NONE',  ( -4.015218494013213402, 7.625434522713817387, 0.07065147036973244699 ) ) ;
#82978 = CARTESIAN_POINT ( 'NONE',  ( -1.364683531250000748, -0.6781249996585803075, 0.000000000000000000 ) ) ;
#82979 = CARTESIAN_POINT ( 'NONE',  ( 4.417713501739753745, 1.067903927642421591, -1.374066674465204363 ) ) ;
#82980 = CARTESIAN_POINT ( 'NONE',  ( -8.752560982291628378, 15.99999996917861189, -9.356054898117346141 ) ) ;
#82981 = CARTESIAN_POINT ( 'NONE',  ( 5.029711800989886683, 4.970344644017389513, 1.040834085586084257E-14 ) ) ;
#82982 = FACE_OUTER_BOUND ( 'NONE', #149252, .T. ) ;
#82983 = CARTESIAN_POINT ( 'NONE',  ( 1.903414394802248166, 1.797162532295241366, 1.201017911493490020 ) ) ;
#82984 = CARTESIAN_POINT ( 'NONE',  ( 4.903672622533055581, 0.3418847601762939337, 1.986741992616162245 ) ) ;
#82985 = CARTESIAN_POINT ( 'NONE',  ( 0.7500000000000006661, 12.94791666734946389, -1.299038105676657340 ) ) ;
#82986 = CARTESIAN_POINT ( 'NONE',  ( 1.270647086845246188, -1.370953960119488668, 1.671340013135722558 ) ) ;
#82987 = CARTESIAN_POINT ( 'NONE',  ( 3.942224353883512222, 1.961846943226858597, 0.1946112770482635312 ) ) ;
#82988 = CARTESIAN_POINT ( 'NONE',  ( 2.477749938138404051, 1.209727786519874559, 1.556487202666415604 ) ) ;
#82989 = CARTESIAN_POINT ( 'NONE',  ( 10.39230484541330135, 3.038454817776198968, 5.999999999999906741 ) ) ;
#82990 = CARTESIAN_POINT ( 'NONE',  ( 3.685046248344743258, 1.408799512439436352, 1.336988689110546913 ) ) ;
#82993 = ORIENTED_EDGE ( 'NONE', *, *, #43007, .F. ) ;
#82992 = CARTESIAN_POINT ( 'NONE',  ( -3.294361253650757604, -0.1042918288308124219, 0.000000000000000000 ) ) ;
#82991 = CARTESIAN_POINT ( 'NONE',  ( -9.042925270190641740, 11.57316545335434199, 1.443375672974064550 ) ) ;
#82994 = CARTESIAN_POINT ( 'NONE',  ( -4.678972410047611774, 5.591794245544547515, 1.082531754730549078 ) ) ;
#82995 = CARTESIAN_POINT ( 'NONE',  ( 4.923546060418115822, 5.773167154356443120, -1.199719254218452047 ) ) ;
#82996 = CARTESIAN_POINT ( 'NONE',  ( -4.457598643843001973, 8.422558527783969851, 0.000000000000000000 ) ) ;
#82997 = CARTESIAN_POINT ( 'NONE',  ( -8.961576348508641487, 11.47825837805867799, -1.443375672974058777 ) ) ;
#82998 = CARTESIAN_POINT ( 'NONE',  ( 1.641937377912294771, -1.598774535768614280, -1.521335986861327427 ) ) ;
#82999 = CARTESIAN_POINT ( 'NONE',  ( -3.285556943749998737, -2.880208332855377584, 1.896917185911908499 ) ) ;
#83000 = CARTESIAN_POINT ( 'NONE',  ( 5.330891710049517229, -1.845885424482188286, -0.6645199359083459045 ) ) ;
#83001 = ORIENTED_EDGE ( 'NONE', *, *, #21559, .T. ) ;
#83002 = CARTESIAN_POINT ( 'NONE',  ( 3.696581757058306383, 1.494387559712303526, -1.500228622805776624 ) ) ;
#83003 = CARTESIAN_POINT ( 'NONE',  ( -1.402160292154681736E-14, 2.368750000682818602, -1.732050807568863648 ) ) ;
#83005 = CARTESIAN_POINT ( 'NONE',  ( -5.904739593951539689, 6.847616600153594746, 1.199719254218450271 ) ) ;
#83004 = CARTESIAN_POINT ( 'NONE',  ( 0.07459516483345089710, 7.629137130509094256, -2.355503875070711572 ) ) ;
#83006 = CARTESIAN_POINT ( 'NONE',  ( 3.837712106225504183, 1.832433245109680531, 0.1787696065849928018 ) ) ;
#83007 = VERTEX_POINT ( 'NONE', #38040 ) ;
#83008 = UNCERTAINTY_MEASURE_WITH_UNIT (LENGTH_MEASURE( 1.000000000000000082E-05 ), #206182, 'distance_accuracy_value', 'NONE');
#83009 = CARTESIAN_POINT ( 'NONE',  ( -6.997979842947967377, 11.31606025008131233, -0.7998128361456291469 ) ) ;
#83010 = CARTESIAN_POINT ( 'NONE',  ( 5.010073305087408002, -0.7609581946756528437, 1.979555329295646260 ) ) ;
#83011 = DIRECTION ( 'NONE',  ( 0.000000000000000000, 0.000000000000000000, 1.000000000000000000 ) ) ;
#83012 = CARTESIAN_POINT ( 'NONE',  ( 5.473741331615251227, 7.409117525016355010, -1.599625672291262513 ) ) ;
#83013 = EDGE_CURVE ( 'NONE', #116397, #60282, #1240, .T. ) ;
#83014 = ORIENTED_EDGE ( 'NONE', *, *, #88762, .F. ) ;
#83015 = CARTESIAN_POINT ( 'NONE',  ( 5.395800779767854216, -0.7457615368846971515, 1.921284171288279996 ) ) ;
#83018 = CARTESIAN_POINT ( 'NONE',  ( 1.997363575765517485, -1.840834563946552649, 0.04656924640939614363 ) ) ;
#83017 = CARTESIAN_POINT ( 'NONE',  ( 0.9767415019392856612, 1.717539547389279830, 0.7171521658363362306 ) ) ;
#83016 = CARTESIAN_POINT ( 'NONE',  ( 4.082413651490639062, 7.776916670132135501, 0.000000000000000000 ) ) ;
#83019 = CARTESIAN_POINT ( 'NONE',  ( 6.936968151686458306, 11.24487994360957188, 0.7998128361456462443 ) ) ;
#83020 = CARTESIAN_POINT ( 'NONE',  ( -6.420668264523499147, 9.648474187656182366, 1.199719254218452935 ) ) ;
#83021 = CARTESIAN_POINT ( 'NONE',  ( -1.013809028830076341E-14, -7.550885189219946447, -9.573337995800475397 ) ) ;
#83022 = CARTESIAN_POINT ( 'NONE',  ( 2.368051099418837069, 2.164043333312406503, -0.4318774905316472013 ) ) ;
#83023 = CARTESIAN_POINT ( 'NONE',  ( 5.149841461411730492, 0.7164311094934887603, -2.146032026599023812 ) ) ;
#83024 = CARTESIAN_POINT ( 'NONE',  ( -7.727784370109414880, 8.118095974656867497, 0.7216878364870578100 ) ) ;
#83025 = CARTESIAN_POINT ( 'NONE',  ( 4.957183922012514898, -1.549878356133486124, 0.9377188026478706639 ) ) ;
#83026 = CARTESIAN_POINT ( 'NONE',  ( 4.997249278368244951, -0.2745004324337502744, 1.895803710022869959 ) ) ;
#83027 = ADVANCED_FACE ( 'NONE', ( #16430 ), #197222, .T. ) ;
#83028 = CARTESIAN_POINT ( 'NONE',  ( 1.084637062511527361, 3.088621193390831632, -1.105835307554789759 ) ) ;
#83029 = STYLED_ITEM ( 'NONE', ( #29630 ), #162104 ) ;
#83030 = CARTESIAN_POINT ( 'NONE',  ( 5.032044620589739559, 0.9611010790777809731, -1.604743002217932313 ) ) ;
#83031 = EDGE_CURVE ( 'NONE', #192043, #163067, #85711, .T. ) ;
#83032 = CARTESIAN_POINT ( 'NONE',  ( 4.668306603206507255, -0.7948602423475581435, -1.682893250223691517 ) ) ;
#83033 = CARTESIAN_POINT ( 'NONE',  ( -1.364683531249997417, 5.009375000341425022, 1.214306433183764966E-14 ) ) ;
#83034 = CARTESIAN_POINT ( 'NONE',  ( 6.104346055523492964, -0.6409971714030155976, -1.649885601521252410 ) ) ;
#83035 = CARTESIAN_POINT ( 'NONE',  ( -0.2409995289980038091, -0.004801160710915519658, -2.000252362011435636 ) ) ;
#83037 = CARTESIAN_POINT ( 'NONE',  ( 2.701903229428818776, -0.6601559168808753819, 2.000001591751764618 ) ) ;
#83036 = CARTESIAN_POINT ( 'NONE',  ( -4.406036734316906234, 4.242723732898890709, -0.7216878364870207285 ) ) ;
#83038 = CARTESIAN_POINT ( 'NONE',  ( 7.899597058256738968, 12.36794700127490820, 1.040834085586084257E-14 ) ) ;
#83040 = CARTESIAN_POINT ( 'NONE',  ( -10.32861409551237486, 10.94447128771960287, 1.040834085586084257E-14 ) ) ;
#83039 = CARTESIAN_POINT ( 'NONE',  ( -0.7500000000000249800, -1.058333333333314030, 1.299038105676659116 ) ) ;
#83041 = FACE_OUTER_BOUND ( 'NONE', #74747, .T. ) ;
#83042 = CARTESIAN_POINT ( 'NONE',  ( 2.373312353838610722, -1.759458965525468210, -0.9916931515873882441 ) ) ;
#83043 = CARTESIAN_POINT ( 'NONE',  ( -0.6823417656250212460, 2.551041667008084435, 1.181850606188767472 ) ) ;
#83044 = CARTESIAN_POINT ( 'NONE',  ( 5.196852952739813070, 4.957416621151553571, -0.7998128361456221525 ) ) ;
#83045 = ORIENTED_EDGE ( 'NONE', *, *, #103113, .T. ) ;
#83046 = CARTESIAN_POINT ( 'NONE',  ( 2.038557401052975671, 2.137775048120754029, 0.3193135401893046899 ) ) ;
#83047 = CARTESIAN_POINT ( 'NONE',  ( 6.890000000000008562, 1.260399741928097672, 2.114076522472335462 ) ) ;
#83050 = FACE_OUTER_BOUND ( 'NONE', #161337, .T. ) ;
#83049 = CARTESIAN_POINT ( 'NONE',  ( -5.951324661304710162, 4.742844146918499426, -2.438848701833497667 ) ) ;
#83048 = CARTESIAN_POINT ( 'NONE',  ( 4.248501033035879004, 6.049946853332221153, -1.599625672291273171 ) ) ;
#83051 = CARTESIAN_POINT ( 'NONE',  ( 8.554831740098642001, 12.92446143018304916, 0.7216878364870438212 ) ) ;
#83052 = CARTESIAN_POINT ( 'NONE',  ( -2.279984679289828176, 5.601133616484927025, -0.06592222766762731445 ) ) ;
#83053 = CARTESIAN_POINT ( 'NONE',  ( -6.046573322014817897, 9.998159942418544333, 0.7216878364870458196 ) ) ;
#83054 = CARTESIAN_POINT ( 'NONE',  ( 1.048660896456204528, -1.724490848714568259, 1.352309724062021878 ) ) ;
#83055 = CARTESIAN_POINT ( 'NONE',  ( 0.1465803529717422671, 8.209140712741676893, 2.038183922479804178 ) ) ;
#83056 = CARTESIAN_POINT ( 'NONE',  ( 1.675094374204841419, -2.148779999652763895, -0.7084808733194192243 ) ) ;
#83057 = CARTESIAN_POINT ( 'NONE',  ( -8.290974629956718189, 9.631557475493025322, -1.199719254218446718 ) ) ;
#83058 = CARTESIAN_POINT ( 'NONE',  ( -4.894130264408873110, 5.772535398974209642, -1.082531754730543971 ) ) ;
#83059 = CARTESIAN_POINT ( 'NONE',  ( -1.364683531250012516, 3.592708333674750509, 0.7879004041258379498 ) ) ;
#83060 = CARTESIAN_POINT ( 'NONE',  ( 4.615647837050825153, 8.347533190886938570, 0.2882115401751338402 ) ) ;
#83061 = CARTESIAN_POINT ( 'NONE',  ( -1.500000000000001110, 11.52083333333333393, 0.8660254037844419273 ) ) ;
#83062 = CARTESIAN_POINT ( 'NONE',  ( 5.063044020060520900, 4.871582543017558109, 0.7998128361456352531 ) ) ;
#83063 = CARTESIAN_POINT ( 'NONE',  ( 3.022431051408695613, 1.665045927894950095, 0.5999815234925524043 ) ) ;
#83064 =( GEOMETRIC_REPRESENTATION_CONTEXT ( 3 ) GLOBAL_UNCERTAINTY_ASSIGNED_CONTEXT ( ( #15737 ) ) GLOBAL_UNIT_ASSIGNED_CONTEXT ( ( #142410, #45963, #182320 ) ) REPRESENTATION_CONTEXT ( 'NONE', 'WORKASPACE' ) );
#83065 = CARTESIAN_POINT ( 'NONE',  ( 6.176841753231244958, -2.093540797633717254, -0.6980159708611932690 ) ) ;
#83066 = CARTESIAN_POINT ( 'NONE',  ( -0.6823417656250039265, 15.38020833367473372, -1.181850606188755259 ) ) ;
#83067 = CARTESIAN_POINT ( 'NONE',  ( -4.274563570058511175, 8.209017608368725405, 0.000000000000000000 ) ) ;
#83068 = CARTESIAN_POINT ( 'NONE',  ( 4.868767636308747093, -0.2496254991312534810, -2.000855965115163837 ) ) ;
#83070 = ORIENTED_EDGE ( 'NONE', *, *, #52529, .T. ) ;
#83069 = CARTESIAN_POINT ( 'NONE',  ( 4.939644399817936460, -1.717766137778716118, 0.5755910463909068575 ) ) ;
#83071 = CARTESIAN_POINT ( 'NONE',  ( 2.852262661058731386, 0.6285613048715790185, 1.762029509812724992 ) ) ;
#83072 = CARTESIAN_POINT ( 'NONE',  ( 3.010663864534826928, 0.6931938328994196041, 1.950912564768356505 ) ) ;
#83073 = DIRECTION ( 'NONE',  ( -1.000000000000000000, 7.771561172376097755E-16, 4.440892098500627148E-16 ) ) ;
#83074 = CARTESIAN_POINT ( 'NONE',  ( 2.338023529656753752, -1.104205016203146705, -1.561194055274425452 ) ) ;
#83075 = CARTESIAN_POINT ( 'NONE',  ( -1.438722645073123196, 7.870286565763556119, 3.684014302713788602 ) ) ;
#83076 = CARTESIAN_POINT ( 'NONE',  ( -9.812680342707254866, 4.108039100808300148, -6.337802944732694677 ) ) ;
#83077 = DIRECTION ( 'NONE',  ( 0.000000000000000000, 0.000000000000000000, 1.000000000000000000 ) ) ;
#83078 = CARTESIAN_POINT ( 'NONE',  ( -0.6823417656249969321, 4.030208333674754506, -1.181850606188749264 ) ) ;
#83079 = CARTESIAN_POINT ( 'NONE',  ( 1.371198541116287917, -1.641758494746584418, -0.9804709962101464393 ) ) ;
#83080 = CARTESIAN_POINT ( 'NONE',  ( 4.895902868310594513, 8.725987423088758632, 0.000000000000000000 ) ) ;
#83081 = CARTESIAN_POINT ( 'NONE',  ( 2.523818479427087702, 1.924573107942130656, -0.3798230296482503210 ) ) ;
#83082 = DIRECTION ( 'NONE',  ( 0.000000000000000000, -1.000000000000000000, 0.000000000000000000 ) ) ;
#83083 = EDGE_CURVE ( 'NONE', #211313, #95167, #156899, .T. ) ;
#83084 = CARTESIAN_POINT ( 'NONE',  ( -4.472210567661380587, 6.310941310395290493, 1.599625672291270506 ) ) ;
#83085 = CARTESIAN_POINT ( 'NONE',  ( 5.607717026683647354, 1.607092460389969446, 1.383685132418293495 ) ) ;
#83087 = DIRECTION ( 'NONE',  ( 0.000000000000000000, 1.000000000000000000, 0.000000000000000000 ) ) ;
#83086 = CARTESIAN_POINT ( 'NONE',  ( 8.829384350997564468, 11.32403438096243775, 1.599625672291281386 ) ) ;
#83088 = CARTESIAN_POINT ( 'NONE',  ( 6.485619883616900339, 1.357675630217811014, 1.429558606944077326 ) ) ;
#83089 = CARTESIAN_POINT ( 'NONE',  ( 1.364683531249990311, 2.884375000341422801, 1.214306433183764966E-14 ) ) ;
#83090 = CARTESIAN_POINT ( 'NONE',  ( 2.267839937129061401, 0.5327387516648759425, -1.941401684534331817 ) ) ;
#83092 = CARTESIAN_POINT ( 'NONE',  ( 1.616979318382205433, 0.2114564432566454211, 2.106663336370690143 ) ) ;
#83091 = CARTESIAN_POINT ( 'NONE',  ( -8.026063749610063525, 8.466088584074293877, -0.7216878364870278340 ) ) ;
#83093 = CARTESIAN_POINT ( 'NONE',  ( 1.492392680117907711, 7.408236896935762594, 4.235501437639942246 ) ) ;
#83094 = CARTESIAN_POINT ( 'NONE',  ( 2.998552181135270001, 2.054425100943928051, 0.2560010573490826835 ) ) ;
#83095 = CARTESIAN_POINT ( 'NONE',  ( 3.067887898442204442, 6.801229324816399746, 0.7998128361456271485 ) ) ;
#83096 = CARTESIAN_POINT ( 'NONE',  ( 4.386945222473598527, 7.275797305264619652, -1.199719254218452047 ) ) ;
#83097 = ORIENTED_EDGE ( 'NONE', *, *, #55534, .F. ) ;
#83099 = CARTESIAN_POINT ( 'NONE',  ( 4.976006071415387311, 5.764094157194782575, 1.199719254218462483 ) ) ;
#83098 = CARTESIAN_POINT ( 'NONE',  ( 5.701146808890831252, -0.5089937999912234057, 2.027600676370949095 ) ) ;
#83101 = EDGE_LOOP ( 'NONE', ( #46479, #140019, #31812, #208324 ) ) ;
#83100 = CARTESIAN_POINT ( 'NONE',  ( 3.926616521958687045, 1.733384925006593136, 0.5729815612169064654 ) ) ;
#83102 = CARTESIAN_POINT ( 'NONE',  ( 8.218213668177886788, 12.73966637951625813, 0.7998128361456462443 ) ) ;
#83103 = CARTESIAN_POINT ( 'NONE',  ( 6.890000000000008562, 2.965158640989657535, 2.452917560796506802 ) ) ;
#83104 = CARTESIAN_POINT ( 'NONE',  ( 10.18930308530835660, 13.31154919269470760, 7.183432580020707725 ) ) ;
#83105 = CARTESIAN_POINT ( 'NONE',  ( 5.280388062626482970, -1.229865305990836877, 1.832093573602276759 ) ) ;
#83106 = CARTESIAN_POINT ( 'NONE',  ( 1.364683531250000748, 10.56770833367473195, -0.7879004041258355073 ) ) ;
#83107 = ADVANCED_FACE ( 'NONE', ( #183213 ), #20089, .T. ) ;
#83108 = ORIENTED_EDGE ( 'NONE', *, *, #100532, .F. ) ;
#83109 = CARTESIAN_POINT ( 'NONE',  ( 4.055252259792781366, -1.662250449027093735, 0.9452659147194606426 ) ) ;
#83110 = CARTESIAN_POINT ( 'NONE',  ( -8.513630394377489807, 12.01998699582738972, -1.199719254218446718 ) ) ;
#83111 = CARTESIAN_POINT ( 'NONE',  ( 7.365103760721646076, 9.615707025640515937, 1.599625672291281386 ) ) ;
#83112 = CARTESIAN_POINT ( 'NONE',  ( -0.6801582343750368631, 2.130208333674714183, -1.178068619123862515 ) ) ;
#83113 = CARTESIAN_POINT ( 'NONE',  ( 4.812781342726866640, 5.677628323678546529, 1.082531754730560403 ) ) ;
#83114 = CARTESIAN_POINT ( 'NONE',  ( 3.188928480291414846, 8.980740528189164351, -2.451733079074511767 ) ) ;
#83115 = CARTESIAN_POINT ( 'NONE',  ( 8.790438134619865451, 13.29428800202395955, -8.101059483297394337 ) ) ;
#83116 = CARTESIAN_POINT ( 'NONE',  ( -0.05938221139379848412, -1.422385081007140117, -1.168950373246782526 ) ) ;
#83117 = VERTEX_POINT ( 'NONE', #106288 ) ;
#83118 = ORIENTED_EDGE ( 'NONE', *, *, #118396, .F. ) ;
#83119 = CARTESIAN_POINT ( 'NONE',  ( 5.724925646405265134, 7.336609705370862322, 1.269948841093468506 ) ) ;
#83120 = CARTESIAN_POINT ( 'NONE',  ( 4.991395955090764502, 1.385047395102714685, 1.257364466828891914 ) ) ;
#83121 = CARTESIAN_POINT ( 'NONE',  ( 5.820193082016415609, 10.01225203898631655, 0.000000000000000000 ) ) ;
#83122 = CARTESIAN_POINT ( 'NONE',  ( 1.734723475976807094E-15, 15.00041888085534758, 12.17999951260719982 ) ) ;
#83123 = CARTESIAN_POINT ( 'NONE',  ( -7.592202833972775622, 8.920286730132099606, 1.082531754730558626 ) ) ;
#83124 = CARTESIAN_POINT ( 'NONE',  ( 5.009901455449552010, 5.803638771901306725, -1.199719254218452047 ) ) ;
#83125 = CARTESIAN_POINT ( 'NONE',  ( 1.569134323820881027, 1.734487354001874371, 0.9329377246683704383 ) ) ;
#83126 = CARTESIAN_POINT ( 'NONE',  ( 2.671500097371417137, 1.427951006967288272, 1.423949442620517702 ) ) ;
#83127 = CARTESIAN_POINT ( 'NONE',  ( -7.832860060393135093, 10.16142270859057462, 1.599625672291295375 ) ) ;
#83128 = CARTESIAN_POINT ( 'NONE',  ( 7.191674137406095291, 7.354984346587396082, 0.000000000000000000 ) ) ;
#83130 = EDGE_CURVE ( 'NONE', #108528, #50089, #4883, .T. ) ;
#83129 = DIRECTION ( 'NONE',  ( 0.000000000000000000, 0.000000000000000000, -1.000000000000000000 ) ) ;
#83131 = CARTESIAN_POINT ( 'NONE',  ( 2.783357461837578484, 1.550338952211056220, 1.549093164327268068 ) ) ;
#83132 = CARTESIAN_POINT ( 'NONE',  ( 6.639320575229281651, -0.0007625845807879281287, 2.103388539994067497 ) ) ;
#83133 = CARTESIAN_POINT ( 'NONE',  ( -3.273404022695637572, 5.906389562198459231, 1.199719254218462483 ) ) ;
#83134 = CARTESIAN_POINT ( 'NONE',  ( 1.123270288250311610, 3.110197346350006331, 0.7749999999993734123 ) ) ;
#83135 = CARTESIAN_POINT ( 'NONE',  ( -0.08058608058609216529, -8.270571484000473816, -10.99970480893080271 ) ) ;
#83136 = EDGE_CURVE ( 'NONE', #23505, #21255, #70414, .T. ) ;
#83137 = CARTESIAN_POINT ( 'NONE',  ( 3.770576118376296471, 7.413106214832098750, 0.7216878364870257245 ) ) ;
#83138 = CARTESIAN_POINT ( 'NONE',  ( 7.086107841436786181, 11.41887624831828418, 1.040834085586084257E-14 ) ) ;
#83139 = CARTESIAN_POINT ( 'NONE',  ( 4.858757509019037357, 5.629766575900002401, 2.499999999999999556 ) ) ;
#83140 = CARTESIAN_POINT ( 'NONE',  ( 6.156811154381533591, 9.236677875870187293, -1.082531754730548412 ) ) ;
#83141 = ORIENTED_EDGE ( 'NONE', *, *, #65438, .T. ) ;
#83143 = CARTESIAN_POINT ( 'NONE',  ( 0.1881394758670457412, 1.160778376788082378, 1.644543748126830796 ) ) ;
#83142 = CARTESIAN_POINT ( 'NONE',  ( 4.599059095968327071, -0.4863373063577690059, 1.775805238918099382 ) ) ;
#83144 = CARTESIAN_POINT ( 'NONE',  ( 2.794613785990595733, -2.145299970026095071, 0.8252070097543462435 ) ) ;
#83146 = CARTESIAN_POINT ( 'NONE',  ( 0.8657744530725123289, -1.852701964455932604, 0.1747518070307155780 ) ) ;
#83145 = CARTESIAN_POINT ( 'NONE',  ( 3.606105671554957759, 4.269840040644637291, -1.082531754730543083 ) ) ;
#83147 = CARTESIAN_POINT ( 'NONE',  ( 1.001543065824772753E-15, -3.521874999522041083, 3.793834371823811669 ) ) ;
#83148 = CARTESIAN_POINT ( 'NONE',  ( -4.253507506385335368, 5.985511395581417204, 1.599625672291267398 ) ) ;
#83149 = CARTESIAN_POINT ( 'NONE',  ( 4.834190613173367623, -1.027981871586785889, -1.612434056610718480 ) ) ;
#83150 = CARTESIAN_POINT ( 'NONE',  ( -9.494787648271923786, 9.971673765939062406, 1.040834085586084257E-14 ) ) ;
#83151 = CARTESIAN_POINT ( 'NONE',  ( -6.455090533882206216, 7.663932056684933158, -1.082531754730549967 ) ) ;
#83153 = CARTESIAN_POINT ( 'NONE',  ( 2.694054421766533203, -1.865511834602461949, -0.1395888279770511053 ) ) ;
#83152 = CARTESIAN_POINT ( 'NONE',  ( 3.562131390660903563, -1.402593093800925894, 1.550658987340556294 ) ) ;
#83154 = CARTESIAN_POINT ( 'NONE',  ( 6.616015773788773480, 10.66250946948817813, -0.7216878364870267237 ) ) ;
#83155 = CARTESIAN_POINT ( 'NONE',  ( 1.364683531249988535, 5.717708333674751842, -0.7879004041258300672 ) ) ;
#83156 = CARTESIAN_POINT ( 'NONE',  ( 5.706567001488551227, 1.626822141722890303, 0.8623401093873286349 ) ) ;
#83157 = CARTESIAN_POINT ( 'NONE',  ( 3.871016551901614200, 4.474939717762034697, -1.199719254218446718 ) ) ;
#83158 = CARTESIAN_POINT ( 'NONE',  ( 11.78331023100045627, 13.87999999999998302, 1.799999999999999600 ) ) ;
#83159 = CARTESIAN_POINT ( 'NONE',  ( 5.092313435308955860, -1.712476623254995278, -0.2059198849207622417 ) ) ;
#83160 = CARTESIAN_POINT ( 'NONE',  ( -7.739006755302186846, 7.923262724141010516, 0.7998128361456462443 ) ) ;
#83161 = CARTESIAN_POINT ( 'NONE',  ( 0.5801786448705691379, -0.6264061342569470225, 1.617264071341844245 ) ) ;
#83162 = CARTESIAN_POINT ( 'NONE',  ( 6.516270054225981490, -1.036149114087565382, -1.948532232987249424 ) ) ;
#83163 = CARTESIAN_POINT ( 'NONE',  ( 1.499999999999993117, 8.604166666666664298, 0.8660254037844408170 ) ) ;
#83164 = CARTESIAN_POINT ( 'NONE',  ( 4.698188964201695406, 0.9341788774818636787, -1.959971951513925781 ) ) ;
#83165 = CARTESIAN_POINT ( 'NONE',  ( 2.894927146036041510, 1.565677646668685696, -0.9388022922067614795 ) ) ;
#83166 = CARTESIAN_POINT ( 'NONE',  ( 0.9187138386215136787, -1.424830647414500051, 1.348730089142296418 ) ) ;
#83167 = CARTESIAN_POINT ( 'NONE',  ( 5.348860635491798909, -1.915306066586830669, -0.9028416433708542632 ) ) ;
#83168 = ORIENTED_EDGE ( 'NONE', *, *, #180932, .F. ) ;
#83170 = CARTESIAN_POINT ( 'NONE',  ( -1.364683531250010295, 4.342708333674753618, 0.7879004041258379498 ) ) ;
#83169 = CARTESIAN_POINT ( 'NONE',  ( 6.198803536200695241, 1.903451089567553822, 1.277169966706873883 ) ) ;
#83171 = CARTESIAN_POINT ( 'NONE',  ( 8.914649696185335870, 10.35917838609310593, -1.199719254218446718 ) ) ;
#83172 = AXIS2_PLACEMENT_3D ( 'NONE', #39776, #155659, #44861 ) ;
#83173 = CARTESIAN_POINT ( 'NONE',  ( 1.946092837771850492, -1.387361170020007695, -1.603719225630481970 ) ) ;
#83174 = CARTESIAN_POINT ( 'NONE',  ( -5.761852096127856981, 5.824508321678349532, 0.000000000000000000 ) ) ;
#83175 = CARTESIAN_POINT ( 'NONE',  ( -5.734735788456164940, 5.792872629394710593, 0.7216878364870317197 ) ) ;
#83176 = CARTESIAN_POINT ( 'NONE',  ( 6.209878556409044847, 0.6379485578581347571, -2.075210184031409888 ) ) ;
#83178 = CARTESIAN_POINT ( 'NONE',  ( 0.7500000000000006661, 12.94791666734946389, -1.299038105676657340 ) ) ;
#83177 = CARTESIAN_POINT ( 'NONE',  ( 6.883263157960367806, 2.959656548886806071, 2.506466465954690914 ) ) ;
#83180 = ORIENTED_EDGE ( 'NONE', *, *, #121643, .T. ) ;
#83179 = CARTESIAN_POINT ( 'NONE',  ( 2.596574818557799258, -1.139633321999042659, 1.906535983277869661 ) ) ;
#83181 = CARTESIAN_POINT ( 'NONE',  ( 6.276017556857773627, 1.753032240926259311, -0.9962986157117934560 ) ) ;
#83183 = CARTESIAN_POINT ( 'NONE',  ( 4.188373618524662056, 1.107674127198258196, -1.739744320567500280 ) ) ;
#83182 = CARTESIAN_POINT ( 'NONE',  ( 4.630273154266905777, 5.360739087188218122, 1.199719254218464037 ) ) ;
#83185 = CARTESIAN_POINT ( 'NONE',  ( -3.475000000000000533, -3.529166666666667229, -2.006292185433948827 ) ) ;
#83184 = CARTESIAN_POINT ( 'NONE',  ( 5.182959862174088883, 9.268813282503625572, 0.7998128361456331437 ) ) ;
#83186 = CARTESIAN_POINT ( 'NONE',  ( 5.845500506147374153, 6.848780674373954547, 1.199719254218453823 ) ) ;
#83187 = CARTESIAN_POINT ( 'NONE',  ( 3.285556943749998737, -3.492708332855374742, -1.896917185911906500 ) ) ;
#83188 = CARTESIAN_POINT ( 'NONE',  ( 0.1331565106231363538, 0.2470099659030860484, -1.980838409567912572 ) ) ;
#83189 = CARTESIAN_POINT ( 'NONE',  ( 0.9903105584966699348, -0.5097506344743455431, -2.027405242695742515 ) ) ;
#83190 = CARTESIAN_POINT ( 'NONE',  ( 4.827609030688454261, 0.9420861819694618111, -1.581835861328761528 ) ) ;
#83192 = EDGE_LOOP ( 'NONE', ( #158505, #167312, #134263, #108015 ) ) ;
#83191 = CARTESIAN_POINT ( 'NONE',  ( 5.192936529234042808, 6.017179691316550283, -1.199719254218452047 ) ) ;
#83193 = CARTESIAN_POINT ( 'NONE',  ( 1.711479192339813382, -1.712302428074402583, 0.2063632002643790431 ) ) ;
#83194 = CARTESIAN_POINT ( 'NONE',  ( 0.4269707148552639997, -1.727061408318403712, 1.040797348915108111 ) ) ;
#83195 = CARTESIAN_POINT ( 'NONE',  ( 1.460084154473238138, -2.184713004772549372, -0.7151137612169417013 ) ) ;
#83196 = CARTESIAN_POINT ( 'NONE',  ( -5.063080299699540987, 7.994345218703034384, 1.199719254218464037 ) ) ;
#83197 = CARTESIAN_POINT ( 'NONE',  ( 1.282923566313122210, -2.207321063319432231, -0.4954982646878171582 ) ) ;
#83198 = CARTESIAN_POINT ( 'NONE',  ( 4.072956574305106159, -1.964985935830084740, -0.7583447493727160094 ) ) ;
#83199 = CARTESIAN_POINT ( 'NONE',  ( -5.307090785106547415, 5.156303768904543894, -0.7998128361456362523 ) ) ;
#83200 = CARTESIAN_POINT ( 'NONE',  ( 7.474622759835693131, 7.614814729430110951, -0.7998128361456281477 ) ) ;
#83202 = EDGE_CURVE ( 'NONE', #162782, #6739, #2564, .T. ) ;
#83201 = CARTESIAN_POINT ( 'NONE',  ( 5.438229012412886476, 7.437962829272074750, -1.443375672974078761 ) ) ;
#83203 = CARTESIAN_POINT ( 'NONE',  ( 5.718750000000003553, -0.7852924748296825630, 1.895863743164203141 ) ) ;
#83204 = CARTESIAN_POINT ( 'NONE',  ( -6.573005544526917099, 6.562927978236513304, -0.7998128361456291469 ) ) ;
#83205 = CARTESIAN_POINT ( 'NONE',  ( -1.402160292154681736E-14, 2.337500000000022560, -1.732050807568863648 ) ) ;
#83206 = CARTESIAN_POINT ( 'NONE',  ( -5.434120640978981065, 5.234228924097238611, -0.7998128361456221525 ) ) ;
#83207 = CARTESIAN_POINT ( 'NONE',  ( 4.641020947978182321, 2.126209183204033959, 0.6434571820467527292 ) ) ;
#83208 = CARTESIAN_POINT ( 'NONE',  ( 3.187623232016934871, -0.8878212517344568067, 2.003729935572157395 ) ) ;
#83209 = CARTESIAN_POINT ( 'NONE',  ( -6.410307701162927252, 6.373113827645189744, -0.7998128361456291469 ) ) ;
#83210 = CARTESIAN_POINT ( 'NONE',  ( -3.471769853551161411, 6.208092708188416076, 1.199719254218452935 ) ) ;
#83211 = CARTESIAN_POINT ( 'NONE',  ( 5.567072742743464531, -1.671543079161823542, 1.304629437388994395 ) ) ;
#83212 = CARTESIAN_POINT ( 'NONE',  ( 0.6823417656249899377, 3.176041667008085323, -1.181850606188754593 ) ) ;
#83213 = EDGE_CURVE ( 'NONE', #208229, #179210, #107366, .T. ) ;
#83214 = CARTESIAN_POINT ( 'NONE',  ( 6.889999999999967706, 0.005249217920031550542, 1.719840535937327664 ) ) ;
#83215 = CARTESIAN_POINT ( 'NONE',  ( -6.073689629242176480, 6.188318776978391611, -0.7216878364870278340 ) ) ;
#83216 = CARTESIAN_POINT ( 'NONE',  ( 5.396778611113259849, -2.069399493756381769, -0.4625044129713885011 ) ) ;
#83217 = CARTESIAN_POINT ( 'NONE',  ( -6.699137298928187434, 8.909022496873262753, 1.443375672974064550 ) ) ;
#83218 = ORIENTED_EDGE ( 'NONE', *, *, #70698, .T. ) ;
#83220 = CARTESIAN_POINT ( 'NONE',  ( 6.315313271410192719, -0.2696487299426887363, 2.144762774094311375 ) ) ;
#83219 = CARTESIAN_POINT ( 'NONE',  ( -4.828112100242291760, 6.726159765073026264, -1.443375672974066548 ) ) ;
#83221 = CARTESIAN_POINT ( 'NONE',  ( 6.193377243344257543, 6.120028293523423812, -0.7998128361456281477 ) ) ;
#83222 = DIRECTION ( 'NONE',  ( 0.000000000000000000, -1.000000000000000000, 0.000000000000000000 ) ) ;
#83223 = CARTESIAN_POINT ( 'NONE',  ( -1.364683531250012516, 2.592708333674753174, 0.7879004041258379498 ) ) ;
#83224 = CARTESIAN_POINT ( 'NONE',  ( 0.9072687458823289752, -0.7809752019604562223, -1.555474206689683836 ) ) ;
#83225 = CARTESIAN_POINT ( 'NONE',  ( 4.369805582306193870, 3.992528022312320957, 1.214306433183764966E-14 ) ) ;
#83226 = CARTESIAN_POINT ( 'NONE',  ( 3.231779075379134003, 6.036511184309971689, 7.500000000000000000 ) ) ;
#83227 = CARTESIAN_POINT ( 'NONE',  ( 1.364683531249986537, 0.2177083336747502595, -0.7879004041258309554 ) ) ;
#83228 = FACE_OUTER_BOUND ( 'NONE', #182151, .T. ) ;
#83229 = CARTESIAN_POINT ( 'NONE',  ( 4.856408821558930278, 0.8241108818672329139, 1.998647875481096126 ) ) ;
#83230 = CARTESIAN_POINT ( 'NONE',  ( -2.435661151949389147, 5.993355110582911038, 0.7998128361456341429 ) ) ;
#83231 = CARTESIAN_POINT ( 'NONE',  ( -7.063434842595444962, 8.303390740191881392, 1.082531754730549967 ) ) ;
#83232 = CARTESIAN_POINT ( 'NONE',  ( 4.856408821558930278, 0.8241108818672329139, 1.998647875481096126 ) ) ;
#83234 = ORIENTED_EDGE ( 'NONE', *, *, #32740, .T. ) ;
#83233 = CARTESIAN_POINT ( 'NONE',  ( -3.902768115887413014, 5.646591783325653147, -1.599625672291283607 ) ) ;
#83235 = CARTESIAN_POINT ( 'NONE',  ( 1.364683531249990311, 2.884375000341422801, 1.214306433183764966E-14 ) ) ;
#83236 = CARTESIAN_POINT ( 'NONE',  ( 5.430923302262330665, 0.1424395525144121211, 1.966244542718327715 ) ) ;
#83237 = CARTESIAN_POINT ( 'NONE',  ( 5.202368031388965974, -1.227288160380139548, -1.225006654371106452 ) ) ;
#83239 = CARTESIAN_POINT ( 'NONE',  ( 1.839652601550560096, 0.8350199954420146620, -2.026445374841173930 ) ) ;
#83238 = CARTESIAN_POINT ( 'NONE',  ( 1.360316468749949825, -0.9635416663252907021, -0.7853790794159282163 ) ) ;
#83240 = CARTESIAN_POINT ( 'NONE',  ( 2.450585703787050651, 2.307050653106942573, 0.05676454813420374335 ) ) ;
#83241 = CARTESIAN_POINT ( 'NONE',  ( 5.255176862235733992, -1.738700696582769378, -1.105936373271217521 ) ) ;
#83242 = CARTESIAN_POINT ( 'NONE',  ( 0.5330192132981932396, -1.372706249750287322, -1.373872859839823990 ) ) ;
#83243 = CARTESIAN_POINT ( 'NONE',  ( -6.033015167956794933, 9.982342096017511324, -0.7216878364870267237 ) ) ;
#83244 = CARTESIAN_POINT ( 'NONE',  ( -3.006876207180748217, 6.730049018344652190, -0.7998128361456481317 ) ) ;
#83245 = CARTESIAN_POINT ( 'NONE',  ( 3.834746474454188013E-15, 10.81250000000000355, 1.500000000000001554 ) ) ;
#83246 = CARTESIAN_POINT ( 'NONE',  ( 4.377262645480927361, -1.895543854172193399, -0.9507902649282941043 ) ) ;
#83247 = CARTESIAN_POINT ( 'NONE',  ( 5.526144005543697446, 7.442112546579989996, -1.248357989223557452 ) ) ;
#83248 = CARTESIAN_POINT ( 'NONE',  ( 1.389296306420295224, -0.7283806465635984662, -1.880434191983325398 ) ) ;
#83249 = CARTESIAN_POINT ( 'NONE',  ( -5.707619481228817904, 8.642344580533519505, -1.082531754730537976 ) ) ;
#83250 = EDGE_CURVE ( 'NONE', #53136, #71735, #159915, .T. ) ;
#83251 = CARTESIAN_POINT ( 'NONE',  ( 4.630015379333586978, -1.354682855507854278, -1.741961856448564383 ) ) ;
#83252 = CARTESIAN_POINT ( 'NONE',  ( 0.000000000000000000, -1.334374999522042859, -3.793834371823813001 ) ) ;
#83253 = DIRECTION ( 'NONE',  ( 0.000000000000000000, 0.000000000000000000, 1.000000000000000000 ) ) ;
#83254 = CARTESIAN_POINT ( 'NONE',  ( -11.78331023100045627, 12.29999999999998295, 1.799999999999999600 ) ) ;
#83255 = CARTESIAN_POINT ( 'NONE',  ( 0.000000000000000000, 2.817530495244580102, 1.214306433183764966E-14 ) ) ;
#83257 = DIRECTION ( 'NONE',  ( 0.000000000000000000, -1.000000000000000000, 0.000000000000000000 ) ) ;
#83256 = CARTESIAN_POINT ( 'NONE',  ( -5.645675577465527617, 7.454724071444114308, -1.341317915573495334 ) ) ;
#83258 = ORIENTED_EDGE ( 'NONE', *, *, #154305, .F. ) ;
#83259 = CARTESIAN_POINT ( 'NONE',  ( 3.661055773700711224, -1.816817347422092555, -0.9728634070030485193 ) ) ;
#83260 = CARTESIAN_POINT ( 'NONE',  ( -0.6801582343750438575, 1.932291667008062541, 1.178068619123787908 ) ) ;
#83261 = CARTESIAN_POINT ( 'NONE',  ( -4.869349725602420520, 8.832658446511480577, 1.040834085586084257E-14 ) ) ;
#83262 = CARTESIAN_POINT ( 'NONE',  ( 3.949871522956601932, -1.394395303408175080, -1.461305941245706119 ) ) ;
#83263 = CARTESIAN_POINT ( 'NONE',  ( 1.499999999999985123, -0.9541666666666493990, -0.8660254037844323793 ) ) ;
#83264 = CARTESIAN_POINT ( 'NONE',  ( 3.979481780810941949, 4.601482484822914998, 1.199719254218464037 ) ) ;
#83265 = CARTESIAN_POINT ( 'NONE',  ( 1.569287236123186213, 0.1524497474049029966, -2.055318472165644117 ) ) ;
#83266 = CARTESIAN_POINT ( 'NONE',  ( -9.508841981786559927, 15.08576114865397244, -7.212865296072072496 ) ) ;
#83267 = CARTESIAN_POINT ( 'NONE',  ( 5.005985031943777308, 6.863401842066294556, -1.599625672291256295 ) ) ;
#83268 = CARTESIAN_POINT ( 'NONE',  ( -0.2411972340276230808, 7.629137130509075604, -2.500476664557866435 ) ) ;
#83269 = CARTESIAN_POINT ( 'NONE',  ( 1.605144257462550517, -1.827384369528777031, 0.2241066044648756805 ) ) ;
#83270 = CARTESIAN_POINT ( 'NONE',  ( 0.3996046210705077595, 1.915144275937111340, -1.287252092841030260 ) ) ;
#83271 = CARTESIAN_POINT ( 'NONE',  ( 7.035755370848908896, 7.173079118937375931, 0.7998128361456352531 ) ) ;
#83272 = CARTESIAN_POINT ( 'NONE',  ( 1.036653925908154639, 2.129443126370239803, 0.3705773954724436159 ) ) ;
#83273 = CARTESIAN_POINT ( 'NONE',  ( -4.772106882330247046, 4.669805572247793357, -0.7216878364870207285 ) ) ;
#83274 = CARTESIAN_POINT ( 'NONE',  ( 1.710173085450257924, 1.157096902994741772, -1.651345047625000007 ) ) ;
#83275 = ADVANCED_FACE ( 'NONE', ( #108438 ), #146021, .T. ) ;
#83276 = CARTESIAN_POINT ( 'NONE',  ( 1.863111423135884293, -0.7740270289045609875, 2.164224664766948525 ) ) ;
#83277 = DIRECTION ( 'NONE',  ( 1.000000000000000000, -7.771561172376097755E-16, -4.440892098500627148E-16 ) ) ;
#83278 = CARTESIAN_POINT ( 'NONE',  ( 3.621833129746810265, 4.096114899008192367, -2.499999999999995115 ) ) ;
#83279 = CARTESIAN_POINT ( 'NONE',  ( 11.44779963594988814, 10.89999999999998082, 3.600000000000001421 ) ) ;
#83280 = AXIS2_PLACEMENT_3D ( 'NONE', #170349, #24092, #90196 ) ;
#83281 = CARTESIAN_POINT ( 'NONE',  ( 4.346526858336821952, 0.5246154692373095063, 1.900329053005628044 ) ) ;
#83282 = CARTESIAN_POINT ( 'NONE',  ( 4.065638850954083061, 1.320825628876612479, 1.523796413913918846 ) ) ;
#83284 = CARTESIAN_POINT ( 'NONE',  ( 9.286972035236624734, 11.85788667924133399, -1.443375672974058777 ) ) ;
#83283 = CARTESIAN_POINT ( 'NONE',  ( 0.6823417656249882723, 2.176041667008084435, -1.181850606188749264 ) ) ;
#83286 = CARTESIAN_POINT ( 'NONE',  ( 6.164693330894345458, -1.490570670011469812, 1.488127047250583201 ) ) ;
#83285 = CARTESIAN_POINT ( 'NONE',  ( -7.121056995675673740, 9.330985799753529264, -1.599625672291263179 ) ) ;
#83287 = CARTESIAN_POINT ( 'NONE',  ( 5.424307079040114665, 1.017280057988108499, 1.803113764695261523 ) ) ;
#83288 = CARTESIAN_POINT ( 'NONE',  ( 7.481401836642521452, 7.622723652371411696, 1.040834085586084257E-14 ) ) ;
#83289 = CARTESIAN_POINT ( 'NONE',  ( -5.605406444246153974, 8.627059054007450101, -1.199719254218440723 ) ) ;
#83290 = CARTESIAN_POINT ( 'NONE',  ( 1.814759087649971958, 3.975067388631723819, -0.4606438099578624157 ) ) ;
#83291 = CARTESIAN_POINT ( 'NONE',  ( 4.886975862609196142, -1.903224527948672584, -0.6766701927056159027 ) ) ;
#83292 = CARTESIAN_POINT ( 'NONE',  ( -0.7500000000000006661, -0.3604166659838467512, -1.299038105676652011 ) ) ;
#83293 = CARTESIAN_POINT ( 'NONE',  ( 3.914918041407587257, 1.633027907263858491, -1.630791690553441420 ) ) ;
#83294 = CARTESIAN_POINT ( 'NONE',  ( 0.7606827552629210620, -0.6912373536034731591, -1.943445369992405025 ) ) ;
#83295 = CARTESIAN_POINT ( 'NONE',  ( 9.246297574839983824, 9.889694713509232571, 0.7216878364870438212 ) ) ;
#83296 = EDGE_CURVE ( 'NONE', #105328, #172895, #167249, .T. ) ;
#83297 = CARTESIAN_POINT ( 'NONE',  ( 5.885121196783658526, 9.023669275293071834, 1.199719254218452047 ) ) ;
#83298 = CARTESIAN_POINT ( 'NONE',  ( 5.143339171537801846, 7.093924681584509173, 1.599625672291269396 ) ) ;
#83299 = CARTESIAN_POINT ( 'NONE',  ( 1.364683531249986537, 0.7177083336747527298, -0.7879004041258239610 ) ) ;
#83300 = CARTESIAN_POINT ( 'NONE',  ( 5.499767588998890844, 6.445425604367387429, 1.199719254218451159 ) ) ;
#83301 = CARTESIAN_POINT ( 'NONE',  ( 6.439759776366765998, 9.496508258194486629, 1.082531754730558626 ) ) ;
#83302 = CARTESIAN_POINT ( 'NONE',  ( 2.875608777474625732, -0.2152533142569280078, 2.160498500671267585 ) ) ;
#83304 = CARTESIAN_POINT ( 'NONE',  ( 3.333393596924072444, 0.8250370302015205271, -1.646115572170883112 ) ) ;
#83303 = CARTESIAN_POINT ( 'NONE',  ( -5.314433026876900001, 6.262888621853549331, 1.082531754730548412 ) ) ;
#83305 = CARTESIAN_POINT ( 'NONE',  ( -1.364683531250010295, 4.280208333674753618, 0.7879004041258379498 ) ) ;
#83306 = CARTESIAN_POINT ( 'NONE',  ( 4.071962858106247474, -1.261020321617589479, 1.792237525612811355 ) ) ;
#83307 = DIRECTION ( 'NONE',  ( 0.000000000000000000, 1.000000000000000000, 0.000000000000000000 ) ) ;
#83308 = CARTESIAN_POINT ( 'NONE',  ( 4.504895162230450723, 1.751659092587343869, -1.432031112679124085 ) ) ;
#83309 = CYLINDRICAL_SURFACE ( 'NONE', #190924, 0.08000000000000020983 ) ;
#83310 = CARTESIAN_POINT ( 'NONE',  ( 5.726091835933811325, 7.283405380927965744, -1.209259067671350163 ) ) ;
#83311 = PRESENTATION_LAYER_ASSIGNMENT (  '', '', ( #38341 ) ) ;
#83312 = CARTESIAN_POINT ( 'NONE',  ( -4.597623488365601752, 8.377994813152914944, 0.7216878364870267237 ) ) ;
#83313 = CARTESIAN_POINT ( 'NONE',  ( 5.261973015879598314, 5.311592404713873172, -0.7216878364870458196 ) ) ;
#83314 = CARTESIAN_POINT ( 'NONE',  ( 6.116413106003639300, 1.187136285548880066, -1.312641305385914947 ) ) ;
#83315 = CARTESIAN_POINT ( 'NONE',  ( 4.283843839860628222, 1.952122219449687668, -0.4911893120533029622 ) ) ;
#83316 = CARTESIAN_POINT ( 'NONE',  ( 7.904567251967224095, 9.180748867838630645, 1.199719254218462483 ) ) ;
#83317 = CARTESIAN_POINT ( 'NONE',  ( 3.417109911095609132, 1.903178947333901583, 0.9019662245143298396 ) ) ;
#83318 = CARTESIAN_POINT ( 'NONE',  ( 0.9662486314009374189, -1.869180826568194398, -0.4184218257623931181 ) ) ;
#83320 = CARTESIAN_POINT ( 'NONE',  ( 2.835626683552519012, 6.459981564119914310, 0.000000000000000000 ) ) ;
#83319 = CARTESIAN_POINT ( 'NONE',  ( 0.6823417656249969321, 11.77604166700806054, -1.181850606188757036 ) ) ;
#83321 = CARTESIAN_POINT ( 'NONE',  ( 1.609744333363828384, 0.5749553099084430130, -1.883740962975283706 ) ) ;
#83322 = CARTESIAN_POINT ( 'NONE',  ( 4.746356070053968423, 1.034628734442550879, -1.734499354260822468 ) ) ;
#83323 = CARTESIAN_POINT ( 'NONE',  ( 0.3384655940862451029, 0.3152513238553408814, 1.843739016257638141 ) ) ;
#83324 = CARTESIAN_POINT ( 'NONE',  ( 0.9417639971489067952, 1.314929008279978495, 1.456166070238865018 ) ) ;
#83326 = ORIENTED_EDGE ( 'NONE', *, *, #98945, .T. ) ;
#83325 = CARTESIAN_POINT ( 'NONE',  ( 0.1758378621803426134, 1.891278220088285833, -0.2826890867150752551 ) ) ;
#83327 = CARTESIAN_POINT ( 'NONE',  ( 5.395781948558860286, 6.357795697149212444, -1.082531754730542195 ) ) ;
#83328 = AXIS2_PLACEMENT_3D ( 'NONE', #187790, #169418, #55664 ) ;
#83329 = CARTESIAN_POINT ( 'NONE',  ( 0.6823417656249882723, 0.7385416670080829915, -1.181850606188749264 ) ) ;
#83330 = CARTESIAN_POINT ( 'NONE',  ( 5.735183426005796115, -1.690533149647139410, 0.8011652756413772947 ) ) ;
#83331 = CARTESIAN_POINT ( 'NONE',  ( 5.510910596163088569E-16, 6.999999999999992006, -4.500000000000000000 ) ) ;
#83332 = ORIENTED_EDGE ( 'NONE', *, *, #175741, .F. ) ;
#83333 = CARTESIAN_POINT ( 'NONE',  ( 6.772334134356085222, -0.9704686269969391432, -1.828672837219179392 ) ) ;
#83334 = CARTESIAN_POINT ( 'NONE',  ( -0.6125000000000053735, 2.708333333333333481, -1.060881119635955327 ) ) ;
#83335 = CARTESIAN_POINT ( 'NONE',  ( 0.9067890187421032699, 0.5993529260880943177, 1.981728858978973218 ) ) ;
#83336 = CARTESIAN_POINT ( 'NONE',  ( -0.7500000000000249800, -0.05833333333331303105, 1.299038105676659116 ) ) ;
#83337 = CARTESIAN_POINT ( 'NONE',  ( 7.800018446563675489, 7.994443030612759848, -0.7998128361456281477 ) ) ;
#83338 = CARTESIAN_POINT ( 'NONE',  ( -6.842061076390810292, 11.13415502243129218, 0.000000000000000000 ) ) ;
#83339 = CARTESIAN_POINT ( 'NONE',  ( 6.554440917563797875, 6.611545590104705994, -0.7998128361456481317 ) ) ;
#83340 = CARTESIAN_POINT ( 'NONE',  ( 2.911969131885072670, 6.619324097166378706, 0.000000000000000000 ) ) ;
#83341 = CARTESIAN_POINT ( 'NONE',  ( -1.364683531250012516, 1.280208333674755172, 0.7879004041258379498 ) ) ;
#83342 = ORIENTED_EDGE ( 'NONE', *, *, #208712, .F. ) ;
#83343 = CARTESIAN_POINT ( 'NONE',  ( -0.7500000000000006661, 2.358333333333358262, -1.299038105676652011 ) ) ;
#83345 = CARTESIAN_POINT ( 'NONE',  ( 4.630273154266905777, 5.360739087188218122, 1.199719254218464037 ) ) ;
#83344 = CARTESIAN_POINT ( 'NONE',  ( 5.916451087343006954, 0.7937011933104149985, 1.794315766958521241 ) ) ;
#83346 = CARTESIAN_POINT ( 'NONE',  ( 2.864611068004913275, -0.6351033500862738324, 1.913510180259501592 ) ) ;
#83347 = EDGE_CURVE ( 'NONE', #11477, #93554, #160286, .T. ) ;
#83348 = CARTESIAN_POINT ( 'NONE',  ( 3.977677156295666538, -0.7278633372749753194, 1.772268029184346227 ) ) ;
#83349 = CARTESIAN_POINT ( 'NONE',  ( -1.500000000000031530, 4.452083334016148086, 0.8660254037844287156 ) ) ;
#83350 = CARTESIAN_POINT ( 'NONE',  ( 1.294752383181968503, 1.788903229852260246, -1.265732775075766092 ) ) ;
#83351 = CARTESIAN_POINT ( 'NONE',  ( 0.2333690889706717397, 7.629137130509078268, -2.653349640194931247 ) ) ;
#83352 = CARTESIAN_POINT ( 'NONE',  ( 3.057714436724996876, 1.861869414292870006, -0.1796979844640861634 ) ) ;
#83353 = CARTESIAN_POINT ( 'NONE',  ( -1.402160292154681736E-14, -0.3812499993171785673, -1.732050807568870754 ) ) ;
#83354 = CARTESIAN_POINT ( 'NONE',  ( -8.505042434474312074, 8.816971016508505343, -0.7998128361456291469 ) ) ;
#83356 = CARTESIAN_POINT ( 'NONE',  ( 4.921547094770428288, -1.498112151610554665, -1.496348102564814209 ) ) ;
#83355 = CARTESIAN_POINT ( 'NONE',  ( -5.585596099150199834, 5.618876325204420930, -0.7216878364870207285 ) ) ;
#83357 = CARTESIAN_POINT ( 'NONE',  ( -1.364683531250000748, 8.421875000341403350, 0.000000000000000000 ) ) ;
#83358 = CARTESIAN_POINT ( 'NONE',  ( 6.637176860265922684, -0.09746846054551477900, -2.068182370504913159 ) ) ;
#83360 = CARTESIAN_POINT ( 'NONE',  ( 6.620655732516651071, 1.241313378043694238, 2.288056600130850882 ) ) ;
#83359 = CARTESIAN_POINT ( 'NONE',  ( 2.735971011012145127, 2.075282486531265569, 0.2531079119270570610 ) ) ;
#83362 = EDGE_LOOP ( 'NONE', ( #96102, #136654, #17650, #64483 ) ) ;
#83361 = CARTESIAN_POINT ( 'NONE',  ( 0.4985095413094174921, 1.438046592433483761, -0.9519660005063760311 ) ) ;
#83363 = CARTESIAN_POINT ( 'NONE',  ( 7.962716289927667113, 8.184257181204083409, -0.7998128361456291469 ) ) ;
#83364 = CARTESIAN_POINT ( 'NONE',  ( 6.925078400183531713, -0.004750840071900481326, 2.044148492825673014 ) ) ;
#83365 = DIRECTION ( 'NONE',  ( 0.000000000000000000, 0.000000000000000000, 1.000000000000000000 ) ) ;
#83366 = CARTESIAN_POINT ( 'NONE',  ( -9.812993378609343509, 5.211864641514284635, 6.299721592320037367 ) ) ;
#83367 = CARTESIAN_POINT ( 'NONE',  ( 7.266807146800403849, 7.580289214129690478, 1.040834085586084257E-14 ) ) ;
#83369 =( BOUNDED_CURVE ( )  B_SPLINE_CURVE ( 2, ( #205229, #56870, #3811, #123046, #119800, #188997, #16075, #164489, #137064 ),
 .UNSPECIFIED., .F., .T. ) 
 B_SPLINE_CURVE_WITH_KNOTS ( ( 3, 2, 2, 2, 3 ),
 ( 0.8125000000000000000, 0.8154761904761904656, 0.8214285714285713969, 0.8273809523809523281, 0.8303571428571429047 ),
 .UNSPECIFIED. ) 
 CURVE ( )  GEOMETRIC_REPRESENTATION_ITEM ( )  RATIONAL_B_SPLINE_CURVE ( ( 0.9330127018922194093, 0.9330127018922194093, 1.000000000000000000, 0.8660254037844387076, 1.000000000000000000, 0.8660254037844387076, 1.000000000000000000, 0.9330127018922180770, 0.9330127018922194093 ) ) 
 REPRESENTATION_ITEM ( '' )  );
#83368 = CARTESIAN_POINT ( 'NONE',  ( -1.403499169902660437, 7.376709478543006071, -4.304123474984413278 ) ) ;
#83370 = PRODUCT_DEFINITION_FORMATION_WITH_SPECIFIED_SOURCE ( 'ANY', '', #92073, .NOT_KNOWN. ) ;
#83372 = CARTESIAN_POINT ( 'NONE',  ( 0.7678511737040129015, 1.809490520450097284, -0.08760732307166485544 ) ) ;
#83371 = CARTESIAN_POINT ( 'NONE',  ( 7.693325821111733021, 7.940244644243982464, -0.7998128361456341429 ) ) ;
#83373 = CARTESIAN_POINT ( 'NONE',  ( -5.994676475536691029, 10.14553965476814845, 0.7998128361456481317 ) ) ;
#83374 = AXIS2_PLACEMENT_3D ( 'NONE', #56377, #188501, #40133 ) ;
#83375 = CARTESIAN_POINT ( 'NONE',  ( 4.111146893441827821, 5.819424013814004759, 1.599625672291267398 ) ) ;
#83376 = CARTESIAN_POINT ( 'NONE',  ( -6.160225556963538018, 6.983552031129079296, 0.9223575212774417498 ) ) ;
#83377 = CARTESIAN_POINT ( 'NONE',  ( 7.686546744304875389, 7.932335721302671949, 0.7998128361456291469 ) ) ;
#83378 = CARTESIAN_POINT ( 'NONE',  ( 10.99970480893080627, -9.999999999999994671, 0.08058608058608522640 ) ) ;
#83379 = VECTOR ( 'NONE', #140646, 1000.000000000000000 ) ;
#83380 = CARTESIAN_POINT ( 'NONE',  ( -0.2409995289980224054, 7.629137130509101361, -2.600476469121244527 ) ) ;
#83381 = CARTESIAN_POINT ( 'NONE',  ( 3.994353263318512148, 7.604006752988897055, -0.01585061804776008443 ) ) ;
#83382 = CARTESIAN_POINT ( 'NONE',  ( 8.758204044747994743, 12.20135990463928266, 1.082531754730546636 ) ) ;
#83383 = VERTEX_POINT ( 'NONE', #55744 ) ;
#83384 = CARTESIAN_POINT ( 'NONE',  ( 2.594024687173156263, 0.8801344893799438740, -1.639794913454610148 ) ) ;
#83385 = CARTESIAN_POINT ( 'NONE',  ( 0.1224727961543301408, 0.3280879897031144798, 1.887133295268013766 ) ) ;
#83386 = CARTESIAN_POINT ( 'NONE',  ( 0.09436191691250192526, -0.3928898508825870439, -1.789253991261535726 ) ) ;
#83387 = DIRECTION ( 'NONE',  ( -0.000000000000000000, 1.000000000000000000, -0.000000000000000000 ) ) ;
#83388 = CARTESIAN_POINT ( 'NONE',  ( 0.000000000000000000, 0.000000000000000000, 0.000000000000000000 ) ) ;
#83389 = CARTESIAN_POINT ( 'NONE',  ( 1.833506991698445443, 2.501547993919093660, 2.496244204820597723 ) ) ;
#83390 = CARTESIAN_POINT ( 'NONE',  ( -2.955314298098991266, 6.391691081183366485, 0.7216878364870317197 ) ) ;
#83391 = CARTESIAN_POINT ( 'NONE',  ( 8.758204044748005401, 10.28062147603659504, 1.082531754730549967 ) ) ;
#83392 = CARTESIAN_POINT ( 'NONE',  ( 4.873860229706322933, -1.932217566332248282, 0.3801659098390720581 ) ) ;
#83393 = CARTESIAN_POINT ( 'NONE',  ( 1.155114678095255254, 0.4172207117813032662, 2.078868179971034902 ) ) ;
#83394 = CARTESIAN_POINT ( 'NONE',  ( -4.869349725602420520, 8.832658446511480577, 1.040834085586084257E-14 ) ) ;
#83395 = DIRECTION ( 'NONE',  ( 0.000000000000000000, 0.000000000000000000, 1.000000000000000000 ) ) ;
#83397 = ADVANCED_FACE ( 'NONE', ( #154322 ), #194912, .T. ) ;
#83396 = CYLINDRICAL_SURFACE ( 'NONE', #18147, 1.250000000000000000 ) ;
#83398 = B_SPLINE_CURVE_WITH_KNOTS ( 'NONE', 3,
 ( #133653, #86989, #68581, #117425, #148797, #52364 ),
 .UNSPECIFIED., .F., .F.,
 ( 4, 2, 4 ),
 ( 2.337445424124602418E-15, 0.0003119544853778809289, 0.0006239089707534244264 ),
 .UNSPECIFIED. ) ;
#83399 = CARTESIAN_POINT ( 'NONE',  ( 5.806613533822880591, 1.931179984464112653, 1.035834350304319695 ) ) ;
#83400 = DIRECTION ( 'NONE',  ( 0.000000000000000000, 1.000000000000000000, 0.000000000000000000 ) ) ;
#83401 = CARTESIAN_POINT ( 'NONE',  ( 4.295867091898570855, -0.7379356464434319030, 1.779637345161827922 ) ) ;
#83402 = CARTESIAN_POINT ( 'NONE',  ( -7.369020184227459858, 8.555943955475521889, 1.199719254218450271 ) ) ;
#83403 = CARTESIAN_POINT ( 'NONE',  ( 0.2877648253245302934, -0.8656086203641421006, 1.607325130595547602 ) ) ;
#83404 = CARTESIAN_POINT ( 'NONE',  ( 1.577102763248950046, -2.096353118739826993, -0.6898709473643764856 ) ) ;
#83405 = CARTESIAN_POINT ( 'NONE',  ( -0.4545465019492412884, 7.933486811681471629, 1.993247486878100494 ) ) ;
#83406 = ORIENTED_EDGE ( 'NONE', *, *, #6564, .T. ) ;
#83407 = FACE_OUTER_BOUND ( 'NONE', #210112, .T. ) ;
#83408 = ORIENTED_EDGE ( 'NONE', *, *, #116484, .F. ) ;
#83409 = CARTESIAN_POINT ( 'NONE',  ( 5.735196696812420392, -0.04448252213613138051, -1.969098798407813433 ) ) ;
#83410 = CARTESIAN_POINT ( 'NONE',  ( 1.593202639421680278, -0.6524502387153191529, 1.829324111618094717 ) ) ;
#83411 = CARTESIAN_POINT ( 'NONE',  ( 6.784486029815019137, -2.232095771774603055, 0.5478248251382932255 ) ) ;
#83413 = CARTESIAN_POINT ( 'NONE',  ( 4.680409711739222267, 1.147293496411544433, -1.465074471950976953 ) ) ;
#83412 = CARTESIAN_POINT ( 'NONE',  ( -6.957269102468015554, 8.145844036748005834, 1.199719254218452047 ) ) ;
#83414 = CARTESIAN_POINT ( 'NONE',  ( 5.677832469072920496, 9.846164657218904992, 0.000000000000000000 ) ) ;
#83416 = EDGE_CURVE ( 'NONE', #169050, #137942, #156466, .T. ) ;
#83415 = CARTESIAN_POINT ( 'NONE',  ( 0.4019237886466778820, 11.32366454968462932, 1.500000000000001554 ) ) ;
#83417 = CARTESIAN_POINT ( 'NONE',  ( 0.000000000000000000, 0.2000000000000057288, 0.000000000000000000 ) ) ;
#83418 = CARTESIAN_POINT ( 'NONE',  ( -6.417086777969760902, 6.381022750586497594, 0.7998128361456341429 ) ) ;
#83419 = CARTESIAN_POINT ( 'NONE',  ( -3.174017359375036929, 6.717120995997236221, 0.7216878364870338292 ) ) ;
#83420 = CARTESIAN_POINT ( 'NONE',  ( 0.3104468679729632807, 1.506874830639578056, -1.591553791636945991 ) ) ;
#83421 = CARTESIAN_POINT ( 'NONE',  ( 5.666945020832181434, 5.713783400500082266, 0.7216878364870317197 ) ) ;
#83422 = VERTEX_POINT ( 'NONE', #89334 ) ;
#83423 = DIRECTION ( 'NONE',  ( -1.561251128379126077E-17, -1.301042606982605475E-17, -1.000000000000000000 ) ) ;
#83424 = CARTESIAN_POINT ( 'NONE',  ( 0.000000000000000000, -7.723431457505077979, 0.000000000000000000 ) ) ;
#83425 = CARTESIAN_POINT ( 'NONE',  ( 1.172165686010542274, -1.159919637379997814, 1.409874495853599141 ) ) ;
#83426 = CARTESIAN_POINT ( 'NONE',  ( -5.271422797614987665, 5.044414773505913274, -0.7998128361456221525 ) ) ;
#83427 = CARTESIAN_POINT ( 'NONE',  ( 3.199597886960439119, 1.569373658825726769, 0.7380672391785416675 ) ) ;
#83428 = CARTESIAN_POINT ( 'NONE',  ( -6.600870636098118638, 6.767368133241304484, -0.2259646751960984468 ) ) ;
#83429 = CARTESIAN_POINT ( 'NONE',  ( 6.509000000000032315, 0.5738235599486035676, 2.152438501345500743 ) ) ;
#83430 = CARTESIAN_POINT ( 'NONE',  ( 0.1331565106231571705, 6.948071080078889850, -2.540993614958915181 ) ) ;
#83431 = CARTESIAN_POINT ( 'NONE',  ( 0.2231027806867662000, -0.09612335957175778545, 1.924217376148322334 ) ) ;
#83432 = CARTESIAN_POINT ( 'NONE',  ( 4.768382384511014038, -0.8351381170168621360, -1.775225883709200980 ) ) ;
#83433 = CARTESIAN_POINT ( 'NONE',  ( -7.557780564614042795, 10.90482886110335414, -1.199719254218446718 ) ) ;
#83434 = CARTESIAN_POINT ( 'NONE',  ( 5.774883364416965037, 8.824782127540085952, -1.199719254218440723 ) ) ;
#83435 = CARTESIAN_POINT ( 'NONE',  ( 4.319064098534145302, 1.638436671179326787, -1.346072318137331969 ) ) ;
#83436 = CARTESIAN_POINT ( 'NONE',  ( 5.806634928402749196, 9.996434193103704402, -0.7998128361456481317 ) ) ;
#83437 = CARTESIAN_POINT ( 'NONE',  ( -7.971304249830880373, 11.38727316052296601, 1.199719254218453823 ) ) ;
#83439 = ADVANCED_FACE ( 'NONE', ( #139146 ), #129310, .T. ) ;
#83438 = CIRCLE ( 'NONE', #385, 2.750000000000000444 ) ;
#83440 = LINE ( 'NONE', #117077, #42535 ) ;
#83441 = CARTESIAN_POINT ( 'NONE',  ( 2.588806720547200513, 2.007000696110202043, 0.5072723548179418618 ) ) ;
#83443 = CARTESIAN_POINT ( 'NONE',  ( -1.364683531250014514, -0.1572916663252435232, 0.7879004041258379498 ) ) ;
#83442 = FILL_AREA_STYLE ('',( #116013 ) ) ;
#83444 = ORIENTED_EDGE ( 'NONE', *, *, #154040, .T. ) ;
#83445 = CARTESIAN_POINT ( 'NONE',  ( 2.848558797923263164, 0.3346648989216906012, -2.274091979294257992 ) ) ;
#83446 = CARTESIAN_POINT ( 'NONE',  ( 7.782016984564049444, 11.06247500109133064, 1.082531754730557072 ) ) ;
#83448 = CARTESIAN_POINT ( 'NONE',  ( 3.285556943750000070, -2.384374999522043126, 0.000000000000000000 ) ) ;
#83447 = CARTESIAN_POINT ( 'NONE',  ( 6.373741612200162443, 8.529394195690610303, 1.443375672974065660 ) ) ;
#83449 = CARTESIAN_POINT ( 'NONE',  ( 0.000000000000000000, 8.920000000000001705, 0.000000000000000000 ) ) ;
#83450 = DIRECTION ( 'NONE',  ( 1.000000000000000000, 0.000000000000000000, 0.000000000000000000 ) ) ;
#83451 = ORIENTED_EDGE ( 'NONE', *, *, #188907, .T. ) ;
#83452 = CARTESIAN_POINT ( 'NONE',  ( -2.331034670843834533E-15, -6.027819618361843546, 10.79920600060117941 ) ) ;
#83453 = CARTESIAN_POINT ( 'NONE',  ( 3.814637755342592307, -0.6046605605216844870, -1.814329123173196834 ) ) ;
#83454 = CARTESIAN_POINT ( 'NONE',  ( 0.9311234436981525864, -1.296869630441517707, 3.474999999999998757 ) ) ;
#83455 = CARTESIAN_POINT ( 'NONE',  ( 5.579022813628022881, -0.04626586813367798007, -1.724316369773688962 ) ) ;
#83456 = CARTESIAN_POINT ( 'NONE',  ( 3.643767777461913493, 2.000731686840724333, -0.2516315899964287617 ) ) ;
#83457 = CARTESIAN_POINT ( 'NONE',  ( 4.852278370791485607, 0.2271405875100707961, -2.287421213010778942 ) ) ;
#83458 = CARTESIAN_POINT ( 'NONE',  ( 11.43209210103587914, 11.15596075983914481, 3.649125173352121276 ) ) ;
#83459 = CARTESIAN_POINT ( 'NONE',  ( 0.2060869173217265982, -0.5842117877600698783, 2.128085570573131413 ) ) ;
#83460 = CARTESIAN_POINT ( 'NONE',  ( -4.177320726786319049, 6.927272377009067839, -1.082531754730551743 ) ) ;
#83461 = CARTESIAN_POINT ( 'NONE',  ( 6.415310830085463323, -0.2139434178000785558, 1.756706237510232915 ) ) ;
#83463 = CARTESIAN_POINT ( 'NONE',  ( 2.308868829589076022, 2.048438961056008090, 1.028902946192054912 ) ) ;
#83462 = CARTESIAN_POINT ( 'NONE',  ( 6.886615681098613884, 6.999082814228660077, 0.000000000000000000 ) ) ;
#83464 = CARTESIAN_POINT ( 'NONE',  ( 0.5150585655138568697, -0.9269755740852363424, -1.472709990541859693 ) ) ;
#83465 = CARTESIAN_POINT ( 'NONE',  ( -2.676845263694313637, 5.210404343363602919, -1.199719254218446718 ) ) ;
#83466 = CIRCLE ( 'NONE', #45471, 0.08000000000000020983 ) ;
#83467 = CARTESIAN_POINT ( 'NONE',  ( 6.632779825423476439, -1.959453823303359377, 0.9815127000676395763 ) ) ;
#83468 = CARTESIAN_POINT ( 'NONE',  ( -3.980200614063634568, 6.801261928786307642, 1.199719254218452935 ) ) ;
#83469 = CARTESIAN_POINT ( 'NONE',  ( -3.755786496842897795E-14, -0.01562499965858205574, 1.570758158831768281 ) ) ;
#83470 = CARTESIAN_POINT ( 'NONE',  ( 6.619590326553026038, 0.3579758704960536719, -2.039031579972025554 ) ) ;
#83471 = CARTESIAN_POINT ( 'NONE',  ( 0.8840003597419334724, -2.016708404047353742, 0.004841148455551891328 ) ) ;
#83472 = CARTESIAN_POINT ( 'NONE',  ( -0.7500000000000249800, 0.2229166673494847872, 1.299038105676659116 ) ) ;
#83473 = CARTESIAN_POINT ( 'NONE',  ( 5.303319688262892129, 1.576177044413902717, 1.107479782286522996 ) ) ;
#83474 = CARTESIAN_POINT ( 'NONE',  ( 1.364683531249997417, 11.48437500034139802, 2.602085213965210642E-15 ) ) ;
#83475 = CARTESIAN_POINT ( 'NONE',  ( 2.654761906407083760, 2.205155901917950967, 0.2675573109941364880 ) ) ;
#83476 = VERTEX_POINT ( 'NONE', #140235 ) ;
#83477 = DIRECTION ( 'NONE',  ( 0.000000000000000000, 0.000000000000000000, -1.000000000000000000 ) ) ;
#83478 = PLANE ( 'NONE',  #133991 ) ;
#83479 = CARTESIAN_POINT ( 'NONE',  ( 8.594979316059474073, 12.11489407112305372, 1.199719254218450271 ) ) ;
#83480 = DIRECTION ( 'NONE',  ( 0.000000000000000000, 1.000000000000000000, 0.000000000000000000 ) ) ;
#83481 = CARTESIAN_POINT ( 'NONE',  ( 4.177133728293176418, 1.140962030703307928, 1.314357115670391707 ) ) ;
#83483 = CARTESIAN_POINT ( 'NONE',  ( 3.455471728117681440, 1.544996161402897528, 1.208956721487665087 ) ) ;
#83482 = AXIS2_PLACEMENT_3D ( 'NONE', #54602, #74058, #186725 ) ;
#83485 = CARTESIAN_POINT ( 'NONE',  ( -6.561783159334137139, 8.678499657355050800, -1.443375672974059665 ) ) ;
#83484 = CARTESIAN_POINT ( 'NONE',  ( 4.630273154266905777, 5.360739087188218122, 1.199719254218464037 ) ) ;
#83486 = CARTESIAN_POINT ( 'NONE',  ( -5.901816349531303629, 6.006251404816039141, -0.1731548415426099052 ) ) ;
#83487 = CARTESIAN_POINT ( 'NONE',  ( -10.89999999999920632, -3.430288072414404179E-15, 0.2598076211376223466 ) ) ;
#83488 = CARTESIAN_POINT ( 'NONE',  ( 0.7485702846574161518, -2.046882729015482738, -0.2544144183350918742 ) ) ;
#83489 = CARTESIAN_POINT ( 'NONE',  ( -7.507464373665155399, 9.781794407407920389, 1.599625672291295375 ) ) ;
#83490 = CARTESIAN_POINT ( 'NONE',  ( -3.538314903042294457, 6.111489239315849531, 1.082531754730560403 ) ) ;
#83491 = CARTESIAN_POINT ( 'NONE',  ( 4.821500071095637274, -1.429446227384461032, -1.422610148874188463 ) ) ;
#83492 = CARTESIAN_POINT ( 'NONE',  ( 1.727766546026089145, -2.130035881452702728, 0.7632205929882311946 ) ) ;
#83493 = ORIENTED_EDGE ( 'NONE', *, *, #68596, .F. ) ;
#83494 = CARTESIAN_POINT ( 'NONE',  ( -1.402160292154681736E-14, 0.4937500006828175469, 1.732050807568877637 ) ) ;
#83495 = CARTESIAN_POINT ( 'NONE',  ( 2.319419987651088810, -1.815478447740950685, 0.4500915571382518854 ) ) ;
#83496 = CARTESIAN_POINT ( 'NONE',  ( 1.863478119473166439, -0.08537559288352389308, -1.732189446134152266 ) ) ;
#83497 = CARTESIAN_POINT ( 'NONE',  ( 5.144143540903125533, 0.6357783856077160456, 2.097287126430439130 ) ) ;
#83498 = CARTESIAN_POINT ( 'NONE',  ( 6.528381088282158906, 1.336169653064466889, -1.881230508112927025 ) ) ;
#83499 = CARTESIAN_POINT ( 'NONE',  ( 0.9189065912094130928, 1.903898908998642447, 0.7894373168981814182 ) ) ;
#83500 = CARTESIAN_POINT ( 'NONE',  ( 3.222533412629301708, 0.04844597582449915174, 1.941506634493498362 ) ) ;
#83501 = CARTESIAN_POINT ( 'NONE',  ( -3.917943204224921150, 5.594019709727598766, -1.443375672974051449 ) ) ;
#83502 = CARTESIAN_POINT ( 'NONE',  ( 6.134044790494318278, 0.9221746925026914621, -1.627378824227587062 ) ) ;
#83503 = CARTESIAN_POINT ( 'NONE',  ( 1.312500000000000888, 1.451031289061174734, 1.451031289061067486 ) ) ;
#83504 = CARTESIAN_POINT ( 'NONE',  ( 4.017310073039977780, 7.571390042887482963, 0.3083681156060176232 ) ) ;
#83505 = CARTESIAN_POINT ( 'NONE',  ( 6.626327358740755180, 0.3474107405085808953, -1.985797104380654376 ) ) ;
#83506 = CARTESIAN_POINT ( 'NONE',  ( 2.957086901556340575, 6.464035461875470290, 0.7216878364870257245 ) ) ;
#83507 = CARTESIAN_POINT ( 'NONE',  ( 1.360316468749943608, 1.494791667008105174, 0.7853790794158440614 ) ) ;
#83508 = CARTESIAN_POINT ( 'NONE',  ( 4.764296165657141202, 1.880435471729305030, -0.7283773170061805802 ) ) ;
#83509 = CARTESIAN_POINT ( 'NONE',  ( -3.511198595814942980, 5.119484333249288532, 1.443375672974064550 ) ) ;
#83510 = CARTESIAN_POINT ( 'NONE',  ( 8.829384350997564468, 11.32403438096243775, 1.599625672291281386 ) ) ;
#83511 = CARTESIAN_POINT ( 'NONE',  ( 5.740951700743842423, 5.662474837148078421, -0.7998128361456481317 ) ) ;
#83513 = SURFACE_STYLE_USAGE ( .BOTH. , #181022 ) ;
#83512 = CARTESIAN_POINT ( 'NONE',  ( 2.349991895876184511, 1.825291697999480434, 0.04531359951509549705 ) ) ;
#83514 = CARTESIAN_POINT ( 'NONE',  ( 6.661184041420940005, -7.473374494058216300, -6.773376349083132908 ) ) ;
#83515 = CARTESIAN_POINT ( 'NONE',  ( -9.644676237148278375, 5.067654118421841325, 6.575762993896887565 ) ) ;
#83516 = ORIENTED_EDGE ( 'NONE', *, *, #190385, .T. ) ;
#83517 = CARTESIAN_POINT ( 'NONE',  ( -6.278834536460198734, 6.497930845391236332, 0.7216878364870257245 ) ) ;
#83518 = UNCERTAINTY_MEASURE_WITH_UNIT (LENGTH_MEASURE( 1.000000000000000082E-05 ), #149343, 'distance_accuracy_value', 'NONE');
#83519 = CARTESIAN_POINT ( 'NONE',  ( -1.386567914617391262, 8.090296256147718523, 10.72428812184712932 ) ) ;
#83520 = CARTESIAN_POINT ( 'NONE',  ( -9.657485491635913633, 10.16148791653038330, 1.040834085586084257E-14 ) ) ;
#83521 = CARTESIAN_POINT ( 'NONE',  ( -0.03488881496042146174, -1.619560933857542073, 1.206636643155176714 ) ) ;
#83522 = CARTESIAN_POINT ( 'NONE',  ( 0.3816889160728508812, 0.2035859187828891470, -2.110680546376259681 ) ) ;
#83523 = ORIENTED_EDGE ( 'NONE', *, *, #136119, .F. ) ;
#83524 = CARTESIAN_POINT ( 'NONE',  ( -5.641074431737709283, 8.738948049406083385, -1.199719254218452047 ) ) ;
#83525 = CARTESIAN_POINT ( 'NONE',  ( 4.680589345215795838, 6.483773540883647435, -1.599625672291256295 ) ) ;
#83526 = CARTESIAN_POINT ( 'NONE',  ( 5.981337812661591258, 1.905142945929317211, -0.7864339424841911841 ) ) ;
#83527 = CARTESIAN_POINT ( 'NONE',  ( 5.555314621531947772, -1.277044735018734833, 1.560499014526220307 ) ) ;
#83528 = EDGE_LOOP ( 'NONE', ( #98215, #83001, #45035, #169919 ) ) ;
#83529 = ORIENTED_EDGE ( 'NONE', *, *, #104333, .F. ) ;
#83530 = CARTESIAN_POINT ( 'NONE',  ( 10.02012520139314589, 1.794419290072776896, 6.231960695612015932 ) ) ;
#83531 = CARTESIAN_POINT ( 'NONE',  ( -0.2108831679771168421, 6.948330828014878335, -2.492181822431015270 ) ) ;
#83532 = CIRCLE ( 'NONE', #131970, 0.04999999999999937828 ) ;
#83535 = ORIENTED_EDGE ( 'NONE', *, *, #19728, .F. ) ;
#83534 = CARTESIAN_POINT ( 'NONE',  ( 0.000000000000000000, -0.9200000000000041478, 0.000000000000000000 ) ) ;
#83533 = CARTESIAN_POINT ( 'NONE',  ( -7.144220599758281054, 7.299621885998258897, 0.7998128361456341429 ) ) ;
#83536 = CARTESIAN_POINT ( 'NONE',  ( 4.895464504754282409, 8.144056917144915531, 1.010406422583273178 ) ) ;
#83537 = CARTESIAN_POINT ( 'NONE',  ( 5.290388671387995956, -1.915306256023459053, 0.6297802918850338161 ) ) ;
#83538 = CARTESIAN_POINT ( 'NONE',  ( 4.962772036422566480, 0.1772586797372834311, -1.832584332494808121 ) ) ;
#83539 = TOROIDAL_SURFACE ( 'NONE', #204575, 2.649999999999999911, 0.1000000000000000056 ) ;
#83540 = CARTESIAN_POINT ( 'NONE',  ( -1.063950011417350128, -4.204658361605618566, -0.1571845235116862138 ) ) ;
#83541 = CARTESIAN_POINT ( 'NONE',  ( 3.827072092044791596, 2.190881801378454785, 0.7251257774964211533 ) ) ;
#83542 = CARTESIAN_POINT ( 'NONE',  ( 5.182959862174088883, 9.268813282503625572, 0.7998128361456331437 ) ) ;
#83543 = CARTESIAN_POINT ( 'NONE',  ( 4.288457955665158750, -2.137403104576699242, -0.3218062170811594735 ) ) ;
#83544 = CARTESIAN_POINT ( 'NONE',  ( 8.620286740190458374, 8.951422706510690830, 1.040834085586084257E-14 ) ) ;
#83545 = CARTESIAN_POINT ( 'NONE',  ( 6.515202330376022921, -1.784155196879381622, 0.4545711315065634195 ) ) ;
#83546 = CARTESIAN_POINT ( 'NONE',  ( -3.948449050077848632, 5.629609863222681199, 1.599625672291267398 ) ) ;
#83547 = EDGE_CURVE ( 'NONE', #164595, #111991, #122692, .T. ) ;
#83548 = FACE_OUTER_BOUND ( 'NONE', #186720, .T. ) ;
#83549 = CARTESIAN_POINT ( 'NONE',  ( -4.468294144155606773, 7.370704380560280100, 1.199719254218452935 ) ) ;
#83550 = CARTESIAN_POINT ( 'NONE',  ( 3.871829239884491791, 1.038646522470688671, 1.555605274479121114 ) ) ;
#83553 = CARTESIAN_POINT ( 'NONE',  ( -5.855142236255304944, 7.924361590421551860, -1.599625672291271394 ) ) ;
#83552 = CARTESIAN_POINT ( 'NONE',  ( 0.7499999999999885647, -0.7354166659838470288, 1.299038105676657340 ) ) ;
#83551 = CARTESIAN_POINT ( 'NONE',  ( 1.177825114000274898, 1.883588471398514264, -0.3297955356276888184 ) ) ;
#83554 = CARTESIAN_POINT ( 'NONE',  ( 3.317197348578094562, 1.995112415077514356, 0.9436014139095407760 ) ) ;
#83555 = CARTESIAN_POINT ( 'NONE',  ( -11.96215121607992415, 9.771664462191758105, 0.9565349792967587916 ) ) ;
#83556 = CARTESIAN_POINT ( 'NONE',  ( 3.357615597678655917, 7.068968630600412695, 0.7998128361456321445 ) ) ;
#83557 = CARTESIAN_POINT ( 'NONE',  ( 7.634649897826744080, 9.040084647953621655, 1.082531754730549078 ) ) ;
#83558 = CARTESIAN_POINT ( 'NONE',  ( -4.322352044658376968, 3.937165561723182883, 0.7998128361456341429 ) ) ;
#83559 = CARTESIAN_POINT ( 'NONE',  ( -7.729556973122450714, 8.190440354830551328, 0.000000000000000000 ) ) ;
#83560 = CARTESIAN_POINT ( 'NONE',  ( 0.5089730629182923627, 1.712948150172272976, 0.9756560103859630573 ) ) ;
#83561 = CARTESIAN_POINT ( 'NONE',  ( 0.4644773334415828736, 2.281836724062924038, -0.3429670027690605583 ) ) ;
#83562 = CARTESIAN_POINT ( 'NONE',  ( 1.557006721180295150, 1.605793932651664813, -1.126831546849601740 ) ) ;
#83563 = CARTESIAN_POINT ( 'NONE',  ( 4.627816428071820809, 2.001945081875619259, -0.4960309448565465851 ) ) ;
#83564 = CARTESIAN_POINT ( 'NONE',  ( 4.175548123328908900, 7.815297210618305179, -0.7216878364870197293 ) ) ;
#83565 = CARTESIAN_POINT ( 'NONE',  ( 7.015418140428412386, 7.149352350113456822, 0.7998128361456331437 ) ) ;
#83566 = ORIENTED_EDGE ( 'NONE', *, *, #187477, .F. ) ;
#83567 =( BOUNDED_CURVE ( )  B_SPLINE_CURVE ( 2, ( #191286, #92768, #168916, #86604, #10409, #44009, #174022, #152670, #202456 ),
 .UNSPECIFIED., .F., .T. ) 
 B_SPLINE_CURVE_WITH_KNOTS ( ( 3, 2, 2, 2, 3 ),
 ( 0.4375000000000000000, 0.4444444444444444198, 0.4583333333333333148, 0.4722222222222222099, 0.4791666666666666852 ),
 .UNSPECIFIED. ) 
 CURVE ( )  GEOMETRIC_REPRESENTATION_ITEM ( )  RATIONAL_B_SPLINE_CURVE ( ( 0.9330127018922194093, 0.9330127018922194093, 1.000000000000000000, 0.8660254037844387076, 1.000000000000000000, 0.8660254037844387076, 1.000000000000000000, 0.9330127018922190762, 0.9330127018922194093 ) ) 
 REPRESENTATION_ITEM ( '' )  );
#83568 = CARTESIAN_POINT ( 'NONE',  ( 6.927853306458739979, 10.06595070996845642, 1.082531754730558626 ) ) ;
#83569 = CARTESIAN_POINT ( 'NONE',  ( 0.6823417656249899377, 4.488541667008086655, -1.181850606188754593 ) ) ;
#83570 = DIRECTION ( 'NONE',  ( 0.000000000000000000, -1.000000000000000000, -9.023263958591317418E-17 ) ) ;
#83571 = CARTESIAN_POINT ( 'NONE',  ( 4.500943809612556024, 4.353448654077163305, 1.214306433183764966E-14 ) ) ;
#83572 = CARTESIAN_POINT ( 'NONE',  ( 0.4269466478069834925, -1.418992435970769739, 1.643201522047117669 ) ) ;
#83573 = TRIMMED_CURVE ( 'NONE', #176468, ( PARAMETER_VALUE ( 5.355238923655765149 ), #109946 ), ( PARAMETER_VALUE ( 0.000000000000000000 ), #175955 ), .T., .PARAMETER. ) ;
#83575 =( NAMED_UNIT ( * ) SI_UNIT ( $, .STERADIAN. ) SOLID_ANGLE_UNIT ( ) );
#83574 = CARTESIAN_POINT ( 'NONE',  ( 9.617101990990372329, -9.241291349679091383, -0.3048231516917216388 ) ) ;
#83576 = CARTESIAN_POINT ( 'NONE',  ( -2.157015650737198253, 3.934209603697780278, 11.36298392073394048 ) ) ;
#83577 = DIRECTION ( 'NONE',  ( 1.000000000000000000, 0.000000000000000000, 0.000000000000000000 ) ) ;
#83578 = CARTESIAN_POINT ( 'NONE',  ( 1.299835797595794151, -1.870726058509405210, -0.005653028302576856845 ) ) ;
#83579 = CARTESIAN_POINT ( 'NONE',  ( 5.764953170560049855, -1.951456690425241947, -0.9300186209130756332 ) ) ;
#83580 = CARTESIAN_POINT ( 'NONE',  ( -6.133306371789854161, 5.998871118906519584, 0.1305517085098181207 ) ) ;
#83581 =( LENGTH_UNIT ( ) NAMED_UNIT ( * ) SI_UNIT ( .MILLI., .METRE. ) );
#83582 = CARTESIAN_POINT ( 'NONE',  ( 6.512538272292041519, 6.827515365185738538, -0.5364851146780359459 ) ) ;
#83583 = CARTESIAN_POINT ( 'NONE',  ( -1.201851678989727383E-14, 5.009375000341421469, -1.575800808251660134 ) ) ;
#83584 = CARTESIAN_POINT ( 'NONE',  ( 0.8910925258837493201, -0.04752833427993513604, -1.911862225341356858 ) ) ;
#83585 = CARTESIAN_POINT ( 'NONE',  ( 2.922431196026415101, 1.665835785064853969, 0.5981315555363684311 ) ) ;
#83586 = CARTESIAN_POINT ( 'NONE',  ( 0.8031952904608251620, 1.686239601473665140, -0.9019194118903075541 ) ) ;
#83588 = CARTESIAN_POINT ( 'NONE',  ( 4.464398116780900594, -1.859039872360370937, -0.4615888831297955686 ) ) ;
#83587 = CARTESIAN_POINT ( 'NONE',  ( 2.862582142408669927, -3.212557612082180825, 1.662679547930521640 ) ) ;
#83589 = CARTESIAN_POINT ( 'NONE',  ( -1.500000000000015099, -0.8708333333333129200, -0.8660254037844383745 ) ) ;
#83590 = CARTESIAN_POINT ( 'NONE',  ( 5.617622257330707747, 0.3859593044726419286, -1.931177630036359005 ) ) ;
#83591 = CARTESIAN_POINT ( 'NONE',  ( 0.8266187642571948269, -0.9586779626098644869, -1.891633453305548773 ) ) ;
#83592 = DIRECTION ( 'NONE',  ( 1.276756478318932585E-15, -1.000000000000000000, 1.665334536937738262E-16 ) ) ;
#83593 = CARTESIAN_POINT ( 'NONE',  ( 3.555401268124198655, 0.4554524271490404952, -1.814226883376020671 ) ) ;
#83595 = EDGE_LOOP ( 'NONE', ( #79480, #42671, #67609, #76541 ) ) ;
#83594 = CARTESIAN_POINT ( 'NONE',  ( 0.9436603434208358232, 0.7422609627109194586, -1.668170528445270140 ) ) ;
#83597 = CARTESIAN_POINT ( 'NONE',  ( -4.109529958273621553, 7.808552361378945150, 0.7216878364870283891 ) ) ;
#83596 = CARTESIAN_POINT ( 'NONE',  ( 3.369938178094655346, 2.153121441420174698, -0.4834393813165636100 ) ) ;
#83598 = CARTESIAN_POINT ( 'NONE',  ( 1.364683531249988535, 4.217708333674752730, -0.7879004041258239610 ) ) ;
#83599 = CARTESIAN_POINT ( 'NONE',  ( 1.557159421845564218, 1.687539990290163772, -1.185865425756290392 ) ) ;
#83600 = CARTESIAN_POINT ( 'NONE',  ( 5.880485940025228508, 7.883652901494672349, 1.599625672291267398 ) ) ;
#83601 = CARTESIAN_POINT ( 'NONE',  ( -7.818248136574758256, 12.27303992597924420, 0.000000000000000000 ) ) ;
#83602 = DIRECTION ( 'NONE',  ( 1.000000000000000000, 0.000000000000000000, -4.440892098500751393E-16 ) ) ;
#83603 = CARTESIAN_POINT ( 'NONE',  ( 11.96212011828583677, 11.32812445049936656, -0.9569185076418588176 ) ) ;
#83604 = VECTOR ( 'NONE', #164604, 1000.000000000000000 ) ;
#83605 = CARTESIAN_POINT ( 'NONE',  ( 7.842465510862060896, 8.114240948952696542, 0.000000000000000000 ) ) ;
#83606 = ORIENTED_EDGE ( 'NONE', *, *, #178239, .F. ) ;
#83607 = CARTESIAN_POINT ( 'NONE',  ( 4.791501694037465953, -1.894250426384593844, 0.8359921707915063394 ) ) ;
#83608 = CARTESIAN_POINT ( 'NONE',  ( 0.6823417656249882723, -1.094791666325249713, 1.181850606188755259 ) ) ;
#83609 = CARTESIAN_POINT ( 'NONE',  ( 1.247603677004164746, -1.703183937513498281, -1.330886036463780009 ) ) ;
#83610 = CARTESIAN_POINT ( 'NONE',  ( -4.945771867956824330, 7.989995641179508112, -1.012621479200847441 ) ) ;
#83611 = CARTESIAN_POINT ( 'NONE',  ( 2.227218753574769838, 1.805135905798272100, 0.9059672028350268524 ) ) ;
#83612 = CARTESIAN_POINT ( 'NONE',  ( 1.734723475976807094E-15, -7.105553651663779391, 0.000000000000000000 ) ) ;
#83613 = EDGE_LOOP ( 'NONE', ( #128513, #101241, #112215, #14162, #109689, #211247, #160379, #77599 ) ) ;
#83615 = CARTESIAN_POINT ( 'NONE',  ( 9.436111725431318931, 10.11114455586577776, -0.7216878364870257245 ) ) ;
#83614 = CARTESIAN_POINT ( 'NONE',  ( 3.475000000000000533, -3.295833333333334725, -2.006292185433951047 ) ) ;
#83616 = CARTESIAN_POINT ( 'NONE',  ( 6.520861224751243412, 2.010896128390584625, -0.1455136175190149816 ) ) ;
#83617 = CARTESIAN_POINT ( 'NONE',  ( 0.6730650033222317363, 1.776164188848127878, -0.9548607967814757291 ) ) ;
#83618 = CARTESIAN_POINT ( 'NONE',  ( 6.639320575229251453, 6.034321252505787214, 2.798156424428144717 ) ) ;
#83619 = CARTESIAN_POINT ( 'NONE',  ( 4.933237592207079025, -1.549687834843778811, -1.549900206446311657 ) ) ;
#83620 = CARTESIAN_POINT ( 'NONE',  ( -0.7500000000000215383, 3.472916667349487785, 1.299038105676671107 ) ) ;
#83621 = CARTESIAN_POINT ( 'NONE',  ( 3.726736447152957599, 1.348887845406310682, -1.355897031963343213 ) ) ;
#83622 = CARTESIAN_POINT ( 'NONE',  ( -5.590039407536138150, 5.416134151747256986, 0.000000000000000000 ) ) ;
#83623 = CARTESIAN_POINT ( 'NONE',  ( 3.172244755473273781, 6.644776614786712443, 0.000000000000000000 ) ) ;
#83625 = CARTESIAN_POINT ( 'NONE',  ( 2.056267757160272325, -1.238304521155994209, 1.591332585091954854 ) ) ;
#83624 = CARTESIAN_POINT ( 'NONE',  ( 3.719872605471085336, 6.605953636083950364, 2.420000000000000373 ) ) ;
#83626 = CARTESIAN_POINT ( 'NONE',  ( -0.6823417656250003738, 11.96354166700806765, 1.181850606188754593 ) ) ;
#83628 = CARTESIAN_POINT ( 'NONE',  ( -5.330290668828105538, 6.247702530834755130, 1.199719254218452935 ) ) ;
#83627 = CARTESIAN_POINT ( 'NONE',  ( 0.3809655214361170050, -0.2885804254640594868, -2.274098033663536356 ) ) ;
#83629 = CARTESIAN_POINT ( 'NONE',  ( 3.698037441923990087, -1.722821800119245683, -0.08474311298608917797 ) ) ;
#83630 = CARTESIAN_POINT ( 'NONE',  ( 6.339319342841494453, 9.553567112360518365, -1.199719254218452047 ) ) ;
#83631 = CARTESIAN_POINT ( 'NONE',  ( 2.672928840188529609, 6.270167413528593414, 0.000000000000000000 ) ) ;
#83632 = CIRCLE ( 'NONE', #104508, 0.08000000000000014044 ) ;
#83633 = CARTESIAN_POINT ( 'NONE',  ( -1.217358635584790738, 2.941465920220512231, -0.7749999999999944711 ) ) ;
#83634 = CARTESIAN_POINT ( 'NONE',  ( 0.8187140321147531319, -1.423520202335259999, 1.350257566363553208 ) ) ;
#83635 = CARTESIAN_POINT ( 'NONE',  ( 0.1753634416057497647, 4.084635187426246539, -2.698744815386323381 ) ) ;
#83636 = EDGE_LOOP ( 'NONE', ( #190634, #190286, #200641, #100172 ) ) ;
#83637 = CARTESIAN_POINT ( 'NONE',  ( 3.580526426040127941, -1.214262702978758712, 1.344428254631929276 ) ) ;
#83638 = VERTEX_POINT ( 'NONE', #188944 ) ;
#83639 = CARTESIAN_POINT ( 'NONE',  ( 6.692885107001518286, 7.837396042037102717, -1.199719254218452047 ) ) ;
#83640 = FACE_OUTER_BOUND ( 'NONE', #2509, .T. ) ;
#83641 = CARTESIAN_POINT ( 'NONE',  ( 4.775916358578648158, 1.790991888885495431, -0.2707881515907252234 ) ) ;
#83642 = CARTESIAN_POINT ( 'NONE',  ( 7.309254211098767051, 7.700087132469628948, 0.7216878364870267237 ) ) ;
#83643 = CARTESIAN_POINT ( 'NONE',  ( -5.956409969451652131, 6.075908546082715134, -0.6293437877468227581 ) ) ;
#83644 = CARTESIAN_POINT ( 'NONE',  ( 5.815065281910236195, 6.023992952839542170, -0.4647386070683479642 ) ) ;
#83645 = EDGE_LOOP ( 'NONE', ( #177931, #80179 ) ) ;
#83647 = CARTESIAN_POINT ( 'NONE',  ( 8.757677159423465696, 12.30470822171437284, 1.199719254218450271 ) ) ;
#83646 = CARTESIAN_POINT ( 'NONE',  ( 6.180112001919068732, -1.034620502799053599, -1.546732508075428392 ) ) ;
#83648 = CARTESIAN_POINT ( 'NONE',  ( 4.077677060472849391, -0.7296757366501721576, 1.771397967703478793 ) ) ;
#83649 = DIRECTION ( 'NONE',  ( -1.000000000000000000, 4.984021416236792516E-16, 0.000000000000000000 ) ) ;
#83650 = DIRECTION ( 'NONE',  ( 1.000000000000000000, 0.000000000000000000, -0.000000000000000000 ) ) ;
#83651 = CARTESIAN_POINT ( 'NONE',  ( 1.364683531249988757, -0.8656249996585805295, 0.000000000000000000 ) ) ;
#83652 = CARTESIAN_POINT ( 'NONE',  ( 5.178851490740187913, 8.985817805931475277, 0.7216878364870438212 ) ) ;
#83654 = CARTESIAN_POINT ( 'NONE',  ( 5.823477710672365859, -1.535350753823118586, -1.458276433397849514 ) ) ;
#83653 = CARTESIAN_POINT ( 'NONE',  ( -4.288456660624211381, 3.897620947016656956, 1.214306433183764966E-14 ) ) ;
#83655 = CARTESIAN_POINT ( 'NONE',  ( 1.006953172832128374, 1.636353683469338183, -1.412668763314451903 ) ) ;
#83656 = CARTESIAN_POINT ( 'NONE',  ( -5.529746549527323474, 7.544733289238903851, -1.599625672291271394 ) ) ;
#83657 = CARTESIAN_POINT ( 'NONE',  ( 5.252858170651868441, 5.093032385374103299, -0.7998128361456481317 ) ) ;
#83658 = CARTESIAN_POINT ( 'NONE',  ( 1.166719304534512558, -1.648536928579244165, -0.7845717211837843763 ) ) ;
#83659 = CARTESIAN_POINT ( 'NONE',  ( -2.591579918506545344, 6.175260338232929413, 1.040834085586084257E-14 ) ) ;
#83660 = CARTESIAN_POINT ( 'NONE',  ( 3.381694320706640333, 1.157239582903809128, 1.411935816614327655 ) ) ;
#83661 = CARTESIAN_POINT ( 'NONE',  ( 10.32808049211214652, 11.37156981856230686, -7.280726186550563028 ) ) ;
#83662 = ORIENTED_EDGE ( 'NONE', *, *, #212227, .T. ) ;
#83663 = CARTESIAN_POINT ( 'NONE',  ( 2.312896453495900673, -1.524290774635113088, 1.247285826271822939 ) ) ;
#83664 = CARTESIAN_POINT ( 'NONE',  ( 4.458499667006603495, -1.736235857128598070, -0.8702183630341918663 ) ) ;
#83665 = CARTESIAN_POINT ( 'NONE',  ( -5.029148636026397945, 4.832037928311032182, 0.7998128361456281477 ) ) ;
#83667 = CARTESIAN_POINT ( 'NONE',  ( 5.801066647469003357, -0.3129311994157328303, -2.097281602037828208 ) ) ;
#83666 = CARTESIAN_POINT ( 'NONE',  ( 5.885121196783658526, 9.023669275293071834, 1.199719254218452047 ) ) ;
#83669 = EDGE_CURVE ( 'NONE', #9073, #205992, #101519, .T. ) ;
#83668 = DIRECTION ( 'NONE',  ( 0.000000000000000000, 1.000000000000000000, 0.000000000000000000 ) ) ;
#83670 = CARTESIAN_POINT ( 'NONE',  ( 3.053266463924544372, -1.685387242695039811, 0.9035085923766730254 ) ) ;
#83671 = CARTESIAN_POINT ( 'NONE',  ( 5.936406840065503232, 6.128608848081334770, 0.7476236741628620175 ) ) ;
#83672 = CARTESIAN_POINT ( 'NONE',  ( -1.270904146967317017, 3.121556430829590223, -0.7749999999999892530 ) ) ;
#83673 = DIRECTION ( 'NONE',  ( 0.000000000000000000, -1.000000000000000000, 0.000000000000000000 ) ) ;
#83674 = CARTESIAN_POINT ( 'NONE',  ( 5.228604516725597229, 6.129068686715179126, -1.199719254218450271 ) ) ;
#83675 = CARTESIAN_POINT ( 'NONE',  ( 4.334856428067313416, 6.080418470877079429, -1.599625672291256295 ) ) ;
#83676 = FACE_OUTER_BOUND ( 'NONE', #165466, .T. ) ;
#83678 = CARTESIAN_POINT ( 'NONE',  ( 6.087125082597877324, 1.679220375458953862, 1.116214469231976869 ) ) ;
#83677 = CARTESIAN_POINT ( 'NONE',  ( 4.529811765687052016, -1.125283923072720071, -1.437579299059896343 ) ) ;
#83679 = CARTESIAN_POINT ( 'NONE',  ( 0.3175553531547097852, 3.956598013261177105, -11.53924059509142452 ) ) ;
#83680 = CARTESIAN_POINT ( 'NONE',  ( -7.849807752632384172, 12.10193344480572897, 0.000000000000000000 ) ) ;
#83681 = VECTOR ( 'NONE', #187382, 1000.000000000000114 ) ;
#83682 = CARTESIAN_POINT ( 'NONE',  ( -6.198085906554800850, 7.039857339855744023, 1.052733950999720003 ) ) ;
#83683 = CARTESIAN_POINT ( 'NONE',  ( -1.499999999999997780, 3.900000000000021672, 1.214306433183764966E-14 ) ) ;
#83684 = CARTESIAN_POINT ( 'NONE',  ( 5.998880656844745474, 1.528293836345222312, -1.078463600801618405 ) ) ;
#83685 = CARTESIAN_POINT ( 'NONE',  ( 7.721532178182734185, 8.967207948423393304, 1.199719254218462483 ) ) ;
#83686 =( GEOMETRIC_REPRESENTATION_CONTEXT ( 3 ) GLOBAL_UNCERTAINTY_ASSIGNED_CONTEXT ( ( #21125 ) ) GLOBAL_UNIT_ASSIGNED_CONTEXT ( ( #138828, #104188, #6655 ) ) REPRESENTATION_CONTEXT ( 'NONE', 'WORKASPACE' ) );
#83687 = CARTESIAN_POINT ( 'NONE',  ( -3.978428010606240850, 6.728917548094202949, -1.199719254218452047 ) ) ;
#83688 = CARTESIAN_POINT ( 'NONE',  ( 3.344057444064992168, 7.053150784717805877, 1.040834085586084257E-14 ) ) ;
#83689 = CARTESIAN_POINT ( 'NONE',  ( -0.6823417656250003738, 9.963541667008065872, 1.181850606188754593 ) ) ;
#83690 = CARTESIAN_POINT ( 'NONE',  ( -6.033542053281340856, 6.997886136038390603, -1.199719254218446718 ) ) ;
#83691 = CARTESIAN_POINT ( 'NONE',  ( 2.198393463710220264, 5.716542807637226886, 0.7998128361456462443 ) ) ;
#83692 = CARTESIAN_POINT ( 'NONE',  ( -5.772739544368596043, 9.956889578397179363, -0.7998128361456362523 ) ) ;
#83693 = CARTESIAN_POINT ( 'NONE',  ( -5.096975683733680818, 8.033889833409558534, -1.199719254218452047 ) ) ;
#83694 = CARTESIAN_POINT ( 'NONE',  ( 6.455955546751245500, -0.7393474466994474081, 2.041418194955111787 ) ) ;
#83695 = EDGE_CURVE ( 'NONE', #35846, #82118, #51711, .T. ) ;
#83696 = CARTESIAN_POINT ( 'NONE',  ( 1.687271568794300070, 1.762372639767064042, 1.173053760763353104 ) ) ;
#83697 = CARTESIAN_POINT ( 'NONE',  ( 8.890396042259068210, 11.39521468743417998, -1.599625672291257406 ) ) ;
#83698 = CARTESIAN_POINT ( 'NONE',  ( -3.620328817674902666, 3.489345133412038447, 2.447831560964403685 ) ) ;
#83699 = CARTESIAN_POINT ( 'NONE',  ( 5.752806990244247132, -0.4974732019265226679, -2.009498513695342936 ) ) ;
#83701 = CARTESIAN_POINT ( 'NONE',  ( 4.167679133687917314, 7.375052378509237450, -0.7893339205088979460 ) ) ;
#83700 = CARTESIAN_POINT ( 'NONE',  ( 1.188719773494644860, 1.394467456127197025, 1.202481090285527632 ) ) ;
#83702 = CARTESIAN_POINT ( 'NONE',  ( 5.992340707560151358, 8.014150130285418783, 1.443375672974062551 ) ) ;
#83703 = CARTESIAN_POINT ( 'NONE',  ( -3.474999999999998312, -3.470833333333334103, 2.006292185433951047 ) ) ;
#83704 = CARTESIAN_POINT ( 'NONE',  ( 1.096115288130569798, -2.292435215939184534, 0.004638672314880368241 ) ) ;
#83706 = DIRECTION ( 'NONE',  ( 0.000000000000000000, 1.000000000000000000, 0.000000000000000000 ) ) ;
#83705 = CARTESIAN_POINT ( 'NONE',  ( 2.359223927328457648E-13, 7.078193277237625480, 2.121339347286388843 ) ) ;
#83707 = CARTESIAN_POINT ( 'NONE',  ( 2.443496805918866865, -1.782974011999260977, 0.6919810379762069141 ) ) ;
#83708 = ORIENTED_EDGE ( 'NONE', *, *, #199736, .F. ) ;
#83709 = CARTESIAN_POINT ( 'NONE',  ( 6.738039155867407537, 10.80487008191325771, -0.7216878364870267237 ) ) ;
#83710 = CARTESIAN_POINT ( 'NONE',  ( 0.9670423206251937964, -1.584547017232017518, 1.241716394148101088 ) ) ;
#83711 = CARTESIAN_POINT ( 'NONE',  ( 0.7253527386562284018, 0.1980078388067410544, -1.951770168129369543 ) ) ;
#83712 = CARTESIAN_POINT ( 'NONE',  ( -6.337068562759858636, 6.936200024879327408, -0.9492287992594623525 ) ) ;
#83714 = DIRECTION ( 'NONE',  ( -0.5996521035822321988, 0.8002608041566222630, 0.000000000000000000 ) ) ;
#83713 = CARTESIAN_POINT ( 'NONE',  ( -7.771848369131641121, 10.09024240211882351, -1.599625672291263179 ) ) ;
#83715 = CARTESIAN_POINT ( 'NONE',  ( -10.41980074470002648, 5.020554563858687480, 5.279403930596816785 ) ) ;
#83717 = CARTESIAN_POINT ( 'NONE',  ( 2.570886989259568267, 0.08925172825972882418, -1.767725737713058631 ) ) ;
#83716 = CARTESIAN_POINT ( 'NONE',  ( 4.435544174077206137, 0.8940267830384877046, -1.889970096008020128 ) ) ;
#83718 = LINE ( 'NONE', #2444, #88449 ) ;
#83720 = CARTESIAN_POINT ( 'NONE',  ( 5.419995920891611085, 1.369053228189264670, -1.838397148955115412 ) ) ;
#83719 = CARTESIAN_POINT ( 'NONE',  ( -11.39017651643713869, 6.534219839500422289, 3.782342671282047153 ) ) ;
#83721 = CARTESIAN_POINT ( 'NONE',  ( 3.152039231231161587, -1.317153252834550425, 1.137565551706197775 ) ) ;
#83722 = CARTESIAN_POINT ( 'NONE',  ( 8.920375002787457319, 12.49452237230570084, 1.199719254218450271 ) ) ;
#83723 = MECHANICAL_DESIGN_GEOMETRIC_PRESENTATION_REPRESENTATION (  '', ( #28391 ), #52801 ) ;
#83724 = CARTESIAN_POINT ( 'NONE',  ( 5.306037014901791693, 7.283738832175834510, 1.599625672291269396 ) ) ;
#83725 = CARTESIAN_POINT ( 'NONE',  ( 3.251044507966997177, -1.707695807076513805, -0.2988343314351063484 ) ) ;
#83726 = CARTESIAN_POINT ( 'NONE',  ( 3.209609721163650509, -1.773450621654437009, -1.252290679139915319 ) ) ;
#83727 = CARTESIAN_POINT ( 'NONE',  ( 4.416205349749311004, 6.175325546172740765, 1.599625672291267398 ) ) ;
#83728 = CARTESIAN_POINT ( 'NONE',  ( 5.155482549980198392, 1.942097955248718533, -0.5424665614216088727 ) ) ;
#83729 = CARTESIAN_POINT ( 'NONE',  ( 6.739650031034449817, -0.2601230917362121753, 2.000000000000034639 ) ) ;
#83730 = CARTESIAN_POINT ( 'NONE',  ( -1.499999999999997780, 4.681250000682819490, 1.214306433183764966E-14 ) ) ;
#83731 = CARTESIAN_POINT ( 'NONE',  ( 2.204012588094861780, -1.926017964255047010, 0.04517517324725479899 ) ) ;
#83732 = CARTESIAN_POINT ( 'NONE',  ( 1.500000000000001332, 9.156250000682799595, 0.000000000000000000 ) ) ;
#83733 = CARTESIAN_POINT ( 'NONE',  ( 5.256174644204150148, 0.8999736644031709476, -2.031094499404682008 ) ) ;
#83734 = ORIENTED_EDGE ( 'NONE', *, *, #108718, .T. ) ;
#83735 = CARTESIAN_POINT ( 'NONE',  ( -0.2106854629474881058, 5.722459385925042774, -2.591190942950042597 ) ) ;
#83736 = CARTESIAN_POINT ( 'NONE',  ( 1.499999999999987121, 2.045833333333356929, -0.8660254037844262731 ) ) ;
#83737 = CARTESIAN_POINT ( 'NONE',  ( 5.438792177376376991, 9.497007973581119700, 1.040834085586084257E-14 ) ) ;
#83738 = CARTESIAN_POINT ( 'NONE',  ( 4.812781342726866640, 5.677628323678546529, 1.082531754730560403 ) ) ;
#83739 = CARTESIAN_POINT ( 'NONE',  ( -1.642778471875000035, -1.567708332855376252, -2.845375778867859751 ) ) ;
#83740 = CARTESIAN_POINT ( 'NONE',  ( 1.700152687198818402, 1.534743396142525640, 1.606060300191413548 ) ) ;
#83741 = CARTESIAN_POINT ( 'NONE',  ( 6.426224708462171087, 1.007414738832881573, 1.683299376423300853 ) ) ;
#83742 = CARTESIAN_POINT ( 'NONE',  ( 8.920901888111997025, 10.47043562662792304, 1.082531754730549967 ) ) ;
#83743 = CARTESIAN_POINT ( 'NONE',  ( 6.907534427287327361, -0.5096537312613695914, 2.212693016512882416 ) ) ;
#83744 = CIRCLE ( 'NONE', #18019, 1.250000000000000444 ) ;
#83745 = CARTESIAN_POINT ( 'NONE',  ( 3.854260808034858155, 7.718664386007802136, -0.7998128361456362523 ) ) ;
#83746 = B_SPLINE_CURVE_WITH_KNOTS ( 'NONE', 3,
 ( #48898, #196214, #181014, #147471, #145376, #162654 ),
 .UNSPECIFIED., .F., .F.,
 ( 4, 2, 4 ),
 ( 0.000000000000000000, 0.0007995527602724504957, 0.001599105520544900991 ),
 .UNSPECIFIED. ) ;
#83747 = CARTESIAN_POINT ( 'NONE',  ( -0.1048463755018592264, -0.8645036352170620830, -1.819965476435807306 ) ) ;
#83748 = CARTESIAN_POINT ( 'NONE',  ( 4.650865732144216835, -0.4487226328800034691, -2.013136760839563166 ) ) ;
#83749 = CARTESIAN_POINT ( 'NONE',  ( -4.069418662396130593, 7.899405539437467816, -0.7998128361456281477 ) ) ;
#83750 = B_SPLINE_CURVE_WITH_KNOTS ( 'NONE', 3,
 ( #85670, #19597, #53175, #83530, #115043, #183172, #151756 ),
 .UNSPECIFIED., .F., .F.,
 ( 4, 3, 4 ),
 ( 0.000000000000000000, 0.0008000000000004423928, 0.002977368225425629754 ),
 .UNSPECIFIED. ) ;
#83751 = CARTESIAN_POINT ( 'NONE',  ( -1.201851678989727383E-14, 4.118750000682818602, -1.732050807568863648 ) ) ;
#83752 = CARTESIAN_POINT ( 'NONE',  ( -0.6823417656250003738, -0.5322916663252491576, -1.181850606188749264 ) ) ;
#83753 = CARTESIAN_POINT ( 'NONE',  ( 5.466025653875023593, 0.9211120992074215419, 1.627924866423650530 ) ) ;
#83754 = CARTESIAN_POINT ( 'NONE',  ( 4.570818470097482766, -0.8114142876072638622, 1.532583664885181607 ) ) ;
#83755 = CARTESIAN_POINT ( 'NONE',  ( 4.458407330353141518, -1.557363759602323761, -0.7771466779550126880 ) ) ;
#83756 = CARTESIAN_POINT ( 'NONE',  ( 4.871457266011829823, 4.577788319968905562, -0.7998128361456221525 ) ) ;
#83757 = CARTESIAN_POINT ( 'NONE',  ( 1.470720204089857930, -2.178542539925924171, -0.7136519110988813752 ) ) ;
#83758 = CARTESIAN_POINT ( 'NONE',  ( 1.364683531249988535, 4.967708333674756283, -0.7879004041258300672 ) ) ;
#83759 = CARTESIAN_POINT ( 'NONE',  ( 5.161704669080129371, 1.031500688015974054, 1.818515148517543034 ) ) ;
#83760 = CARTESIAN_POINT ( 'NONE',  ( 0.1988192939417210425, -0.4940924592915455493, 1.773541111592655373 ) ) ;
#83761 = CARTESIAN_POINT ( 'NONE',  ( 0.1007326007325003298, -10.00000000000001243, 10.99953876047307944 ) ) ;
#83762 = CARTESIAN_POINT ( 'NONE',  ( 2.074842474778653134, -0.8596299393073093542, 1.824119475507138821 ) ) ;
#83763 = CARTESIAN_POINT ( 'NONE',  ( 0.3577192552456122665, 2.167005522336755696, -0.3256184645209562190 ) ) ;
#83764 = CARTESIAN_POINT ( 'NONE',  ( 0.000000000000000000, 18.91999999999999815, 0.000000000000000000 ) ) ;
#83765 = CARTESIAN_POINT ( 'NONE',  ( -8.199983978166823562, 8.461069484149769337, -0.7998128361456291469 ) ) ;
#83766 = CARTESIAN_POINT ( 'NONE',  ( 6.654354466208897811, 6.657835053532175529, 0.7998128361456341429 ) ) ;
#83767 = CARTESIAN_POINT ( 'NONE',  ( -1.360316468749998675, 2.411458333674741716, 0.7853790794158941324 ) ) ;
#83768 = CARTESIAN_POINT ( 'NONE',  ( 3.281995766809755466, 2.068381274212594878, -0.4664580258975092875 ) ) ;
#83769 = CARTESIAN_POINT ( 'NONE',  ( -1.364683531250014514, -0.2197916663252438285, 0.7879004041258379498 ) ) ;
#83770 = CARTESIAN_POINT ( 'NONE',  ( 5.795480788678070816, 1.385457615097264394, 1.189071861804301466 ) ) ;
#83771 = ORIENTED_EDGE ( 'NONE', *, *, #66008, .T. ) ;
#83772 = CARTESIAN_POINT ( 'NONE',  ( -5.582925393777276035, 9.735439736040634173, 0.7998128361456291469 ) ) ;
#83773 = DIRECTION ( 'NONE',  ( -7.387867266669436732E-31, 1.000000000000000000, 8.546850786086424434E-32 ) ) ;
#83774 = CARTESIAN_POINT ( 'NONE',  ( 1.737499999999999378, -2.172916665710750816, -3.009438278150925683 ) ) ;
#83775 = CARTESIAN_POINT ( 'NONE',  ( -5.371001409308059138, 9.417918744168066070, -0.7998128361456231517 ) ) ;
#83776 = CARTESIAN_POINT ( 'NONE',  ( 2.935811755974365500, -1.945362344549756539, 0.5428778075214285570 ) ) ;
#83777 = CARTESIAN_POINT ( 'NONE',  ( 0.2355646933672841947, -1.925288835042149760, 0.8538303211676525617 ) ) ;
#83778 = CIRCLE ( 'NONE', #14658, 11.09999999999999964 ) ;
#83779 = CARTESIAN_POINT ( 'NONE',  ( 9.028840231696797503, 12.62106513936658203, -1.199719254218446718 ) ) ;
#83780 = CARTESIAN_POINT ( 'NONE',  ( 3.625696855625531345, 1.816486592755601315, -0.4036080491761192546 ) ) ;
#83781 = CARTESIAN_POINT ( 'NONE',  ( 8.646349277213076334, 11.11049346154719508, 1.599625672291281386 ) ) ;
#83782 = DIRECTION ( 'NONE',  ( -0.000000000000000000, -1.000000000000000000, -0.000000000000000000 ) ) ;
#83783 = CARTESIAN_POINT ( 'NONE',  ( -4.613852347352193739, 4.277249248199312071, 1.214306433183764966E-14 ) ) ;
#83784 = CARTESIAN_POINT ( 'NONE',  ( -6.509886312855995172, 10.74661779830734254, -0.7998128361456291469 ) ) ;
#83785 = CARTESIAN_POINT ( 'NONE',  ( 6.631718597260928050, -1.344210725561691300, -1.562263648894322898 ) ) ;
#83787 = CARTESIAN_POINT ( 'NONE',  ( -4.596643646408070438, 7.147595147647359148, 1.363028123281652793 ) ) ;
#83786 = CARTESIAN_POINT ( 'NONE',  ( -6.237633190739009237, 9.434933268240943249, 1.199719254218452047 ) ) ;
#83788 = CARTESIAN_POINT ( 'NONE',  ( 0.6823417656249882723, -0.9072916663252494907, 1.181850606188755259 ) ) ;
#83789 = CARTESIAN_POINT ( 'NONE',  ( 1.387607149621207236, -0.04906231267952190778, 1.733339852973712292 ) ) ;
#83790 = CARTESIAN_POINT ( 'NONE',  ( 1.464397578914914400, 0.1305661322733233098, -1.735479185401978208 ) ) ;
#83792 = CARTESIAN_POINT ( 'NONE',  ( 6.792271770766432404, 10.86814146596211472, 1.040834085586084257E-14 ) ) ;
#83791 = CARTESIAN_POINT ( 'NONE',  ( 6.252564486485036710, 0.7173172151448119482, 2.193443857502775263 ) ) ;
#83793 = CARTESIAN_POINT ( 'NONE',  ( 2.891631901464575272, 6.595597328342462262, 0.000000000000000000 ) ) ;
#83794 = CARTESIAN_POINT ( 'NONE',  ( 1.563821040897996895, 2.030780823367520416, -0.3493207144565529942 ) ) ;
#83795 = CARTESIAN_POINT ( 'NONE',  ( 5.250031796989762967, 7.148123067953287446, 1.599625672291267398 ) ) ;
#83796 = EDGE_CURVE ( 'NONE', #129718, #95637, #90470, .T. ) ;
#83797 = CARTESIAN_POINT ( 'NONE',  ( 6.327535152267887320, -1.632159162827769405, 1.618470562452605455 ) ) ;
#83798 = CARTESIAN_POINT ( 'NONE',  ( 1.737499999999999378, -1.516666666666666163, -3.009438278150925683 ) ) ;
#83799 = CARTESIAN_POINT ( 'NONE',  ( -4.098307573080856692, 8.003385611894792362, 0.7998128361456352531 ) ) ;
#83800 = CARTESIAN_POINT ( 'NONE',  ( 0.4968692282744023303, 1.640418903650592508, -1.093199247851096789 ) ) ;
#83802 = CARTESIAN_POINT ( 'NONE',  ( -6.943184063974178422, 8.233374508458908281, -1.082531754730549967 ) ) ;
#83801 = CARTESIAN_POINT ( 'NONE',  ( 4.623256175466385010, 1.666654777633369555, 0.9376445158523971646 ) ) ;
#83803 = CARTESIAN_POINT ( 'NONE',  ( 6.445939570963194143, 0.8488519614954292969, -2.037301952897092594 ) ) ;
#83804 = CARTESIAN_POINT ( 'NONE',  ( -7.047292192037971859, -5.787795860784245683, -7.664865541498026680 ) ) ;
#83805 = CARTESIAN_POINT ( 'NONE',  ( 3.512971199272317602, 6.152197928242737923, -1.082531754730549967 ) ) ;
#83806 = ADVANCED_FACE ( 'NONE', ( #22139 ), #5896, .T. ) ;
#83807 = CARTESIAN_POINT ( 'NONE',  ( -4.678972410047611774, 5.591794245544547515, 1.082531754730549078 ) ) ;
#83808 = CARTESIAN_POINT ( 'NONE',  ( 0.2057307448365216507, 1.498047248056989522, 1.354806506954453482 ) ) ;
#83809 = CARTESIAN_POINT ( 'NONE',  ( 3.417284581939382448, 2.085149140145211799, 0.9887805580795704374 ) ) ;
#83810 = CARTESIAN_POINT ( 'NONE',  ( 5.301206097546149465, -1.683542251207278628, 1.007010407901312465 ) ) ;
#83811 = CARTESIAN_POINT ( 'NONE',  ( 1.762477828903946442, -0.7011357286515782494, -1.832381215946830011 ) ) ;
#83812 = CARTESIAN_POINT ( 'NONE',  ( 2.236732156574683827, 5.553345249405011508, 1.040834085586084257E-14 ) ) ;
#83813 = CARTESIAN_POINT ( 'NONE',  ( -9.351030441618698674, 15.43943296112659880, 7.441731298566530484 ) ) ;
#83814 = VERTEX_POINT ( 'NONE', #14448 ) ;
#83815 = CARTESIAN_POINT ( 'NONE',  ( 0.5325983862809284819, 0.6208049431430485710, 2.024263306480874380 ) ) ;
#83817 = CARTESIAN_POINT ( 'NONE',  ( -7.995557903757128493, 10.35123685918189729, 1.599625672291295375 ) ) ;
#83816 = CARTESIAN_POINT ( 'NONE',  ( -4.076197739202962467, 7.907314462378773001, 1.040834085586084257E-14 ) ) ;
#83818 = CARTESIAN_POINT ( 'NONE',  ( 0.2867153840934756337, 1.362228626754984573, 1.238794746348782505 ) ) ;
#83819 = CARTESIAN_POINT ( 'NONE',  ( 4.663029205760478746, 1.682383395889605282, -1.372325453836314768 ) ) ;
#83820 = CARTESIAN_POINT ( 'NONE',  ( 9.472440634255924863, 13.10139178464343424, -7.368143507540152015 ) ) ;
#83821 = CARTESIAN_POINT ( 'NONE',  ( 2.109781586379317897, 1.642293606977158538, 1.341614810521203349 ) ) ;
#83822 = CARTESIAN_POINT ( 'NONE',  ( -0.7500000000000215383, 3.222916667349487341, 1.299038105676671107 ) ) ;
#83823 = CARTESIAN_POINT ( 'NONE',  ( 8.703444544968814256, 12.24143683818393313, -1.199719254218446718 ) ) ;
#83824 = CARTESIAN_POINT ( 'NONE',  ( 11.89835103415199313, 13.82893085832465552, -1.561208891256347986 ) ) ;
#83825 = CARTESIAN_POINT ( 'NONE',  ( 6.533654944624902150, 6.813559398729744032, -0.4760831665120857648 ) ) ;
#83826 = CARTESIAN_POINT ( 'NONE',  ( 2.126313425470290674, 1.189129703756890644, -1.682874868902742405 ) ) ;
#83828 = CARTESIAN_POINT ( 'NONE',  ( 8.370495502396751775, 14.07684108737213080, -8.536638310158815912 ) ) ;
#83827 = CARTESIAN_POINT ( 'NONE',  ( -9.365985188942097750, 9.821404230054264772, 0.7998128361456462443 ) ) ;
#83829 = CARTESIAN_POINT ( 'NONE',  ( 0.6823417656249899377, 1.592708333674752730, 1.181850606188755259 ) ) ;
#83830 = CARTESIAN_POINT ( 'NONE',  ( -0.02264175331115856477, -0.002534049983802035520, -2.089079740194145440 ) ) ;
#83831 = LINE ( 'NONE', #149923, #56410 ) ;
#83832 = ORIENTED_EDGE ( 'NONE', *, *, #132234, .F. ) ;
#83833 = CARTESIAN_POINT ( 'NONE',  ( 4.195896582043898704, 1.251535281948525036, 1.445917311372606262 ) ) ;
#83834 = AXIS2_PLACEMENT_3D ( 'NONE', #140374, #24427, #206391 ) ;
#83835 = CARTESIAN_POINT ( 'NONE',  ( 11.80235830595198543, 12.30000000000000071, -1.696088231482801856 ) ) ;
#83836 = CARTESIAN_POINT ( 'NONE',  ( 1.107111304455286049, 1.712943910497457756, -1.478075018494163118 ) ) ;
#83837 = VECTOR ( 'NONE', #50032, 1000.000000000000000 ) ;
#83838 = CARTESIAN_POINT ( 'NONE',  ( -2.279742385392243165, 5.811449882932888222, -0.7998128361456281477 ) ) ;
#83840 = EDGE_CURVE ( 'NONE', #11451, #146910, #41375, .T. ) ;
#83839 = CARTESIAN_POINT ( 'NONE',  ( 1.283166710957379220, 0.1313358247177751625, -1.806845861898898953 ) ) ;
#83841 = CARTESIAN_POINT ( 'NONE',  ( 2.518635572904056374, 0.2389622604833125386, 1.900711705027556153 ) ) ;
#83842 = CARTESIAN_POINT ( 'NONE',  ( 2.875506610227479332, -0.2054619808779626633, 2.060159609288146232 ) ) ;
#83843 = CARTESIAN_POINT ( 'NONE',  ( -0.6823417656250212460, 1.863541667008083991, 1.181850606188755259 ) ) ;
#83844 = CARTESIAN_POINT ( 'NONE',  ( 0.5496082175940236736, 0.6205544711120424273, -1.871312427623121000 ) ) ;
#83845 = CARTESIAN_POINT ( 'NONE',  ( 4.986905038743431717, -0.2377927182869009337, -1.911709049817163164 ) ) ;
#83847 = CARTESIAN_POINT ( 'NONE',  ( 6.373787108001086388, 6.824503602047865769, -0.5760177672454840359 ) ) ;
#83846 = CARTESIAN_POINT ( 'NONE',  ( 0.5226545517994193313, -1.239659060731788998, -1.946298918093934960 ) ) ;
#83848 = CARTESIAN_POINT ( 'NONE',  ( 1.364683531249988535, 1.863541667008086211, 0.7879004041258500513 ) ) ;
#83849 = CARTESIAN_POINT ( 'NONE',  ( 4.844214494511547286, -0.9753611933653669741, 1.817521503207474076 ) ) ;
#83850 = CARTESIAN_POINT ( 'NONE',  ( -6.898401231254901234, 6.942556279419168419, -0.7998128361456291469 ) ) ;
#83851 = CARTESIAN_POINT ( 'NONE',  ( 9.101601193475611140, 9.512956235343358102, -0.7998128361456221525 ) ) ;
#83852 = CARTESIAN_POINT ( 'NONE',  ( 3.284841267552055299, 6.405332120898776793, -0.9495590844852133117 ) ) ;
#83854 = CARTESIAN_POINT ( 'NONE',  ( -0.7500000000000215383, 3.441666666666689967, 1.299038105676671107 ) ) ;
#83853 = CARTESIAN_POINT ( 'NONE',  ( 5.210040546657988436, -2.096114648464560748, 0.2032773619186321323 ) ) ;
#83855 = EDGE_CURVE ( 'NONE', #173182, #171829, #27514, .T. ) ;
#83856 = CARTESIAN_POINT ( 'NONE',  ( 1.258521197368984268, -2.171350058325251187, -0.0004004535333074903960 ) ) ;
#83857 = CARTESIAN_POINT ( 'NONE',  ( -0.6823417656250003738, 2.530208333674753618, -1.181850606188749264 ) ) ;
#83858 = CARTESIAN_POINT ( 'NONE',  ( 5.009125465012424172, 1.878017946038791575, 1.070212309444783294 ) ) ;
#83859 = CARTESIAN_POINT ( 'NONE',  ( 5.654946514622759324, 0.3960909877551482827, 1.980269227310478275 ) ) ;
#83860 = DIRECTION ( 'NONE',  ( -1.000000000000000000, 0.000000000000000000, 0.000000000000000000 ) ) ;
#83863 = CARTESIAN_POINT ( 'NONE',  ( 4.961921032921539521, 7.772363057508363759, -1.082531754730549078 ) ) ;
#83862 = CARTESIAN_POINT ( 'NONE',  ( 0.000000000000000000, -2.646874999522040639, -3.793834371823813001 ) ) ;
#83861 = CARTESIAN_POINT ( 'NONE',  ( 5.528692779322568640, 9.672168352510192690, 0.7998128361456341429 ) ) ;
#83864 = CARTESIAN_POINT ( 'NONE',  ( -4.444040490229335560, 8.406740681901359480, 0.7998128361456352531 ) ) ;
#83865 = CARTESIAN_POINT ( 'NONE',  ( 3.942592416894859841, -1.490970858180175940, 1.357867534901323614 ) ) ;
#83866 = CARTESIAN_POINT ( 'NONE',  ( -7.828943636887387925, 11.22118577875556156, 1.199719254218453823 ) ) ;
#83868 = DIRECTION ( 'NONE',  ( 0.1470157664651973450, 0.7071067811865536790, -0.6916548014802195166 ) ) ;
#83867 = CARTESIAN_POINT ( 'NONE',  ( -4.274898507010545856, 3.881803101134051470, -0.7998128361456221525 ) ) ;
#83869 = CARTESIAN_POINT ( 'NONE',  ( -0.6823417656249969321, 4.467708333674755394, -1.181850606188749264 ) ) ;
#83871 = FACE_OUTER_BOUND ( 'NONE', #39026, .T. ) ;
#83870 = CARTESIAN_POINT ( 'NONE',  ( 4.627887939457571598, -1.327398817707679868, -1.706084338546076662 ) ) ;
#83872 = CYLINDRICAL_SURFACE ( 'NONE', #125720, 1.500000000000000222 ) ;
#83874 = CARTESIAN_POINT ( 'NONE',  ( 5.694935465533643715, 1.779635825068434984, 0.9480254120717497290 ) ) ;
#83873 = CARTESIAN_POINT ( 'NONE',  ( -8.324343128666356506, 8.814081192973304724, 1.040834085586084257E-14 ) ) ;
#83875 = CARTESIAN_POINT ( 'NONE',  ( 1.499999999999990896, 5.775000000000023448, 1.040834085586084257E-14 ) ) ;
#83876 = CARTESIAN_POINT ( 'NONE',  ( 0.8204219880046401681, 1.592052673282555286, 0.6642659308724234712 ) ) ;
#83877 = CARTESIAN_POINT ( 'NONE',  ( 3.953084306836263995, 6.769626237021087789, 1.199719254218452047 ) ) ;
#83878 = AXIS2_PLACEMENT_3D ( 'NONE', #91418, #90335, #59956 ) ;
#83880 = CARTESIAN_POINT ( 'NONE',  ( 5.345657705538078730, 9.458627433094950021, 0.7998128361456331437 ) ) ;
#83879 = CARTESIAN_POINT ( 'NONE',  ( 6.629573927402440781, 10.67832731537079383, 1.040834085586084257E-14 ) ) ;
#83881 = CARTESIAN_POINT ( 'NONE',  ( -10.50060100873255031, 5.377693802073524765, 5.808388628131299747 ) ) ;
#83882 = CARTESIAN_POINT ( 'NONE',  ( 6.010993879215096314, 1.649516084216671397, 0.8821100558755521348 ) ) ;
#83883 = CARTESIAN_POINT ( 'NONE',  ( 0.1002437576986033446, -0.9471954198254585178, 1.776316830230479260 ) ) ;
#83884 =( NAMED_UNIT ( * ) PLANE_ANGLE_UNIT ( ) SI_UNIT ( $, .RADIAN. ) );
#83885 = CARTESIAN_POINT ( 'NONE',  ( -7.404161286394468355, 7.810812053647902431, 0.000000000000000000 ) ) ;
#83886 = VERTEX_POINT ( 'NONE', #161803 ) ;
#83888 = CARTESIAN_POINT ( 'NONE',  ( 1.282827611874960416, 1.646826022920354848, -1.163289555428485667 ) ) ;
#83887 = CARTESIAN_POINT ( 'NONE',  ( 1.752743329737327826, 2.097873456429504735, 0.3079802404963859486 ) ) ;
#83889 = CARTESIAN_POINT ( 'NONE',  ( 2.777393361597128685, 0.2615887081860277519, -1.792441719956331170 ) ) ;
#83890 = CARTESIAN_POINT ( 'NONE',  ( 6.607619761813720238, 8.802252036906432764, 1.599625672291268286 ) ) ;
#83891 = CARTESIAN_POINT ( 'NONE',  ( 6.772347375734490527, -1.334533509509854943, 1.701269717329929820 ) ) ;
#83892 = CARTESIAN_POINT ( 'NONE',  ( 6.856673000209174695, 9.022537805042615489, 1.599625672291281386 ) ) ;
#83893 = AXIS2_PLACEMENT_3D ( 'NONE', #130075, #197112, #147320 ) ;
#83895 = CARTESIAN_POINT ( 'NONE',  ( 0.7959256443332961561, -0.8641892358523853845, -1.709830222631677943 ) ) ;
#83894 = CARTESIAN_POINT ( 'NONE',  ( -5.525111292768871252, 6.404716915440499037, -1.199719254218446718 ) ) ;
#83896 = VECTOR ( 'NONE', #125218, 1000.000000000000114 ) ;
#83897 = CARTESIAN_POINT ( 'NONE',  ( -1.499999999999996669, 5.129166666666691299, -0.8660254037844395958 ) ) ;
#83898 =( NAMED_UNIT ( * ) PLANE_ANGLE_UNIT ( ) SI_UNIT ( $, .RADIAN. ) );
#83899 = CARTESIAN_POINT ( 'NONE',  ( 4.785665035499516051, 8.527100274817353665, -0.7216878364870207285 ) ) ;
#83900 = CARTESIAN_POINT ( 'NONE',  ( -1.364683531250014514, 0.3010416670080866552, -0.7879004041258359514 ) ) ;
#83901 = CARTESIAN_POINT ( 'NONE',  ( 2.399429999938675007, 5.743159399996332404, 0.000000000000000000 ) ) ;
#83902 = CARTESIAN_POINT ( 'NONE',  ( -8.462260433223891098, 13.02438760540324481, -0.7998128361456281477 ) ) ;
#83903 = CARTESIAN_POINT ( 'NONE',  ( 3.977527890101069996, 2.036293384626610248, -0.7259696361804208742 ) ) ;
#83904 = CARTESIAN_POINT ( 'NONE',  ( -5.099275172515603138, 8.002885897026576600, 1.082531754730549967 ) ) ;
#83905 = CARTESIAN_POINT ( 'NONE',  ( 6.373741612200174878, 6.608655767087927124, 0.7216878364870328300 ) ) ;
#83906 = CARTESIAN_POINT ( 'NONE',  ( 2.039458538997685366, 0.004855507148140979744, 2.120778211687989856 ) ) ;
#83907 = CARTESIAN_POINT ( 'NONE',  ( 6.668987789458199700, -1.670617902683011025, -0.7365018021969899076 ) ) ;
#83908 = CARTESIAN_POINT ( 'NONE',  ( 2.794160851653566535, -1.965818266918018864, -0.1488234875552247316 ) ) ;
#83909 = CARTESIAN_POINT ( 'NONE',  ( 5.431871263539022721, -1.864374737420209760, 0.4251265778823994368 ) ) ;
#83910 = VERTEX_POINT ( 'NONE', #110970 ) ;
#83911 = CARTESIAN_POINT ( 'NONE',  ( 3.511198596259283544, 6.271927390929313617, -7.499999999999997335 ) ) ;
#83912 = CARTESIAN_POINT ( 'NONE',  ( 5.916450756658795385, 0.7966118609284984498, 1.801439653064011548 ) ) ;
#83913 = CARTESIAN_POINT ( 'NONE',  ( 1.007640649619114148, -0.8727987561519714443, -1.734835989144311919 ) ) ;
#83914 = VERTEX_POINT ( 'NONE', #194285 ) ;
#83915 = CARTESIAN_POINT ( 'NONE',  ( -4.984557751679625781, 5.844347460828191565, 1.199719254218452935 ) ) ;
#83917 = CARTESIAN_POINT ( 'NONE',  ( 6.016786309414542622, 10.24161080428416426, 0.7998128361456341429 ) ) ;
#83916 = CARTESIAN_POINT ( 'NONE',  ( -7.621091744657483069, 8.063897588288083895, 0.7216878364870317197 ) ) ;
#83918 = CARTESIAN_POINT ( 'NONE',  ( 5.770966940911189447, 9.884545197705074671, -0.7998128361456291469 ) ) ;
#83921 = EDGE_CURVE ( 'NONE', #19237, #36083, #196341, .T. ) ;
#83920 = CARTESIAN_POINT ( 'NONE',  ( 3.702785349863636277, 7.334016984900627811, -0.7216878364870338292 ) ) ;
#83919 = CARTESIAN_POINT ( 'NONE',  ( 6.877010230629674759, 9.046264573866535486, 1.599625672291281386 ) ) ;
#83923 = ORIENTED_EDGE ( 'NONE', *, *, #103873, .T. ) ;
#83922 = CARTESIAN_POINT ( 'NONE',  ( 6.094389051209717856, -1.018956457145767436, 1.618003106988876283 ) ) ;
#83924 = CARTESIAN_POINT ( 'NONE',  ( 3.739080281021702312, 0.3231575147602770426, 2.182976880621155136 ) ) ;
#83925 = MECHANICAL_DESIGN_GEOMETRIC_PRESENTATION_REPRESENTATION (  '', ( #35529 ), #59820 ) ;
#83926 = CARTESIAN_POINT ( 'NONE',  ( 2.134064618640969524, -1.441378300436758630, -1.671108464803609417 ) ) ;
#83927 = DIRECTION ( 'NONE',  ( 8.881784197001252323E-16, 0.000000000000000000, 1.000000000000000000 ) ) ;
#83928 = CARTESIAN_POINT ( 'NONE',  ( 0.5043727151736315806, -1.897847990334254886, -0.2338014693106793551 ) ) ;
#83929 = CARTESIAN_POINT ( 'NONE',  ( 0.2663167167780124411, -9.037303891206541095, -9.496500708127754820 ) ) ;
#83930 = CARTESIAN_POINT ( 'NONE',  ( 8.563946585326370098, 13.14302144952281814, 0.7998128361456462443 ) ) ;
#83931 = CARTESIAN_POINT ( 'NONE',  ( 3.543477799061961253, 1.872898848466747479, -0.8826743078152868849 ) ) ;
#83932 = CARTESIAN_POINT ( 'NONE',  ( -5.870844209917351009, 6.808071985447069707, -1.199719254218446718 ) ) ;
#83933 = CARTESIAN_POINT ( 'NONE',  ( -6.325812300595961446, 6.871976577178664058, 0.6903976412777796945 ) ) ;
#83935 = CARTESIAN_POINT ( 'NONE',  ( 1.762795743007524063, -1.528684080660724920, 1.528680807790387286 ) ) ;
#83934 = CARTESIAN_POINT ( 'NONE',  ( -4.939248034080176097, 4.656877549381960080, 1.214306433183764966E-14 ) ) ;
#83936 = CARTESIAN_POINT ( 'NONE',  ( 3.421585747727782678, -1.306972202059282218, -1.759028276249123168 ) ) ;
#83937 = CARTESIAN_POINT ( 'NONE',  ( -1.225000000000001865, 0.7291666666666755114, -0.7072540797572917093 ) ) ;
#83938 = CARTESIAN_POINT ( 'NONE',  ( 4.312902262922978736, 5.164712407232485702, -1.082531754730548412 ) ) ;
#83939 = CARTESIAN_POINT ( 'NONE',  ( 1.499999999999822586, 7.176846818246208848, 4.202462424328222035 ) ) ;
#83940 = CARTESIAN_POINT ( 'NONE',  ( 1.364683531249996529, 14.77604166700806410, 0.7879004041258405033 ) ) ;
#83941 = CARTESIAN_POINT ( 'NONE',  ( -5.764151584465413869, 6.753873599078290546, -1.199719254218453823 ) ) ;
#83942 = CARTESIAN_POINT ( 'NONE',  ( 6.416678112323896954, -1.140949303232444478, -1.306061676789990855 ) ) ;
#83943 = CARTESIAN_POINT ( 'NONE',  ( -10.46653140006992899, 11.31330084294416771, -0.7216878364870267237 ) ) ;
#83944 = CARTESIAN_POINT ( 'NONE',  ( 3.696198088285786998, 0.9351842759567146057, -1.847102243037239910 ) ) ;
#83945 = CARTESIAN_POINT ( 'NONE',  ( 5.853141746508254251, 0.1553614259057617408, -2.111562834372962438 ) ) ;
#83946 = CARTESIAN_POINT ( 'NONE',  ( 6.582647274634798151, 7.638508894284114170, 1.199719254218462483 ) ) ;
#83947 = CARTESIAN_POINT ( 'NONE',  ( -1.364683531249997417, 5.259375000341425022, 1.214306433183764966E-14 ) ) ;
#83948 = CARTESIAN_POINT ( 'NONE',  ( 2.869919493663297683, -1.948696178941822899, 0.2840860843679354764 ) ) ;
#83949 = CARTESIAN_POINT ( 'NONE',  ( 1.177825114000274898, 1.883588471398514264, -0.3297955356276888184 ) ) ;
#83950 = CARTESIAN_POINT ( 'NONE',  ( 6.456980045808101032, 0.3985590825250818203, -2.257207781175464056 ) ) ;
#83951 = CARTESIAN_POINT ( 'NONE',  ( 3.404746562951190381, 1.438594061741470753, -1.123979961188771304 ) ) ;
#83952 = EDGE_CURVE ( 'NONE', #6371, #54971, #151695, .T. ) ;
#83953 = CARTESIAN_POINT ( 'NONE',  ( 5.225741863424510747, 5.061396693608882558, 0.7998128361456352531 ) ) ;
#83954 = CARTESIAN_POINT ( 'NONE',  ( 4.487385655998878953, 6.258369236797239665, 1.443375672974062551 ) ) ;
#83955 = CARTESIAN_POINT ( 'NONE',  ( -7.366157530926372488, 7.488271962369228874, -0.7998128361456291469 ) ) ;
#83956 = VERTEX_POINT ( 'NONE', #209444 ) ;
#83957 = ORIENTED_EDGE ( 'NONE', *, *, #127735, .F. ) ;
#83958 = CARTESIAN_POINT ( 'NONE',  ( 4.412362193956616885, -2.012844744014946841, -0.04520991500436136873 ) ) ;
#83959 =( BOUNDED_SURFACE ( )  B_SPLINE_SURFACE ( 3, 2, ( 
 ( #126919, #172392, #142047 ),
 ( #27185, #122663, #189689 ),
 ( #192877, #174542, #93291 ),
 ( #73812, #188626, #139906 ),
 ( #107449, #44532, #108515 ),
 ( #156146, #26118, #92229 ) ),
 .UNSPECIFIED., .F., .F., .T. ) 
 B_SPLINE_SURFACE_WITH_KNOTS ( ( 4, 2, 4 ),
 ( 3, 3 ),
 ( 0.000000000000000000, 0.0003831327362561326704, 0.0007662654725122653408 ),
 ( 0.000000000000000000, 1.000000000000000000 ),
 .UNSPECIFIED. ) 
 GEOMETRIC_REPRESENTATION_ITEM ( )  RATIONAL_B_SPLINE_SURFACE ( (
 ( 1.000000000000000000, 0.5879095031487664436, 1.000000000000000000),
 ( 1.000000000000000000, 0.5873691247585943742, 1.000000000000000000),
 ( 1.000000000000000000, 0.6054349545487748285, 1.000000000000000000),
 ( 1.000000000000000000, 0.6533334602776329492, 1.000000000000000000),
 ( 1.000000000000000000, 0.6828746263143679052, 1.000000000000000000),
 ( 1.000000000000000000, 0.7071067811865475727, 1.000000000000000000) ) ) 
 REPRESENTATION_ITEM ( '' )  SURFACE ( )  );
#83960 = CARTESIAN_POINT ( 'NONE',  ( 4.100408672059585591, 1.951911038179511726, 0.1965976633130430695 ) ) ;
#83961 = CARTESIAN_POINT ( 'NONE',  ( -8.369460898337653276, 8.658792557682392754, 0.7998128361456462443 ) ) ;
#83962 = CARTESIAN_POINT ( 'NONE',  ( -5.949330478298285207, 5.835307067636438028, 0.7998128361456341429 ) ) ;
#83963 = CARTESIAN_POINT ( 'NONE',  ( 0.1753634416057497647, 4.084635187426246539, -2.698744815386323381 ) ) ;
#83965 = CARTESIAN_POINT ( 'NONE',  ( 5.260532772634206822, -1.280100971201453497, 1.222426461919926322 ) ) ;
#83964 = CARTESIAN_POINT ( 'NONE',  ( 0.4332924875789189167, -1.481350984940564830, -1.475676199967065338 ) ) ;
#83966 = CARTESIAN_POINT ( 'NONE',  ( 10.93220419382046416, -5.754340240174431464, -5.996486861200787814E-16 ) ) ;
#83967 = CARTESIAN_POINT ( 'NONE',  ( 1.922082643403967506, 1.260107670313360240, -1.792737600334909365 ) ) ;
#83968 = CARTESIAN_POINT ( 'NONE',  ( 0.04591871184063747030, -1.399829139283098822, 1.033961902999945170 ) ) ;
#83969 = CARTESIAN_POINT ( 'NONE',  ( 8.098297826064319693, 8.342435640030188893, 0.7998128361456481317 ) ) ;
#83970 = CARTESIAN_POINT ( 'NONE',  ( 0.1333692844072559280, 6.947498546895843674, -2.648624074793118233 ) ) ;
#83971 = CARTESIAN_POINT ( 'NONE',  ( 0.3809451599157384627, 1.611386624718774918, -0.6158283211408090985 ) ) ;
#83972 = CARTESIAN_POINT ( 'NONE',  ( 1.142455020822298106, -0.05817821010643645790, -2.297781139197229372 ) ) ;
#83973 =( BOUNDED_CURVE ( )  B_SPLINE_CURVE ( 2, ( #126777, #61691, #160257, #174399, #44390, #74744, #110511 ),
 .UNSPECIFIED., .F., .T. ) 
 B_SPLINE_CURVE_WITH_KNOTS ( ( 3, 2, 2, 3 ),
 ( 0.2624999999999999001, 0.2666666666666666075, 0.2708333333333333148, 0.2750000000000000777 ),
 .UNSPECIFIED. ) 
 CURVE ( )  GEOMETRIC_REPRESENTATION_ITEM ( )  RATIONAL_B_SPLINE_CURVE ( ( 1.000000000000003553, 0.8660254037844351549, 1.000000000000000000, 0.8660254037844387076, 1.000000000000000000, 0.8660254037844369313, 1.000000000000001776 ) ) 
 REPRESENTATION_ITEM ( '' )  );
#83974 = CARTESIAN_POINT ( 'NONE',  ( 0.7674258922165803076, 2.110627382301712540, -0.5898035449652739848 ) ) ;
#83975 = CARTESIAN_POINT ( 'NONE',  ( 6.397740202767369766, 0.1737558121157663782, 1.725068634017632885 ) ) ;
#83976 = CARTESIAN_POINT ( 'NONE',  ( 2.754729969050898841, 0.7443088323898851000, 2.077706851784946185 ) ) ;
#83977 = CIRCLE ( 'NONE', #142793, 2.500000000000007994 ) ;
#83978 = CARTESIAN_POINT ( 'NONE',  ( 0.5148107762544695820, 0.8296010825015688317, 2.006500992472683098 ) ) ;
#83979 = CARTESIAN_POINT ( 'NONE',  ( 1.973964399615803389, -0.9004667817871301327, 1.916432390954267984 ) ) ;
#83980 = CARTESIAN_POINT ( 'NONE',  ( 6.719405205105350554, -7.217450603038201962, -6.716119544744036496 ) ) ;
#83981 = CARTESIAN_POINT ( 'NONE',  ( 5.368162667233546514, 0.9496366811117643580, 1.675975028240711540 ) ) ;
#83982 = VERTEX_POINT ( 'NONE', #30738 ) ;
#83984 = CARTESIAN_POINT ( 'NONE',  ( -1.364683531250014514, -0.9072916663252470482, 0.7879004041258379498 ) ) ;
#83983 = CARTESIAN_POINT ( 'NONE',  ( 2.121020962670455923, 0.004254578539099414594, 2.292545472008022056 ) ) ;
#83985 = CARTESIAN_POINT ( 'NONE',  ( 2.523789150438203510, 6.096171108819874007, 0.7998128361456462443 ) ) ;
#83986 = CARTESIAN_POINT ( 'NONE',  ( 5.840865249388943248, 5.708764300575555062, 0.7998128361456341429 ) ) ;
#83987 = CARTESIAN_POINT ( 'NONE',  ( 4.512477240926440203, -2.220771887297602110, -0.05487108470654011860 ) ) ;
#83988 = CARTESIAN_POINT ( 'NONE',  ( -7.917598520700757980, 9.299915031314755609, 1.082531754730558626 ) ) ;
#83989 = EDGE_CURVE ( 'NONE', #69637, #200355, #98138, .T. ) ;
#83990 = CARTESIAN_POINT ( 'NONE',  ( 0.3388969742604112101, -7.666862915010149493, -10.99522790877599832 ) ) ;
#83991 = CARTESIAN_POINT ( 'NONE',  ( 6.168596704537822717, 6.299043698156668647, 1.040834085586084257E-14 ) ) ;
#83992 = CARTESIAN_POINT ( 'NONE',  ( -7.497295758232720431, 10.73030023703809555, -1.082531754730543083 ) ) ;
#83993 = CARTESIAN_POINT ( 'NONE',  ( 6.238160076063542725, 6.450477308261824305, -0.7216878364870458196 ) ) ;
#83994 = ORIENTED_EDGE ( 'NONE', *, *, #65201, .T. ) ;
#83995 = CARTESIAN_POINT ( 'NONE',  ( 3.322888845334175389, 0.9041102021897020613, -1.802417075407992897 ) ) ;
#83997 = CARTESIAN_POINT ( 'NONE',  ( 0.8837254586576195337, -1.959797800638187093, 0.6432524670345032280 ) ) ;
#83996 = CARTESIAN_POINT ( 'NONE',  ( 8.274553823041976841, 8.548067636504127265, 1.040834085586084257E-14 ) ) ;
#83998 = CARTESIAN_POINT ( 'NONE',  ( 5.139949632912227173, 8.050339434155988627, -1.082531754730548412 ) ) ;
#83999 = B_SPLINE_CURVE_WITH_KNOTS ( 'NONE', 3,
 ( #115704, #181695, #165460, #48533, #32271, #79943, #50646 ),
 .UNSPECIFIED., .F., .F.,
 ( 4, 3, 4 ),
 ( 0.000000000000000000, 0.0008000000000004425012, 0.002977368225425631489 ),
 .UNSPECIFIED. ) ;
#84000 = CARTESIAN_POINT ( 'NONE',  ( -2.303566469087102497, 5.490909403443315462, -0.7594041750639659583 ) ) ;
#84001 = CARTESIAN_POINT ( 'NONE',  ( -0.6823417656249969321, 3.467708333674754506, -1.181850606188749264 ) ) ;
#84002 = CARTESIAN_POINT ( 'NONE',  ( 4.400438482046089561, 1.694813852089768869, -1.389250428430639950 ) ) ;
#84003 = CARTESIAN_POINT ( 'NONE',  ( 1.547500230860882287, -1.423960469535384465, 1.427938386157491246 ) ) ;
#84004 = CARTESIAN_POINT ( 'NONE',  ( 0.8020088176248600931, 1.394402496181508466, -1.202495849378336423 ) ) ;
#84005 = CARTESIAN_POINT ( 'NONE',  ( 5.618756969397510126, -0.05950314066365805510, 2.291748599322357194 ) ) ;
#84006 = CARTESIAN_POINT ( 'NONE',  ( 3.995923475689294513, -0.5793754966058572986, -1.747668199984537152 ) ) ;
#84007 = CARTESIAN_POINT ( 'NONE',  ( 7.853197290813620945, 10.18514947741448573, 1.599625672291281386 ) ) ;
#84008 = CARTESIAN_POINT ( 'NONE',  ( 4.049673113991675955, 0.6152068410551281286, -1.718917501701062278 ) ) ;
#84009 = CARTESIAN_POINT ( 'NONE',  ( 4.922500090287251773, -1.427935867408920645, -1.423962988533589158 ) ) ;
#84010 = CARTESIAN_POINT ( 'NONE',  ( -7.167456763118792651, 11.51378332361394818, 0.000000000000000000 ) ) ;
#84012 = CARTESIAN_POINT ( 'NONE',  ( -6.363572996767778100, 8.517530811019446091, -1.599625672291271394 ) ) ;
#84011 = CARTESIAN_POINT ( 'NONE',  ( 4.592800228568824750, -0.4914316458759260264, -2.208360408168393629 ) ) ;
#84013 = CARTESIAN_POINT ( 'NONE',  ( -0.02264175331115856477, -0.002534049983802035520, -2.089079740194145440 ) ) ;
#84014 = CARTESIAN_POINT ( 'NONE',  ( -0.7500000000000215383, 4.222916667349481123, 1.299038105676671107 ) ) ;
#84015 = CARTESIAN_POINT ( 'NONE',  ( 4.809070886388271404, -1.664838503569150419, 1.230558894880565246 ) ) ;
#84016 = CARTESIAN_POINT ( 'NONE',  ( 9.053093885623066939, 11.58502883802551153, -1.599625672291262513 ) ) ;
#84017 = CARTESIAN_POINT ( 'NONE',  ( -1.360316468750026653, 2.192708333674788346, 0.7853790794158680422 ) ) ;
#84018 = SHAPE_DEFINITION_REPRESENTATION ( #64521, #62426 ) ;
#84020 = CARTESIAN_POINT ( 'NONE',  ( 2.262220261732431403, 0.8237980678013016034, 1.741618625116077235 ) ) ;
#84019 = CARTESIAN_POINT ( 'NONE',  ( -8.864333505236459132, 9.236143932397675727, 1.040834085586084257E-14 ) ) ;
#84021 = UNCERTAINTY_MEASURE_WITH_UNIT (LENGTH_MEASURE( 1.000000000000000082E-05 ), #70164, 'distance_accuracy_value', 'NONE');
#84022 = DIRECTION ( 'NONE',  ( 0.000000000000000000, 1.000000000000000000, 0.000000000000000000 ) ) ;
#84023 = CARTESIAN_POINT ( 'NONE',  ( 6.895365913452266682, -1.760736289220961481, 0.8823945077177670626 ) ) ;
#84024 = CARTESIAN_POINT ( 'NONE',  ( 4.706088717274906408, 5.623429937309770921, 1.082531754730549078 ) ) ;
#84025 = CARTESIAN_POINT ( 'NONE',  ( 4.499659979152191625, 7.015106111828595559, -1.153029749421132566 ) ) ;
#84026 = CARTESIAN_POINT ( 'NONE',  ( -4.762992037102518950, 4.451245552908022596, -0.7998128361456221525 ) ) ;
#84028 = CARTESIAN_POINT ( 'NONE',  ( 1.406790049154776234, -2.211310019597735987, -0.2114152780076440363 ) ) ;
#84027 = CARTESIAN_POINT ( 'NONE',  ( 0.5453776912951785460, 0.1620316879334358084, 2.114494688702214020 ) ) ;
#84029 = AXIS2_PLACEMENT_3D ( 'NONE', #114159, #80513, #180152 ) ;
#84030 = CARTESIAN_POINT ( 'NONE',  ( 3.329229500047115042, 0.04992189587533709533, 2.105534426424925165 ) ) ;
#84031 = CARTESIAN_POINT ( 'NONE',  ( -6.291865805193673111, 9.498204651771386509, -1.199719254218452047 ) ) ;
#84032 = CARTESIAN_POINT ( 'NONE',  ( 7.558834334818744338, 8.777393797832065303, 1.199719254218462483 ) ) ;
#84033 = CARTESIAN_POINT ( 'NONE',  ( 0.4493573998385214652, 1.374985906440568506, 1.254353302672887693 ) ) ;
#84034 = CARTESIAN_POINT ( 'NONE',  ( 5.099838337034727331, 9.101561826515851550, -0.7998128361456281477 ) ) ;
#84035 = CARTESIAN_POINT ( 'NONE',  ( -4.192242263785030509, 7.388029550104924681, -0.8017062249071702507 ) ) ;
#84036 = CARTESIAN_POINT ( 'NONE',  ( 4.039439701867726384, 6.800097854565950506, 1.199719254218462483 ) ) ;
#84037 = CARTESIAN_POINT ( 'NONE',  ( -5.885648082108231982, 7.959951743916638733, 1.443375672974058777 ) ) ;
#84038 = CARTESIAN_POINT ( 'NONE',  ( -8.541273586929371220, 9.067166727613487964, 0.7216878364870438212 ) ) ;
#84039 =( BOUNDED_SURFACE ( )  B_SPLINE_SURFACE ( 3, 2, ( 
 ( #52504, #103392, #55702 ),
 ( #185688, #117570, #36239 ),
 ( #1589, #37317, #101248 ),
 ( #168391, #21039, #87137 ),
 ( #102317, #171584, #4778 ),
 ( #51450, #70856, #121857 ),
 ( #38388, #22098, #183565 ),
 ( #3716, #135901, #201919 ) ),
 .UNSPECIFIED., .F., .F., .T. ) 
 B_SPLINE_SURFACE_WITH_KNOTS ( ( 4, 2, 2, 4 ),
 ( 3, 3 ),
 ( 0.000000000000000000, 0.0004401918256853558494, 0.0006602877385280337200, 0.0008803836513707116989 ),
 ( 0.000000000000000000, 1.000000000000000000 ),
 .UNSPECIFIED. ) 
 GEOMETRIC_REPRESENTATION_ITEM ( )  RATIONAL_B_SPLINE_SURFACE ( (
 ( 1.000000000000000000, 0.6787756258918318242, 1.000000000000000000),
 ( 1.000000000000000000, 0.6284487096092253866, 1.000000000000000000),
 ( 1.000000000000000000, 0.5704014816693694367, 1.000000000000000000),
 ( 1.000000000000000000, 0.4882303283124204696, 1.000000000000000000),
 ( 1.000000000000000000, 0.4617370933882668504, 1.000000000000000000),
 ( 1.000000000000000000, 0.4222438920368297710, 1.000000000000000000),
 ( 1.000000000000000000, 0.4105126989449011665, 1.000000000000000000),
 ( 1.000000000000000000, 0.4127341956165110348, 1.000000000000000000) ) ) 
 REPRESENTATION_ITEM ( '' )  SURFACE ( )  );
#84040 = CARTESIAN_POINT ( 'NONE',  ( 1.019968326173793960, -0.5097545255977399270, 2.058319881341897695 ) ) ;
#84041 = CARTESIAN_POINT ( 'NONE',  ( -4.613517410400161722, 8.604463755433990002, -0.7998128361456362523 ) ) ;
#84043 = CARTESIAN_POINT ( 'NONE',  ( 4.791432466842788784, -1.794507165602466037, 0.7932701521168731285 ) ) ;
#84042 = CARTESIAN_POINT ( 'NONE',  ( -1.225000000000002309, 0.7291666666666755114, -0.7072540797572917093 ) ) ;
#84044 = CARTESIAN_POINT ( 'NONE',  ( 3.713887418366210280, -2.130098009959373151, 0.3673708613747132534 ) ) ;
#84045 = CARTESIAN_POINT ( 'NONE',  ( 1.399689850468607277, -0.6632477835330424787, -1.717811453623831808 ) ) ;
#84046 = CARTESIAN_POINT ( 'NONE',  ( -4.034408581249735448, 7.597519823075112200, 0.2926387080343200164 ) ) ;
#84047 = CARTESIAN_POINT ( 'NONE',  ( -0.6823417656250246877, -0.8864583329919115684, 1.181850606188755259 ) ) ;
#84048 = EDGE_CURVE ( 'NONE', #14213, #73245, #42279, .T. ) ;
#84049 = CARTESIAN_POINT ( 'NONE',  ( 5.103314706128504241, -1.731452751257630096, 0.1754873227253881951 ) ) ;
#84050 = CARTESIAN_POINT ( 'NONE',  ( 0.6674790882333445641, 16.00000000000000711, -11.66566053519551005 ) ) ;
#84051 = CARTESIAN_POINT ( 'NONE',  ( 4.189106276942576201, 7.831115056500907556, 1.040834085586084257E-14 ) ) ;
#84052 = CARTESIAN_POINT ( 'NONE',  ( -10.12897898315521061, 6.154003805053667620, 5.673299828594959848 ) ) ;
#84053 = CARTESIAN_POINT ( 'NONE',  ( 2.184651956524386041, -2.119909832212972578, -0.4221607449544013679 ) ) ;
#84054 =( GEOMETRIC_REPRESENTATION_CONTEXT ( 3 ) GLOBAL_UNCERTAINTY_ASSIGNED_CONTEXT ( ( #28073 ) ) GLOBAL_UNIT_ASSIGNED_CONTEXT ( ( #48390, #112370, #165307 ) ) REPRESENTATION_CONTEXT ( 'NONE', 'WORKASPACE' ) );
#84055 = CARTESIAN_POINT ( 'NONE',  ( 3.813827237909522605, -1.649828814528127907, 1.158511658058670957 ) ) ;
#84056 = CARTESIAN_POINT ( 'NONE',  ( -9.368320956918621434, 11.95279375453699622, 1.443375672974076540 ) ) ;
#84058 = AXIS2_PLACEMENT_3D ( 'NONE', #109891, #143428, #175904 ) ;
#84057 = CARTESIAN_POINT ( 'NONE',  ( 1.499129196564863209, 1.767075381950654611, -1.244890797856931686 ) ) ;
#84059 = CARTESIAN_POINT ( 'NONE',  ( 3.748864756286158340, -1.612500686720008236, 1.134000162313458793 ) ) ;
#84060 = CARTESIAN_POINT ( 'NONE',  ( 3.720204347993858462, 1.845125290474887159, 0.6061553137183937068 ) ) ;
#84063 = ORIENTED_EDGE ( 'NONE', *, *, #27652, .F. ) ;
#84062 = DIRECTION ( 'NONE',  ( 0.2150645590070887347, -0.8781765503997437383, 0.4272624273056235267 ) ) ;
#84061 = CARTESIAN_POINT ( 'NONE',  ( -9.368320956918621434, 11.95279375453699622, 1.443375672974076540 ) ) ;
#84064 = CARTESIAN_POINT ( 'NONE',  ( -6.312203035614172286, 9.521931420595302953, -1.199719254218452047 ) ) ;
#84065 = CARTESIAN_POINT ( 'NONE',  ( 4.934241560730721510, 4.721313007132757811, 0.000000000000000000 ) ) ;
#84066 = ADVANCED_FACE ( 'NONE', ( #97878 ), #212210, .F. ) ;
#84067 = CARTESIAN_POINT ( 'NONE',  ( -4.411198876399886615, 6.239761003923544713, -1.599625672291271394 ) ) ;
#84069 = EDGE_LOOP ( 'NONE', ( #63742, #75788, #148613, #202992 ) ) ;
#84068 = CARTESIAN_POINT ( 'NONE',  ( -6.479871072688648148, 6.524547437750345402, 0.000000000000000000 ) ) ;
#84070 = CARTESIAN_POINT ( 'NONE',  ( -9.503902493055310430, 11.15060299906175167, 1.082531754730558626 ) ) ;
#84071 = CARTESIAN_POINT ( 'NONE',  ( 6.821333373144921275, -0.1693730316576994299, 2.270769535942236406 ) ) ;
#84072 = CARTESIAN_POINT ( 'NONE',  ( 0.000000000000000000, -2.996874999522043392, -3.793834371823813001 ) ) ;
#84073 = AXIS2_PLACEMENT_3D ( 'NONE', #77062, #44595, #95494 ) ;
#84074 = CARTESIAN_POINT ( 'NONE',  ( 5.049637047142223167, 1.450995767963231264, 1.320413740667214508 ) ) ;
#84075 = CARTESIAN_POINT ( 'NONE',  ( 1.336564801266389990, 0.5826540126645517459, -1.930418273149013153 ) ) ;
#84076 = ORIENTED_EDGE ( 'NONE', *, *, #211296, .T. ) ;
#84077 = CARTESIAN_POINT ( 'NONE',  ( 2.975892561826110505, -0.8538584053617600533, 1.937700190512989362 ) ) ;
#84078 = CARTESIAN_POINT ( 'NONE',  ( -0.7500000000000215383, 3.472916667349487785, 1.299038105676671107 ) ) ;
#84080 = CARTESIAN_POINT ( 'NONE',  ( -6.417086777969760902, 6.381022750586497594, 0.7998128361456341429 ) ) ;
#84079 = CARTESIAN_POINT ( 'NONE',  ( 9.499668754396997983, -7.215568602690315636, 0.07933194018460217045 ) ) ;
#84081 = CARTESIAN_POINT ( 'NONE',  ( 4.523293815724619193, -1.134750198001058585, -1.449786353205910538 ) ) ;
#84082 = VERTEX_POINT ( 'NONE', #163938 ) ;
#84083 = CARTESIAN_POINT ( 'NONE',  ( -8.188234707649510113, 11.64035869464474082, -1.199719254218446718 ) ) ;
#84085 = MANIFOLD_SOLID_BREP ( 'Fillet1', #212477 ) ;
#84084 = DIRECTION ( 'NONE',  ( 1.000000000000000000, -0.000000000000000000, -0.000000000000000000 ) ) ;
#84086 = CARTESIAN_POINT ( 'NONE',  ( 5.256147377898004791, 0.8573370980917979223, -1.939729252509444279 ) ) ;
#84087 = CARTESIAN_POINT ( 'NONE',  ( 0.000000000000000000, 0.08000000000000020983, 0.000000000000000000 ) ) ;
#84088 = CARTESIAN_POINT ( 'NONE',  ( 4.801558957534076022, 8.753569217098425170, 0.7998128361456462443 ) ) ;
#84089 = AXIS2_PLACEMENT_3D ( 'NONE', #188742, #121703, #204972 ) ;
#84090 = CARTESIAN_POINT ( 'NONE',  ( 5.958293153512181917, 0.8310434803317863217, 1.885964484847465705 ) ) ;
#84093 = CARTESIAN_POINT ( 'NONE',  ( 2.366542893654680402, 0.08848056876738576160, -1.839231530397527736 ) ) ;
#84092 = CARTESIAN_POINT ( 'NONE',  ( 1.082201983675265655, 1.112762242526295298, -1.491567265455741476 ) ) ;
#84091 = CARTESIAN_POINT ( 'NONE',  ( 0.000000000000000000, 8.920000000000001705, 2.080000000000000071 ) ) ;
#84094 = CARTESIAN_POINT ( 'NONE',  ( 8.422639742587595180, 10.84949900448412130, -1.599625672291268286 ) ) ;
#84095 = CARTESIAN_POINT ( 'NONE',  ( -1.364683531249997417, 5.759375000341418804, 1.214306433183764966E-14 ) ) ;
#84096 = DIRECTION ( 'NONE',  ( -0.000000000000000000, -1.000000000000000000, -0.000000000000000000 ) ) ;
#84097 = CARTESIAN_POINT ( 'NONE',  ( 1.224999999999971001, 2.187500000682782275, -4.683753385137379155E-14 ) ) ;
#84098 = CARTESIAN_POINT ( 'NONE',  ( 2.420803835572300500, 1.440536793087299205, -1.671967039616916617 ) ) ;
#84099 = CARTESIAN_POINT ( 'NONE',  ( 5.009165025557245521, 1.964990322317389015, 1.121224042300600576 ) ) ;
#84100 = CARTESIAN_POINT ( 'NONE',  ( -7.049876689426106680, 9.247942109129029475, -1.443375672974059665 ) ) ;
#84101 = CARTESIAN_POINT ( 'NONE',  ( 4.201270403262004294, 1.615401881959299235, -0.8201500932763347018 ) ) ;
#84102 = CARTESIAN_POINT ( 'NONE',  ( 5.225768846659354594, 0.7701814094057590765, -1.754262016157917881 ) ) ;
#84103 = CARTESIAN_POINT ( 'NONE',  ( -1.364683531250010295, 5.092708333674757171, 0.7879004041258379498 ) ) ;
#84104 = CARTESIAN_POINT ( 'NONE',  ( 3.889495165534775811, 1.427134975246695969, 1.360358076685687978 ) ) ;
#84105 = CARTESIAN_POINT ( 'NONE',  ( 5.471519871388384360, 1.802534880541529994, -0.5000026934619330454 ) ) ;
#84106 = CARTESIAN_POINT ( 'NONE',  ( 5.107777090148794663, 0.5842497386982176133, -1.767012650282340003 ) ) ;
#84107 = CARTESIAN_POINT ( 'NONE',  ( 5.752768645092715794, -1.392961553103783112, 1.091694246300749738 ) ) ;
#84109 = CARTESIAN_POINT ( 'NONE',  ( 1.348413808652969337, 2.103741849630758054, 0.1016320799899407962 ) ) ;
#84108 = CARTESIAN_POINT ( 'NONE',  ( -4.270455198180246548, 4.084545274072787890, 0.7216878364870317197 ) ) ;
#84110 = EDGE_CURVE ( 'NONE', #103298, #65129, #69519, .T. ) ;
#84111 = CARTESIAN_POINT ( 'NONE',  ( 9.236128959407556849, 11.79856975744075598, -1.599625672291262513 ) ) ;
#84113 = CARTESIAN_POINT ( 'NONE',  ( -1.284279953904132077, 2.878360285806111474, -0.7749999999999935829 ) ) ;
#84112 = DIRECTION ( 'NONE',  ( -0.6483454320283799088, 0.000000000000000000, 0.7613463080411786432 ) ) ;
#84114 = CARTESIAN_POINT ( 'NONE',  ( 3.621431001533811589, 1.820626359085864454, 1.087046460333654485 ) ) ;
#84115 = DIRECTION ( 'NONE',  ( 0.000000000000000000, 1.000000000000000000, 0.000000000000000000 ) ) ;
#84116 = CARTESIAN_POINT ( 'NONE',  ( 2.092062652781300880, 1.246029564253118282, 1.589516146451919631 ) ) ;
#84117 = CARTESIAN_POINT ( 'NONE',  ( 1.364683531249988757, 1.884375000341421913, 0.000000000000000000 ) ) ;
#84118 = CARTESIAN_POINT ( 'NONE',  ( -1.115562610750309283E-14, 10.31250000000000000, 1.500000000000001554 ) ) ;
#84119 = EDGE_CURVE ( 'NONE', #97605, #201490, #97231, .T. ) ;
#84120 = CARTESIAN_POINT ( 'NONE',  ( 3.822509244049070887, 6.547012320444182798, -1.199719254218452047 ) ) ;
#84121 = VERTEX_POINT ( 'NONE', #117366 ) ;
#84122 = CARTESIAN_POINT ( 'NONE',  ( 1.810078809455554438, -2.145489296895970011, 0.2626290421628638128 ) ) ;
#84123 = CARTESIAN_POINT ( 'NONE',  ( 6.890000000000012115, 1.205492346117660762, 2.388860368086835884 ) ) ;
#84126 = FACE_OUTER_BOUND ( 'NONE', #50957, .T. ) ;
#84125 = CARTESIAN_POINT ( 'NONE',  ( 11.94980361723080264, 10.09761943414563312, -1.099999926404445771 ) ) ;
#84124 = CARTESIAN_POINT ( 'NONE',  ( 3.898851692381625877, 6.706354853490643642, -1.199719254218452047 ) ) ;
#84127 = CARTESIAN_POINT ( 'NONE',  ( 9.531018800282598846, 12.14260790512831889, 1.443375672974076540 ) ) ;
#84128 = CARTESIAN_POINT ( 'NONE',  ( -7.952857047016746783, -6.836289462023503738, 7.401194801147176427 ) ) ;
#84129 = CARTESIAN_POINT ( 'NONE',  ( -7.890482213473404727, 8.307910125248191946, 0.7216878364870578100 ) ) ;
#84130 = CARTESIAN_POINT ( 'NONE',  ( 0.7498831369015904746, 2.188782640433343474, -0.1130235578899463078 ) ) ;
#84131 = CARTESIAN_POINT ( 'NONE',  ( 1.451998047844732964, 7.315968950354620581, 4.301760722576522866 ) ) ;
#84133 = CARTESIAN_POINT ( 'NONE',  ( -1.364683531250010740, 12.63020833367473372, 0.7879004041258445001 ) ) ;
#84132 = CARTESIAN_POINT ( 'NONE',  ( 1.323510708689378479, -0.05371019744930016770, 2.262043349595239228 ) ) ;
#84134 = CARTESIAN_POINT ( 'NONE',  ( -8.483651433849100698, 10.92067931095586886, 1.599625672291269396 ) ) ;
#84135 = CARTESIAN_POINT ( 'NONE',  ( -3.429849674132936066, 6.945315686556313040, -0.7216878364870257245 ) ) ;
#84136 = CARTESIAN_POINT ( 'NONE',  ( 0.6823417656249899377, 2.155208333674753174, 1.181850606188767472 ) ) ;
#84137 = CARTESIAN_POINT ( 'NONE',  ( 4.622017735560743468, 8.339529265130579461, 0.3277269337885590494 ) ) ;
#84138 = CARTESIAN_POINT ( 'NONE',  ( 0.7500000000000006661, 11.58333333333333393, 1.299038105676657340 ) ) ;
#84139 = CARTESIAN_POINT ( 'NONE',  ( 3.902768115887398803, 5.646591783325653147, -1.599625672291269396 ) ) ;
#84140 = CARTESIAN_POINT ( 'NONE',  ( 2.741159958678766717, -1.308340514575502045, -1.191892431489706805 ) ) ;
#84141 = MECHANICAL_DESIGN_GEOMETRIC_PRESENTATION_REPRESENTATION (  '', ( #87697 ), #60019 ) ;
#84142 = CARTESIAN_POINT ( 'NONE',  ( 6.141676493652540536, -1.594220855400224401, -1.526124331276897950 ) ) ;
#84143 = COLOUR_RGB ( '', 0.72549020, 0.75294118, 0.79215686) ;
#84144 = VERTEX_POINT ( 'NONE', #149814 ) ;
#84145 = CARTESIAN_POINT ( 'NONE',  ( -6.798487682609798632, 6.896266815991691779, 0.7998128361456341429 ) ) ;
#84146 = CARTESIAN_POINT ( 'NONE',  ( 5.466422796518627614, -1.967893101392578448, -0.4390109167287381542 ) ) ;
#84148 = VERTEX_POINT ( 'NONE', #201724 ) ;
#84147 = CARTESIAN_POINT ( 'NONE',  ( 4.957183922012514898, -1.549878356133486124, 0.9377188026478706639 ) ) ;
#84149 = CARTESIAN_POINT ( 'NONE',  ( 2.957714569337116739, 1.861795396119047208, -0.1817069356538636715 ) ) ;
#84150 = CARTESIAN_POINT ( 'NONE',  ( 2.711853232431875593, 0.5564382603544040240, -1.993978196652478996 ) ) ;
#84151 = CARTESIAN_POINT ( 'NONE',  ( -6.902509602688818191, 9.146290184594002781, -1.443375672974066548 ) ) ;
#84152 = CARTESIAN_POINT ( 'NONE',  ( 1.986440140746603911, -1.173720106059353396, 1.509789020923378189 ) ) ;
#84153 = DIRECTION ( 'NONE',  ( 0.000000000000000000, -1.000000000000000000, 0.000000000000000000 ) ) ;
#84154 = CARTESIAN_POINT ( 'NONE',  ( -9.420111044277531320, 2.999985932080179829, -6.906458289183190047 ) ) ;
#84155 = CARTESIAN_POINT ( 'NONE',  ( -3.469446951953614189E-15, 3.500000000000003109, 2.602085213965210642E-15 ) ) ;
#84156 = B_SPLINE_CURVE_WITH_KNOTS ( 'NONE', 3,
 ( #174544, #21824, #43474, #190747 ),
 .UNSPECIFIED., .F., .F.,
 ( 4, 4 ),
 ( 7.548539127806008953E-17, 0.0001647631253658502772 ),
 .UNSPECIFIED. ) ;
#84157 = CARTESIAN_POINT ( 'NONE',  ( 1.364683531249990311, 4.926041667008083991, 0.7879004041258500513 ) ) ;
#84158 = CARTESIAN_POINT ( 'NONE',  ( 0.1406777020166137260, 1.830675540527426648, 0.5531436448603862521 ) ) ;
#84159 = CARTESIAN_POINT ( 'NONE',  ( 5.560252395380206991, 7.580323442733986283, 1.443375672974065660 ) ) ;
#84160 = CARTESIAN_POINT ( 'NONE',  ( 1.890992312513404716, 0.1891058464698439912, 1.952711869325058691 ) ) ;
#84161 = CARTESIAN_POINT ( 'NONE',  ( 6.670655732516623360, 7.629137130509072051, 2.773739711112707784 ) ) ;
#84162 = CARTESIAN_POINT ( 'NONE',  ( -4.610654757099099221, 7.536791762327691657, 1.199719254218452935 ) ) ;
#84163 = CARTESIAN_POINT ( 'NONE',  ( 4.974906307097914926, -1.534222593358970821, 1.464151343314526343 ) ) ;
#84165 = SURFACE_STYLE_USAGE ( .BOTH. , #186997 ) ;
#84164 = CARTESIAN_POINT ( 'NONE',  ( 9.596473800374404561, 10.09030761005864285, 0.000000000000000000 ) ) ;
#84166 = CARTESIAN_POINT ( 'NONE',  ( 6.555938671473301227, 1.966215360770405818, -0.1428278144062731236 ) ) ;
#84167 = CARTESIAN_POINT ( 'NONE',  ( -0.6823417656250212460, 2.551041667008084435, 1.181850606188767472 ) ) ;
#84168 = CARTESIAN_POINT ( 'NONE',  ( 1.494390954318410625, -1.073482900754536784, 1.702939308294330489 ) ) ;
#84170 = CARTESIAN_POINT ( 'NONE',  ( 1.247838713208373029, 2.085211562554165621, -0.3660346322543471809 ) ) ;
#84169 = CARTESIAN_POINT ( 'NONE',  ( -7.375272376154101472, 7.706831981708990753, -0.7216878364870278340 ) ) ;
#84171 = CARTESIAN_POINT ( 'NONE',  ( 11.39809020714891830, 7.521243758227223353, 3.778010186578677931 ) ) ;
#84172 = CARTESIAN_POINT ( 'NONE',  ( 2.857943571468853250, -0.6518772230660694333, 1.965110387975615991 ) ) ;
#84173 = CARTESIAN_POINT ( 'NONE',  ( 4.797606254389322089, 6.690569611577942943, 1.599625672291268286 ) ) ;
#84174 = CARTESIAN_POINT ( 'NONE',  ( 5.747730777550676073, 5.670383760089384495, 0.000000000000000000 ) ) ;
#84175 = ORIENTED_EDGE ( 'NONE', *, *, #66221, .T. ) ;
#84177 = CARTESIAN_POINT ( 'NONE',  ( 4.059776932288224671, 6.823824623389866950, 1.199719254218462483 ) ) ;
#84176 = CARTESIAN_POINT ( 'NONE',  ( 5.349593081218750434, 2.088290806564324420, -0.1017214290881287009 ) ) ;
#84180 = ORIENTED_EDGE ( 'NONE', *, *, #40172, .F. ) ;
#84179 = CARTESIAN_POINT ( 'NONE',  ( 2.437905218827548737, -1.044187398466125627, -1.480012136316358085 ) ) ;
#84178 = CARTESIAN_POINT ( 'NONE',  ( 4.260648785556298890, -1.352668379831567069, 1.226179085325199258 ) ) ;
#84181 = CARTESIAN_POINT ( 'NONE',  ( 9.402743226277308963, 10.92862083786708816, -1.199719254218446718 ) ) ;
#84182 =( NAMED_UNIT ( * ) SI_UNIT ( $, .STERADIAN. ) SOLID_ANGLE_UNIT ( ) );
#84183 = CARTESIAN_POINT ( 'NONE',  ( 9.269816152938050280, 13.50982561720567254, -6.801071679830670291 ) ) ;
#84184 = CARTESIAN_POINT ( 'NONE',  ( 5.350674426004140116, 0.6359874849255695572, 2.113150234885258438 ) ) ;
#84185 = CARTESIAN_POINT ( 'NONE',  ( -1.364683531250010740, 9.942708333674728394, 0.7879004041258445001 ) ) ;
#84186 = ORIENTED_EDGE ( 'NONE', *, *, #2174, .T. ) ;
#84187 = CARTESIAN_POINT ( 'NONE',  ( 4.301352856729808494, 1.706663192164651122, -0.8627939227693476321 ) ) ;
#84188 = CARTESIAN_POINT ( 'NONE',  ( -2.923754682041362241, 6.562797562356882608, 0.7998128361456341429 ) ) ;
#84189 = CARTESIAN_POINT ( 'NONE',  ( 8.457588896826466751, 8.761608555919362828, 1.040834085586084257E-14 ) ) ;
#84190 = CARTESIAN_POINT ( 'NONE',  ( 0.6801582343749935644, 0.2552083336747196229, 1.178068619123780802 ) ) ;
#84191 = CARTESIAN_POINT ( 'NONE',  ( 3.673896439178918172, 6.269667698141953238, 1.082531754730558626 ) ) ;
#84192 = CARTESIAN_POINT ( 'NONE',  ( -11.86686399458719343, 12.49071270224662200, 1.056461745586970480 ) ) ;
#84193 = CARTESIAN_POINT ( 'NONE',  ( 1.419999999999990603, 6.280000000000042881, 2.873333333333337070 ) ) ;
#84194 = CARTESIAN_POINT ( 'NONE',  ( -0.1296875068448159751, 0.001480089298542403009, -1.826395826379861864 ) ) ;
#84195 = ORIENTED_EDGE ( 'NONE', *, *, #123168, .F. ) ;
#84196 = CARTESIAN_POINT ( 'NONE',  ( 3.672993792711932048, 0.04889617625786558258, -1.870083761627352237 ) ) ;
#84197 = CARTESIAN_POINT ( 'NONE',  ( 5.833751235630055376, 10.02806988486892514, 0.7998128361456331437 ) ) ;
#84198 = DIRECTION ( 'NONE',  ( 1.224643483124941457E-16, 0.002327115863041261980, 0.9999972922622142324 ) ) ;
#84199 = CIRCLE ( 'NONE', #60091, 0.07999999999999940492 ) ;
#84200 = AXIS2_PLACEMENT_3D ( 'NONE', #28574, #80518, #213682 ) ;
#84201 = CARTESIAN_POINT ( 'NONE',  ( -7.131225611108100715, 9.342849184424693476, 1.443375672974078761 ) ) ;
#84202 = CARTESIAN_POINT ( 'NONE',  ( 5.066996723205273057, 6.934582148538044777, 1.599625672291267398 ) ) ;
#84203 = CARTESIAN_POINT ( 'NONE',  ( 0.6198874644624132735, 1.948816017023939251, -0.2832832528399802374 ) ) ;
#84204 = CARTESIAN_POINT ( 'NONE',  ( 1.739861462675455828, 2.010826045486389102, -0.1511602461454417123 ) ) ;
#84205 = CIRCLE ( 'NONE', #80826, 3.017800438942085606 ) ;
#84206 = CARTESIAN_POINT ( 'NONE',  ( -9.006694118179950692, 9.402231314165087284, 1.040834085586084257E-14 ) ) ;
#84207 = CARTESIAN_POINT ( 'NONE',  ( 5.169401708560450004, 9.252995436621013425, 0.000000000000000000 ) ) ;
#84208 = FILL_AREA_STYLE_COLOUR ( '', #149765 ) ;
#84209 = CARTESIAN_POINT ( 'NONE',  ( 2.660326705311684581, -1.510451929809487170, 1.587989696798755013 ) ) ;
#84210 = CARTESIAN_POINT ( 'NONE',  ( 6.551389018236878137, -1.469694460105780864, -1.082916835497591102 ) ) ;
#84211 = CARTESIAN_POINT ( 'NONE',  ( -3.948449050077848632, 5.629609863222681199, 1.599625672291267398 ) ) ;
#84212 = EDGE_CURVE ( 'NONE', #199345, #172448, #49227, .T. ) ;
#84213 = CARTESIAN_POINT ( 'NONE',  ( 3.607878275012302627, 7.223292064240769861, 0.7216878364870257245 ) ) ;
#84214 = CARTESIAN_POINT ( 'NONE',  ( 8.097244055859613709, 10.46987070330147063, -1.599625672291262513 ) ) ;
#84215 = CARTESIAN_POINT ( 'NONE',  ( 3.571683402196252910, 6.254382171615883834, 1.199719254218462483 ) ) ;
#84216 = CARTESIAN_POINT ( 'NONE',  ( 5.058600711674583472, 8.915801573680086634, 0.000000000000000000 ) ) ;
#84217 = VERTEX_POINT ( 'NONE', #104261 ) ;
#84219 = CARTESIAN_POINT ( 'NONE',  ( 0.2760392706695756759, 1.990868297383071139, -0.2976099395228733457 ) ) ;
#84218 = CARTESIAN_POINT ( 'NONE',  ( 4.282634502089007533, 1.642705626968201216, -0.8318752211165170163 ) ) ;
#84220 = CARTESIAN_POINT ( 'NONE',  ( 3.286738001609066817, -2.216000729425780413, 0.6097190577039524051 ) ) ;
#84222 = CARTESIAN_POINT ( 'NONE',  ( 0.5845111633032008536, 1.778450750175617712, 0.5478710867917855332 ) ) ;
#84221 = CARTESIAN_POINT ( 'NONE',  ( 3.159872497350143750, 2.806782174840458666, -2.466584723216997510 ) ) ;
#84223 = CARTESIAN_POINT ( 'NONE',  ( 3.475000000000000533, -0.4958333333333350690, -2.006292185433951047 ) ) ;
#84224 = CARTESIAN_POINT ( 'NONE',  ( -3.906720819032141190, 7.709591388846142479, -0.7998128361456281477 ) ) ;
#84225 = DIRECTION ( 'NONE',  ( -1.000000000000000000, 7.771561172376097755E-16, 4.440892098500627148E-16 ) ) ;
#84226 = CARTESIAN_POINT ( 'NONE',  ( 4.974826827724895928, -1.381046924789817831, 1.323090558688621909 ) ) ;
#84227 = CARTESIAN_POINT ( 'NONE',  ( -9.104463846776669200, 10.58062822844965645, -1.199719254218441611 ) ) ;
#84228 = CARTESIAN_POINT ( 'NONE',  ( 6.170003545802125622, 6.961323287618347955, -0.9016653442153206299 ) ) ;
#84229 = CARTESIAN_POINT ( 'NONE',  ( -7.607533591043815768, 8.048079742405473525, 0.000000000000000000 ) ) ;
#84231 = CARTESIAN_POINT ( 'NONE',  ( 2.377632874612686020, 1.149002834218125102, 1.476114537088555112 ) ) ;
#84230 = CARTESIAN_POINT ( 'NONE',  ( 4.212501570603551571, 1.912301062189927015, 0.8455808105151915166 ) ) ;
#84232 = CARTESIAN_POINT ( 'NONE',  ( 6.453317930424781856, 10.47269531889685545, -0.7216878364870267237 ) ) ;
#84233 = CARTESIAN_POINT ( 'NONE',  ( 0.6823417656249917140, 5.655208333674749177, 1.181850606188765695 ) ) ;
#84234 = CARTESIAN_POINT ( 'NONE',  ( 5.671403949121008203, 1.101820082107987098, 1.475039313902235305 ) ) ;
#84235 = CARTESIAN_POINT ( 'NONE',  ( 3.009020027229115879, 5.597941567487558778, -1.199719254218446718 ) ) ;
#84237 = CARTESIAN_POINT ( 'NONE',  ( 4.222474775652216294, 7.013638773981186958, 1.199719254218462483 ) ) ;
#84236 = LINE ( 'NONE', #135147, #75524 ) ;
#84238 = CARTESIAN_POINT ( 'NONE',  ( 4.318794280271901265, 1.578467719028648686, 0.6958846415187101009 ) ) ;
#84239 = CARTESIAN_POINT ( 'NONE',  ( -8.064402442030170093, 8.302891025323665630, 0.7998128361456602331 ) ) ;
#84240 = CARTESIAN_POINT ( 'NONE',  ( 6.252570086353132162, 0.6882034672392455255, 2.096894461246688213 ) ) ;
#84241 = CARTESIAN_POINT ( 'NONE',  ( 6.983263157960386103, 3.689421308571324776, 2.567857239638075217 ) ) ;
#84242 = CARTESIAN_POINT ( 'NONE',  ( 11.07790593930098311, 11.29999999999999893, -0.7000000000000009548 ) ) ;
#84243 = CARTESIAN_POINT ( 'NONE',  ( 9.579764304849151202, -9.999999999999994671, -0.06720017513373727214 ) ) ;
#84244 = CARTESIAN_POINT ( 'NONE',  ( 5.172805277531332457, 1.502137693623846193, -1.567733665727601089 ) ) ;
#84245 = CARTESIAN_POINT ( 'NONE',  ( 2.824607995650964209, 1.719152210223941823, 0.6149139946348627372 ) ) ;
#84246 = CARTESIAN_POINT ( 'NONE',  ( 1.500000000000001332, 12.37499999999999645, 0.000000000000000000 ) ) ;
#84247 = CARTESIAN_POINT ( 'NONE',  ( 5.401600794869550803, -2.065136407520694828, 0.4665587172485561318 ) ) ;
#84248 = ORIENTED_EDGE ( 'NONE', *, *, #210974, .T. ) ;
#84250 = CARTESIAN_POINT ( 'NONE',  ( 0.6823417656249899377, 2.655208333674753618, 1.181850606188767472 ) ) ;
#84249 = CARTESIAN_POINT ( 'NONE',  ( 5.724266765471021756, 2.208406811287708660, 0.6146092054917261516 ) ) ;
#84251 = CARTESIAN_POINT ( 'NONE',  ( 8.215351014876830504, 11.67199438640995801, -1.199719254218446718 ) ) ;
#84252 = CARTESIAN_POINT ( 'NONE',  ( 1.137531110418067204, -0.04838959064331486287, 2.120096749846810624 ) ) ;
#84253 = CARTESIAN_POINT ( 'NONE',  ( -4.446711195602245148, 7.171284913969171448, -1.082531754730549967 ) ) ;
#84254 = EDGE_CURVE ( 'NONE', #195414, #205644, #183317, .T. ) ;
#84255 = CARTESIAN_POINT ( 'NONE',  ( 2.250290310188348464, 5.569163095287620990, 0.7216878364870438212 ) ) ;
#84256 = CARTESIAN_POINT ( 'NONE',  ( -4.392478580703220281, 8.068382744221649361, 1.040834085586084257E-14 ) ) ;
#84257 = CARTESIAN_POINT ( 'NONE',  ( 6.877770952621925282, -2.108145516380425910, 0.5186976372570563099 ) ) ;
#84259 = CARTESIAN_POINT ( 'NONE',  ( 1.499999999999997113, 12.67708333401612819, -0.8660254037844378194 ) ) ;
#84258 = CARTESIAN_POINT ( 'NONE',  ( 6.883263157960369583, 7.629137130509070275, 2.653810918356712900 ) ) ;
#84261 = EDGE_LOOP ( 'NONE', ( #56734, #76031, #175435, #191749, #84715, #119248, #88627, #16560, #209806, #44133, #136308, #158532, #212569, #118606, #139970, #126515, #160354, #59223, #187636 ) ) ;
#84260 = CARTESIAN_POINT ( 'NONE',  ( 1.401376347886007068, -0.3305552470432049916, -2.196467622588905932 ) ) ;
#84262 = CARTESIAN_POINT ( 'NONE',  ( 5.959611329766300258, -1.915599147091971544, -0.6298778581111733610 ) ) ;
#84264 = CARTESIAN_POINT ( 'NONE',  ( 4.082923458916259740, 1.956979318386397715, 0.6515942777399350572 ) ) ;
#84263 = CARTESIAN_POINT ( 'NONE',  ( 3.147464216666835402, 6.823792019419957278, -0.7998128361456291469 ) ) ;
#84266 = CARTESIAN_POINT ( 'NONE',  ( -1.737500000000000266, -3.208333333333333925, -3.009438278150923907 ) ) ;
#84265 = CARTESIAN_POINT ( 'NONE',  ( 7.666209513884374438, 7.908608952478760834, 0.7998128361456281477 ) ) ;
#84267 = CARTESIAN_POINT ( 'NONE',  ( 7.361151057576892143, 7.552707420120024828, 0.7998128361456291469 ) ) ;
#84268 = CARTESIAN_POINT ( 'NONE',  ( 3.285556943750000070, -2.821874999522043570, 0.000000000000000000 ) ) ;
#84269 = CARTESIAN_POINT ( 'NONE',  ( 0.4278232814946582585, 1.072867435734598196, -1.794206126505201837 ) ) ;
#84270 = CARTESIAN_POINT ( 'NONE',  ( 4.131482539099665452, 0.5404898895830790861, 1.942541833525657680 ) ) ;
#84271 = CARTESIAN_POINT ( 'NONE',  ( 4.862772069579198941, 0.1752732939881325724, -1.832877676746891726 ) ) ;
#84272 = CARTESIAN_POINT ( 'NONE',  ( 5.138703914779377158, 5.953908307786102583, 1.199719254218462483 ) ) ;
#84273 = CARTESIAN_POINT ( 'NONE',  ( 1.113767329461469835, -0.7700024601069790364, -1.543427451845545084 ) ) ;
#84274 = CARTESIAN_POINT ( 'NONE',  ( -0.04763828917917976857, -1.313539345393003321, 1.530161206715647149 ) ) ;
#84275 = CARTESIAN_POINT ( 'NONE',  ( 1.055823836731560439, -1.452736638576918038, 1.781478128903237756 ) ) ;
#84276 = CARTESIAN_POINT ( 'NONE',  ( -6.586563698140583512, 6.578745824119123675, 1.040834085586084257E-14 ) ) ;
#84277 = CARTESIAN_POINT ( 'NONE',  ( 0.9137757228094539608, -0.3311857980235459742, 2.237941903941061739 ) ) ;
#84278 = CARTESIAN_POINT ( 'NONE',  ( 2.490967578435684615, -0.3607690000238995554, -2.074772605841824991 ) ) ;
#84279 = CARTESIAN_POINT ( 'NONE',  ( -6.134138155540168391, 6.121192367743780949, 0.000000000000000000 ) ) ;
#84280 = CARTESIAN_POINT ( 'NONE',  ( 6.962275575817444384, 8.081408578997208991, -1.199719254218446718 ) ) ;
#84281 = CARTESIAN_POINT ( 'NONE',  ( 5.519577934094852978, 7.532869904567736974, 1.443375672974064550 ) ) ;
#84282 = CARTESIAN_POINT ( 'NONE',  ( 5.562500000000004441, -1.451031289061337937, -1.451031289060889851 ) ) ;
#84283 = CARTESIAN_POINT ( 'NONE',  ( -5.225778143063529946, 8.184159369294361497, 1.199719254218452047 ) ) ;
#84284 = UNCERTAINTY_MEASURE_WITH_UNIT (LENGTH_MEASURE( 1.000000000000000082E-05 ), #8436, 'distance_accuracy_value', 'NONE');
#84285 = CARTESIAN_POINT ( 'NONE',  ( -0.7500000000000215383, 2.691666666666689522, 1.299038105676671107 ) ) ;
#84286 = CARTESIAN_POINT ( 'NONE',  ( -4.810445574750349174, 4.506608013497163334, 0.7998128361456341429 ) ) ;
#84287 = CARTESIAN_POINT ( 'NONE',  ( 4.623389083599304783, 1.933371432498669273, 1.093773624979002879 ) ) ;
#84288 = CARTESIAN_POINT ( 'NONE',  ( 3.767680093253112705, 1.217039798425190167, 1.822233383357040104 ) ) ;
#84289 = CARTESIAN_POINT ( 'NONE',  ( -6.033542053281340856, 6.997886136038390603, -1.199719254218446718 ) ) ;
#84290 = CARTESIAN_POINT ( 'NONE',  ( -2.959422669532919326, 6.674686557755516780, 0.7998128361456352531 ) ) ;
#84291 = AXIS2_PLACEMENT_3D ( 'NONE', #4508, #70579, #42411 ) ;
#84292 = CARTESIAN_POINT ( 'NONE',  ( -1.201851678989727383E-14, 3.196875000341420137, -1.575800808251660134 ) ) ;
#84293 = CARTESIAN_POINT ( 'NONE',  ( 6.890000000000037872, 2.400824642991986391, 2.659875214078717853 ) ) ;
#84294 = CARTESIAN_POINT ( 'NONE',  ( -4.772106882330234612, 6.590544000850479200, -1.443375672974053447 ) ) ;
#84295 = CARTESIAN_POINT ( 'NONE',  ( 6.205353461901607304, 1.844339991697005798, -1.046509186232460697 ) ) ;
#84296 = CARTESIAN_POINT ( 'NONE',  ( -6.997416678428844072, 8.296645891989347987, 1.082531754730549078 ) ) ;
#84297 = VERTEX_POINT ( 'NONE', #70654 ) ;
#84300 =( GEOMETRIC_REPRESENTATION_CONTEXT ( 3 ) GLOBAL_UNCERTAINTY_ASSIGNED_CONTEXT ( ( #155432 ) ) GLOBAL_UNIT_ASSIGNED_CONTEXT ( ( #174971, #160837, #107887 ) ) REPRESENTATION_CONTEXT ( 'NONE', 'WORKASPACE' ) );
#84299 = CARTESIAN_POINT ( 'NONE',  ( 6.157120911006636277, -1.851533521339579380, -1.115484332758958974 ) ) ;
#84298 = CARTESIAN_POINT ( 'NONE',  ( -4.936577329151611515, 7.813071746435248599, 1.082531754730549967 ) ) ;
#84301 = CARTESIAN_POINT ( 'NONE',  ( 6.030679399980265920, 5.930214142932100252, -0.7998128361456281477 ) ) ;
#84302 = CARTESIAN_POINT ( 'NONE',  ( 6.110883706712432861, -0.2185277653131960651, 1.828168259763853998 ) ) ;
#84303 = CARTESIAN_POINT ( 'NONE',  ( 0.3282377607281126153, 0.8861645503674525637, 1.224999999999959455 ) ) ;
#84304 = CARTESIAN_POINT ( 'NONE',  ( 1.364683531249988757, 2.196875000341415252, 1.214306433183764966E-14 ) ) ;
#84305 = CARTESIAN_POINT ( 'NONE',  ( 0.8369945909703061515, 0.7069334548283608965, -1.590575932886540755 ) ) ;
#84306 = CARTESIAN_POINT ( 'NONE',  ( -9.498884310698272770, -9.900000000000076739, 0.1658036423890281996 ) ) ;
#84307 = CARTESIAN_POINT ( 'NONE',  ( -0.07074886611256257785, 8.280404612018088528, 2.000278354478734144 ) ) ;
#84308 = CARTESIAN_POINT ( 'NONE',  ( 5.630352418794719149, 6.139657267270441920, -0.8181431533968346326 ) ) ;
#84309 = CARTESIAN_POINT ( 'NONE',  ( 5.348557406608104969, 0.6236849695623291057, 2.069784783864880851 ) ) ;
#84310 = CARTESIAN_POINT ( 'NONE',  ( -3.785751206713858785, 5.439795712631356750, 1.599625672291267398 ) ) ;
#84311 = VECTOR ( 'NONE', #15849, 1000.000000000000000 ) ;
#84312 = CARTESIAN_POINT ( 'NONE',  ( -6.792271770322117597, 9.907772251142352715, 1.082531754730549967 ) ) ;
#84313 = CARTESIAN_POINT ( 'NONE',  ( 4.381803836707322652, 1.409801062080328959, 1.638821348427916602 ) ) ;
#84314 = CARTESIAN_POINT ( 'NONE',  ( -1.201851678989727383E-14, 3.696875000341422801, -1.575800808251660134 ) ) ;
#84315 = CARTESIAN_POINT ( 'NONE',  ( 6.397732417105159719, -0.6663202349154914161, 1.855440513692607540 ) ) ;
#84316 = CARTESIAN_POINT ( 'NONE',  ( 4.639819690880945480, -0.0003889188416681537710, -1.734034292319245552 ) ) ;
#84318 = CARTESIAN_POINT ( 'NONE',  ( 1.681448347407452193, 1.514353137444489406, 1.584415833815432162 ) ) ;
#84317 = CARTESIAN_POINT ( 'NONE',  ( -10.51588623913388254, 11.11317498266430803, -3.554197739806004286 ) ) ;
#84319 = CARTESIAN_POINT ( 'NONE',  ( 1.852963337694241819, 0.7249817717532834882, 2.190821962643316301 ) ) ;
#84320 = CARTESIAN_POINT ( 'NONE',  ( 4.657529158609388986, 0.4554517582456064084, -2.009643979410648651 ) ) ;
#84321 = CARTESIAN_POINT ( 'NONE',  ( 0.04082682177056726897, -1.500436592000290670, -1.232479804542076618 ) ) ;
#84322 = CARTESIAN_POINT ( 'NONE',  ( -7.063434842595444962, 8.303390740191881392, 1.082531754730549967 ) ) ;
#84323 = CARTESIAN_POINT ( 'NONE',  ( -4.655245641445871385, 6.524482229810530498, 1.599625672291263179 ) ) ;
#84324 = CARTESIAN_POINT ( 'NONE',  ( -0.4683205530892509683, -8.233137084989849086, -9.568546172724143872 ) ) ;
#84325 = EDGE_CURVE ( 'NONE', #182472, #208480, #149001, .T. ) ;
#84326 = FILL_AREA_STYLE_COLOUR ( '', #98487 ) ;
#84327 = CARTESIAN_POINT ( 'NONE',  ( 1.160779977835691312, 1.203355533934968635, 1.617816888933524710 ) ) ;
#84328 = CARTESIAN_POINT ( 'NONE',  ( -7.171900071504754060, 7.469564292951421436, -0.7216878364870267237 ) ) ;
#84329 = CARTESIAN_POINT ( 'NONE',  ( 4.173040645679537697, -2.057929556117383374, -0.7971749352265260491 ) ) ;
#84330 = CARTESIAN_POINT ( 'NONE',  ( 3.285556943749998737, -2.442708332855375364, -1.896917185911906500 ) ) ;
#84331 = CARTESIAN_POINT ( 'NONE',  ( 1.938117168453708627, -1.000761817645494212, 1.568762535561243121 ) ) ;
#84332 = CARTESIAN_POINT ( 'NONE',  ( 1.407792700327077151, 3.466403870727115422, 0.5229849042009182547 ) ) ;
#84333 = CARTESIAN_POINT ( 'NONE',  ( 2.836961834123311821, 6.429236568308559718, -0.07888921887194833005 ) ) ;
#84334 = CARTESIAN_POINT ( 'NONE',  ( -11.97929049433705373, 9.719999999999998863, -0.7046979865771834106 ) ) ;
#84336 = CARTESIAN_POINT ( 'NONE',  ( 6.925078400183526384, 2.431821113958906544, 2.425929786733098226 ) ) ;
#84335 = CARTESIAN_POINT ( 'NONE',  ( -4.992018142146231519, 8.041046192835899831, -1.132135330316372590 ) ) ;
#84337 = FACE_OUTER_BOUND ( 'NONE', #55926, .T. ) ;
#84338 = ORIENTED_EDGE ( 'NONE', *, *, #158865, .T. ) ;
#84339 = CARTESIAN_POINT ( 'NONE',  ( 3.204032760728621643, -2.058606879712703286, 0.09948017704831073338 ) ) ;
#84340 = CARTESIAN_POINT ( 'NONE',  ( 0.6801582343749831283, 1.223958333674737720, 1.178068619123822547 ) ) ;
#84341 = CARTESIAN_POINT ( 'NONE',  ( -5.530836599371015794, 8.540060901653093950, 1.199719254218452047 ) ) ;
#84342 = CARTESIAN_POINT ( 'NONE',  ( 2.297526485177129540, 1.845687725436034432, -0.8205148536439119678 ) ) ;
#84343 = CARTESIAN_POINT ( 'NONE',  ( 0.7499999999999867883, -0.1833333333333131421, -1.299038105676652899 ) ) ;
#84344 = CARTESIAN_POINT ( 'NONE',  ( 3.521367211247359741, 5.131347717920458962, -1.599625672291262513 ) ) ;
#84345 = CARTESIAN_POINT ( 'NONE',  ( 1.446242185974885963, 2.058501543756698915, 0.1019544441857832273 ) ) ;
#84346 = EDGE_CURVE ( 'NONE', #160528, #70696, #189005, .T. ) ;
#84348 = CARTESIAN_POINT ( 'NONE',  ( 0.6823417656249969321, 12.77604166700806232, -1.181850606188757036 ) ) ;
#84347 = CARTESIAN_POINT ( 'NONE',  ( -0.08053691275167716712, 19.00000000000000000, 11.99972973886014316 ) ) ;
#84349 = CARTESIAN_POINT ( 'NONE',  ( 5.133733721068893807, 9.141106441222381918, 1.040834085586084257E-14 ) ) ;
#84350 = CARTESIAN_POINT ( 'NONE',  ( -0.2408018239684408812, 2.868499929943384874, -2.588695376639174484 ) ) ;
#84351 = CARTESIAN_POINT ( 'NONE',  ( 0.6734667703603390843, -1.024904740748554532, 1.529287851792550335 ) ) ;
#84352 = CARTESIAN_POINT ( 'NONE',  ( 5.268293329372571776, 1.085216321637239023, 1.921556908365213312 ) ) ;
#84353 = CARTESIAN_POINT ( 'NONE',  ( 5.176180785367283654, 9.260904359562321275, -0.7998128361456481317 ) ) ;
#84354 = CARTESIAN_POINT ( 'NONE',  ( 1.669428131952359839, 0.1607934374257547205, -2.155692497560882437 ) ) ;
#84355 = CARTESIAN_POINT ( 'NONE',  ( -4.229780737783618072, 6.918199379847403740, 1.082531754730560403 ) ) ;
#84356 = CARTESIAN_POINT ( 'NONE',  ( 1.991423064788412800, -0.4370762659771566527, 1.968445590580846893 ) ) ;
#84357 = CARTESIAN_POINT ( 'NONE',  ( -5.204170427930421283E-15, -7.126685749120009739, -9.926723642588084928 ) ) ;
#84358 = CARTESIAN_POINT ( 'NONE',  ( -0.5341619149264997812, 6.871487518424857832, 3.795316691233094009 ) ) ;
#84359 = AXIS2_PLACEMENT_3D ( 'NONE', #30226, #96310, #76825 ) ;
#84360 = CARTESIAN_POINT ( 'NONE',  ( 4.135589226209329006, -1.358636868218986216, -1.428786634662780219 ) ) ;
#84361 = CARTESIAN_POINT ( 'NONE',  ( 3.749232653202066778, 0.2420323627391370025, -2.001857840249580800 ) ) ;
#84363 = CARTESIAN_POINT ( 'NONE',  ( 8.392133896734652154, 12.73464727959172293, 0.7216878364870438212 ) ) ;
#84362 = CARTESIAN_POINT ( 'NONE',  ( 0.6823417656249882723, 1.676041667008083769, -1.181850606188749264 ) ) ;
#84365 = CARTESIAN_POINT ( 'NONE',  ( 5.110040610736272804, -2.096041292509024156, 0.2052846074404850174 ) ) ;
#84364 = CARTESIAN_POINT ( 'NONE',  ( -8.040148788103921973, 9.338927326664741457, 1.199719254218462483 ) ) ;
#84366 =( BOUNDED_CURVE ( )  B_SPLINE_CURVE ( 1, ( #21348, #818 ),
 .UNSPECIFIED., .F., .T. ) 
 B_SPLINE_CURVE_WITH_KNOTS ( ( 2, 2 ),
 ( 0.000000000000000000, 6.249999999999788711E-05 ),
 .UNSPECIFIED. ) 
 CURVE ( )  GEOMETRIC_REPRESENTATION_ITEM ( )  RATIONAL_B_SPLINE_CURVE ( ( 0.9345202395942815432, 0.9345202395942815432 ) ) 
 REPRESENTATION_ITEM ( '' )  );
#84367 = AXIS2_PLACEMENT_3D ( 'NONE', #38590, #104667, #77479 ) ;
#84368 = EDGE_CURVE ( 'NONE', #180652, #142732, #3776, .T. ) ;
#84369 = CARTESIAN_POINT ( 'NONE',  ( 5.529760519541640384, 1.996289034380031913, -0.5486624943154896350 ) ) ;
#84370 = CARTESIAN_POINT ( 'NONE',  ( 6.012151052656117933, 9.101594430485762999, 1.199719254218460707 ) ) ;
#84371 = CARTESIAN_POINT ( 'NONE',  ( -7.552055258011950656, 8.769484874890757453, 1.199719254218462483 ) ) ;
#84372 = CARTESIAN_POINT ( 'NONE',  ( -1.446373960595505270, 8.704174803020482187, 2.603708784378574226 ) ) ;
#84373 = CARTESIAN_POINT ( 'NONE',  ( 5.590105174118587428, 1.206514928144377441, 1.619649990711173215 ) ) ;
#84374 = CARTESIAN_POINT ( 'NONE',  ( 1.499999999999987566, -0.4437499993171847845, 0.000000000000000000 ) ) ;
#84375 = ADVANCED_FACE ( 'NONE', ( #72806 ), #74956, .F. ) ;
#84376 = CARTESIAN_POINT ( 'NONE',  ( 1.077094301713815039, 1.904230998939509867, 0.7929820198450258095 ) ) ;
#84377 = CARTESIAN_POINT ( 'NONE',  ( 9.436111725431318931, 10.11114455586577776, -0.7216878364870257245 ) ) ;
#84378 = CARTESIAN_POINT ( 'NONE',  ( 6.505933609711257226, 8.683618192786854095, -1.599625672291281386 ) ) ;
#84379 = CARTESIAN_POINT ( 'NONE',  ( 6.222266154028957885, 6.224008365980749247, 0.7998128361456352531 ) ) ;
#84380 = CARTESIAN_POINT ( 'NONE',  ( -1.402160292154681736E-14, 0.5093750003414236893, -1.575800808251659024 ) ) ;
#84382 = CARTESIAN_POINT ( 'NONE',  ( -7.792125355486790639, -6.646943093533965730, 7.591565991045880146 ) ) ;
#84381 = CARTESIAN_POINT ( 'NONE',  ( 5.554000203453580475, 6.508696987897830688, -1.199719254218452047 ) ) ;
#84383 = CARTESIAN_POINT ( 'NONE',  ( 6.277061933002774374, 9.306694107603160404, 1.082531754730558626 ) ) ;
#84385 = CARTESIAN_POINT ( 'NONE',  ( -6.966220764712169000, 6.002124920821316323, -2.500000000000000444 ) ) ;
#84384 = CARTESIAN_POINT ( 'NONE',  ( 3.068971866484587530, 1.574395709666128296, -1.495330859492151943 ) ) ;
#84387 = CARTESIAN_POINT ( 'NONE',  ( 2.524749765808989466, -1.717266272480859834, 0.6646640004178904215 ) ) ;
#84386 = CARTESIAN_POINT ( 'NONE',  ( -5.422898255786209099, 5.429062174613087599, -0.7216878364870207285 ) ) ;
#84388 = CARTESIAN_POINT ( 'NONE',  ( -1.364683531250010295, 3.780208333674750953, 0.7879004041258379498 ) ) ;
#84389 = CARTESIAN_POINT ( 'NONE',  ( 4.230150181147958044, 2.149441460308566754, 0.4267382380854707336 ) ) ;
#84390 = CARTESIAN_POINT ( 'NONE',  ( 8.786015989428143769, 13.41256886957122951, 8.173703117781000671 ) ) ;
#84391 = CARTESIAN_POINT ( 'NONE',  ( 4.997079013686112958, 1.883918014071528146, -1.252661935414706162 ) ) ;
#84392 = CARTESIAN_POINT ( 'NONE',  ( -4.283486466913726254, 7.084819080452935403, -1.199719254218452047 ) ) ;
#84393 = CARTESIAN_POINT ( 'NONE',  ( -4.922147708203060468, 6.858988491581952118, -1.449652397630277756 ) ) ;
#84394 = CARTESIAN_POINT ( 'NONE',  ( 4.634937608369048334, 8.440560775401745985, -0.4060563726728562139 ) ) ;
#84395 = CARTESIAN_POINT ( 'NONE',  ( -5.275531169048901958, 8.208517892982092334, -1.082531754730549967 ) ) ;
#84396 = CARTESIAN_POINT ( 'NONE',  ( 4.177320726786311056, 5.966903162707725805, -1.443375672974068769 ) ) ;
#84397 = CARTESIAN_POINT ( 'NONE',  ( 0.09216213259799833912, -0.3764253007602496592, -1.735191564994809976 ) ) ;
#84398 = CARTESIAN_POINT ( 'NONE',  ( 4.389318492827157137, -0.002256833108382152835, -2.013265972533995640 ) ) ;
#84399 = CARTESIAN_POINT ( 'NONE',  ( 7.969495366734495434, 8.192166104145387706, 1.040834085586084257E-14 ) ) ;
#84400 = CARTESIAN_POINT ( 'NONE',  ( 3.329229500047115042, 0.04992189587533709533, 2.105534426424925165 ) ) ;
#84401 = CARTESIAN_POINT ( 'NONE',  ( 1.247507242870619981, 1.886983585358002813, -0.3289482045247971165 ) ) ;
#84403 = CARTESIAN_POINT ( 'NONE',  ( -0.7500000000000006661, 2.358333333333358262, -1.299038105676652011 ) ) ;
#84402 = CARTESIAN_POINT ( 'NONE',  ( 1.364683531249997417, 12.48437500034139980, 2.602085213965210642E-15 ) ) ;
#84404 = CARTESIAN_POINT ( 'NONE',  ( 1.961320326556061922, 1.635743983707088622, 1.096704005335534138 ) ) ;
#84405 = CARTESIAN_POINT ( 'NONE',  ( 0.7427767429722329506, -1.606530860214189893, 0.9580933318182258684 ) ) ;
#84406 = CARTESIAN_POINT ( 'NONE',  ( 0.5374593765826127800, 1.831924746014142791, -0.7026076897959919743 ) ) ;
#84408 = ORIENTED_EDGE ( 'NONE', *, *, #192933, .F. ) ;
#84407 = CARTESIAN_POINT ( 'NONE',  ( 6.433875545303581411, -1.754733077360526972, 0.4498553729834730008 ) ) ;
#84409 = CARTESIAN_POINT ( 'NONE',  ( 5.178851490740193242, 8.025448591630130579, 1.082531754730558626 ) ) ;
#84410 = CARTESIAN_POINT ( 'NONE',  ( 0.6823417656249882723, 0.4885416670080827695, -1.181850606188749264 ) ) ;
#84411 = CARTESIAN_POINT ( 'NONE',  ( 6.016445890116215445, 1.255022122864515310, -1.387330985440645037 ) ) ;
#84412 = DIRECTION ( 'NONE',  ( 0.9055141421511233579, 0.4243160830846685050, 2.454401000341482920E-15 ) ) ;
#84413 = CARTESIAN_POINT ( 'NONE',  ( 5.506714918851105089, 0.5956099481174789156, 1.982760374633622424 ) ) ;
#84414 = DIRECTION ( 'NONE',  ( -0.8660254037844362651, 0.000000000000000000, 0.5000000000000041078 ) ) ;
#84415 = CARTESIAN_POINT ( 'NONE',  ( -4.977251789548269301, 4.979417640660637190, 0.7216878364870257245 ) ) ;
#84417 = CARTESIAN_POINT ( 'NONE',  ( 0.1685321339487330372, -0.8835925182541467526, -1.870455940253319183 ) ) ;
#84416 = AXIS2_PLACEMENT_3D ( 'NONE', #117736, #166413, #116657 ) ;
#84418 = CARTESIAN_POINT ( 'NONE',  ( 0.7499999999999885647, 0.4833333333333564297, 1.299038105676657340 ) ) ;
#84419 = CARTESIAN_POINT ( 'NONE',  ( 6.154511665599609493, 9.267681812253174556, 1.199719254218462483 ) ) ;
#84420 = CARTESIAN_POINT ( 'NONE',  ( -6.516665389662827934, 10.75452672124865217, 0.000000000000000000 ) ) ;
#84421 = CARTESIAN_POINT ( 'NONE',  ( 5.773793314573267388, 7.829454515125894964, 1.599625672291268286 ) ) ;
#84422 = CARTESIAN_POINT ( 'NONE',  ( 1.364683531249988757, 0.6343750003414208027, 0.000000000000000000 ) ) ;
#84423 = CARTESIAN_POINT ( 'NONE',  ( 0.7499999999999885647, 2.316666666666689078, -1.299038105676652899 ) ) ;
#84425 = CARTESIAN_POINT ( 'NONE',  ( 3.876741858503734761, 6.610283703974623393, 1.199719254218462483 ) ) ;
#84424 = CARTESIAN_POINT ( 'NONE',  ( 5.371523934717264304, -0.2895824386080196322, 1.940264742196501802 ) ) ;
#84426 = CARTESIAN_POINT ( 'NONE',  ( 3.444685325028495004, 1.276847194542466646, 1.560261755768836744 ) ) ;
#84427 = CARTESIAN_POINT ( 'NONE',  ( 2.518635572904056374, 0.2389622604833125386, 1.900711705027556153 ) ) ;
#84428 = DIRECTION ( 'NONE',  ( -1.000000000000000000, 0.000000000000000000, 0.000000000000000000 ) ) ;
#84429 = CARTESIAN_POINT ( 'NONE',  ( 0.5916818631664169104, -0.7834642122952638621, 2.046923429677327100 ) ) ;
#84430 = CARTESIAN_POINT ( 'NONE',  ( 0.2333690889706717397, 6.947499272388762748, -2.648434294982876303 ) ) ;
#84431 = CARTESIAN_POINT ( 'NONE',  ( 2.917106759524803472, -0.1871779394605546654, 1.861177454839262113 ) ) ;
#84432 = CARTESIAN_POINT ( 'NONE',  ( -0.7500000000000006661, -0.6104166659838470288, -1.299038105676652011 ) ) ;
#84433 = CARTESIAN_POINT ( 'NONE',  ( -8.179646747746328828, 8.437342715325849341, -0.7998128361456291469 ) ) ;
#84435 = CARTESIAN_POINT ( 'NONE',  ( 4.675474996081856460, 1.569897879423647336, 1.420792320860002178 ) ) ;
#84434 = CARTESIAN_POINT ( 'NONE',  ( -2.982430605326321427, 6.423326772948587227, -0.7216878364870267237 ) ) ;
#84436 = CARTESIAN_POINT ( 'NONE',  ( 5.594708818112484217, 5.774250729507365953, 0.6894988139244705438 ) ) ;
#84437 = CARTESIAN_POINT ( 'NONE',  ( 5.687960312649480876, -1.310561514506687564, -1.602779375087557412 ) ) ;
#84439 = CARTESIAN_POINT ( 'NONE',  ( -4.558393992215756363, 7.582615019230624753, -1.001024991534285702 ) ) ;
#84438 = CARTESIAN_POINT ( 'NONE',  ( 2.243796185194739223, 2.090353954619321275, 0.04827919579214814960 ) ) ;
#84441 = VERTEX_POINT ( 'NONE', #139985 ) ;
#84440 = CARTESIAN_POINT ( 'NONE',  ( 1.008351294761783423, 1.310062561100222123, -1.121974927168223335 ) ) ;
#84442 = CARTESIAN_POINT ( 'NONE',  ( 7.949158136313996259, 8.168439335321471262, 1.040834085586084257E-14 ) ) ;
#84443 = CARTESIAN_POINT ( 'NONE',  ( 9.397848989302721279, 13.71838071990982577, 7.462089927986413684 ) ) ;
#84444 = CARTESIAN_POINT ( 'NONE',  ( -11.01135777277262129, 13.39999999999998259, 1.399999999999998579 ) ) ;
#84445 = CARTESIAN_POINT ( 'NONE',  ( -10.36733242867369142, 5.031604590660524678, 7.295138277318285347 ) ) ;
#84446 = CARTESIAN_POINT ( 'NONE',  ( 5.951666246274792016, 8.927065806420504401, 1.082531754730558626 ) ) ;
#84447 = CYLINDRICAL_SURFACE ( 'NONE', #103112, 0.08000000000000020983 ) ;
#84449 = CARTESIAN_POINT ( 'NONE',  ( 1.013979471798792886, -1.811656969585205612, -0.0007847632289004204901 ) ) ;
#84448 = CARTESIAN_POINT ( 'NONE',  ( 6.210516883511641772, 9.403297576475722508, 1.199719254218452047 ) ) ;
#84450 = CARTESIAN_POINT ( 'NONE',  ( -8.843996274815957293, 9.212417163573759282, 1.040834085586084257E-14 ) ) ;
#84451 = CARTESIAN_POINT ( 'NONE',  ( 5.542585869888291938, 5.360771691158120689, -0.7998128361456211532 ) ) ;
#84452 = CARTESIAN_POINT ( 'NONE',  ( -5.157723666773176063, 7.780300641499326098, 1.171761296108381201 ) ) ;
#84453 = CARTESIAN_POINT ( 'NONE',  ( 5.528692779322568640, 9.672168352510192690, 0.7998128361456341429 ) ) ;
#84454 = DIRECTION ( 'NONE',  ( 0.000000000000000000, 0.000000000000000000, 1.000000000000000000 ) ) ;
#84455 = CARTESIAN_POINT ( 'NONE',  ( 2.679285714285720044, 0.4970443252110459120, 0.000000000000000000 ) ) ;
#84456 = CARTESIAN_POINT ( 'NONE',  ( 9.747949258545622442, 10.47495501116581984, 0.000000000000000000 ) ) ;
#84457 = EDGE_LOOP ( 'NONE', ( #81837, #17550, #161688, #47173 ) ) ;
#84458 = CARTESIAN_POINT ( 'NONE',  ( 0.6322731411384452382, 0.5572298914768618605, 1.832739050869176101 ) ) ;
#84459 = CARTESIAN_POINT ( 'NONE',  ( 0.2059360158346480729, 1.574223368660916611, 1.420867075595611650 ) ) ;
#84460 = CARTESIAN_POINT ( 'NONE',  ( -1.899821779672251632, 8.994870868756308369, 0.7750000000000013545 ) ) ;
#84461 = CARTESIAN_POINT ( 'NONE',  ( 2.273584122437516175, 5.675375552130928369, 0.4747937928818931064 ) ) ;
#84462 = CARTESIAN_POINT ( 'NONE',  ( -1.547033095191295171, 8.694673270357780481, -2.507079848779465436 ) ) ;
#84463 = CARTESIAN_POINT ( 'NONE',  ( -4.284013352238265959, 5.060732334775157604, -1.082531754730544860 ) ) ;
#84464 = CARTESIAN_POINT ( 'NONE',  ( 8.378575743565351175, 11.75846021992619406, -1.082531754730543083 ) ) ;
#84465 = CARTESIAN_POINT ( 'NONE',  ( 4.065260974683176265, 1.686948271169801616, 1.016115061114295504 ) ) ;
#84466 = CARTESIAN_POINT ( 'NONE',  ( 1.014494059972574691, -2.120667955011676487, 0.003750198165439199392 ) ) ;
#84467 = CARTESIAN_POINT ( 'NONE',  ( -4.543954038874438162, 8.453030145328826350, 1.040834085586084257E-14 ) ) ;
#84468 = CARTESIAN_POINT ( 'NONE',  ( -11.04724700974751350, 7.053076968211740017, -4.573939983942181264 ) ) ;
#84469 = SPHERICAL_SURFACE ( 'NONE', #204925, 1.250000000000000000 ) ;
#84470 = CARTESIAN_POINT ( 'NONE',  ( 6.158177532299373702, -1.552315630085840947, 1.547116483708823598 ) ) ;
#84471 = DIRECTION ( 'NONE',  ( 0.000000000000000000, 0.000000000000000000, 1.000000000000000000 ) ) ;
#84472 = CARTESIAN_POINT ( 'NONE',  ( 4.577124784165859772, 0.0005310917307651402686, -1.926566264685470875 ) ) ;
#84473 = CARTESIAN_POINT ( 'NONE',  ( -6.672584156219988571, 10.93643194889866521, -0.7998128361456291469 ) ) ;
#84474 = CARTESIAN_POINT ( 'NONE',  ( -0.1411974294641839822, -0.0004739540254219998553, -1.900147702309517239 ) ) ;
#84475 = CARTESIAN_POINT ( 'NONE',  ( 0.7509353727821498348, 0.6442623716619542140, 2.110749664216593047 ) ) ;
#84476 = EDGE_CURVE ( 'NONE', #56229, #138513, #95291, .T. ) ;
#84477 = CARTESIAN_POINT ( 'NONE',  ( -0.1108833634137010304, 7.629137130509073828, -2.496956624467902675 ) ) ;
#84478 = ORIENTED_EDGE ( 'NONE', *, *, #116366, .F. ) ;
#84479 = DIRECTION ( 'NONE',  ( 0.7592566023653004592, -0.6507913734559641616, -1.725633230170963105E-31 ) ) ;
#84480 = CARTESIAN_POINT ( 'NONE',  ( 6.121921657745279077, 1.940899573806122325, -0.3330216297181831653 ) ) ;
#84481 = CARTESIAN_POINT ( 'NONE',  ( 0.2923913620977801053, 1.614019350141202569, -1.079779171115168523 ) ) ;
#84482 = CARTESIAN_POINT ( 'NONE',  ( 6.520923251934013898, 2.292922446452568597, -0.1593734864932250250 ) ) ;
#84484 = CARTESIAN_POINT ( 'NONE',  ( 4.504654980070036174, 0.4933668235826896287, 1.794306199697106363 ) ) ;
#84483 = CARTESIAN_POINT ( 'NONE',  ( -6.607619761813764647, 8.802252036906432764, 1.599625672291269396 ) ) ;
#84485 = CARTESIAN_POINT ( 'NONE',  ( 6.658989722967328717, 7.797851427330578566, 1.199719254218452935 ) ) ;
#84486 = CARTESIAN_POINT ( 'NONE',  ( -1.734723475976807094E-15, 2.999999999999988898, -6.938893903907228378E-15 ) ) ;
#84487 = CARTESIAN_POINT ( 'NONE',  ( -6.389970470742427189, 6.349387058821269747, -0.7998128361456291469 ) ) ;
#84488 = CARTESIAN_POINT ( 'NONE',  ( -3.330162143076817571, -0.9219660286950489558, 0.1033982544314127755 ) ) ;
#84489 = CARTESIAN_POINT ( 'NONE',  ( 0.1698123575781598782, 1.266975945507025081, 1.788028528876134393 ) ) ;
#84490 = CARTESIAN_POINT ( 'NONE',  ( 4.026408433578586354, 7.641300905909586660, 1.040834085586084257E-14 ) ) ;
#84491 = ORIENTED_EDGE ( 'NONE', *, *, #46115, .F. ) ;
#84492 = EDGE_CURVE ( 'NONE', #89282, #120769, #20439, .T. ) ;
#84493 = CARTESIAN_POINT ( 'NONE',  ( 10.87166355890667191, -6.717152734873750752, -0.1969747848976913240 ) ) ;
#84494 = CARTESIAN_POINT ( 'NONE',  ( -1.138412281109779656E-15, -6.948429295162514840, -9.261794192843264995 ) ) ;
#84495 = CARTESIAN_POINT ( 'NONE',  ( 0.5041868517345666767, -0.6120625888205477594, -1.720162557568189809 ) ) ;
#84496 = CARTESIAN_POINT ( 'NONE',  ( -3.653032323878261600, 6.349289246911547835, -1.199719254218452047 ) ) ;
#84497 = CARTESIAN_POINT ( 'NONE',  ( 3.551122959743778562, -1.161752147869070884, 1.287673551650715842 ) ) ;
#84498 = CARTESIAN_POINT ( 'NONE',  ( 1.782949938078045582, -1.600000000000000755, -2.093702347113241213 ) ) ;
#84499 = CARTESIAN_POINT ( 'NONE',  ( -0.3282377607281437570, 2.801335450315371567, 1.224999999999956790 ) ) ;
#84500 = CARTESIAN_POINT ( 'NONE',  ( 6.856061878569608298E-15, 0.1875000000000181521, -1.225000000000034950 ) ) ;
#84501 = CARTESIAN_POINT ( 'NONE',  ( 0.3637320452541660254, 1.905723972499345997, -0.2814332051396683521 ) ) ;
#84502 = CARTESIAN_POINT ( 'NONE',  ( 4.047668389856577065, 1.417901948909123799, 1.355967163993692992 ) ) ;
#84503 = ADVANCED_FACE ( 'NONE', ( #61906 ), #212393, .F. ) ;
#84504 = CARTESIAN_POINT ( 'NONE',  ( -8.533967624797991647, 12.04371376465130439, -1.199719254218446718 ) ) ;
#84505 = CARTESIAN_POINT ( 'NONE',  ( 6.972971076130050072, 7.029554431773520129, 1.040834085586084257E-14 ) ) ;
#84506 = CARTESIAN_POINT ( 'NONE',  ( 4.916704032076687270, -0.7149955815140829340, -1.996424279390257572 ) ) ;
#84507 = CARTESIAN_POINT ( 'NONE',  ( 6.047819040147648373, 9.213483425884394507, 1.199719254218452047 ) ) ;
#84508 = EDGE_CURVE ( 'NONE', #93339, #180365, #168141, .T. ) ;
#84509 = AXIS2_PLACEMENT_3D ( 'NONE', #34926, #186521, #6691 ) ;
#84510 = CARTESIAN_POINT ( 'NONE',  ( -8.136864746495904299, 12.64475930422059768, -0.7998128361456281477 ) ) ;
#84511 = CARTESIAN_POINT ( 'NONE',  ( 5.684946482831785275, 5.526859072925533134, -0.7998128361456231517 ) ) ;
#84512 = CARTESIAN_POINT ( 'NONE',  ( 2.641538584800803502, 1.894577224340647792, -0.8349662684224223863 ) ) ;
#84513 = CARTESIAN_POINT ( 'NONE',  ( 1.364683531249988757, 0.4468750003414206917, 0.000000000000000000 ) ) ;
#84516 = ORIENTED_EDGE ( 'NONE', *, *, #151365, .T. ) ;
#84515 = CARTESIAN_POINT ( 'NONE',  ( 4.037882060770150439, -2.125535223720369071, 0.6451317522137323124 ) ) ;
#84514 = CIRCLE ( 'NONE', #164157, 0.04999999999999970440 ) ;
#84517 = CARTESIAN_POINT ( 'NONE',  ( 2.620138118368781743, 0.2850873451692262361, 2.280912332010568644 ) ) ;
#84518 = CARTESIAN_POINT ( 'NONE',  ( 7.117667457494414762, 11.24776976714476184, 1.040834085586084257E-14 ) ) ;
#84520 = CARTESIAN_POINT ( 'NONE',  ( 3.285556943750000070, -3.084374999522042415, 0.000000000000000000 ) ) ;
#84519 = CARTESIAN_POINT ( 'NONE',  ( 2.878073747850912412, 6.579779482459851003, -0.7998128361456362523 ) ) ;
#84521 = PLANE ( 'NONE',  #82068 ) ;
#84522 = DIRECTION ( 'NONE',  ( -1.000000000000000000, 5.578564026256504688E-16, 0.000000000000000000 ) ) ;
#84523 = ORIENTED_EDGE ( 'NONE', *, *, #176754, .T. ) ;
#84524 = CARTESIAN_POINT ( 'NONE',  ( -0.4294425147611466986, -9.199999999999988631, 9.490288674561783822 ) ) ;
#84525 = CARTESIAN_POINT ( 'NONE',  ( 4.324404969281474109, -0.8226261416362996570, -1.726585468271451651 ) ) ;
#84526 = CARTESIAN_POINT ( 'NONE',  ( -0.2091928449107274546, 6.366027919468703722, -3.121370559291495539 ) ) ;
#84527 = CARTESIAN_POINT ( 'NONE',  ( 4.840679758638335883, 0.2971110944181546976, 1.698800604571904849 ) ) ;
#84528 = CARTESIAN_POINT ( 'NONE',  ( 3.889861467948488638, -2.010801299972611478, 0.1531677096566556318 ) ) ;
#84529 = CARTESIAN_POINT ( 'NONE',  ( 5.660817213934862480, 1.366460917787317930, 1.848312285176759717 ) ) ;
#84530 = CARTESIAN_POINT ( 'NONE',  ( 0.6125000000000019318, 1.229166667349464115, -1.060881119635941339 ) ) ;
#84531 = CARTESIAN_POINT ( 'NONE',  ( 0.1884680354247054990, -1.036234488384666586, 1.948478269905975946 ) ) ;
#84532 = CARTESIAN_POINT ( 'NONE',  ( -4.475600106286965918, 8.235634200727838916, 0.7216878364870338292 ) ) ;
#84533 = CARTESIAN_POINT ( 'NONE',  ( 5.712081065023381754, -0.7967057657092267986, -1.580296573674238259 ) ) ;
#84535 = CARTESIAN_POINT ( 'NONE',  ( 1.465189672511356900, 0.1648890142370383061, -2.286389102023842490 ) ) ;
#84534 = CARTESIAN_POINT ( 'NONE',  ( 4.766573523656222555, 7.718696989977711809, 1.199719254218452047 ) ) ;
#84536 = CARTESIAN_POINT ( 'NONE',  ( 0.4798830478778244868, -0.2081801751476043960, -1.727770289196085329 ) ) ;
#84537 = DIRECTION ( 'NONE',  ( -1.665334536937739149E-15, 5.551115123125797493E-17, -1.000000000000000000 ) ) ;
#84538 = SURFACE_STYLE_FILL_AREA ( #150628 ) ;
#84539 = CARTESIAN_POINT ( 'NONE',  ( -4.034433228518296666, 6.864533312316751790, -1.199719254218450271 ) ) ;
#84540 = CARTESIAN_POINT ( 'NONE',  ( -1.360316468750028651, -0.8281249996586054207, -3.469446951953614189E-14 ) ) ;
#84541 = CARTESIAN_POINT ( 'NONE',  ( 0.5445930744353757458, 3.250057683544679943, 0.3999999999999542255 ) ) ;
#84542 = CARTESIAN_POINT ( 'NONE',  ( 0.5905675304203241716, 1.115885162268255293, -1.862360684160404123 ) ) ;
#84543 = CARTESIAN_POINT ( 'NONE',  ( 1.288296401830712368, -0.7303101666344159471, -1.879802715551846859 ) ) ;
#84544 = CARTESIAN_POINT ( 'NONE',  ( 0.7499999999999867883, -0.1520833326505155458, -1.299038105676652899 ) ) ;
#84545 = CARTESIAN_POINT ( 'NONE',  ( 5.039640240021522999, -1.363685002003648616, -1.361047059521299785 ) ) ;
#84546 = CARTESIAN_POINT ( 'NONE',  ( -8.012344526598182026E-15, 11.04687500034139980, -1.575800808251669460 ) ) ;
#84547 = AXIS2_PLACEMENT_3D ( 'NONE', #182979, #54057, #202403 ) ;
#84548 = CARTESIAN_POINT ( 'NONE',  ( 2.584490447655915624, 1.192291587189574065, 1.874175285706691341 ) ) ;
#84549 = ORIENTED_EDGE ( 'NONE', *, *, #132737, .T. ) ;
#84551 = DIRECTION ( 'NONE',  ( 3.330669073875478989E-16, -4.632576442341012461E-16, -1.000000000000000000 ) ) ;
#84550 = CARTESIAN_POINT ( 'NONE',  ( 1.499999999999821032, 7.240846818246208905, -4.154462424328214887 ) ) ;
#84552 = CARTESIAN_POINT ( 'NONE',  ( 3.777440027531570266, 7.356463756349603145, 0.3513329828547242517 ) ) ;
#84553 = CARTESIAN_POINT ( 'NONE',  ( 10.24048609702354717, 10.84165528948263457, -0.7998128361456281477 ) ) ;
#84554 = CYLINDRICAL_SURFACE ( 'NONE', #63075, 6.249999999999995559 ) ;
#84555 = LINE ( 'NONE', #86689, #204728 ) ;
#84556 = CARTESIAN_POINT ( 'NONE',  ( 4.141972075035261547, 0.4693275899197508760, 1.675879475284934195 ) ) ;
#84557 = CARTESIAN_POINT ( 'NONE',  ( 2.189831975649577878, -1.279155337443920404, -1.487614327915102619 ) ) ;
#84559 = CARTESIAN_POINT ( 'NONE',  ( -7.537970219518091319, 7.896646132300314314, -0.7216878364870278340 ) ) ;
#84558 = CARTESIAN_POINT ( 'NONE',  ( 3.659811400685081040, 6.357198169852855685, -1.199719254218446718 ) ) ;
#84560 = FILL_AREA_STYLE ('',( #34733 ) ) ;
#84561 = CARTESIAN_POINT ( 'NONE',  ( 1.082570677935968062, 1.230128212588364356, -1.655568962787755005 ) ) ;
#84562 = CARTESIAN_POINT ( 'NONE',  ( -7.344766530301162000, 9.591980256816594164, 1.599625672291295375 ) ) ;
#84563 = SHAPE_REPRESENTATION ( 'MAS-692', ( #207832, #27890, #100542, #59109, #128323, #159309, #34824, #62517, #180180, #197335, #90213, #211241, #103962, #173239, #186969, #138757, #69589, #100697, #14249, #187122, #135354, #3876, #207992 ), #86790 ) ;
#84564 = CARTESIAN_POINT ( 'NONE',  ( -4.487385655998893164, 6.258369236797239665, 1.443375672974064550 ) ) ;
#84565 = CIRCLE ( 'NONE', #74224, 10.25000000000000000 ) ;
#84566 = CARTESIAN_POINT ( 'NONE',  ( 1.024742985469536016, 1.345695571256789513, -1.818664117639690714 ) ) ;
#84567 = EDGE_LOOP ( 'NONE', ( #99280, #39674, #106208, #27268 ) ) ;
#84568 = CARTESIAN_POINT ( 'NONE',  ( 0.7499999999999867883, 0.09791666734948467621, -1.299038105676652899 ) ) ;
#84570 = CARTESIAN_POINT ( 'NONE',  ( 2.530351333283612281, 1.813318468827030072, 0.4585936022679508728 ) ) ;
#84569 = B_SPLINE_CURVE_WITH_KNOTS ( 'NONE', 3,
 ( #54164, #134383, #120302, #52033, #186276, #37913, #101843, #135423, #201445, #53088, #119221, #103988, #71450, #137563, #33639, #99712, #7521, #121378, #174335, #26978, #142917, #24847, #10726, #187352, #154868, #206797, #123526, #173266 ),
 .UNSPECIFIED., .F., .F.,
 ( 4, 2, 2, 2, 2, 2, 2, 1, 2, 2, 1, 2, 2, 2, 4 ),
 ( 0.9162434286749613355, 0.9214697481986482419, 0.9240829079604917506, 0.9266960677223353704, 0.9319223872460228320, 0.9371487067697102935, 0.9423750262933977551, 0.9476013458170851056, 0.9528276653407725671, 0.9554408251026164089, 0.9580539848644601397, 0.9685066239118349518, 0.9737329434355221913, 0.9789592629592095419, 0.9998645410539588330 ),
 .UNSPECIFIED. ) ;
#84571 = CARTESIAN_POINT ( 'NONE',  ( 1.547078507373225165, -1.226440487959565173, 1.226290910655163380 ) ) ;
#84572 = CARTESIAN_POINT ( 'NONE',  ( 4.933237592207079025, -1.549687834843778811, -1.549900206446311657 ) ) ;
#84573 = CARTESIAN_POINT ( 'NONE',  ( 5.210162647842351724, -2.297074225899544242, 0.2200332968223562558 ) ) ;
#84574 = CARTESIAN_POINT ( 'NONE',  ( 1.797801859905317823, -0.6954313725856995365, 1.940136720205553278 ) ) ;
#84575 = CARTESIAN_POINT ( 'NONE',  ( 3.064326467805338350, -1.794528509343394473, -0.7426413790867588682 ) ) ;
#84576 = CARTESIAN_POINT ( 'NONE',  ( -5.070386261386537363, 5.017798181146802428, 1.214306433183764966E-14 ) ) ;
#84577 = AXIS2_PLACEMENT_3D ( 'NONE', #176102, #61270, #194467 ) ;
#84578 = CARTESIAN_POINT ( 'NONE',  ( 6.239502018287079288, -1.354773164471131164, -1.289998633004642237 ) ) ;
#84579 = CARTESIAN_POINT ( 'NONE',  ( 1.656250000000001554, -1.895863743164051485, 0.7852924748300756930 ) ) ;
#84580 = CARTESIAN_POINT ( 'NONE',  ( 1.406843869218815657, 13.32828740661201472, -0.1535876347566223210 ) ) ;
#84581 = CARTESIAN_POINT ( 'NONE',  ( 0.1570416503036062006, -0.3615154868755916517, -1.700924732364687220 ) ) ;
#84582 = EDGE_CURVE ( 'NONE', #58688, #112883, #201098, .T. ) ;
#84583 = CARTESIAN_POINT ( 'NONE',  ( 5.261973015879598314, 5.311592404713873172, -0.7216878364870458196 ) ) ;
#84584 = CARTESIAN_POINT ( 'NONE',  ( 1.360316468749983576, 1.515625000341386253, -4.163336342344337027E-14 ) ) ;
#84585 = CARTESIAN_POINT ( 'NONE',  ( 4.113907844847329187, 0.1017495355152969322, 2.013985960686740295 ) ) ;
#84586 = CARTESIAN_POINT ( 'NONE',  ( -2.751941993449643409, 6.154423392425789174, 0.7216878364870317197 ) ) ;
#84587 = CARTESIAN_POINT ( 'NONE',  ( 9.582915646760733708, 10.07448976417602893, 0.7998128361456462443 ) ) ;
#84588 = CARTESIAN_POINT ( 'NONE',  ( 4.228163802615382494, 6.026220084508304708, -1.599625672291269396 ) ) ;
#84590 = CARTESIAN_POINT ( 'NONE',  ( 1.255262969126037241E-15, 2.000000000000001776, -10.25000000000000000 ) ) ;
#84589 = CARTESIAN_POINT ( 'NONE',  ( 2.314841291766779108, 1.630546960418734148, 0.8213866120303781049 ) ) ;
#84591 = CARTESIAN_POINT ( 'NONE',  ( -4.285259070371116863, 7.157163461145040095, 1.199719254218452935 ) ) ;
#84592 = CARTESIAN_POINT ( 'NONE',  ( 2.550000000000000266, -7.105553651663779391, -1.849324200890695824 ) ) ;
#84593 = ORIENTED_EDGE ( 'NONE', *, *, #88639, .F. ) ;
#84594 = CARTESIAN_POINT ( 'NONE',  ( -4.462041952228942954, 8.219816354326809460, -0.7216878364870338292 ) ) ;
#84595 = CARTESIAN_POINT ( 'NONE',  ( -2.103486388414573138, 5.605817886458954291, 1.040834085586084257E-14 ) ) ;
#84596 = CARTESIAN_POINT ( 'NONE',  ( -7.947050595904583403, 12.42330946186405249, 0.7998128361456481317 ) ) ;
#84597 = CARTESIAN_POINT ( 'NONE',  ( 0.4572932007271997001, -1.730182198833930318, 1.041906760498239271 ) ) ;
#84599 = EDGE_LOOP ( 'NONE', ( #156978, #128271, #38175, #80308, #91739 ) ) ;
#84598 = CARTESIAN_POINT ( 'NONE',  ( 0.4168467196605326053, -0.7183999135813922132, -1.995210048009891102 ) ) ;
#84600 = CARTESIAN_POINT ( 'NONE',  ( -6.074935347375019390, 9.245119117649618801, 1.199719254218452047 ) ) ;
#84601 = CARTESIAN_POINT ( 'NONE',  ( 5.087333953625774008, 6.958308917361963886, 1.599625672291267398 ) ) ;
#84602 = CARTESIAN_POINT ( 'NONE',  ( 5.524313221898556669, 1.229557446212639071, -1.653754484787550494 ) ) ;
#84603 = CARTESIAN_POINT ( 'NONE',  ( 5.186172726741035355, 1.650080556555008293, 1.158690440749516881 ) ) ;
#84604 = ORIENTED_EDGE ( 'NONE', *, *, #178698, .F. ) ;
#84605 = CARTESIAN_POINT ( 'NONE',  ( 4.738043757352738083, 4.889522902105694513, -0.8057966945447234686 ) ) ;
#84606 = CARTESIAN_POINT ( 'NONE',  ( -0.2108831679770960255, 0.2438762813419328990, -1.931650693707862132 ) ) ;
#84608 = ORIENTED_EDGE ( 'NONE', *, *, #202732, .F. ) ;
#84607 = CARTESIAN_POINT ( 'NONE',  ( -5.108390017298964914, 9.181815130149269422, 0.000000000000000000 ) ) ;
#84609 = CARTESIAN_POINT ( 'NONE',  ( 4.684384365712907616, 8.380862967975740929, 0.5977175665230231028 ) ) ;
#84610 = CARTESIAN_POINT ( 'NONE',  ( 5.413435409655408925, 0.5825687168248098180, 1.930121546480124461 ) ) ;
#84611 = CARTESIAN_POINT ( 'NONE',  ( 4.435397664686764330, 0.7849604969769330420, -1.665558179074405620 ) ) ;
#84612 = CARTESIAN_POINT ( 'NONE',  ( 0.07661050522431847587, 7.629137130509112907, -2.310792076560589603 ) ) ;
#84613 = CARTESIAN_POINT ( 'NONE',  ( 2.174872218848258765, -1.417835807431093276, 1.820694940605925849 ) ) ;
#84614 = CARTESIAN_POINT ( 'NONE',  ( 6.318982112420993502, 9.529840343536603697, -1.199719254218452047 ) ) ;
#84615 = CARTESIAN_POINT ( 'NONE',  ( 5.132170659515546518, 1.116069247042193124, -1.851066442873222639 ) ) ;
#84616 = CARTESIAN_POINT ( 'NONE',  ( 7.904567251967224095, 9.180748867838630645, 1.199719254218462483 ) ) ;
#84617 = CARTESIAN_POINT ( 'NONE',  ( 0.2220789341932476180, 1.858810982918417620, 0.5625763381651854855 ) ) ;
#84618 = CARTESIAN_POINT ( 'NONE',  ( -3.588104209110990706, 7.337872010604796991, 1.040834085586084257E-14 ) ) ;
#84619 = CARTESIAN_POINT ( 'NONE',  ( -1.123270288250315163, 2.985197346350006331, -0.7749999999993613109 ) ) ;
#84620 = CARTESIAN_POINT ( 'NONE',  ( -3.318713740295064163, 7.093859473644694269, 0.000000000000000000 ) ) ;
#84621 = CARTESIAN_POINT ( 'NONE',  ( 3.713615009860570915, -1.843089489661839053, 0.3189824552965599969 ) ) ;
#84624 = CARTESIAN_POINT ( 'NONE',  ( -4.586401103172829785, 8.572828063668767484, 0.7998128361456281477 ) ) ;
#84623 = CARTESIAN_POINT ( 'NONE',  ( -0.7500000000000249800, -0.5270833326505158789, 1.299038105676659116 ) ) ;
#84622 = CARTESIAN_POINT ( 'NONE',  ( 0.7910927259777954523, -0.04954035392716604758, -1.911929172785244102 ) ) ;
#84625 = CARTESIAN_POINT ( 'NONE',  ( 2.719571217284349363, -0.2154062111461417517, 2.196339928330424129 ) ) ;
#84626 = ADVANCED_FACE ( 'NONE', ( #128068 ), #143204, .F. ) ;
#84627 = CARTESIAN_POINT ( 'NONE',  ( -4.540505084823442949, 7.125209978135113253, 1.295423358617282972 ) ) ;
#84628 = CARTESIAN_POINT ( 'NONE',  ( 3.330499290451326200, 7.037332938835193730, -0.7998128361456291469 ) ) ;
#84629 = CARTESIAN_POINT ( 'NONE',  ( 7.987161891782087686, 8.490979426600148372, -0.7216878364870317197 ) ) ;
#84630 = CARTESIAN_POINT ( 'NONE',  ( -3.438964519360665051, 7.163875705896082913, -0.7998128361456281477 ) ) ;
#84631 = CARTESIAN_POINT ( 'NONE',  ( -5.750066545527201534, 9.722511713174800008, 0.000000000000000000 ) ) ;
#84632 = CARTESIAN_POINT ( 'NONE',  ( 1.036326318785439016, 1.941456103877332140, 0.3412654001589945918 ) ) ;
#84633 = CARTESIAN_POINT ( 'NONE',  ( 0.1304780226794301778, -1.424241760892838382, -1.816604428824322159 ) ) ;
#84634 = CARTESIAN_POINT ( 'NONE',  ( 1.064813361795993618, 1.487921858168140377, -1.278797858372302088 ) ) ;
#84635 = CARTESIAN_POINT ( 'NONE',  ( 3.854389151762872778, -2.059979072249884080, -0.1062074158154867054 ) ) ;
#84636 = CARTESIAN_POINT ( 'NONE',  ( 5.829642864196162400, 7.824335979694092558, 1.443375672974062551 ) ) ;
#84637 = CARTESIAN_POINT ( 'NONE',  ( 6.964048179274811012, 8.153752959689313684, 1.199719254218452047 ) ) ;
#84638 = VERTEX_POINT ( 'NONE', #46741 ) ;
#84639 = CARTESIAN_POINT ( 'NONE',  ( 6.602457619730749627, 10.64669162308715222, 0.7216878364870438212 ) ) ;
#84640 = CARTESIAN_POINT ( 'NONE',  ( -1.201851678989727383E-14, 5.259375000341421469, -1.575800808251660134 ) ) ;
#84641 = DIRECTION ( 'NONE',  ( 0.000000000000000000, 9.023263958591318651E-17, -1.000000000000000000 ) ) ;
#84642 = CARTESIAN_POINT ( 'NONE',  ( 5.165293336682183600, 5.128523102325077687, -0.7216878364870197293 ) ) ;
#84643 = CARTESIAN_POINT ( 'NONE',  ( 6.478989045741552211, 2.023467559352111866, 0.7875856005067942700 ) ) ;
#84645 = CARTESIAN_POINT ( 'NONE',  ( 6.198766299729112639, 1.534709720371667308, 1.016988835930050739 ) ) ;
#84644 = CARTESIAN_POINT ( 'NONE',  ( 9.590670562337447080, -9.593477663480472373, -0.1674057773689586193 ) ) ;
#84646 = EDGE_CURVE ( 'NONE', #195163, #170224, #124986, .T. ) ;
#84647 = TOROIDAL_SURFACE ( 'NONE', #153763, 11.92000000000000171, 0.08000000000000000167 ) ;
#84648 = CARTESIAN_POINT ( 'NONE',  ( 5.503988762639142607, 6.221932061145267312, -0.9643604338056003256 ) ) ;
#84649 = CARTESIAN_POINT ( 'NONE',  ( -10.50059885609813115, 5.377696206510352184, -5.808392519734754345 ) ) ;
#84650 = CARTESIAN_POINT ( 'NONE',  ( 1.686563950722594685, -0.2693046698774223535, -1.850923959389898288 ) ) ;
#84651 = CARTESIAN_POINT ( 'NONE',  ( -6.138286310890375574, 5.995785266799176227, -0.01092221066891288506 ) ) ;
#84652 = CARTESIAN_POINT ( 'NONE',  ( -2.535011536075354677, 5.133042487381361596, -7.499999999999997335 ) ) ;
#84653 = CARTESIAN_POINT ( 'NONE',  ( 5.561552386509557522, 7.525632394756676113, -1.337405013919689800 ) ) ;
#84654 = CARTESIAN_POINT ( 'NONE',  ( -1.364683531249997417, 5.571875000341417916, 1.214306433183764966E-14 ) ) ;
#84655 = CARTESIAN_POINT ( 'NONE',  ( 1.049298088506251947, -1.728493729547800895, 0.8183166869351959916 ) ) ;
#84656 =( BOUNDED_CURVE ( )  B_SPLINE_CURVE ( 3, ( #60753, #10920, #63954, #126916 ),
 .UNSPECIFIED., .F., .T. ) 
 B_SPLINE_CURVE_WITH_KNOTS ( ( 4, 4 ),
 ( 1.576609981660940463, 1.599396078175049585 ),
 .UNSPECIFIED. ) 
 CURVE ( )  GEOMETRIC_REPRESENTATION_ITEM ( )  RATIONAL_B_SPLINE_CURVE ( ( 1.000000000000000000, 0.9999567332851475587, 0.9999567332851475587, 1.000000000000000000 ) ) 
 REPRESENTATION_ITEM ( '' )  );
#84657 = CARTESIAN_POINT ( 'NONE',  ( 3.291635156611854462, -0.7182737719314927771, 1.617730789815795545 ) ) ;
#84658 = CARTESIAN_POINT ( 'NONE',  ( 0.2231138172586397683, 1.663799575440491285, 0.9424754157791456199 ) ) ;
#84660 = CARTESIAN_POINT ( 'NONE',  ( 4.358935675595962955, -0.003970376728411328937, -1.915793142021319007 ) ) ;
#84659 = CARTESIAN_POINT ( 'NONE',  ( 0.000000000000000000, 15.50000000000019362, 0.000000000000000000 ) ) ;
#84661 = CARTESIAN_POINT ( 'NONE',  ( -0.1409997244345879974, 6.947781918643359589, -2.595319453918026653 ) ) ;
#84662 = CARTESIAN_POINT ( 'NONE',  ( 5.582459562482231519, 1.174703874196600495, -1.580708309230594688 ) ) ;
#84663 = CARTESIAN_POINT ( 'NONE',  ( 0.6156802735862785259, 1.737094954450137285, 1.216079458918501333 ) ) ;
#84664 = CARTESIAN_POINT ( 'NONE',  ( 0.000000000000000000, 13.49999999999999822, -1.500000000000000222 ) ) ;
#84665 = CARTESIAN_POINT ( 'NONE',  ( 3.731198135974967300, -1.728734619261709904, 0.7151963084984153118 ) ) ;
#84667 = EDGE_LOOP ( 'NONE', ( #152047, #127341 ) ) ;
#84666 = CARTESIAN_POINT ( 'NONE',  ( 0.8381832108898427114, 1.798179982845280467, 0.3147962740308178353 ) ) ;
#84669 = CARTESIAN_POINT ( 'NONE',  ( 10.04957930738609839, 3.829867255648771618, 5.932860765075322007 ) ) ;
#84668 = CARTESIAN_POINT ( 'NONE',  ( 3.211752199052122503, -0.4303563718574507369, 2.164345902561148005 ) ) ;
#84670 = CARTESIAN_POINT ( 'NONE',  ( -0.6823417656249969321, 4.280208333674755394, -1.181850606188749264 ) ) ;
#84671 = CARTESIAN_POINT ( 'NONE',  ( 0.5552253240413919100, 1.715889405040219584, -1.144428160675447614 ) ) ;
#84672 = CARTESIAN_POINT ( 'NONE',  ( 7.610204295972345712, 7.772993188256215547, 0.7998128361456341429 ) ) ;
#84674 = CARTESIAN_POINT ( 'NONE',  ( -9.667127221743832877, 11.23706883257798772, 1.199719254218462483 ) ) ;
#84673 = AXIS2_PLACEMENT_3D ( 'NONE', #1895, #71168, #152451 ) ;
#84675 = CARTESIAN_POINT ( 'NONE',  ( -4.363689859051672393, 15.44735444335154639, -11.13992621954916906 ) ) ;
#84676 = CARTESIAN_POINT ( 'NONE',  ( -3.424027514449416554, -0.02102871867356865404, -0.4191108859519457885 ) ) ;
#84677 = EDGE_CURVE ( 'NONE', #110107, #46524, #190582, .T. ) ;
#84678 = CARTESIAN_POINT ( 'NONE',  ( 0.1753634416057497925, 0.0001173177735149660839, -2.144164757042037017 ) ) ;
#84679 = VERTEX_POINT ( 'NONE', #31546 ) ;
#84680 = CARTESIAN_POINT ( 'NONE',  ( 3.613788337741298040, 0.5058112091442801272, -2.007490274132675445 ) ) ;
#84682 = CARTESIAN_POINT ( 'NONE',  ( -1.500000000000011324, 4.379166666666688634, -0.8660254037844313801 ) ) ;
#84681 = AXIS2_PLACEMENT_3D ( 'NONE', #65792, #114653, #131941 ) ;
#84683 = CARTESIAN_POINT ( 'NONE',  ( 1.440939128517594758, 0.4201678954103040819, 2.120193794684998245 ) ) ;
#84684 = CARTESIAN_POINT ( 'NONE',  ( -6.615421019548638704, 6.757903343899189785, 0.08170615477586136433 ) ) ;
#84685 = CARTESIAN_POINT ( 'NONE',  ( 1.822921661270057836, 1.494980448624585234, -1.358156064218164927 ) ) ;
#84686 = CARTESIAN_POINT ( 'NONE',  ( 0.000000000000000000, 11.37999999999998302, 0.000000000000000000 ) ) ;
#84687 = ORIENTED_EDGE ( 'NONE', *, *, #209983, .T. ) ;
#84689 = CARTESIAN_POINT ( 'NONE',  ( 9.273413882067330860, 9.921330405274451536, -0.7216878364870257245 ) ) ;
#84688 = CARTESIAN_POINT ( 'NONE',  ( -3.475000000000000533, -3.149999999999999911, 0.000000000000000000 ) ) ;
#84690 = CARTESIAN_POINT ( 'NONE',  ( 2.580963302752299349, 0.4788041664877049075, 0.000000000000000000 ) ) ;
#84691 = CARTESIAN_POINT ( 'NONE',  ( 0.7082206942033396624, 1.197301205363930254, -1.622488844446705381 ) ) ;
#84692 = CARTESIAN_POINT ( 'NONE',  ( 4.898067072109578035, -0.7382639882421681010, -2.063579870930781546 ) ) ;
#84693 = VECTOR ( 'NONE', #47029, 1000.000000000000000 ) ;
#84694 = CARTESIAN_POINT ( 'NONE',  ( 0.7499999999999902300, 3.014583334016149418, 1.299038105676669330 ) ) ;
#84695 = CARTESIAN_POINT ( 'NONE',  ( 3.797043250571481732, -0.1924442655423033721, -1.902711443722324258 ) ) ;
#84696 = CARTESIAN_POINT ( 'NONE',  ( -3.730464822054482710, 7.503959392372201442, 1.040834085586084257E-14 ) ) ;
#84697 = CARTESIAN_POINT ( 'NONE',  ( 5.151735183068521629, 5.112705256442466428, 1.040834085586084257E-14 ) ) ;
#84699 = CARTESIAN_POINT ( 'NONE',  ( 0.7906389332529573100, 1.525030349845598820, -1.319245847334844735 ) ) ;
#84698 = CARTESIAN_POINT ( 'NONE',  ( -10.45297324601190425, 11.29748299654313470, 0.7216878364870438212 ) ) ;
#84700 = CARTESIAN_POINT ( 'NONE',  ( -8.012344526598182026E-15, 12.10937500034140157, -1.575800808251669460 ) ) ;
#84702 = CARTESIAN_POINT ( 'NONE',  ( -4.294900800479008574, 8.232744377192641849, 0.000000000000000000 ) ) ;
#84701 = CARTESIAN_POINT ( 'NONE',  ( 0.9257723888009254942, -1.459437212925698502, -1.767766894381626486 ) ) ;
#84703 = CARTESIAN_POINT ( 'NONE',  ( 3.662884335446520367, -1.521034750653621481, -0.8131990640867832187 ) ) ;
#84704 = CARTESIAN_POINT ( 'NONE',  ( -4.370663978927101567, 5.060324124126029943, -1.009771797811724214 ) ) ;
#84705 = CARTESIAN_POINT ( 'NONE',  ( 4.009460741339333723, 5.700790169694431420, -1.599625672291256295 ) ) ;
#84706 = DIRECTION ( 'NONE',  ( 0.000000000000000000, -1.000000000000000000, -0.000000000000000000 ) ) ;
#84707 = CARTESIAN_POINT ( 'NONE',  ( 1.152704166800899932, -0.4732522875653189520, -1.903817266927515961 ) ) ;
#84708 = FACE_OUTER_BOUND ( 'NONE', #150070, .T. ) ;
#84709 = CARTESIAN_POINT ( 'NONE',  ( 4.436542580169809291, 6.199052314996659874, 1.599625672291267398 ) ) ;
#84710 = CARTESIAN_POINT ( 'NONE',  ( 0.07556134207192893859, 0.6772206542668850471, -2.324809334106460845 ) ) ;
#84711 = ORIENTED_EDGE ( 'NONE', *, *, #87773, .F. ) ;
#84712 = FILL_AREA_STYLE ('',( #100950 ) ) ;
#84713 = VERTEX_POINT ( 'NONE', #162612 ) ;
#84714 = CARTESIAN_POINT ( 'NONE',  ( 3.492628052329676880, -1.746589362535276191, -0.4802254367691183856 ) ) ;
#84715 = ORIENTED_EDGE ( 'NONE', *, *, #80739, .F. ) ;
#84716 = CARTESIAN_POINT ( 'NONE',  ( 6.180537922983273091, 8.303989891604203422, -1.599625672291281386 ) ) ;
#84717 = CARTESIAN_POINT ( 'NONE',  ( 4.951724851890283219, -1.284874556838147219, -1.277195305962516292 ) ) ;
#84718 = CARTESIAN_POINT ( 'NONE',  ( 7.146556367734776316, 7.510272981878305387, 0.7216878364870267237 ) ) ;
#84719 = SURFACE_STYLE_USAGE ( .BOTH. , #167048 ) ;
#84720 = CARTESIAN_POINT ( 'NONE',  ( 5.253083726123439767, 6.394172465367824465, -1.148862164228587890 ) ) ;
#84722 = CARTESIAN_POINT ( 'NONE',  ( 10.21336978979620191, 10.81001959771741205, 0.7998128361456462443 ) ) ;
#84721 = CARTESIAN_POINT ( 'NONE',  ( 6.355886303346764521, -0.6260325832568144344, 1.752714347800623518 ) ) ;
#84723 = CARTESIAN_POINT ( 'NONE',  ( 3.321808155663192874, 0.8583493116562285197, -1.712590381118280991 ) ) ;
#84724 = CARTESIAN_POINT ( 'NONE',  ( 4.828112100242276661, 6.726159765073026264, -1.443375672974068769 ) ) ;
#84725 = CARTESIAN_POINT ( 'NONE',  ( -10.84554942614793127, 5.653270432668692891, -6.476099931950408006 ) ) ;
#84726 = CIRCLE ( 'NONE', #18982, 0.08000000000000020983 ) ;
#84727 = CARTESIAN_POINT ( 'NONE',  ( 0.000000000000000000, 2.000000000000001776, 0.000000000000000000 ) ) ;
#84728 = CARTESIAN_POINT ( 'NONE',  ( -1.402160292154681736E-14, -0.9281249996585830830, 1.575800808251672791 ) ) ;
#84729 = CARTESIAN_POINT ( 'NONE',  ( 6.968527767744109980, 7.232296605230681408, 0.7216878364870317197 ) ) ;
#84730 = CARTESIAN_POINT ( 'NONE',  ( -9.110716038703348119, 12.61262389758715408, 1.082531754730560403 ) ) ;
#84731 = CARTESIAN_POINT ( 'NONE',  ( 0.6026772488060898603, -0.7295331166810550272, -2.035022307366324945 ) ) ;
#84732 = CARTESIAN_POINT ( 'NONE',  ( -4.450819567036169211, 8.414649604842665553, -0.7998128361456362523 ) ) ;
#84733 = VECTOR ( 'NONE', #164682, 1000.000000000000114 ) ;
#84734 = CARTESIAN_POINT ( 'NONE',  ( 4.044074958626150185, 7.940114228364351767, 0.7998128361456271485 ) ) ;
#84735 = CARTESIAN_POINT ( 'NONE',  ( 0.7623938366894518204, -1.325735992016435105, 1.255310662410371370 ) ) ;
#84736 = CARTESIAN_POINT ( 'NONE',  ( -6.254388934605767503, 6.191208599995166040, 0.7998128361456341429 ) ) ;
#84737 = CARTESIAN_POINT ( 'NONE',  ( 3.575057022766346293, 0.04566639709948847742, -1.825179878808772305 ) ) ;
#84738 = CARTESIAN_POINT ( 'NONE',  ( 12.54948750854022954, 7.400697955233512815, 0.9574523190714994136 ) ) ;
#84739 = CARTESIAN_POINT ( 'NONE',  ( 2.197387184563174944, 1.746976956643018442, -0.7784620831182070821 ) ) ;
#84740 = VERTEX_POINT ( 'NONE', #12077 ) ;
#84741 = CARTESIAN_POINT ( 'NONE',  ( 3.244544899158372520, -1.939951241085198896, -0.3392403660903812734 ) ) ;
#84742 = CARTESIAN_POINT ( 'NONE',  ( 5.390160969041248862, -0.4756269310413098750, -1.882793909387857179 ) ) ;
#84743 = CARTESIAN_POINT ( 'NONE',  ( -5.915100157312088491, 10.12297696016459092, -0.7998128361456362523 ) ) ;
#84745 = CARTESIAN_POINT ( 'NONE',  ( 4.254221937059123881, 0.9039275175388861161, -1.918405034562712830 ) ) ;
#84744 = CARTESIAN_POINT ( 'NONE',  ( 5.110497557708379546, 4.926945003606695295, -0.7998128361456481317 ) ) ;
#84746 = CARTESIAN_POINT ( 'NONE',  ( 11.01135777277262306, 10.09374813218825473, 1.399999999999998579 ) ) ;
#84747 = CARTESIAN_POINT ( 'NONE',  ( 9.745613490124728884, 10.26430391476735338, 0.7998128361456462443 ) ) ;
#84748 = CARTESIAN_POINT ( 'NONE',  ( 5.870433092755101612, 6.171306251675328092, 0.8628692295504901688 ) ) ;
#84749 = CARTESIAN_POINT ( 'NONE',  ( -1.150196859685088002, 3.060958678954801115, -0.7749999999999883649 ) ) ;
#84750 = ORIENTED_EDGE ( 'NONE', *, *, #82708, .T. ) ;
#84751 = CARTESIAN_POINT ( 'NONE',  ( 11.01135777277262306, 0.000000000000000000, -1.400000000000001910 ) ) ;
#84752 = CARTESIAN_POINT ( 'NONE',  ( 4.039439701867726384, 6.800097854565950506, 1.199719254218462483 ) ) ;
#84753 = CARTESIAN_POINT ( 'NONE',  ( 4.701645408888975197, 8.707279753670952971, 0.000000000000000000 ) ) ;
#84754 = DIRECTION ( 'NONE',  ( 0.000000000000000000, 0.000000000000000000, 1.000000000000000000 ) ) ;
#84755 = CARTESIAN_POINT ( 'NONE',  ( 5.549374350267230582, -1.441814640532925074, -1.119852386600270533 ) ) ;
#84756 = CARTESIAN_POINT ( 'NONE',  ( 10.99949329275126253, -9.914220445327725173, -0.1055954338740888176 ) ) ;
#84757 = CARTESIAN_POINT ( 'NONE',  ( -8.920901888112002354, 11.43080484092926241, 1.443375672974064550 ) ) ;
#84758 = CARTESIAN_POINT ( 'NONE',  ( -4.745581203565001793, 8.305819929356548670, 0.7838639097331673300 ) ) ;
#84759 = DIRECTION ( 'NONE',  ( 1.165734175856416734E-15, -0.5005768354468322912, -0.8656921114426507913 ) ) ;
#84760 = CARTESIAN_POINT ( 'NONE',  ( 5.770339134078734666, -1.185559297855027561, 1.446973003893243348 ) ) ;
#84761 = CARTESIAN_POINT ( 'NONE',  ( 8.260995669428309540, 8.532249790621511565, 0.7998128361456481317 ) ) ;
#84762 = CARTESIAN_POINT ( 'NONE',  ( 3.475144788579834110, 0.04656949993332368254, -1.926097043150078791 ) ) ;
#84763 = CARTESIAN_POINT ( 'NONE',  ( -3.276266675996675204, 6.974061555304760240, -0.7998128361456282587 ) ) ;
#84764 = EDGE_CURVE ( 'NONE', #144610, #197667, #135270, .T. ) ;
#84765 = CARTESIAN_POINT ( 'NONE',  ( 2.693266070609028784, 6.293894182352508970, 0.000000000000000000 ) ) ;
#84766 = CARTESIAN_POINT ( 'NONE',  ( -1.364683531250000748, 9.421875000341396245, 0.000000000000000000 ) ) ;
#84767 = CARTESIAN_POINT ( 'NONE',  ( -6.112028321662274166, 6.025121218227761588, 0.7998128361456341429 ) ) ;
#84768 = CARTESIAN_POINT ( 'NONE',  ( 3.765413976293345844, 5.416068943807445635, 1.599625672291267398 ) ) ;
#84769 = CARTESIAN_POINT ( 'NONE',  ( -4.950135482320939140, 4.947781948895412008, -0.7216878364870338292 ) ) ;
#84770 = AXIS2_PLACEMENT_3D ( 'NONE', #74632, #140739, #158031 ) ;
#84771 = CARTESIAN_POINT ( 'NONE',  ( 0.7732552308061869661, 1.865071980587120315, -1.002124039132473055 ) ) ;
#84772 = CARTESIAN_POINT ( 'NONE',  ( 8.432281472695482449, 11.92507992053172572, 1.199719254218450271 ) ) ;
#84773 = CARTESIAN_POINT ( 'NONE',  ( 0.4084509640503868333, 6.973232988006186517, 3.930977317341532107 ) ) ;
#84774 = CARTESIAN_POINT ( 'NONE',  ( 5.893440691016273547, -1.874049447596724427, 0.8799615681738190975 ) ) ;
#84776 = CARTESIAN_POINT ( 'NONE',  ( 4.067188154045468629, 7.737431308562400467, -0.5659913801023385149 ) ) ;
#84775 = CARTESIAN_POINT ( 'NONE',  ( 1.663359199420410883, 0.9473472845980964729, 1.578708189602283873 ) ) ;
#84777 = CARTESIAN_POINT ( 'NONE',  ( 6.805829924380118356, 7.042482454639357847, 0.7216878364870317197 ) ) ;
#84779 = CARTESIAN_POINT ( 'NONE',  ( 0.4784947886781562576, 6.877463695696398815, 3.690354617645239976 ) ) ;
#84778 = CARTESIAN_POINT ( 'NONE',  ( 4.014622883422321209, 5.777089012116397804, -1.443375672974068769 ) ) ;
#84780 = CARTESIAN_POINT ( 'NONE',  ( 2.010137459244505820, -1.083026110817113086, -2.020279618534262855 ) ) ;
#84781 = CARTESIAN_POINT ( 'NONE',  ( -0.01727558406095473439, -0.1313277740116538805, -1.795991579427682838 ) ) ;
#84782 = ORIENTED_EDGE ( 'NONE', *, *, #165066, .F. ) ;
#84783 = CARTESIAN_POINT ( 'NONE',  ( 7.741342523278698096, 10.05465224862374285, 1.443375672974076540 ) ) ;
#84784 = EDGE_CURVE ( 'NONE', #70814, #10691, #129129, .T. ) ;
#84785 = CARTESIAN_POINT ( 'NONE',  ( 0.6682274066662279299, 2.010706302723582972, -0.1030755154480169355 ) ) ;
#84786 = CARTESIAN_POINT ( 'NONE',  ( 1.375751926856683127, -1.915142299924106339, 0.4244507266663796741 ) ) ;
#84787 = CARTESIAN_POINT ( 'NONE',  ( 3.189213936345663747, 2.817530495244580102, -2.450448857954562243 ) ) ;
#84789 = CARTESIAN_POINT ( 'NONE',  ( -10.33433454857960321, 4.766519530047388820, -5.444264161973041638 ) ) ;
#84788 = CARTESIAN_POINT ( 'NONE',  ( -8.799405390469187793, 10.22472669609091689, -1.199719254218446718 ) ) ;
#84790 = DIRECTION ( 'NONE',  ( -0.000000000000000000, -1.000000000000000000, -0.000000000000000000 ) ) ;
#84792 = CARTESIAN_POINT ( 'NONE',  ( 2.729092984789914578, -1.652188407247729529, 0.6350153418272014294 ) ) ;
#84791 = CARTESIAN_POINT ( 'NONE',  ( 4.189459526602421491, -0.8002100119003925371, 1.931633446273020693 ) ) ;
#84793 = DIRECTION ( 'NONE',  ( 1.000000000000000000, 0.000000000000000000, 0.000000000000000000 ) ) ;
#84795 = CARTESIAN_POINT ( 'NONE',  ( 5.261813964552005451, 1.126222290254262015, 1.996463630829442337 ) ) ;
#84794 = CARTESIAN_POINT ( 'NONE',  ( -12.00015887837301420, 8.029270226016196332, -0.2577645811446898638 ) ) ;
#84796 = CARTESIAN_POINT ( 'NONE',  ( 3.345385115808647392, 1.740516467222261499, -0.001323508237265763176 ) ) ;
#84797 = CARTESIAN_POINT ( 'NONE',  ( 9.215791728987056786, 11.77484298861683598, -1.599625672291262513 ) ) ;
#84798 = CARTESIAN_POINT ( 'NONE',  ( 6.398522151006641678, 6.429640362454684954, 0.000000000000000000 ) ) ;
#84799 = CARTESIAN_POINT ( 'NONE',  ( 3.795997188448175130, -1.602592684597732298, 0.6622489764130984335 ) ) ;
#84800 = CARTESIAN_POINT ( 'NONE',  ( 4.035715546050927749, 2.045666111725014780, -0.7279006231073074096 ) ) ;
#84801 = CARTESIAN_POINT ( 'NONE',  ( 3.798255590122797898, 7.583048621785260401, -0.7998128361456221525 ) ) ;
#84802 = CARTESIAN_POINT ( 'NONE',  ( 4.680875185974167074, 1.673856063443099895, -1.124242729735332347 ) ) ;
#84803 = CARTESIAN_POINT ( 'NONE',  ( 1.218750000000000888, -0.7852924748299231483, 1.895863743164115656 ) ) ;
#84804 = CARTESIAN_POINT ( 'NONE',  ( 1.499999999999990896, 4.556250000682819490, 1.214306433183764966E-14 ) ) ;
#84805 = CARTESIAN_POINT ( 'NONE',  ( 1.782126058915745936, -1.032679515686143024, 1.626040290554785717 ) ) ;
#84806 = CARTESIAN_POINT ( 'NONE',  ( -0.6823417656250003738, 15.15104166700806410, 1.181850606188754593 ) ) ;
#84807 = CARTESIAN_POINT ( 'NONE',  ( 5.801095770108652516, -0.3255204119565913157, -2.197341616521626406 ) ) ;
#84808 = ORIENTED_EDGE ( 'NONE', *, *, #127713, .F. ) ;
#84809 = CARTESIAN_POINT ( 'NONE',  ( 6.883263157960391787, -0.001104538646235289417, 1.946037152736757925 ) ) ;
#84810 = CARTESIAN_POINT ( 'NONE',  ( 1.499999999999987121, 1.504166666666690411, 0.8660254037844524744 ) ) ;
#84811 = CARTESIAN_POINT ( 'NONE',  ( 6.124532705071213279, 8.168374127381657246, -1.599625672291262513 ) ) ;
#84812 = CARTESIAN_POINT ( 'NONE',  ( 5.355107487273504496, 6.310342158982962246, -1.082531754730543083 ) ) ;
#84813 = CARTESIAN_POINT ( 'NONE',  ( 1.642778471875001811, -1.392708332855374653, 2.845375778867859751 ) ) ;
#84814 = CARTESIAN_POINT ( 'NONE',  ( 0.7334294796089964041, 2.054545164755026576, 0.8448789909778311458 ) ) ;
#84815 = CARTESIAN_POINT ( 'NONE',  ( 6.127397123722368555, 0.1457569626216181913, -1.956525209266091192 ) ) ;
#84816 = CARTESIAN_POINT ( 'NONE',  ( 8.758204044748005401, 10.28062147603659504, 1.082531754730549967 ) ) ;
#84817 = CARTESIAN_POINT ( 'NONE',  ( 0.2848239700905849103, 3.301821615535860399, 1.981129458308562352 ) ) ;
#84818 = CARTESIAN_POINT ( 'NONE',  ( 6.415309710857563630, -0.2865549832780675543, 2.244158528320794765 ) ) ;
#84819 = CIRCLE ( 'NONE', #212669, 0.08000000000000008493 ) ;
#84820 = CARTESIAN_POINT ( 'NONE',  ( 5.554000203453580475, 6.508696987897830688, -1.199719254218452047 ) ) ;
#84821 = CARTESIAN_POINT ( 'NONE',  ( -5.831415467653581430, 5.975941931783510519, 0.7216878364870257245 ) ) ;
#84822 = CARTESIAN_POINT ( 'NONE',  ( 4.176276986610152342, -1.057847390704643509, -1.770619276543743625 ) ) ;
#84823 = CARTESIAN_POINT ( 'NONE',  ( -4.283486466913726254, 7.084819080452935403, -1.199719254218452047 ) ) ;
#84824 = CIRCLE ( 'NONE', #109182, 0.07999999999999993228 ) ;
#84825 = CARTESIAN_POINT ( 'NONE',  ( -1.500000000000011324, 3.952083334016153415, 0.8660254037844403729 ) ) ;
#84826 = CARTESIAN_POINT ( 'NONE',  ( 1.364683531249986537, -0.6364583329919177856, 0.7879004041258500513 ) ) ;
#84827 = CARTESIAN_POINT ( 'NONE',  ( 6.292256349370360269, -1.861554482619768525, -0.1834065582871149958 ) ) ;
#84828 = CARTESIAN_POINT ( 'NONE',  ( 4.605968593894432139, -0.07825817699743177480, 1.732511586087708499 ) ) ;
#84829 = CARTESIAN_POINT ( 'NONE',  ( 4.194663043249587275, 1.400965740628885126, 1.032472458625796286 ) ) ;
#84830 = DIRECTION ( 'NONE',  ( 1.000000000000000000, 0.000000000000000000, 0.000000000000000000 ) ) ;
#84831 = CARTESIAN_POINT ( 'NONE',  ( 1.646416196899816997, 0.7239943723881783200, 2.175097950400638691 ) ) ;
#84832 = CARTESIAN_POINT ( 'NONE',  ( 0.6823417656249917140, 4.405208333674755394, 1.181850606188765695 ) ) ;
#84833 = CARTESIAN_POINT ( 'NONE',  ( 5.495677747024089399, -2.090933975967598446, 0.001106539467419370270 ) ) ;
#84834 = CARTESIAN_POINT ( 'NONE',  ( 0.3218710511002781383, 1.760991339961643920, 0.5373333866721883290 ) ) ;
#84835 = CARTESIAN_POINT ( 'NONE',  ( -1.607015867998808023, -0.9165151389911689872, 1.199999999999999734 ) ) ;
#84836 = CARTESIAN_POINT ( 'NONE',  ( 2.039685609654022347, -1.556907966322677472, 1.281362143053674130 ) ) ;
#84837 = CARTESIAN_POINT ( 'NONE',  ( 4.559605246071184226, 3.300000000000025135, 0.7750000000000135669 ) ) ;
#84838 = CARTESIAN_POINT ( 'NONE',  ( 9.192976028328162741, 13.26461296551308600, -9.042127702714923387 ) ) ;
#84839 = CARTESIAN_POINT ( 'NONE',  ( -7.015454420067433361, 10.27211502579893754, 1.199719254218453823 ) ) ;
#84840 =( BOUNDED_CURVE ( )  B_SPLINE_CURVE ( 2, ( #79492, #80561, #29690 ),
 .UNSPECIFIED., .F., .T. ) 
 B_SPLINE_CURVE_WITH_KNOTS ( ( 3, 3 ),
 ( 0.000000000000000000, 0.0008788941494526597391 ),
 .UNSPECIFIED. ) 
 CURVE ( )  GEOMETRIC_REPRESENTATION_ITEM ( )  RATIONAL_B_SPLINE_CURVE ( ( 1.000000000000000000, 0.9858700613453033057, 0.9747206155903836988 ) ) 
 REPRESENTATION_ITEM ( '' )  );
#84841 = CARTESIAN_POINT ( 'NONE',  ( 4.808338034340912337, 8.761478140039733020, 1.040834085586084257E-14 ) ) ;
#84842 = CARTESIAN_POINT ( 'NONE',  ( 2.789816089392273213, 2.012775272720100705, -0.6673941125509493810 ) ) ;
#84843 = CARTESIAN_POINT ( 'NONE',  ( -1.402160292154681736E-14, -0.1781249996585796136, 1.575800808251672791 ) ) ;
#84844 = CARTESIAN_POINT ( 'NONE',  ( 5.690036971771410101, -0.8169618954828453683, 1.632782195682795257 ) ) ;
#84845 = EDGE_LOOP ( 'NONE', ( #32660, #36462, #174532, #86200, #213211 ) ) ;
#84846 = CARTESIAN_POINT ( 'NONE',  ( -5.284646014276622950, 9.387447126623207794, -0.7998128361456362523 ) ) ;
#84847 = CARTESIAN_POINT ( 'NONE',  ( -0.001128590447031348198, 8.210952333604092601, -2.038660652713623733 ) ) ;
#84848 = CARTESIAN_POINT ( 'NONE',  ( 1.642778471875001811, -1.130208332855375808, 2.845375778867859751 ) ) ;
#84849 = CARTESIAN_POINT ( 'NONE',  ( -7.393273838153706201, 7.519907654134449615, 0.7998128361456341429 ) ) ;
#84850 = CARTESIAN_POINT ( 'NONE',  ( 3.357680014348028763, -1.532128950806666445, -1.316242992507418386 ) ) ;
#84851 = CARTESIAN_POINT ( 'NONE',  ( 6.387735258934439386, 1.517164627179751646, 1.602757196154185770 ) ) ;
#84852 = FACE_OUTER_BOUND ( 'NONE', #105406, .T. ) ;
#84853 = CARTESIAN_POINT ( 'NONE',  ( 3.660865129197692358, 1.469539745679597553, -1.141665872729610287 ) ) ;
#84854 = CARTESIAN_POINT ( 'NONE',  ( 8.594979316059474073, 12.11489407112305372, 1.199719254218450271 ) ) ;
#84855 = CARTESIAN_POINT ( 'NONE',  ( -9.671688505580934958, 4.446957226446405009, -7.030662469568692785 ) ) ;
#84856 = ORIENTED_EDGE ( 'NONE', *, *, #124486, .F. ) ;
#84857 = CARTESIAN_POINT ( 'NONE',  ( -3.415764635639130020, 6.072476943965863683, 1.199719254218462483 ) ) ;
#84858 = CARTESIAN_POINT ( 'NONE',  ( -6.659026002606323047, 10.92061410301605662, 0.000000000000000000 ) ) ;
#84859 = TOROIDAL_SURFACE ( 'NONE', #147182, 2.600000000000000089, 0.1000000000000000056 ) ;
#84861 = CARTESIAN_POINT ( 'NONE',  ( -5.120997767102647202, 6.698429628811411796, 1.435921996857256300 ) ) ;
#84860 = CARTESIAN_POINT ( 'NONE',  ( -7.937372586157736443, 8.224965870130965584, 0.7998128361456341429 ) ) ;
#84862 = CARTESIAN_POINT ( 'NONE',  ( 1.364683531249984538, -1.094791666325247936, -0.7879004041258309554 ) ) ;
#84863 = CARTESIAN_POINT ( 'NONE',  ( 1.493026163575939425, 1.669116110853157808, 0.4689669769783275100 ) ) ;
#84864 = CARTESIAN_POINT ( 'NONE',  ( 1.798380396644788659, 1.445777515557338688, 0.9684012028719732879 ) ) ;
#84866 = CARTESIAN_POINT ( 'NONE',  ( 7.565086526745395723, 10.80938946696957004, -1.082531754730543083 ) ) ;
#84865 = CARTESIAN_POINT ( 'NONE',  ( 6.586558022634583232, -2.261718397432868066, -0.4576183726279075548 ) ) ;
#84867 = CARTESIAN_POINT ( 'NONE',  ( -10.78237064342727791, 6.270194388237658956, -4.501389708959286473 ) ) ;
#84868 = CARTESIAN_POINT ( 'NONE',  ( 1.071639231386111391, 1.986785141929363618, -0.5470796107636519690 ) ) ;
#84869 = CARTESIAN_POINT ( 'NONE',  ( 0.5618747747782488755, 1.677749815653075460, -1.117659098820653174 ) ) ;
#84870 = CARTESIAN_POINT ( 'NONE',  ( 1.737500000000001155, -1.633333333333333748, 3.009438278150922130 ) ) ;
#84871 = CARTESIAN_POINT ( 'NONE',  ( -4.599959256786493533, 8.588645909551377855, 0.000000000000000000 ) ) ;
#84872 = CARTESIAN_POINT ( 'NONE',  ( 6.825078400183573812, 0.002648415797040087893, 1.855566311045192540 ) ) ;
#84874 = CARTESIAN_POINT ( 'NONE',  ( -5.804299160426229953, 8.825413882922319431, -1.082531754730549967 ) ) ;
#84873 = CARTESIAN_POINT ( 'NONE',  ( 4.869353489999923568, -1.618680692612521455, -1.018082601613921723 ) ) ;
#84875 = CARTESIAN_POINT ( 'NONE',  ( 5.883472226557855400, 2.040502603023553796, -0.8411249186189362348 ) ) ;
#84876 = CARTESIAN_POINT ( 'NONE',  ( 1.224999999999974998, 2.416666667349527842, 0.7072540797572656190 ) ) ;
#84877 = EDGE_CURVE ( 'NONE', #96508, #84297, #34893, .T. ) ;
#84878 = CARTESIAN_POINT ( 'NONE',  ( 0.000000000000000000, -6.583980363594976737, 0.000000000000000000 ) ) ;
#84879 = CARTESIAN_POINT ( 'NONE',  ( 5.207740400980577888, 5.248321020665011716, 0.000000000000000000 ) ) ;
#84880 = AXIS2_PLACEMENT_3D ( 'NONE', #17621, #12565, #62395 ) ;
#84881 = CARTESIAN_POINT ( 'NONE',  ( -7.095713291905736853, 9.371694488680407886, 1.599625672291269396 ) ) ;
#84882 = CARTESIAN_POINT ( 'NONE',  ( 6.393239817247728496, -0.1034752114322245314, -2.118097640427937911 ) ) ;
#84883 = CARTESIAN_POINT ( 'NONE',  ( 3.540313787445231508, 1.039887675495542618, -2.060077152250729071 ) ) ;
#84884 = CARTESIAN_POINT ( 'NONE',  ( 5.230891786122516152, -1.846674803186045821, -0.6626716404555529349 ) ) ;
#84885 = CARTESIAN_POINT ( 'NONE',  ( 0.9011314981347726683, -1.685442764318560771, 1.003610994683441948 ) ) ;
#84886 = DIRECTION ( 'NONE',  ( 1.000000000000000000, 0.000000000000000000, 0.000000000000000000 ) ) ;
#84887 = DIRECTION ( 'NONE',  ( 0.000000000000000000, 1.000000000000000000, 0.000000000000000000 ) ) ;
#84888 = EDGE_LOOP ( 'NONE', ( #12127, #44472, #155303, #142134, #16181 ) ) ;
#84889 = CARTESIAN_POINT ( 'NONE',  ( 0.4271636869729276698, -1.812546591343185298, 1.094284096637233583 ) ) ;
#84891 = CARTESIAN_POINT ( 'NONE',  ( -8.616370316684697883, 10.01118577667568132, -1.199719254218446718 ) ) ;
#84890 = CARTESIAN_POINT ( 'NONE',  ( -5.759516327706961647, 5.613857225279885732, -0.7998128361456221525 ) ) ;
#84892 = FILL_AREA_STYLE ('',( #38281 ) ) ;
#84893 = CARTESIAN_POINT ( 'NONE',  ( 2.835037514343414777, -2.076374246603398532, -0.6340929010987955694 ) ) ;
#84894 = CARTESIAN_POINT ( 'NONE',  ( -0.3866901564497973731, 3.102326550341738098, 2.027579305719746205 ) ) ;
#84896 = EDGE_CURVE ( 'NONE', #132409, #72572, #45279, .T. ) ;
#84895 = CARTESIAN_POINT ( 'NONE',  ( 0.7914572142167939361, -0.05789999323873443182, -2.119991495365561640 ) ) ;
#84897 = CARTESIAN_POINT ( 'NONE',  ( -1.500000000000011324, 3.202083334016150307, 0.8660254037844403729 ) ) ;
#84898 = CARTESIAN_POINT ( 'NONE',  ( 9.887974103068218668, 10.43039129653476493, 0.7998128361456462443 ) ) ;
#84899 = CARTESIAN_POINT ( 'NONE',  ( 11.92046840572485777, 13.65252124794270472, -1.382231356234943753 ) ) ;
#84900 = CARTESIAN_POINT ( 'NONE',  ( 6.493754380866193721, 6.839952184459461293, 0.5864284347954504817 ) ) ;
#84901 = CARTESIAN_POINT ( 'NONE',  ( 1.792332366127664223, -2.050593157767267805, -0.2048568651325937962 ) ) ;
#84903 = CARTESIAN_POINT ( 'NONE',  ( 8.131124540793322808, 14.25330072365142620, -8.765600733912146225 ) ) ;
#84902 = CARTESIAN_POINT ( 'NONE',  ( -10.01677656239806247, 10.58066083241955901, 0.7998128361456462443 ) ) ;
#84904 = CARTESIAN_POINT ( 'NONE',  ( 0.6823417656249882723, 2.176041667008084435, -1.181850606188749264 ) ) ;
#84905 = CARTESIAN_POINT ( 'NONE',  ( 0.07755575628183573877, -0.002876890934064984650, -2.188974970840869005 ) ) ;
#84906 = CARTESIAN_POINT ( 'NONE',  ( -4.957044826794427372, 6.512741263611735221, 2.499999999999999112 ) ) ;
#84907 = CARTESIAN_POINT ( 'NONE',  ( 4.565046243057500952, -1.533749416048999947, 1.141898535029245432 ) ) ;
#84908 = CARTESIAN_POINT ( 'NONE',  ( 11.78331023100045627, 9.799999999999982947, 1.799999999999999600 ) ) ;
#84909 = CARTESIAN_POINT ( 'NONE',  ( 1.054439146255849780, 2.259743442402757818, -0.1116689827955052033 ) ) ;
#84910 = CARTESIAN_POINT ( 'NONE',  ( -2.252626078164912560, 5.779814191167667481, 0.7998128361456341429 ) ) ;
#84911 = CARTESIAN_POINT ( 'NONE',  ( 1.476514701902143623, -1.279619142688562805, 1.282606640394849951 ) ) ;
#84912 = CARTESIAN_POINT ( 'NONE',  ( 0.3564614995229599681, -1.804831555932787657, -0.6427613734035338977 ) ) ;
#84913 = CARTESIAN_POINT ( 'NONE',  ( 1.539598694730393680, 1.913698299121506352, -0.7905179490511196061 ) ) ;
#84914 = CARTESIAN_POINT ( 'NONE',  ( -1.402160292154681736E-14, 0.1343750003414218575, 1.575800808251672791 ) ) ;
#84915 = CARTESIAN_POINT ( 'NONE',  ( 0.9714808946714141857, 1.900638238906343425, -0.5234924991099793035 ) ) ;
#84916 = CARTESIAN_POINT ( 'NONE',  ( 5.883413297016587329, 1.779079706761811153, -0.7395700111451685155 ) ) ;
#84918 = CARTESIAN_POINT ( 'NONE',  ( 6.477827756726281194, 6.756902019748111776, -0.2091553196570776485 ) ) ;
#84917 = CARTESIAN_POINT ( 'NONE',  ( 6.604147088760183415, -2.206502607372296421, 0.04933187264975073122 ) ) ;
#84919 = CARTESIAN_POINT ( 'NONE',  ( -1.402160292154681736E-14, 2.196875000341423689, -1.575800808251660134 ) ) ;
#84920 = CARTESIAN_POINT ( 'NONE',  ( 3.736832797123919025, -1.987151705994869344, -0.5527697292582544053 ) ) ;
#84921 =( BOUNDED_SURFACE ( )  B_SPLINE_SURFACE ( 1, 2, ( 
 ( #197955, #148168, #149217, #214170, #127741, #49584, #161214, #193698, #111461, #211002, #115708, #181698, #33328, #62625, #112519, #104756, #182773, #38677, #116776, #34391, #117854, #119993, #201143, #154567, #53860, #183846, #152425, #20270, #135126, #166538, #35458, #2937, #185970, #101536, #86354, #187045, #52781, #36524, #100463, #51731, #67929, #102611, #203279, #136188, #1869, #199005, #167605, #150303, #70074, #87429, #168666, #153497, #37603, #121078, #202206, #170805, #66860, #103684, #22396, #169733, #21322, #19203, #85282, #54926, #88505, #133005, #50650, #18126, #84215, #134074, #118920, #184900, #5067, #71142, #137259, #151368, #69009, #4004, #89580, #178022, #7214, #29640, #73288, #57062, #156708, #110944, #193190, #61062, #105849, #144492, #23472, #123226, #127221, #24539, #95726, #45903, #90647, #176951, #44838, #28567, #94654, #161778, #155629, #160698, #12292, #139391, #8298, #205424, #78372, #74383, #189191, #140484, #210500, #62135, #128295, #194257, #209416, #106937, #112021, #6143, #40828, #171876, #72213, #172960, #138320, #204336, #55994, #122145, #188113, #39744, #8736, #3642, #134775, #38315, #135825, #37247, #136894, #199727, #151014, #53493, #24980, #119630, #200783, #69721, #20964, #87061, #201849, #153133, #185614, #190673, #19913, #52435, #104391, #206931, #36165, #58560, #118561, #68652, #18840, #102244, #2582, #184545, #103317, #26044, #168317, #35096, #186686, #169379, #75874, #85998, #51373, #183487, #4706, #124714, #42334, #101167, #108449, #70780, #152072, #202921, #54565, #174468, #140917, #120713, #117496, #170438, #91083, #157143, #92157, #74817, #158210, #9799, #167254, #84926, #80131, #126847, #94287, #125778, #191740, #176581, #47668, #212252, #141981, #128975, #110579, #78003, #76926, #159252, #27114, #178720, #60683, #28192, #10853, #146235, #62814, #161406, #15116, #207995, #45529, #143052, #177656, #160327, #12990, #111644, #109517, #209047, #192804, #63886, #59622, #43395, #79065, #113779, #144127, #30335, #14044, #175524, #29264, #44463, #210120, #61761, #127929, #193881, #95356, #145183, #130041, #96420, #162471, #196034, #97475, #211189, #194954, #179781, #46590, #31401, #163531, #165654, #32455, #34575, #132128, #148348, #2046, #197080, #116962, #19383, #134253, #36704, #67050, #168847, #150487, #131091, #119098, #102791, #164586, #100647, #985, #49768, #84399, #133187, #185080, #48717, #52960, #114831, #180830, #198137, #200260, #199187, #81205, #68117, #115894, #166724, #18316, #149403, #98525, #181879, #17241, #51911, #33516, #118034, #201321, #50835, #182960, #16172, #65978, #82256, #184020, #3117, #35637, #214348, #213316, #99588, #83316, #101716, #167787, #85462, #151548, #69187, #135308, #147284, #64940, #108192, #155812, #74560, #73476, #205603, #203453, #55108, #156886, #140660, #86533, #206675, #70255, #37787, #103861, #6327, #72400, #173140, #107117, #89766, #20450, #24721, #169910, #87607, #58306, #5247, #190421, #71322, #187226, #138500, #7396, #23655, #106039, #21499, #90823, #153677, #38855, #172062, #204523, #152599, #124462, #56172, #139577, #57241, #123401, #189365, #4184, #137437, #41007, #8473, #104939, #122334, #170979, #136369, #188291, #22578, #39931, #202388, #54040, #120177, #186153, #154744, #88684, #209862, #11673, #111391, #174217, #125525, #27937, #210934, #94032, #175273, #192550, #61500, #127666, #176330, #193628, #160070, #162215, #208800, #26859, #12730, #178464, #10603, #30074, #92963, #43152, #207742, #76679, #191484, #109265, #77748, #63636, #159009, #9550, #161143, #143869, #47410, #142794, #25791, #157957, #45270, #96165, #13802, #75625, #79874, #44205, #60429, #177394, #126589, #145984, #112451, #29008, #91901, #95094, #110325, #78804, #129791, #144927, #62559, #128723, #194695, #46337, #195771, #141735, #59368, #80948, #64692, #148095, #135055, #114587, #98275, #117784, #131874, #132926, #198931, #116699, #152351, #7142, #103604, #21245, #53785, #40751, #171800, #138250, #140405, #52709, #22314, #169661, #88426, #71066, #55915, #122074, #87352, #137183, #73213, #106858, #102530, #168592, #8225, #74309, #118841, #144678 ),
 ( #206424, #176082, #26609, #178215, #158756, #92709, #46090, #10351, #142536, #147845, #166208, #65486, #212816, #198689, #197634, #165147, #49279, #33016, #116452, #182446, #149975, #1545, #67607, #183519, #101200, #18873, #148643, #165950, #182182, #2347, #103085, #35937, #116195, #98832, #99888, #50074, #184313, #201615, #68423, #53264, #168085, #20736, #102017, #4474, #54339, #19685, #86831, #85763, #151843, #149706, #1286, #169142, #152895, #32750, #70545, #16476, #198428, #33809, #167023, #18618, #119395, #185384, #3420, #181129, #37003, #17534, #83623, #136664, #67344, #202689, #133489, #199492, #84697, #69486, #135594, #52202, #51137, #164882, #117259, #183258, #118328, #150784, #82556, #209, #134551, #66280, #132427, #34862, #100936, #200554, #153972, #204816, #138796, #137733, #39153, #5539, #56467, #105234, #203752, #171275, #122629, #155036, #188591, #40223, #22868, #187522, #88984, #6622, #55396, #21790, #72701, #71620, #121551, #106334, #38087, #172356, #23945, #90050, #156109, #120477, #186450, #104158, #87899, #170206, #43694, #171528, #107672, #74041, #56721, #91378, #140131, #126070, #203998, #59913, #137981, #55647, #139052, #207227, #206157, #175820, #75106, #205079, #173701, #192031, #109811, #23121, #25276, #57785, #122889, #157438, #123945, #88154, #121803, #154222, #187770, #39402, #188848, #58851, #189914, #5794, #125007, #40484, #9032, #41559, #156365, #105496, #106588, #24192, #190964, #172616, #42630, #208282, #108739, #26341, #89238, #72950, #155289, #92454, #10092, #158493, #6872, #71871, #76166, #142271, #30638, #47970, #129286, #114087, #14349, #81504, #96722, #65227, #115134, #162771, #147583, #80439, #212557, #210422, #62064, #163835, #213601, #93511, #131378, #77226, #44762, #110870, #13298, #79371, #180077, #31700, #146538, #27413, #97775, #176875, #94578, #197374, #12222, #49015, #78295, #194181, #145490, #64196, #130337, #113011, #28487, #15414, #160621, #128219, #179020, #211485, #159552, #11149, #63122, #196326, #143345, #209340, #60988, #127141, #144420, #193113, #45826, #111947, #195262, #177949, #29563, #46896, #95655, #161706, #91063, #41247, #157123, #74797, #89995, #23889, #139817, #73720, #106279, #22813, #57479, #204760, #72646, #107355, #187467, #205846, #206909, #24961, #92135, #156046, #158190, #173377, #39097, #40165, #7635, #8712, #140898, #58539, #124694, #123638, #189601, #190652, #42313, #172300, #88927, #108429, #56412, #138742, #174449, #105182, #26025, #203697, #55343, #121495, #171218, #154981, #6566, #122573, #188535, #5487, #133432, #69434, #184259, #18563, #53210, #35885, #87846, #165898, #21737, #99832, #83568, #100885, #103031, #101961, #137676, #36951, #166972, #135539, #3364, #118274, #149650, #84639, #200503, #169086, #150730, #201564, #170151, #168027, #19631, #1231, #34810, #51082, #85702, #186394, #119341, #199439, #182126, #183204, #117207, #185328, #70492, #151790, #136608, #20685, #104101, #86776, #153917, #50013, #152847, #71568, #4422, #202633, #2290, #68367, #38031, #116137, #33755, #67293, #134500, #52146, #54283, #120420, #10820, #111610, #45493, #28156, #173363, #177621, #108413, #26012, #211153, #158175, #128939, #9767, #125743, #76894, #160291, #176545, #44427, #190639, #29230, #174436, #59586, #110544, #159220, #194917, #79031, #143018, #11894, #94252, #77968, #144090, #62777, #92123, #210086, #61725, #141948, #209013, #75841, #127893, #60649, #207960, #193844, #126812, #46555, #74783, #145147, #8699, #140882, #191704, #95322, #93187, #24945, #161371, #43363, #12953, #192768, #27080, #58526, #109485, #175493, #91049, #157110, #206895, #124681, #42299, #82224, #80097, #97442, #113744, #148315, #34543, #181846, #47633, #30298, #31366, #195999, #115861, #133153, #214314, #199155, #99555, #166689, #33482, #150454, #200228, #165620, #18280, #17208, #83284, #81171, #147251, #100613, #84363, #178685, #2015, #162435, #130008, #179748, #98490, #164553, #50800, #116927, #149369, #112675, #182927, #163498, #15081, #68084, #213283, #134219, #64909, #131058, #16139, #951, #67017, #198104, #197046, #96383, #48683, #114799, #49733, #65946 ) ),
 .UNSPECIFIED., .F., .F., .T. ) 
 B_SPLINE_SURFACE_WITH_KNOTS ( ( 2, 2 ),
 ( 3, 2, 2, 2, 2, 2, 2, 2, 2, 2, 2, 2, 2, 2, 2, 2, 2, 2, 2, 2, 2, 2, 2, 2, 2, 2, 2, 2, 2, 2, 2, 2, 2, 2, 2, 2, 2, 2, 2, 2, 2, 2, 2, 2, 2, 2, 2, 2, 2, 2, 2, 2, 2, 2, 2, 2, 2, 2, 2, 2, 2, 2, 2, 2, 2, 2, 2, 2, 2, 2, 2, 2, 2, 2, 2, 2, 2, 2, 2, 2, 2, 2, 2, 2, 2, 2, 2, 2, 2, 2, 2, 2, 2, 2, 2, 2, 2, 2, 2, 2, 2, 2, 2, 2, 2, 2, 2, 2, 2, 2, 2, 2, 2, 2, 2, 2, 2, 2, 2, 2, 2, 2, 2, 2, 2, 2, 2, 2, 2, 2, 2, 2, 2, 2, 2, 2, 2, 2, 2, 2, 2, 2, 2, 2, 2, 2, 2, 2, 2, 2, 2, 2, 2, 2, 2, 2, 2, 2, 2, 2, 2, 2, 2, 2, 2, 2, 2, 2, 2, 2, 2, 2, 2, 2, 2, 2, 2, 2, 2, 2, 2, 2, 2, 2, 2, 2, 2, 2, 2, 2, 2, 2, 2, 2, 2, 2, 2, 2, 2, 2, 2, 2, 2, 2, 2, 2, 2, 2, 2, 2, 2, 2, 2, 2, 2, 2, 2, 2, 2, 2, 2, 2, 2, 2, 2, 2, 2, 2, 2, 2, 2, 2, 2, 2, 2, 2, 2, 2, 2, 2, 3 ),
 ( 0.000000000000000000, 1.000000000000000000 ),
 ( 0.000000000000000000, 0.004166666666666666609, 0.008333333333333333218, 0.01250000000000000069, 0.01666666666666666644, 0.02083333333333333218, 0.02500000000000000139, 0.02916666666666666713, 0.03333333333333333287, 0.03749999999999999861, 0.04166666666666666435, 0.04583333333333333010, 0.05000000000000000278, 0.05416666666666666852, 0.05833333333333333426, 0.06250000000000000000, 0.06666666666666666574, 0.07083333333333333148, 0.07499999999999999722, 0.07916666666666666297, 0.08333333333333332871, 0.08749999999999999445, 0.09166666666666666019, 0.09583333333333333981, 0.1000000000000000056, 0.1041666666666666713, 0.1083333333333333370, 0.1125000000000000028, 0.1166666666666666685, 0.1208333333333333343, 0.1250000000000000000, 0.1291666666666666796, 0.1333333333333333315, 0.1375000000000000111, 0.1416666666666666630, 0.1458333333333333426, 0.1499999999999999944, 0.1541666666666666741, 0.1583333333333333259, 0.1625000000000000056, 0.1666666666666666574, 0.1708333333333333370, 0.1749999999999999889, 0.1791666666666666685, 0.1833333333333333204, 0.1875000000000000000, 0.1916666666666666796, 0.1958333333333333315, 0.2000000000000000111, 0.2041666666666666630, 0.2083333333333333426, 0.2124999999999999944, 0.2166666666666666741, 0.2208333333333333259, 0.2250000000000000056, 0.2291666666666666574, 0.2333333333333333370, 0.2374999999999999889, 0.2416666666666666685, 0.2458333333333333204, 0.2500000000000000000, 0.2541666666666666519, 0.2583333333333333592, 0.2625000000000000111, 0.2666666666666666630, 0.2708333333333333148, 0.2750000000000000222, 0.2791666666666666741, 0.2833333333333333259, 0.2874999999999999778, 0.2916666666666666852, 0.2958333333333333370, 0.2999999999999999889, 0.3041666666666666408, 0.3083333333333333481, 0.3125000000000000000, 0.3166666666666666519, 0.3208333333333333592, 0.3250000000000000111, 0.3291666666666666630, 0.3333333333333333148, 0.3375000000000000222, 0.3416666666666666741, 0.3458333333333333259, 0.3499999999999999778, 0.3541666666666666852, 0.3583333333333333370, 0.3624999999999999889, 0.3666666666666666408, 0.3708333333333333481, 0.3750000000000000000, 0.3791666666666666519, 0.3833333333333333592, 0.3875000000000000111, 0.3916666666666666630, 0.3958333333333333148, 0.4000000000000000222, 0.4041666666666666741, 0.4083333333333333259, 0.4124999999999999778, 0.4166666666666666852, 0.4208333333333333370, 0.4249999999999999889, 0.4291666666666666408, 0.4333333333333333481, 0.4375000000000000000, 0.4416666666666666519, 0.4458333333333333592, 0.4500000000000000111, 0.4541666666666666630, 0.4583333333333333148, 0.4625000000000000222, 0.4666666666666666741, 0.4708333333333333259, 0.4749999999999999778, 0.4791666666666666852, 0.4833333333333333370, 0.4874999999999999889, 0.4916666666666666408, 0.4958333333333333481, 0.5000000000000000000, 0.5041666666666666519, 0.5083333333333333037, 0.5124999999999999556, 0.5166666666666667185, 0.5208333333333333703, 0.5250000000000000222, 0.5291666666666666741, 0.5333333333333333259, 0.5374999999999999778, 0.5416666666666666297, 0.5458333333333332815, 0.5500000000000000444, 0.5541666666666666963, 0.5583333333333333481, 0.5625000000000000000, 0.5666666666666666519, 0.5708333333333333037, 0.5749999999999999556, 0.5791666666666667185, 0.5833333333333333703, 0.5875000000000000222, 0.5916666666666666741, 0.5958333333333333259, 0.5999999999999999778, 0.6041666666666666297, 0.6083333333333332815, 0.6125000000000000444, 0.6166666666666666963, 0.6208333333333333481, 0.6250000000000000000, 0.6291666666666666519, 0.6333333333333333037, 0.6374999999999999556, 0.6416666666666667185, 0.6458333333333333703, 0.6500000000000000222, 0.6541666666666666741, 0.6583333333333333259, 0.6624999999999999778, 0.6666666666666666297, 0.6708333333333332815, 0.6750000000000000444, 0.6791666666666666963, 0.6833333333333333481, 0.6875000000000000000, 0.6916666666666666519, 0.6958333333333333037, 0.6999999999999999556, 0.7041666666666667185, 0.7083333333333333703, 0.7125000000000000222, 0.7166666666666666741, 0.7208333333333333259, 0.7249999999999999778, 0.7291666666666666297, 0.7333333333333332815, 0.7375000000000000444, 0.7416666666666666963, 0.7458333333333333481, 0.7500000000000000000, 0.7541666666666666519, 0.7583333333333333037, 0.7624999999999999556, 0.7666666666666667185, 0.7708333333333333703, 0.7750000000000000222, 0.7791666666666666741, 0.7833333333333333259, 0.7874999999999999778, 0.7916666666666666297, 0.7958333333333332815, 0.8000000000000000444, 0.8041666666666666963, 0.8083333333333333481, 0.8125000000000000000, 0.8166666666666666519, 0.8208333333333333037, 0.8249999999999999556, 0.8291666666666667185, 0.8333333333333333703, 0.8375000000000000222, 0.8416666666666666741, 0.8458333333333333259, 0.8499999999999999778, 0.8541666666666666297, 0.8583333333333332815, 0.8625000000000000444, 0.8666666666666666963, 0.8708333333333333481, 0.8750000000000000000, 0.8791666666666666519, 0.8833333333333333037, 0.8874999999999999556, 0.8916666666666667185, 0.8958333333333333703, 0.9000000000000000222, 0.9041666666666666741, 0.9083333333333333259, 0.9124999999999999778, 0.9166666666666666297, 0.9208333333333332815, 0.9250000000000000444, 0.9291666666666666963, 0.9333333333333333481, 0.9375000000000000000, 0.9416666666666666519, 0.9458333333333333037, 0.9499999999999999556, 0.9541666666666667185, 0.9583333333333333703, 0.9625000000000000222, 0.9666666666666666741, 0.9708333333333333259, 0.9749999999999999778, 0.9791666666666666297, 0.9833333333333332815, 0.9875000000000000444, 0.9916666666666666963, 0.9958333333333333481, 1.000000000000000000 ),
 .UNSPECIFIED. ) 
 GEOMETRIC_REPRESENTATION_ITEM ( )  RATIONAL_B_SPLINE_SURFACE ( (
 ( 1.000000000000000000, 0.8660254037844387076, 1.000000000000000000, 0.8660254037844387076, 1.000000000000000000, 0.8660254037844387076, 1.000000000000000000, 0.8660254037844387076, 1.000000000000000000, 0.8660254037844387076, 1.000000000000000000, 0.8660254037844387076, 1.000000000000000000, 0.8660254037844387076, 1.000000000000000000, 0.8660254037844387076, 1.000000000000000000, 0.8660254037844387076, 1.000000000000000000, 0.8660254037844387076, 1.000000000000000000, 0.8660254037844387076, 1.000000000000000000, 0.8660254037844387076, 1.000000000000000000, 0.8660254037844387076, 1.000000000000000000, 0.8660254037844387076, 1.000000000000000000, 0.8660254037844387076, 1.000000000000000000, 0.8660254037844387076, 1.000000000000000000, 0.8660254037844387076, 1.000000000000000000, 0.8660254037844387076, 1.000000000000000000, 0.8660254037844387076, 1.000000000000000000, 0.8660254037844387076, 1.000000000000000000, 0.8660254037844387076, 1.000000000000000000, 0.8660254037844387076, 1.000000000000000000, 0.8660254037844387076, 1.000000000000000000, 0.8660254037844387076, 1.000000000000000000, 0.8660254037844387076, 1.000000000000000000, 0.8660254037844387076, 1.000000000000000000, 0.8660254037844387076, 1.000000000000000000, 0.8660254037844387076, 1.000000000000000000, 0.8660254037844387076, 1.000000000000000000, 0.8660254037844387076, 1.000000000000000000, 0.8660254037844387076, 1.000000000000000000, 0.8660254037844387076, 1.000000000000000000, 0.8660254037844387076, 1.000000000000000000, 0.8660254037844387076, 1.000000000000000000, 0.8660254037844387076, 1.000000000000000000, 0.8660254037844387076, 1.000000000000000000, 0.8660254037844387076, 1.000000000000000000, 0.8660254037844387076, 1.000000000000000000, 0.8660254037844387076, 1.000000000000000000, 0.8660254037844387076, 1.000000000000000000, 0.8660254037844387076, 1.000000000000000000, 0.8660254037844387076, 1.000000000000000000, 0.8660254037844387076, 1.000000000000000000, 0.8660254037844387076, 1.000000000000000000, 0.8660254037844387076, 1.000000000000000000, 0.8660254037844387076, 1.000000000000000000, 0.8660254037844387076, 1.000000000000000000, 0.8660254037844387076, 1.000000000000000000, 0.8660254037844387076, 1.000000000000000000, 0.8660254037844387076, 1.000000000000000000, 0.8660254037844387076, 1.000000000000000000, 0.8660254037844387076, 1.000000000000000000, 0.8660254037844387076, 1.000000000000000000, 0.8660254037844387076, 1.000000000000000000, 0.8660254037844387076, 1.000000000000000000, 0.8660254037844387076, 1.000000000000000000, 0.8660254037844387076, 1.000000000000000000, 0.8660254037844387076, 1.000000000000000000, 0.8660254037844387076, 1.000000000000000000, 0.8660254037844387076, 1.000000000000000000, 0.8660254037844387076, 1.000000000000000000, 0.8660254037844387076, 1.000000000000000000, 0.8660254037844387076, 1.000000000000000000, 0.8660254037844387076, 1.000000000000000000, 0.8660254037844387076, 1.000000000000000000, 0.8660254037844387076, 1.000000000000000000, 0.8660254037844387076, 1.000000000000000000, 0.8660254037844387076, 1.000000000000000000, 0.8660254037844387076, 1.000000000000000000, 0.8660254037844387076, 1.000000000000000000, 0.8660254037844387076, 1.000000000000000000, 0.8660254037844387076, 1.000000000000000000, 0.8660254037844387076, 1.000000000000000000, 0.8660254037844387076, 1.000000000000000000, 0.8660254037844387076, 1.000000000000000000, 0.8660254037844387076, 1.000000000000000000, 0.8660254037844387076, 1.000000000000000000, 0.8660254037844387076, 1.000000000000000000, 0.8660254037844387076, 1.000000000000000000, 0.8660254037844387076, 1.000000000000000000, 0.8660254037844387076, 1.000000000000000000, 0.8660254037844387076, 1.000000000000000000, 0.8660254037844387076, 1.000000000000000000, 0.8660254037844387076, 1.000000000000000000, 0.8660254037844387076, 1.000000000000000000, 0.8660254037844387076, 1.000000000000000000, 0.8660254037844387076, 1.000000000000000000, 0.8660254037844387076, 1.000000000000000000, 0.8660254037844387076, 1.000000000000000000, 0.8660254037844387076, 1.000000000000000000, 0.8660254037844387076, 1.000000000000000000, 0.8660254037844387076, 1.000000000000000000, 0.8660254037844387076, 1.000000000000000000, 0.8660254037844387076, 1.000000000000000000, 0.8660254037844387076, 1.000000000000000000, 0.8660254037844387076, 1.000000000000000000, 0.8660254037844387076, 1.000000000000000000, 0.8660254037844387076, 1.000000000000000000, 0.8660254037844387076, 1.000000000000000000, 0.8660254037844387076, 1.000000000000000000, 0.8660254037844387076, 1.000000000000000000, 0.8660254037844387076, 1.000000000000000000, 0.8660254037844387076, 1.000000000000000000, 0.8660254037844387076, 1.000000000000000000, 0.8660254037844387076, 1.000000000000000000, 0.8660254037844387076, 1.000000000000000000, 0.8660254037844387076, 1.000000000000000000, 0.8660254037844387076, 1.000000000000000000, 0.8660254037844387076, 1.000000000000000000, 0.8660254037844387076, 1.000000000000000000, 0.8660254037844387076, 1.000000000000000000, 0.8660254037844387076, 1.000000000000000000, 0.8660254037844387076, 1.000000000000000000, 0.8660254037844387076, 1.000000000000000000, 0.8660254037844387076, 1.000000000000000000, 0.8660254037844387076, 1.000000000000000000, 0.8660254037844387076, 1.000000000000000000, 0.8660254037844387076, 1.000000000000000000, 0.8660254037844387076, 1.000000000000000000, 0.8660254037844387076, 1.000000000000000000, 0.8660254037844387076, 1.000000000000000000, 0.8660254037844387076, 1.000000000000000000, 0.8660254037844387076, 1.000000000000000000, 0.8660254037844387076, 1.000000000000000000, 0.8660254037844387076, 1.000000000000000000, 0.8660254037844387076, 1.000000000000000000, 0.8660254037844387076, 1.000000000000000000, 0.8660254037844387076, 1.000000000000000000, 0.8660254037844387076, 1.000000000000000000, 0.8660254037844387076, 1.000000000000000000, 0.8660254037844387076, 1.000000000000000000, 0.8660254037844387076, 1.000000000000000000, 0.8660254037844387076, 1.000000000000000000, 0.8660254037844387076, 1.000000000000000000, 0.8660254037844387076, 1.000000000000000000, 0.8660254037844387076, 1.000000000000000000, 0.8660254037844387076, 1.000000000000000000, 0.8660254037844387076, 1.000000000000000000, 0.8660254037844387076, 1.000000000000000000, 0.8660254037844387076, 1.000000000000000000, 0.8660254037844387076, 1.000000000000000000, 0.8660254037844387076, 1.000000000000000000, 0.8660254037844387076, 1.000000000000000000, 0.8660254037844387076, 1.000000000000000000, 0.8660254037844387076, 1.000000000000000000, 0.8660254037844387076, 1.000000000000000000, 0.8660254037844387076, 1.000000000000000000, 0.8660254037844387076, 1.000000000000000000, 0.8660254037844387076, 1.000000000000000000, 0.8660254037844387076, 1.000000000000000000, 0.8660254037844387076, 1.000000000000000000, 0.8660254037844387076, 1.000000000000000000, 0.8660254037844387076, 1.000000000000000000, 0.8660254037844387076, 1.000000000000000000, 0.8660254037844387076, 1.000000000000000000, 0.8660254037844387076, 1.000000000000000000, 0.8660254037844387076, 1.000000000000000000, 0.8660254037844387076, 1.000000000000000000, 0.8660254037844387076, 1.000000000000000000, 0.8660254037844387076, 1.000000000000000000, 0.8660254037844387076, 1.000000000000000000, 0.8660254037844387076, 1.000000000000000000, 0.8660254037844387076, 1.000000000000000000, 0.8660254037844387076, 1.000000000000000000, 0.8660254037844387076, 1.000000000000000000, 0.8660254037844387076, 1.000000000000000000, 0.8660254037844387076, 1.000000000000000000, 0.8660254037844387076, 1.000000000000000000, 0.8660254037844387076, 1.000000000000000000, 0.8660254037844387076, 1.000000000000000000, 0.8660254037844387076, 1.000000000000000000, 0.8660254037844387076, 1.000000000000000000, 0.8660254037844387076, 1.000000000000000000, 0.8660254037844387076, 1.000000000000000000, 0.8660254037844387076, 1.000000000000000000, 0.8660254037844387076, 1.000000000000000000, 0.8660254037844387076, 1.000000000000000000, 0.8660254037844387076, 1.000000000000000000, 0.8660254037844387076, 1.000000000000000000, 0.8660254037844387076, 1.000000000000000000, 0.8660254037844387076, 1.000000000000000000, 0.8660254037844387076, 1.000000000000000000, 0.8660254037844387076, 1.000000000000000000, 0.8660254037844387076, 1.000000000000000000, 0.8660254037844387076, 1.000000000000000000, 0.8660254037844387076, 1.000000000000000000, 0.8660254037844387076, 1.000000000000000000, 0.8660254037844387076, 1.000000000000000000, 0.8660254037844387076, 1.000000000000000000, 0.8660254037844387076, 1.000000000000000000, 0.8660254037844387076, 1.000000000000000000, 0.8660254037844387076, 1.000000000000000000, 0.8660254037844387076, 1.000000000000000000, 0.8660254037844387076, 1.000000000000000000, 0.8660254037844387076, 1.000000000000000000, 0.8660254037844387076, 1.000000000000000000, 0.8660254037844387076, 1.000000000000000000, 0.8660254037844387076, 1.000000000000000000, 0.8660254037844387076, 1.000000000000000000, 0.8660254037844387076, 1.000000000000000000, 0.8660254037844387076, 1.000000000000000000, 0.8660254037844387076, 1.000000000000000000, 0.8660254037844387076, 1.000000000000000000, 0.8660254037844387076, 1.000000000000000000, 0.8660254037844387076, 1.000000000000000000, 0.8660254037844387076, 1.000000000000000000, 0.8660254037844387076, 1.000000000000000000, 0.8660254037844387076, 1.000000000000000000, 0.8660254037844387076, 1.000000000000000000, 0.8660254037844387076, 1.000000000000000000, 0.8660254037844387076, 1.000000000000000000, 0.8660254037844387076, 1.000000000000000000, 0.8660254037844387076, 1.000000000000000000, 0.8660254037844387076, 1.000000000000000000, 0.8660254037844387076, 1.000000000000000000, 0.8660254037844387076, 1.000000000000000000, 0.8660254037844387076, 1.000000000000000000, 0.8660254037844387076, 1.000000000000000000, 0.8660254037844387076, 1.000000000000000000, 0.8660254037844387076, 1.000000000000000000, 0.8660254037844387076, 1.000000000000000000, 0.8660254037844387076, 1.000000000000000000, 0.8660254037844387076, 1.000000000000000000, 0.8660254037844387076, 1.000000000000000000, 0.8660254037844387076, 1.000000000000000000, 0.8660254037844387076, 1.000000000000000000, 0.8660254037844387076, 1.000000000000000000, 0.8660254037844387076, 1.000000000000000000, 0.8660254037844387076, 1.000000000000000000, 0.8660254037844387076, 1.000000000000000000, 0.8660254037844387076, 1.000000000000000000, 0.8660254037844387076, 1.000000000000000000, 0.8660254037844387076, 1.000000000000000000, 0.8660254037844387076, 1.000000000000000000, 0.8660254037844387076, 1.000000000000000000, 0.8660254037844387076, 1.000000000000000000, 0.8660254037844387076, 1.000000000000000000, 0.8660254037844387076, 1.000000000000000000, 0.8660254037844387076, 1.000000000000000000, 0.8660254037844387076, 1.000000000000000000),
 ( 1.000000000000000000, 0.8660254037844387076, 1.000000000000000000, 0.8660254037844387076, 1.000000000000000000, 0.8660254037844387076, 1.000000000000000000, 0.8660254037844387076, 1.000000000000000000, 0.8660254037844387076, 1.000000000000000000, 0.8660254037844387076, 1.000000000000000000, 0.8660254037844387076, 1.000000000000000000, 0.8660254037844387076, 1.000000000000000000, 0.8660254037844387076, 1.000000000000000000, 0.8660254037844387076, 1.000000000000000000, 0.8660254037844387076, 1.000000000000000000, 0.8660254037844387076, 1.000000000000000000, 0.8660254037844387076, 1.000000000000000000, 0.8660254037844387076, 1.000000000000000000, 0.8660254037844387076, 1.000000000000000000, 0.8660254037844387076, 1.000000000000000000, 0.8660254037844387076, 1.000000000000000000, 0.8660254037844387076, 1.000000000000000000, 0.8660254037844387076, 1.000000000000000000, 0.8660254037844387076, 1.000000000000000000, 0.8660254037844387076, 1.000000000000000000, 0.8660254037844387076, 1.000000000000000000, 0.8660254037844387076, 1.000000000000000000, 0.8660254037844387076, 1.000000000000000000, 0.8660254037844387076, 1.000000000000000000, 0.8660254037844387076, 1.000000000000000000, 0.8660254037844387076, 1.000000000000000000, 0.8660254037844387076, 1.000000000000000000, 0.8660254037844387076, 1.000000000000000000, 0.8660254037844387076, 1.000000000000000000, 0.8660254037844387076, 1.000000000000000000, 0.8660254037844387076, 1.000000000000000000, 0.8660254037844387076, 1.000000000000000000, 0.8660254037844387076, 1.000000000000000000, 0.8660254037844387076, 1.000000000000000000, 0.8660254037844387076, 1.000000000000000000, 0.8660254037844387076, 1.000000000000000000, 0.8660254037844387076, 1.000000000000000000, 0.8660254037844387076, 1.000000000000000000, 0.8660254037844387076, 1.000000000000000000, 0.8660254037844387076, 1.000000000000000000, 0.8660254037844387076, 1.000000000000000000, 0.8660254037844387076, 1.000000000000000000, 0.8660254037844387076, 1.000000000000000000, 0.8660254037844387076, 1.000000000000000000, 0.8660254037844387076, 1.000000000000000000, 0.8660254037844387076, 1.000000000000000000, 0.8660254037844387076, 1.000000000000000000, 0.8660254037844387076, 1.000000000000000000, 0.8660254037844387076, 1.000000000000000000, 0.8660254037844387076, 1.000000000000000000, 0.8660254037844387076, 1.000000000000000000, 0.8660254037844387076, 1.000000000000000000, 0.8660254037844387076, 1.000000000000000000, 0.8660254037844387076, 1.000000000000000000, 0.8660254037844387076, 1.000000000000000000, 0.8660254037844387076, 1.000000000000000000, 0.8660254037844387076, 1.000000000000000000, 0.8660254037844387076, 1.000000000000000000, 0.8660254037844387076, 1.000000000000000000, 0.8660254037844387076, 1.000000000000000000, 0.8660254037844387076, 1.000000000000000000, 0.8660254037844387076, 1.000000000000000000, 0.8660254037844387076, 1.000000000000000000, 0.8660254037844387076, 1.000000000000000000, 0.8660254037844387076, 1.000000000000000000, 0.8660254037844387076, 1.000000000000000000, 0.8660254037844387076, 1.000000000000000000, 0.8660254037844387076, 1.000000000000000000, 0.8660254037844387076, 1.000000000000000000, 0.8660254037844387076, 1.000000000000000000, 0.8660254037844387076, 1.000000000000000000, 0.8660254037844387076, 1.000000000000000000, 0.8660254037844387076, 1.000000000000000000, 0.8660254037844387076, 1.000000000000000000, 0.8660254037844387076, 1.000000000000000000, 0.8660254037844387076, 1.000000000000000000, 0.8660254037844387076, 1.000000000000000000, 0.8660254037844387076, 1.000000000000000000, 0.8660254037844387076, 1.000000000000000000, 0.8660254037844387076, 1.000000000000000000, 0.8660254037844387076, 1.000000000000000000, 0.8660254037844387076, 1.000000000000000000, 0.8660254037844387076, 1.000000000000000000, 0.8660254037844387076, 1.000000000000000000, 0.8660254037844387076, 1.000000000000000000, 0.8660254037844387076, 1.000000000000000000, 0.8660254037844387076, 1.000000000000000000, 0.8660254037844387076, 1.000000000000000000, 0.8660254037844387076, 1.000000000000000000, 0.8660254037844387076, 1.000000000000000000, 0.8660254037844387076, 1.000000000000000000, 0.8660254037844387076, 1.000000000000000000, 0.8660254037844387076, 1.000000000000000000, 0.8660254037844387076, 1.000000000000000000, 0.8660254037844387076, 1.000000000000000000, 0.8660254037844387076, 1.000000000000000000, 0.8660254037844387076, 1.000000000000000000, 0.8660254037844387076, 1.000000000000000000, 0.8660254037844387076, 1.000000000000000000, 0.8660254037844387076, 1.000000000000000000, 0.8660254037844387076, 1.000000000000000000, 0.8660254037844387076, 1.000000000000000000, 0.8660254037844387076, 1.000000000000000000, 0.8660254037844387076, 1.000000000000000000, 0.8660254037844387076, 1.000000000000000000, 0.8660254037844387076, 1.000000000000000000, 0.8660254037844387076, 1.000000000000000000, 0.8660254037844387076, 1.000000000000000000, 0.8660254037844387076, 1.000000000000000000, 0.8660254037844387076, 1.000000000000000000, 0.8660254037844387076, 1.000000000000000000, 0.8660254037844387076, 1.000000000000000000, 0.8660254037844387076, 1.000000000000000000, 0.8660254037844387076, 1.000000000000000000, 0.8660254037844387076, 1.000000000000000000, 0.8660254037844387076, 1.000000000000000000, 0.8660254037844387076, 1.000000000000000000, 0.8660254037844387076, 1.000000000000000000, 0.8660254037844387076, 1.000000000000000000, 0.8660254037844387076, 1.000000000000000000, 0.8660254037844387076, 1.000000000000000000, 0.8660254037844387076, 1.000000000000000000, 0.8660254037844387076, 1.000000000000000000, 0.8660254037844387076, 1.000000000000000000, 0.8660254037844387076, 1.000000000000000000, 0.8660254037844387076, 1.000000000000000000, 0.8660254037844387076, 1.000000000000000000, 0.8660254037844387076, 1.000000000000000000, 0.8660254037844387076, 1.000000000000000000, 0.8660254037844387076, 1.000000000000000000, 0.8660254037844387076, 1.000000000000000000, 0.8660254037844387076, 1.000000000000000000, 0.8660254037844387076, 1.000000000000000000, 0.8660254037844387076, 1.000000000000000000, 0.8660254037844387076, 1.000000000000000000, 0.8660254037844387076, 1.000000000000000000, 0.8660254037844387076, 1.000000000000000000, 0.8660254037844387076, 1.000000000000000000, 0.8660254037844387076, 1.000000000000000000, 0.8660254037844387076, 1.000000000000000000, 0.8660254037844387076, 1.000000000000000000, 0.8660254037844387076, 1.000000000000000000, 0.8660254037844387076, 1.000000000000000000, 0.8660254037844387076, 1.000000000000000000, 0.8660254037844387076, 1.000000000000000000, 0.8660254037844387076, 1.000000000000000000, 0.8660254037844387076, 1.000000000000000000, 0.8660254037844387076, 1.000000000000000000, 0.8660254037844387076, 1.000000000000000000, 0.8660254037844387076, 1.000000000000000000, 0.8660254037844387076, 1.000000000000000000, 0.8660254037844387076, 1.000000000000000000, 0.8660254037844387076, 1.000000000000000000, 0.8660254037844387076, 1.000000000000000000, 0.8660254037844387076, 1.000000000000000000, 0.8660254037844387076, 1.000000000000000000, 0.8660254037844387076, 1.000000000000000000, 0.8660254037844387076, 1.000000000000000000, 0.8660254037844387076, 1.000000000000000000, 0.8660254037844387076, 1.000000000000000000, 0.8660254037844387076, 1.000000000000000000, 0.8660254037844387076, 1.000000000000000000, 0.8660254037844387076, 1.000000000000000000, 0.8660254037844387076, 1.000000000000000000, 0.8660254037844387076, 1.000000000000000000, 0.8660254037844387076, 1.000000000000000000, 0.8660254037844387076, 1.000000000000000000, 0.8660254037844387076, 1.000000000000000000, 0.8660254037844387076, 1.000000000000000000, 0.8660254037844387076, 1.000000000000000000, 0.8660254037844387076, 1.000000000000000000, 0.8660254037844387076, 1.000000000000000000, 0.8660254037844387076, 1.000000000000000000, 0.8660254037844387076, 1.000000000000000000, 0.8660254037844387076, 1.000000000000000000, 0.8660254037844387076, 1.000000000000000000, 0.8660254037844387076, 1.000000000000000000, 0.8660254037844387076, 1.000000000000000000, 0.8660254037844387076, 1.000000000000000000, 0.8660254037844387076, 1.000000000000000000, 0.8660254037844387076, 1.000000000000000000, 0.8660254037844387076, 1.000000000000000000, 0.8660254037844387076, 1.000000000000000000, 0.8660254037844387076, 1.000000000000000000, 0.8660254037844387076, 1.000000000000000000, 0.8660254037844387076, 1.000000000000000000, 0.8660254037844387076, 1.000000000000000000, 0.8660254037844387076, 1.000000000000000000, 0.8660254037844387076, 1.000000000000000000, 0.8660254037844387076, 1.000000000000000000, 0.8660254037844387076, 1.000000000000000000, 0.8660254037844387076, 1.000000000000000000, 0.8660254037844387076, 1.000000000000000000, 0.8660254037844387076, 1.000000000000000000, 0.8660254037844387076, 1.000000000000000000, 0.8660254037844387076, 1.000000000000000000, 0.8660254037844387076, 1.000000000000000000, 0.8660254037844387076, 1.000000000000000000, 0.8660254037844387076, 1.000000000000000000, 0.8660254037844387076, 1.000000000000000000, 0.8660254037844387076, 1.000000000000000000, 0.8660254037844387076, 1.000000000000000000, 0.8660254037844387076, 1.000000000000000000, 0.8660254037844387076, 1.000000000000000000, 0.8660254037844387076, 1.000000000000000000, 0.8660254037844387076, 1.000000000000000000, 0.8660254037844387076, 1.000000000000000000, 0.8660254037844387076, 1.000000000000000000, 0.8660254037844387076, 1.000000000000000000, 0.8660254037844387076, 1.000000000000000000, 0.8660254037844387076, 1.000000000000000000, 0.8660254037844387076, 1.000000000000000000, 0.8660254037844387076, 1.000000000000000000, 0.8660254037844387076, 1.000000000000000000, 0.8660254037844387076, 1.000000000000000000, 0.8660254037844387076, 1.000000000000000000, 0.8660254037844387076, 1.000000000000000000, 0.8660254037844387076, 1.000000000000000000, 0.8660254037844387076, 1.000000000000000000, 0.8660254037844387076, 1.000000000000000000, 0.8660254037844387076, 1.000000000000000000, 0.8660254037844387076, 1.000000000000000000, 0.8660254037844387076, 1.000000000000000000, 0.8660254037844387076, 1.000000000000000000, 0.8660254037844387076, 1.000000000000000000, 0.8660254037844387076, 1.000000000000000000, 0.8660254037844387076, 1.000000000000000000, 0.8660254037844387076, 1.000000000000000000, 0.8660254037844387076, 1.000000000000000000, 0.8660254037844387076, 1.000000000000000000, 0.8660254037844387076, 1.000000000000000000, 0.8660254037844387076, 1.000000000000000000, 0.8660254037844387076, 1.000000000000000000, 0.8660254037844387076, 1.000000000000000000, 0.8660254037844387076, 1.000000000000000000, 0.8660254037844387076, 1.000000000000000000, 0.8660254037844387076, 1.000000000000000000, 0.8660254037844387076, 1.000000000000000000, 0.8660254037844387076, 1.000000000000000000) ) ) 
 REPRESENTATION_ITEM ( '' )  SURFACE ( )  );
#84922 = CARTESIAN_POINT ( 'NONE',  ( -6.684333426737305572, 7.757142738403693727, -1.199719254218446718 ) ) ;
#84923 = CARTESIAN_POINT ( 'NONE',  ( 7.065770611016287006, 11.39514947949436774, 1.040834085586084257E-14 ) ) ;
#84924 = LINE ( 'NONE', #182412, #207151 ) ;
#84925 = EDGE_CURVE ( 'NONE', #181416, #51191, #15053, .T. ) ;
#84926 = CARTESIAN_POINT ( 'NONE',  ( 6.844168616800228477, 6.879284895888727824, -0.7998128361456281477 ) ) ;
#84928 = CARTESIAN_POINT ( 'NONE',  ( -1.500000000000011324, 3.170833333333354265, 0.8660254037844403729 ) ) ;
#84927 = CARTESIAN_POINT ( 'NONE',  ( 5.544006925699364707, 0.8563935509715396854, -1.924162301928746821 ) ) ;
#84929 = CARTESIAN_POINT ( 'NONE',  ( 1.240952474410524031, -2.118199589774888647, -0.4760015480929754017 ) ) ;
#84930 = CARTESIAN_POINT ( 'NONE',  ( -1.201851678989727383E-14, 1.134375000341418582, 1.575800808251672791 ) ) ;
#84931 = CARTESIAN_POINT ( 'NONE',  ( 4.815789973571149574, -2.120931333841672650, 0.4164600335647972162 ) ) ;
#84932 = CARTESIAN_POINT ( 'NONE',  ( 5.672522982350666432, 0.8204337683548768023, 1.845723718880077469 ) ) ;
#84933 = DIRECTION ( 'NONE',  ( 1.214306433183764966E-17, 1.000000000000000000, 5.200010849845536803E-32 ) ) ;
#84936 = CARTESIAN_POINT ( 'NONE',  ( 6.371969008742804697, 7.496680600697164465, -1.082531754730543083 ) ) ;
#84935 = CARTESIAN_POINT ( 'NONE',  ( 1.642778471875000035, -2.326041666188709112, -2.845375778867859751 ) ) ;
#84934 = CARTESIAN_POINT ( 'NONE',  ( -6.730704588151846579, 14.55213479732962512, -9.891043484334160141 ) ) ;
#84937 = CARTESIAN_POINT ( 'NONE',  ( -6.818824913030298696, 6.919993584815607335, 0.7998128361456341429 ) ) ;
#84938 = CARTESIAN_POINT ( 'NONE',  ( 3.134000194803722383, 2.016708403948695771, -0.004836970814638129855 ) ) ;
#84939 = CARTESIAN_POINT ( 'NONE',  ( -8.208571938070008400, 11.66408546346865016, -1.199719254218446718 ) ) ;
#84941 = DIRECTION ( 'NONE',  ( 1.000000000000000000, -0.000000000000000000, -0.000000000000000000 ) ) ;
#84940 = CARTESIAN_POINT ( 'NONE',  ( -4.925689880466507908, 4.641059703499347044, -0.7998128361456221525 ) ) ;
#84943 = CARTESIAN_POINT ( 'NONE',  ( 1.364683531250000748, 8.505208333674730170, -0.7879004041258355073 ) ) ;
#84942 = CARTESIAN_POINT ( 'NONE',  ( 4.838837662799537753, 0.3661284547709364734, 2.130314178654398205 ) ) ;
#84944 = CARTESIAN_POINT ( 'NONE',  ( -1.127943160727153060, 3.300000000000025135, -0.7749999999999935829 ) ) ;
#84945 = CARTESIAN_POINT ( 'NONE',  ( 7.110792111438888341, -7.169578370797516698, 7.767011945534281203 ) ) ;
#84947 = CARTESIAN_POINT ( 'NONE',  ( 4.939077454563308933, -1.704950310733845065, -1.076300583479961048 ) ) ;
#84946 = CARTESIAN_POINT ( 'NONE',  ( -8.012505595552038784, 8.450270737673262644, 0.7216878364870578100 ) ) ;
#84948 = CARTESIAN_POINT ( 'NONE',  ( -0.7499999999999972244, 4.608333333333352932, -1.299038105676652011 ) ) ;
#84949 = CARTESIAN_POINT ( 'NONE',  ( 0.3458015845922198239, 1.719860733928044949, 0.1322621976239789499 ) ) ;
#84950 = CARTESIAN_POINT ( 'NONE',  ( 4.850785098639300408, 8.881276058379668825, -0.7998128361456481317 ) ) ;
#84952 = CARTESIAN_POINT ( 'NONE',  ( -3.929058411375401683, 4.999999999999997335, -0.7500000000000006661 ) ) ;
#84951 = CARTESIAN_POINT ( 'NONE',  ( 8.270110514656034084, 9.711179024262627024, 1.082531754730558626 ) ) ;
#84953 = CARTESIAN_POINT ( 'NONE',  ( -11.15559248640632006, 7.313804510108741219, 4.428430090804268637 ) ) ;
#84954 = CARTESIAN_POINT ( 'NONE',  ( 5.255093269098372488, -1.579555527043162488, -1.001684657140684775 ) ) ;
#84955 = CARTESIAN_POINT ( 'NONE',  ( 6.117445361114795865, 1.676175193246462802, 1.114809878595341308 ) ) ;
#84956 = CARTESIAN_POINT ( 'NONE',  ( -4.226491779746760713, 3.979064867095216673, 0.5169678485880250252 ) ) ;
#84957 = B_SPLINE_CURVE_WITH_KNOTS ( 'NONE', 3,
 ( #55976, #54908, #188092, #138303, #206479, #59166 ),
 .UNSPECIFIED., .F., .F.,
 ( 4, 2, 4 ),
 ( 2.491306920542262691E-18, 0.0003472644472073823057, 0.0006945288944147621178 ),
 .UNSPECIFIED. ) ;
#84958 = CARTESIAN_POINT ( 'NONE',  ( -5.275531169048895741, 9.168887107283438809, -0.7216878364870338292 ) ) ;
#84959 = EDGE_LOOP ( 'NONE', ( #31600, #121541 ) ) ;
#84960 = CARTESIAN_POINT ( 'NONE',  ( 10.52076401408022299, 11.37657222595619189, 0.000000000000000000 ) ) ;
#84962 = CARTESIAN_POINT ( 'NONE',  ( 0.4215001937674204280, -1.427952733550428288, -1.423947716221201976 ) ) ;
#84961 = CARTESIAN_POINT ( 'NONE',  ( 2.104293207771616991, -0.9040658786637757460, 1.918231223523607865 ) ) ;
#84963 = CARTESIAN_POINT ( 'NONE',  ( 1.476514701902143623, -1.279619142688562805, 1.282606640394849951 ) ) ;
#84964 = CARTESIAN_POINT ( 'NONE',  ( 6.444921918449731280, 8.612437886315108315, 1.599625672291268286 ) ) ;
#84965 = CARTESIAN_POINT ( 'NONE',  ( 6.385629968321593353, 1.486944277142748794, 1.569300510047972219 ) ) ;
#84966 = AXIS2_PLACEMENT_3D ( 'NONE', #85525, #136434, #69252 ) ;
#84967 = CARTESIAN_POINT ( 'NONE',  ( 7.182068686937156166, 9.402166106225269715, 1.599625672291281386 ) ) ;
#84969 = CARTESIAN_POINT ( 'NONE',  ( 0.2334084307264666924, 0.5983727300521198833, -1.819970363327483076 ) ) ;
#84968 = CARTESIAN_POINT ( 'NONE',  ( -4.660252114795309097, 6.460046772059735432, -1.599625672291256295 ) ) ;
#84970 = CARTESIAN_POINT ( 'NONE',  ( 11.33772463945037146, 13.39999999999998259, 3.599999999999999201 ) ) ;
#84971 = DIRECTION ( 'NONE',  ( -0.000000000000000000, -1.000000000000000000, -0.000000000000000000 ) ) ;
#84972 = VECTOR ( 'NONE', #21726, 1000.000000000000114 ) ;
#84973 = B_SPLINE_CURVE_WITH_KNOTS ( 'NONE', 3,
 ( #106643, #21038, #120785, #87136, #170515, #186762, #119704, #39453, #89292, #22097, #152147, #88210, #3715, #155343 ),
 .UNSPECIFIED., .F., .F.,
 ( 4, 2, 2, 2, 2, 2, 4 ),
 ( 0.5000128224787536713, 0.5890577402443318844, 0.6781026580099100975, 0.7226251168926991486, 0.7671475757754881997, 0.8116700346582772507, 0.8561924935410664128 ),
 .UNSPECIFIED. ) ;
#84974 = CARTESIAN_POINT ( 'NONE',  ( 3.226477370372305753, 4.787309570232886280, 1.443375672974062551 ) ) ;
#84975 = CARTESIAN_POINT ( 'NONE',  ( -8.597841969360544567, 13.18256606422934674, 0.7998128361456341429 ) ) ;
#84976 = CARTESIAN_POINT ( 'NONE',  ( 3.924826023212550030, 2.051882857192890430, 0.6804245187241527715 ) ) ;
#84977 = CARTESIAN_POINT ( 'NONE',  ( -6.455090533882206216, 7.663932056684933158, -1.082531754730549967 ) ) ;
#84978 = CARTESIAN_POINT ( 'NONE',  ( 5.885648082108190238, 7.959951743916638733, 1.443375672974065660 ) ) ;
#84979 = CARTESIAN_POINT ( 'NONE',  ( 1.898838059644195386, -2.080654286433290867, -0.4088066060855889972 ) ) ;
#84980 = CARTESIAN_POINT ( 'NONE',  ( 6.405291383686445350, 1.519602032305459316, 1.011395407323860907 ) ) ;
#84981 = CARTESIAN_POINT ( 'NONE',  ( 1.633988421434044325, 0.9753176276560069358, -1.713140426071022349 ) ) ;
#84982 = CARTESIAN_POINT ( 'NONE',  ( 4.851772015791367743, -1.356534033432246211, -1.348250844427544282 ) ) ;
#84983 = ORIENTED_EDGE ( 'NONE', *, *, #202085, .F. ) ;
#84984 = LINE ( 'NONE', #53555, #11206 ) ;
#84985 = CARTESIAN_POINT ( 'NONE',  ( 6.408657466097477773, 0.6165391127177908270, 1.870651749748206916 ) ) ;
#84986 = CARTESIAN_POINT ( 'NONE',  ( 1.218581363712217591, -0.04816221259190026777, 1.941509521754792855 ) ) ;
#84987 = EDGE_LOOP ( 'NONE', ( #116136, #203685 ) ) ;
#84988 = CARTESIAN_POINT ( 'NONE',  ( -3.688700311369816909, 6.461178242310183784, -1.199719254218450271 ) ) ;
#84990 = CARTESIAN_POINT ( 'NONE',  ( 6.785280070212259318, -6.896483513897647910, -6.645879322773438069 ) ) ;
#84989 = CARTESIAN_POINT ( 'NONE',  ( -7.932929277771797238, 8.427708043588125975, 0.000000000000000000 ) ) ;
#84992 = CARTESIAN_POINT ( 'NONE',  ( 4.380693030546905398, 8.124909279031149012, 0.7216878364870247253 ) ) ;
#84991 = CARTESIAN_POINT ( 'NONE',  ( 7.039708073993665494, 9.236078724457858158, 1.599625672291281386 ) ) ;
#84994 = ORIENTED_EDGE ( 'NONE', *, *, #88440, .F. ) ;
#84993 = CARTESIAN_POINT ( 'NONE',  ( 4.793567869993575314, 1.782951692925707654, -0.6917526515820491273 ) ) ;
#84995 = CARTESIAN_POINT ( 'NONE',  ( 3.791807063958370971, 1.597966631936774684, 1.522356218736670153 ) ) ;
#84996 = CARTESIAN_POINT ( 'NONE',  ( 2.380145745526092593, 1.357289424207007489, 1.739932290444376584 ) ) ;
#84997 = CARTESIAN_POINT ( 'NONE',  ( 1.608462485350656834, 8.735270501766779105, 2.463594439587601492 ) ) ;
#84998 = CARTESIAN_POINT ( 'NONE',  ( 0.6977377480232997975, 1.284608138224270002, 1.416691289136004395 ) ) ;
#84999 = CARTESIAN_POINT ( 'NONE',  ( -10.42545925421531372, 5.088249681016463022, 5.944232428158755077 ) ) ;
#85000 = CARTESIAN_POINT ( 'NONE',  ( -0.4358566159019752195, -8.896924251528570693, 9.793384314894463927 ) ) ;
#85001 = CARTESIAN_POINT ( 'NONE',  ( 0.2999999999999981570, 3.999999999999996447, -0.9782388782689065421 ) ) ;
#85002 = CARTESIAN_POINT ( 'NONE',  ( 3.016144355299533952, 2.060630728401948275, -0.2003171163396169074 ) ) ;
#85003 = CARTESIAN_POINT ( 'NONE',  ( -6.573005544526917099, 6.562927978236513304, -0.7998128361456291469 ) ) ;
#85004 = CIRCLE ( 'NONE', #157703, 11.05000000000000426 ) ;
#85005 = CARTESIAN_POINT ( 'NONE',  ( -5.000347810418038996, 7.933946187056884369, 1.064693650161437022 ) ) ;
#85007 = CARTESIAN_POINT ( 'NONE',  ( 2.079201547314021070, -0.1057080177612122196, -2.159229931372666389 ) ) ;
#85006 = CARTESIAN_POINT ( 'NONE',  ( -3.079673448598517549, 6.744702790006905424, 1.040834085586084257E-14 ) ) ;
#85008 = CARTESIAN_POINT ( 'NONE',  ( 3.333693798916517625, 0.9835563995168915552, -1.958507884819527867 ) ) ;
#85009 = CARTESIAN_POINT ( 'NONE',  ( -0.08174084574804243997, 3.472891232463431788, -1.998431917447621498 ) ) ;
#85010 = DIRECTION ( 'NONE',  ( -0.000000000000000000, 1.000000000000000000, -0.000000000000000000 ) ) ;
#85011 = DIRECTION ( 'NONE',  ( -0.000000000000000000, -1.000000000000000000, -0.000000000000000000 ) ) ;
#85012 = ADVANCED_FACE ( 'NONE', ( #178870 ), #64401, .T. ) ;
#85013 = CARTESIAN_POINT ( 'NONE',  ( -1.402160292154681736E-14, 13.98437500034139624, 1.575800808251682339 ) ) ;
#85014 = CARTESIAN_POINT ( 'NONE',  ( -5.981082042284069367, 7.006959133200059142, 1.199719254218452935 ) ) ;
#85015 = UNCERTAINTY_MEASURE_WITH_UNIT (LENGTH_MEASURE( 1.000000000000000082E-05 ), #24089, 'distance_accuracy_value', 'NONE');
#85016 = CARTESIAN_POINT ( 'NONE',  ( 5.449791032962750137, -1.571470184986222263, -0.7336466892688772168 ) ) ;
#85017 = CARTESIAN_POINT ( 'NONE',  ( -9.327646496521984076, 11.90534021740758064, -1.443375672974059665 ) ) ;
#85018 = CARTESIAN_POINT ( 'NONE',  ( 3.397389602098393802, -1.828008730618407851, 0.9717071122367711977 ) ) ;
#85019 = CARTESIAN_POINT ( 'NONE',  ( 4.991875679739185223, -2.106924267290931851, 0.2088435281543659927 ) ) ;
#85020 = CARTESIAN_POINT ( 'NONE',  ( 5.262536180398716290, 9.291375977107183104, -0.7998128361456291469 ) ) ;
#85021 = CARTESIAN_POINT ( 'NONE',  ( 1.364683531249990311, 4.863541667008084879, 0.7879004041258499402 ) ) ;
#85022 = CARTESIAN_POINT ( 'NONE',  ( 2.553506168856953806, 1.519147476331883517, 1.253303911792477132 ) ) ;
#85023 = CARTESIAN_POINT ( 'NONE',  ( 0.3164790345465406385, -0.6463921985436006379, -1.799943259716822341 ) ) ;
#85024 = CARTESIAN_POINT ( 'NONE',  ( 4.927800006241752406, 1.181458742244513971, -1.964204249851936090 ) ) ;
#85025 = CARTESIAN_POINT ( 'NONE',  ( 2.578497204056416248, -1.747032809129964281, -0.5301130021647950663 ) ) ;
#85026 = CIRCLE ( 'NONE', #168075, 11.00000000000000000 ) ;
#85027 = CARTESIAN_POINT ( 'NONE',  ( 3.770049233051776749, 6.556085317605844232, 1.199719254218451159 ) ) ;
#85028 = CARTESIAN_POINT ( 'NONE',  ( 6.602457619730771832, 6.805214765881779648, 0.7216878364870317197 ) ) ;
#85029 = CARTESIAN_POINT ( 'NONE',  ( -7.854251061018346469, 8.057714414143200443, -0.7998128361456291469 ) ) ;
#85030 = VERTEX_POINT ( 'NONE', #65075 ) ;
#85031 = CARTESIAN_POINT ( 'NONE',  ( 3.761980314931902214, 0.6741652524458006113, -1.897120442666611506 ) ) ;
#85032 = CARTESIAN_POINT ( 'NONE',  ( 4.381663332995835880, -1.878531202089319674, 0.5654445158327011667 ) ) ;
#85033 = CARTESIAN_POINT ( 'NONE',  ( -6.333630315878337136, 10.54098580183340772, 0.000000000000000000 ) ) ;
#85034 = CARTESIAN_POINT ( 'NONE',  ( -4.415151579544611238, 8.302760609444034046, -0.7998128361456281477 ) ) ;
#85035 = CARTESIAN_POINT ( 'NONE',  ( 0.07536363704235479744, 6.947016338497881804, -2.739277465201896078 ) ) ;
#85037 = CARTESIAN_POINT ( 'NONE',  ( 5.893352214189693683, 1.342564598491655437, 1.153274331617970550 ) ) ;
#85036 = CARTESIAN_POINT ( 'NONE',  ( 0.04657986452102218927, -1.676603903080859492, 1.248863468804935151 ) ) ;
#85038 = CARTESIAN_POINT ( 'NONE',  ( 10.99126615174919053, -5.199999999999992184, -0.4382560683119160472 ) ) ;
#85039 = CARTESIAN_POINT ( 'NONE',  ( 2.203317661949526052, -0.4785072280911427667, 2.138412878249687399 ) ) ;
#85040 = CARTESIAN_POINT ( 'NONE',  ( 0.2568327444973814155, 1.721937519821172602, -0.2522849218079876721 ) ) ;
#85041 = CARTESIAN_POINT ( 'NONE',  ( 7.938462636001388795, 9.220293482545153907, -1.199719254218441611 ) ) ;
#85042 = CARTESIAN_POINT ( 'NONE',  ( 0.1335669894368813060, 0.6916768264315333870, -2.234939561487662818 ) ) ;
#85043 = CARTESIAN_POINT ( 'NONE',  ( 0.2578720826223569462, 0.6548769427211723615, 1.595941719785697988 ) ) ;
#85044 = CARTESIAN_POINT ( 'NONE',  ( 0.8612291682562907003, -0.8250023432496387255, 2.145356560901264142 ) ) ;
#85045 = CARTESIAN_POINT ( 'NONE',  ( 0.2225716830646235489, 2.098996182288978218, 0.6302611576235671587 ) ) ;
#85046 = CARTESIAN_POINT ( 'NONE',  ( 6.591143254762334536, 0.9945565086073978600, -1.419977980273220863 ) ) ;
#85047 = CARTESIAN_POINT ( 'NONE',  ( 3.387540773601561916, 1.995160029947869340, -0.9435142334218297178 ) ) ;
#85048 = CARTESIAN_POINT ( 'NONE',  ( 6.584450689261575285, 1.255587272919860942, -1.771131291935989616 ) ) ;
#85049 = CARTESIAN_POINT ( 'NONE',  ( -1.201851678989727383E-14, 3.962500000000022560, 1.732050807568877637 ) ) ;
#85050 = CARTESIAN_POINT ( 'NONE',  ( 1.042374724401398334, 0.8638241406289723923, 1.933313940807819487 ) ) ;
#85051 = CARTESIAN_POINT ( 'NONE',  ( 6.727182134110200273, 0.5640974741700152117, 2.241195997201197443 ) ) ;
#85053 = ADVANCED_FACE ( 'NONE', ( #114973 ), #164727, .F. ) ;
#85052 = CARTESIAN_POINT ( 'NONE',  ( 5.034167752753979208, 0.9906028322895725768, -1.652054708979720399 ) ) ;
#85054 = ORIENTED_EDGE ( 'NONE', *, *, #50115, .T. ) ;
#85056 = CARTESIAN_POINT ( 'NONE',  ( 0.7499999999999902300, 5.816666666666685082, -1.299038105676658228 ) ) ;
#85055 = CARTESIAN_POINT ( 'NONE',  ( 1.382826565882399272, -0.3421621995536459626, -2.266597836251768250 ) ) ;
#85057 = CARTESIAN_POINT ( 'NONE',  ( 4.684505768721569652, 5.424010470718658716, -1.199719254218452047 ) ) ;
#85058 = CARTESIAN_POINT ( 'NONE',  ( 6.328958779480917229, 6.278206752349526631, 0.7998128361456341429 ) ) ;
#85059 = CARTESIAN_POINT ( 'NONE',  ( 5.338630837375411886, 1.324400161455315805, -1.783172940106398485 ) ) ;
#85060 = CARTESIAN_POINT ( 'NONE',  ( -6.887178846062109727, 10.01849717283904262, -1.082531754730537976 ) ) ;
#85061 = DIRECTION ( 'NONE',  ( 0.000000000000000000, -1.000000000000000000, 0.000000000000000000 ) ) ;
#85062 = CARTESIAN_POINT ( 'NONE',  ( 4.663641653420880218, 8.384739662392275861, -0.7216878364870207285 ) ) ;
#85063 = CARTESIAN_POINT ( 'NONE',  ( -7.321039761255057066, 11.48503745486550365, 0.000000000000000000 ) ) ;
#85064 = CARTESIAN_POINT ( 'NONE',  ( 6.373741612200174878, 6.608655767087927124, 0.7216878364870328300 ) ) ;
#85065 = CARTESIAN_POINT ( 'NONE',  ( 2.865861461037176205, -0.1511401116795624278, -2.010826411938296143 ) ) ;
#85067 = CARTESIAN_POINT ( 'NONE',  ( 1.323174825800084609, -1.862915942116917689, -0.8856262590048938899 ) ) ;
#85066 = CARTESIAN_POINT ( 'NONE',  ( 6.103141704446003679, 10.27208242182903142, 0.7998128361456462443 ) ) ;
#85068 = FILL_AREA_STYLE ('',( #200922 ) ) ;
#85069 = EDGE_CURVE ( 'NONE', #146971, #188369, #183627, .T. ) ;
#85070 = CARTESIAN_POINT ( 'NONE',  ( 5.302647476276220573, 8.240153584747313076, -1.082531754730548412 ) ) ;
#85071 = CARTESIAN_POINT ( 'NONE',  ( -3.914023514147247251, 8.998170835453741745, 0.7749999999999996891 ) ) ;
#85072 = CARTESIAN_POINT ( 'NONE',  ( -1.364683531250012516, 3.530208333674758059, 0.7879004041258379498 ) ) ;
#85073 = CARTESIAN_POINT ( 'NONE',  ( 3.890727776643727598, 1.851661642969665067, -1.171806376371389957 ) ) ;
#85074 = CARTESIAN_POINT ( 'NONE',  ( 1.266250242576156815, 1.862016182229693673, -0.7743172429433076154 ) ) ;
#85075 = CARTESIAN_POINT ( 'NONE',  ( 1.259045258496578557, 1.813921241667546758, -0.3151448728593714277 ) ) ;
#85076 = CARTESIAN_POINT ( 'NONE',  ( 5.460555387939631800, -2.071112900911156185, -0.9828140750258400615 ) ) ;
#85077 = CARTESIAN_POINT ( 'NONE',  ( 2.870863542623874221, 1.748142402769039760, -0.5779331317549916136 ) ) ;
#85078 = CARTESIAN_POINT ( 'NONE',  ( 9.759171643738394408, 10.28012176064996197, 0.000000000000000000 ) ) ;
#85079 = FILL_AREA_STYLE ('',( #117652 ) ) ;
#85080 = CARTESIAN_POINT ( 'NONE',  ( 3.733261478165556646, -1.687024869733319221, 0.6981082995600741414 ) ) ;
#85081 = CARTESIAN_POINT ( 'NONE',  ( 5.203750078570229753, 1.864167652161516031, 0.7691231355932278690 ) ) ;
#85082 = CARTESIAN_POINT ( 'NONE',  ( -9.515124878692420296, 9.995400534762978850, 1.040834085586084257E-14 ) ) ;
#85084 = CARTESIAN_POINT ( 'NONE',  ( -7.795011973214244883, 8.058878488363559356, 0.7998128361456341429 ) ) ;
#85083 = CARTESIAN_POINT ( 'NONE',  ( 4.364347144703619286, 1.063191675971109307, 1.997143021516068595 ) ) ;
#85085 = CARTESIAN_POINT ( 'NONE',  ( 6.370163019944321547, 1.079249059096079044, 1.808242165975785909 ) ) ;
#85086 = CARTESIAN_POINT ( 'NONE',  ( -1.930984528693968194, 3.480873151564079837, -0.4000000000000285549 ) ) ;
#85087 = CARTESIAN_POINT ( 'NONE',  ( 3.631357695093720750, 0.05367941694835526995, -2.069842578854002468 ) ) ;
#85088 = CARTESIAN_POINT ( 'NONE',  ( 4.162516854595432747, 4.815023404238158555, 1.199719254218464037 ) ) ;
#85089 = CARTESIAN_POINT ( 'NONE',  ( -4.957638175832625493E-14, 2.359375000341373152, -1.570758158831806250 ) ) ;
#85090 = PRODUCT_CONTEXT ( 'NONE', #86421, 'mechanical' ) ;
#85092 = CARTESIAN_POINT ( 'NONE',  ( 1.629391185616009707, -1.814203104720218951, 0.6484763462606003559 ) ) ;
#85091 = CARTESIAN_POINT ( 'NONE',  ( -9.027031348600448979, 9.425958082989001952, 1.040834085586084257E-14 ) ) ;
#85093 = CARTESIAN_POINT ( 'NONE',  ( 4.870353810550047235, 4.974663864576271521, -0.7564775847674284348 ) ) ;
#85094 = CARTESIAN_POINT ( 'NONE',  ( 6.825064197248748243, -1.799304382776808930, -0.8012231885662893793 ) ) ;
#85095 = CARTESIAN_POINT ( 'NONE',  ( 4.163762572728282763, 6.911454530608037494, -1.082531754730548412 ) ) ;
#85096 = CARTESIAN_POINT ( 'NONE',  ( 5.504159067553832330, 6.221818635116664886, 0.9641881782859774708 ) ) ;
#85097 = CARTESIAN_POINT ( 'NONE',  ( -2.266184231778562541, 5.795632037050281404, 1.040834085586084257E-14 ) ) ;
#85098 = CARTESIAN_POINT ( 'NONE',  ( 1.301376502765494658, -0.3325571857498362260, -2.196291469625763160 ) ) ;
#85099 = CARTESIAN_POINT ( 'NONE',  ( 3.628042789974804450, -1.253006538321174146, -1.692492853607285630 ) ) ;
#85100 = CARTESIAN_POINT ( 'NONE',  ( -5.427006627220116286, 9.553534508390610469, -0.7998128361456362523 ) ) ;
#85101 = CARTESIAN_POINT ( 'NONE',  ( 6.317209508963599340, 9.457495962844502557, 1.199719254218462483 ) ) ;
#85102 = CARTESIAN_POINT ( 'NONE',  ( 0.1857038103042158439, -1.139949723551544114, -1.471474936012186596 ) ) ;
#85103 = CARTESIAN_POINT ( 'NONE',  ( 7.070740804726770357, 8.207951346058097286, 1.199719254218462483 ) ) ;
#85104 = CARTESIAN_POINT ( 'NONE',  ( 5.335297142177534369, 6.183267073083954735, -1.199719254218452047 ) ) ;
#85105 = CARTESIAN_POINT ( 'NONE',  ( -6.509323148336870091, 7.727203440215372865, 1.082531754730549078 ) ) ;
#85106 = CARTESIAN_POINT ( 'NONE',  ( -6.860062538834774237, 10.94723069537516302, 0.7216878364870458196 ) ) ;
#85107 = CARTESIAN_POINT ( 'NONE',  ( 1.740644586495963431, 1.216819214799185866, -1.736574482785017359 ) ) ;
#85108 = CARTESIAN_POINT ( 'NONE',  ( -5.237192476628793614, 9.332084666034067055, 0.7998128361456291469 ) ) ;
#85110 = CARTESIAN_POINT ( 'NONE',  ( 4.105873170248697690, 0.6631157982108953908, -1.846516426336957784 ) ) ;
#85109 = CARTESIAN_POINT ( 'NONE',  ( -1.225000000000014300, 0.7500000000000145439, -2.602085213965210642E-14 ) ) ;
#85111 = CARTESIAN_POINT ( 'NONE',  ( 3.151412294154242844, -1.766339975446712174, -1.245920677233211871 ) ) ;
#85112 = CARTESIAN_POINT ( 'NONE',  ( 1.909461114401575843, -0.8690924446688346183, -1.623246667998109682 ) ) ;
#85113 = CARTESIAN_POINT ( 'NONE',  ( -4.138143308069708759, 7.456237844118314584, -0.6866288536411498944 ) ) ;
#85114 = CARTESIAN_POINT ( 'NONE',  ( 4.203240766677102336, 7.568734712931471265, -0.9219714408205395006 ) ) ;
#85115 = CARTESIAN_POINT ( 'NONE',  ( 4.769343782054527026, 1.005586498893149772, 1.420189556619367410 ) ) ;
#85116 = CARTESIAN_POINT ( 'NONE',  ( 0.3263184169964285508, 14.00000000000028955, -11.67999999558625213 ) ) ;
#85117 = CARTESIAN_POINT ( 'NONE',  ( 6.209271165378815738, 7.306866450105836464, -1.082531754730543083 ) ) ;
#85118 = CARTESIAN_POINT ( 'NONE',  ( -10.99878419127389684, 6.872217442641685103, 3.961452310287494338 ) ) ;
#85119 = CARTESIAN_POINT ( 'NONE',  ( 1.885829143180400624, 1.490600019384461072, 1.565824011241300440 ) ) ;
#85120 = VERTEX_POINT ( 'NONE', #32596 ) ;
#85121 = CARTESIAN_POINT ( 'NONE',  ( 3.532577226125938274, 1.967586357134976094, -0.4389627639644277934 ) ) ;
#85122 = CARTESIAN_POINT ( 'NONE',  ( -0.3713344243775550391, 2.999999999999984901, -0.3713344243775790754 ) ) ;
#85123 = CARTESIAN_POINT ( 'NONE',  ( 0.7960496800812133511, -0.7770375076890515542, 2.017388685454111652 ) ) ;
#85124 = CARTESIAN_POINT ( 'NONE',  ( 3.133621081638960693, -1.322844378366348606, -1.461937730511401190 ) ) ;
#85125 = CIRCLE ( 'NONE', #106056, 0.08000000000000020983 ) ;
#85126 = CARTESIAN_POINT ( 'NONE',  ( -1.333449616921166481, 8.249651149236388648, -11.01993490927447716 ) ) ;
#85127 = CARTESIAN_POINT ( 'NONE',  ( 3.772937862106290563, 1.827633595424851043, -0.6570963203050876889 ) ) ;
#85130 = VERTEX_POINT ( 'NONE', #198273 ) ;
#85129 = CARTESIAN_POINT ( 'NONE',  ( -4.556949027968976829, 5.449433633119473264, 1.082531754730549078 ) ) ;
#85128 = FACE_OUTER_BOUND ( 'NONE', #121830, .T. ) ;
#85131 = CARTESIAN_POINT ( 'NONE',  ( -5.939880696118548187, 6.102484698325975288, 0.000000000000000000 ) ) ;
#85132 = CARTESIAN_POINT ( 'NONE',  ( -0.1106856583840696712, 2.878213433396461962, -2.485464591233726317 ) ) ;
#85133 = CARTESIAN_POINT ( 'NONE',  ( 4.227110032410640095, 8.153655147779589996, 0.7998128361456271485 ) ) ;
#85134 = CARTESIAN_POINT ( 'NONE',  ( -3.871735385154307263, 6.674719161725423788, -1.199719254218450271 ) ) ;
#85135 = CARTESIAN_POINT ( 'NONE',  ( -7.117104292530948229, 7.267986194233038155, -0.7998128361456362523 ) ) ;
#85136 = CARTESIAN_POINT ( 'NONE',  ( -10.45297324601190425, 11.29748299654313470, 0.7216878364870438212 ) ) ;
#85137 = CARTESIAN_POINT ( 'NONE',  ( 6.827182134110238110, -0.009824402486291110986, 2.288967694407697984 ) ) ;
#85138 = CARTESIAN_POINT ( 'NONE',  ( -1.642778471874998480, -3.551041666188709645, 2.845375778867863303 ) ) ;
#85139 = CARTESIAN_POINT ( 'NONE',  ( 4.381663332995835880, -1.878531202089319674, 0.5654445158327011667 ) ) ;
#85140 = CARTESIAN_POINT ( 'NONE',  ( 1.354138928560550070, 0.1455316553338575625, -2.011204400906742240 ) ) ;
#85141 = EDGE_LOOP ( 'NONE', ( #40322, #142285, #153014, #93229, #126701 ) ) ;
#85142 = CARTESIAN_POINT ( 'NONE',  ( 3.573546900796530146, 1.536558363836796337, 1.457006447099787882 ) ) ;
#85143 = CARTESIAN_POINT ( 'NONE',  ( 1.499999999999989120, 2.806250000682818158, 1.214306433183764966E-14 ) ) ;
#85145 = CARTESIAN_POINT ( 'NONE',  ( -6.566226467720086113, 6.555019055295208119, 1.040834085586084257E-14 ) ) ;
#85144 = CARTESIAN_POINT ( 'NONE',  ( 0.07459516483343266169, 4.098104556601829707, -2.310507343083552989 ) ) ;
#85146 = CARTESIAN_POINT ( 'NONE',  ( 3.187279605439637287, -0.7454021820463945236, 1.683677988101241141 ) ) ;
#85147 = ORIENTED_EDGE ( 'NONE', *, *, #121295, .T. ) ;
#85148 =( REPRESENTATION_RELATIONSHIP ('NONE','NONE', #84563, #189584 ) REPRESENTATION_RELATIONSHIP_WITH_TRANSFORMATION ( #109958 )SHAPE_REPRESENTATION_RELATIONSHIP( ) );
#85149 = UNCERTAINTY_MEASURE_WITH_UNIT (LENGTH_MEASURE( 1.000000000000000082E-05 ), #23410, 'distance_accuracy_value', 'NONE');
#85150 = CARTESIAN_POINT ( 'NONE',  ( -8.941766003412679353, 10.39081407785832845, -1.199719254218446718 ) ) ;
#85152 = MANIFOLD_SOLID_BREP ( 'Cut-Extrude3', #91447 ) ;
#85151 = CARTESIAN_POINT ( 'NONE',  ( 0.003385325826184980898, 8.210945192570370921, 2.038658773260200174 ) ) ;
#85154 = EDGE_CURVE ( 'NONE', #214357, #72912, #162948, .T. ) ;
#85153 = CARTESIAN_POINT ( 'NONE',  ( 4.728832233812888752, 1.460412846248357210, -1.537820402542383169 ) ) ;
#85155 = CARTESIAN_POINT ( 'NONE',  ( 6.925078400183544147, 0.003529629153843987736, 1.755452343125717851 ) ) ;
#85156 = CARTESIAN_POINT ( 'NONE',  ( 7.962716289927667113, 8.184257181204083409, -0.7998128361456291469 ) ) ;
#85157 = CARTESIAN_POINT ( 'NONE',  ( 5.606733736089553055, 1.563247385715782700, -1.342922781998987736 ) ) ;
#85159 = CARTESIAN_POINT ( 'NONE',  ( 2.806014743833367131, 1.331929863061011465, -1.271513748034671654 ) ) ;
#85158 = CARTESIAN_POINT ( 'NONE',  ( 0.3790724793553065797, -0.09720884262147008736, 1.858658634516747510 ) ) ;
#85160 = CARTESIAN_POINT ( 'NONE',  ( 9.073431116043567002, 11.60875560684942265, -1.599625672291262513 ) ) ;
#85161 = SURFACE_SIDE_STYLE ('',( #152302 ) ) ;
#85162 = CARTESIAN_POINT ( 'NONE',  ( 10.98633066092261323, -7.699791778944355514, -0.5535395452644623626 ) ) ;
#85163 = MECHANICAL_DESIGN_GEOMETRIC_PRESENTATION_REPRESENTATION (  '', ( #178555 ), #81766 ) ;
#85164 = CARTESIAN_POINT ( 'NONE',  ( 2.403190426070573871, 1.771669130372434564, -1.315670724662293178 ) ) ;
#85165 = CARTESIAN_POINT ( 'NONE',  ( 5.255258077898470326, -1.907309223944063437, -1.216589440439620695 ) ) ;
#85166 = CARTESIAN_POINT ( 'NONE',  ( -7.049876689426103127, 10.20831132343037062, -1.082531754730537976 ) ) ;
#85167 = CARTESIAN_POINT ( 'NONE',  ( 5.185751641416406876, 1.743707907788614619, -0.4909320375018846883 ) ) ;
#85168 = CARTESIAN_POINT ( 'NONE',  ( 4.487445792895001340, -0.5051273088985311910, 1.847880739403139572 ) ) ;
#85169 = CARTESIAN_POINT ( 'NONE',  ( 1.364683531249990311, 5.196875000341417916, 1.214306433183764966E-14 ) ) ;
#85170 = CARTESIAN_POINT ( 'NONE',  ( 4.188322375386017704, -1.949839058108787437, -0.2904977467932718382 ) ) ;
#85171 = CARTESIAN_POINT ( 'NONE',  ( 5.225416543158964977, -1.776039340814106637, 0.5876355328483380269 ) ) ;
#85172 = CARTESIAN_POINT ( 'NONE',  ( 4.281604344665800532, -1.781275985052663158, 0.5390932415961935398 ) ) ;
#85173 = CARTESIAN_POINT ( 'NONE',  ( 3.553238514845298734, 7.337208092372121904, -0.2327671511505452484 ) ) ;
#85174 = CARTESIAN_POINT ( 'NONE',  ( 0.1281391398850126040, 2.011452084832816123, 0.1435147193784985509 ) ) ;
#85176 = CARTESIAN_POINT ( 'NONE',  ( 1.225372267635124635, -0.04993704651819717150, 2.105648344105083947 ) ) ;
#85175 = CARTESIAN_POINT ( 'NONE',  ( -3.755245360860939297, 4.443836344834937613, -1.082531754730548412 ) ) ;
#85177 = CARTESIAN_POINT ( 'NONE',  ( 9.642873567817520808, 12.27310513391906532, 1.599625672291279388 ) ) ;
#85179 = CARTESIAN_POINT ( 'NONE',  ( -0.08000000000000714873, -9.999999999999994671, 10.99970695577494872 ) ) ;
#85178 = DIRECTION ( 'NONE',  ( 0.000000000000000000, 1.000000000000000000, 0.000000000000000000 ) ) ;
#85180 = CARTESIAN_POINT ( 'NONE',  ( 2.918346969001627045, -2.117983955170518851, 0.1081942149789016649 ) ) ;
#85181 = DIRECTION ( 'NONE',  ( 0.000000000000000000, -1.000000000000000000, 0.000000000000000000 ) ) ;
#85182 = CARTESIAN_POINT ( 'NONE',  ( 1.388932113579334660, -1.919223592974130588, -0.6296790815572687050 ) ) ;
#85183 = CARTESIAN_POINT ( 'NONE',  ( 1.364683531249986537, 1.655208333674748955, -0.7879004041258239610 ) ) ;
#85184 = CARTESIAN_POINT ( 'NONE',  ( -3.795919822146293754, 4.491289883001181593, -1.082531754730549967 ) ) ;
#85185 = CARTESIAN_POINT ( 'NONE',  ( 3.714044015139744914, 6.420469553383295391, 1.199719254218462483 ) ) ;
#85186 = ORIENTED_EDGE ( 'NONE', *, *, #116226, .F. ) ;
#85187 = CARTESIAN_POINT ( 'NONE',  ( 1.933122032479916985, 0.2097677157741582865, 2.151362962771664833 ) ) ;
#85188 = CARTESIAN_POINT ( 'NONE',  ( 6.609999999999985221, 3.681232580627872952, 2.794007784547379192 ) ) ;
#85191 = CARTESIAN_POINT ( 'NONE',  ( 5.361443639997856891, 4.701392137926264425, -2.440314829665658714 ) ) ;
#85190 = CARTESIAN_POINT ( 'NONE',  ( -4.226925616482867909, 3.500738074553338741, -2.444828727306142646 ) ) ;
#85189 = CARTESIAN_POINT ( 'NONE',  ( 3.250922972226694352, 7.014770244231638863, 0.7998128361456281477 ) ) ;
#85192 = CARTESIAN_POINT ( 'NONE',  ( 8.690413276235306128, 13.08263988900915109, -0.7216878364870267237 ) ) ;
#85193 = CARTESIAN_POINT ( 'NONE',  ( -0.1296875068448137269, 7.629137130509075604, -2.426516348560475045 ) ) ;
#85194 = CARTESIAN_POINT ( 'NONE',  ( -7.375272376154093479, 9.627570410311676596, -1.443375672974059665 ) ) ;
#85195 = CARTESIAN_POINT ( 'NONE',  ( 1.242012060539962492, 2.189267750446591609, 0.1026977899005257211 ) ) ;
#85196 = CARTESIAN_POINT ( 'NONE',  ( 10.38614328979769041, 3.507114751586604129, 5.996442624206595795 ) ) ;
#85198 = CARTESIAN_POINT ( 'NONE',  ( -1.402160292154681736E-14, 11.67187500034139980, 1.575800808251682339 ) ) ;
#85197 = CARTESIAN_POINT ( 'NONE',  ( 1.341102801589135529, 0.4431706325995210527, 2.218532444564396577 ) ) ;
#85199 = CARTESIAN_POINT ( 'NONE',  ( -9.508345801885592863, 9.987491611821676329, 0.7998128361456462443 ) ) ;
#85200 = B_SPLINE_CURVE_WITH_KNOTS ( 'NONE', 3,
 ( #196757, #100313, #65652, #129713, #81931, #148017, #194616, #79799, #17972, #195698, #131799, #180506, #163203 ),
 .UNSPECIFIED., .F., .F.,
 ( 4, 3, 3, 3, 4 ),
 ( 1.953129352420981408E-17, 6.251590020777592386E-05, 0.0001877400439070772351, 0.0002924247082610473628, 0.0003977189496704516282 ),
 .UNSPECIFIED. ) ;
#85201 = CARTESIAN_POINT ( 'NONE',  ( -3.253593677155282471, 6.739683690082376444, 1.040834085586084257E-14 ) ) ;
#85202 = CARTESIAN_POINT ( 'NONE',  ( -0.6823417656250003738, 2.030208333674753174, -1.181850606188749264 ) ) ;
#85203 = CARTESIAN_POINT ( 'NONE',  ( 4.684024595049480766, 8.263433789595206136, 0.5754648794667740486 ) ) ;
#85204 = CARTESIAN_POINT ( 'NONE',  ( 1.499999999999997113, 9.145833333333330373, -0.8660254037844378194 ) ) ;
#85205 = CARTESIAN_POINT ( 'NONE',  ( 3.773808747373870620, 0.9599976342714054978, 1.432812656881277791 ) ) ;
#85206 = CARTESIAN_POINT ( 'NONE',  ( 4.903208829997618423, 5.749440385532527564, -1.199719254218450271 ) ) ;
#85207 = CARTESIAN_POINT ( 'NONE',  ( 2.301682877085888368, -1.769492147959438322, 0.03813942612425345879 ) ) ;
#85208 = CARTESIAN_POINT ( 'NONE',  ( 5.174942826180319422, -2.076333920960464763, -0.7478091396579674699 ) ) ;
#85209 = VERTEX_POINT ( 'NONE', #148491 ) ;
#85210 = CARTESIAN_POINT ( 'NONE',  ( -4.261005416444848315, 8.193199762486115034, 0.7998128361456352531 ) ) ;
#85211 = CARTESIAN_POINT ( 'NONE',  ( 5.220327442464319567, 1.987051044970666647, 0.3419161450798278157 ) ) ;
#85213 = ORIENTED_EDGE ( 'NONE', *, *, #206026, .T. ) ;
#85212 = CARTESIAN_POINT ( 'NONE',  ( 4.675916410682629198, 1.790815896176844335, -0.2727875059450618478 ) ) ;
#85214 = CARTESIAN_POINT ( 'NONE',  ( 2.694054421766532759, -1.865511834602461505, -0.1395888279770511053 ) ) ;
#85215 = B_SPLINE_CURVE_WITH_KNOTS ( 'NONE', 3,
 ( #54191, #26749, #141619, #59246, #140550, #45166, #125404, #191369, #177283, #158896 ),
 .UNSPECIFIED., .F., .F.,
 ( 4, 3, 3, 4 ),
 ( 2.717543607569314096E-17, 3.125160614615090737E-05, 6.250328995029551141E-05, 0.0001021784628617198687 ),
 .UNSPECIFIED. ) ;
#85216 = CARTESIAN_POINT ( 'NONE',  ( 6.604126001430527637, -1.825160783932573860, 0.05055279568313279792 ) ) ;
#85217 = CARTESIAN_POINT ( 'NONE',  ( 2.267699027020404490, 0.5063876334258295975, -1.844086191983687062 ) ) ;
#85218 = CARTESIAN_POINT ( 'NONE',  ( -1.441120163477494165, 8.287694259231830785, 3.161243217722575327 ) ) ;
#85219 = CARTESIAN_POINT ( 'NONE',  ( -10.67060214796032724, 5.239869845146935212, -6.813287888368859235 ) ) ;
#85220 = CARTESIAN_POINT ( 'NONE',  ( -1.364683531250012516, 3.092708333674755838, 0.7879004041258379498 ) ) ;
#85221 = CARTESIAN_POINT ( 'NONE',  ( 0.05278957052760185897, 0.3289079202175131389, 1.883742972368242174 ) ) ;
#85222 = CARTESIAN_POINT ( 'NONE',  ( 6.888951449519509218, 7.209733910627123876, -0.7216878364870317197 ) ) ;
#85223 = CARTESIAN_POINT ( 'NONE',  ( 1.521847698614446687, 1.933392594956625521, -0.3320675068423510345 ) ) ;
#85224 = LINE ( 'NONE', #65746, #203221 ) ;
#85225 = CARTESIAN_POINT ( 'NONE',  ( -4.938913097128142304, 8.984092056616635347, -0.7998128361456362523 ) ) ;
#85226 = CARTESIAN_POINT ( 'NONE',  ( 5.625269520628737752, 1.871107552910089122, 0.9978724776121964402 ) ) ;
#85228 = FACE_OUTER_BOUND ( 'NONE', #190345, .T. ) ;
#85227 = CARTESIAN_POINT ( 'NONE',  ( 9.206149998879153529, 10.69926207256923689, 1.199719254218453823 ) ) ;
#85229 = CARTESIAN_POINT ( 'NONE',  ( 5.149669460738499183, 0.6209446730581876794, -1.871051946789156650 ) ) ;
#85230 = CARTESIAN_POINT ( 'NONE',  ( 0.6823417656249899377, 3.092708333674754062, 1.181850606188765695 ) ) ;
#85231 = CARTESIAN_POINT ( 'NONE',  ( 0.7736903856863480700, 0.3886292558455446411, -1.975178614941161870 ) ) ;
#85232 = EDGE_LOOP ( 'NONE', ( #211927, #174416, #156561, #105896 ) ) ;
#85233 =( GEOMETRIC_REPRESENTATION_CONTEXT ( 3 ) GLOBAL_UNCERTAINTY_ASSIGNED_CONTEXT ( ( #149029 ) ) GLOBAL_UNIT_ASSIGNED_CONTEXT ( ( #134807, #83884, #50333 ) ) REPRESENTATION_CONTEXT ( 'NONE', 'WORKASPACE' ) );
#85234 = CARTESIAN_POINT ( 'NONE',  ( 0.5447201963149818082, -1.530340168762192254, 1.463345158046714056 ) ) ;
#85235 = CARTESIAN_POINT ( 'NONE',  ( 11.92009470520713066, 6.690327200924609308, -0.9868518554555439914 ) ) ;
#85236 = CARTESIAN_POINT ( 'NONE',  ( 3.033707436314789785, 1.966763487489433970, -0.6469820378900912328 ) ) ;
#85237 = CARTESIAN_POINT ( 'NONE',  ( 3.770049233051776749, 6.556085317605844232, 1.199719254218451159 ) ) ;
#85238 = CARTESIAN_POINT ( 'NONE',  ( 6.547661840756936691, 6.603636667163397256, 0.7998128361456352531 ) ) ;
#85239 = ORIENTED_EDGE ( 'NONE', *, *, #193710, .F. ) ;
#85241 = CARTESIAN_POINT ( 'NONE',  ( 5.705283713252285338, 5.550585841749444249, -0.7998128361456211532 ) ) ;
#85240 = CARTESIAN_POINT ( 'NONE',  ( 4.699217343460686536, -0.5580910489941055541, 2.014698706189700594 ) ) ;
#85244 = ORIENTED_EDGE ( 'NONE', *, *, #22906, .F. ) ;
#85243 = CARTESIAN_POINT ( 'NONE',  ( 2.543383136322028282, -1.689629589678593558, 0.6535807426650240837 ) ) ;
#85242 = CARTESIAN_POINT ( 'NONE',  ( 3.504746488097260748, 1.439749907568649068, -1.122338611188322455 ) ) ;
#85245 = DIRECTION ( 'NONE',  ( 0.000000000000000000, 0.000000000000000000, -1.000000000000000000 ) ) ;
#85246 = CARTESIAN_POINT ( 'NONE',  ( 9.266593812803435526, 13.58595580518854362, 6.819388300972848427 ) ) ;
#85247 = CARTESIAN_POINT ( 'NONE',  ( 4.999154358079874960, 1.837129776665728187, -1.222328095618854693 ) ) ;
#85249 =( BOUNDED_SURFACE ( )  B_SPLINE_SURFACE ( 3, 3, ( 
 ( #131793, #197798, #33177, #99258, #38510, #202031, #51570, #198849, #67766, #133917, #136018, #85118, #69908, #3834, #103513, #151204, #184733, #53691, #199924, #22219, #37436, #104588, #120906, #117695, #170633, #101368, #52622, #119823, #150140, #1712 ),
 ( #21153, #183687, #169572, #35293, #167446, #19040, #2776, #84052, #34234, #185803, #87259, #68846, #634, #132845, #168504, #153323, #4898, #88332, #134966, #200974, #118750, #36359, #102436, #100307, #186878, #54757, #20104, #86191, #70976, #152260 ),
 ( #137086, #203112, #66698, #50496, #116617, #182612, #166373, #17965, #27591, #5974, #42808, #175998, #155460, #125180, #9208, #92627, #76342, #60089, #108916, #26519, #173875, #208457, #205250, #191142, #174938, #142449, #172793, #23300, #24365, #8133 ),
 ( #158670, #154396, #72046, #10267, #126250, #105674, #74219, #204166, #192209, #124123, #156543, #140314, #43871, #190085, #109987, #141395, #56892, #138158, #7043, #73119, #75280, #90477, #207405, #157612, #55821, #206332, #41737, #59024, #139220, #121978 ),
 ( #189021, #123067, #187942, #106765, #171701, #57957, #39572, #107846, #40663, #25448, #89411, #91555, #48141, #160803, #210607, #46003, #78473, #177053, #127323, #64365, #146710, #194360, #93689, #11330, #47069, #80617, #130511, #115308, #128393, #79544 ),
 ( #114254, #212726, #44938, #196498, #211658, #112122, #159731, #180250, #65396, #97953, #63296, #179190, #113186, #95822, #195439, #31874, #12394, #161881, #181298, #77408, #164007, #143525, #94755, #15583, #162942, #81670, #147756, #213774, #131542, #197544 ),
 ( #145662, #30814, #178125, #96893, #111046, #209521, #13468, #29740, #144592, #49189, #62235, #129456, #14523, #28670, #61161, #193294, #100057, #3585, #67518, #84867, #167194, #201791, #17706, #53431, #68592, #37184, #185555, #32925, #54506, #119568 ) ),
 .UNSPECIFIED., .T., .F., .F. ) 
 B_SPLINE_SURFACE_WITH_KNOTS ( ( 4, 3, 4 ),
 ( 4, 2, 2, 2, 2, 2, 2, 2, 2, 2, 2, 2, 2, 2, 4 ),
 ( 0.000000000000000000, 0.5000000000000000000, 1.000000000000000000 ),
 ( 0.3904182756812821231, 0.3921283039710705687, 0.3938383322608589587, 0.3972583888404358499, 0.4040985019995896321, 0.4177787283178971967, 0.4451391809545123257, 0.4999364453639513206, 0.5547656701200603946, 0.5821739285757332460, 0.5958780578035696163, 0.6027301224174878014, 0.6061561547244469494, 0.6078691708779264680, 0.6095821870314059865 ),
 .UNSPECIFIED. ) 
 GEOMETRIC_REPRESENTATION_ITEM ( )  RATIONAL_B_SPLINE_SURFACE ( (
 ( 1.000000000000000000, 1.000000000000000000, 1.000000000000000000, 1.000000000000000000, 1.000000000000000000, 1.000000000000000000, 1.000000000000000000, 1.000000000000000000, 1.000000000000000000, 1.000000000000000000, 1.000000000000000000, 1.000000000000000000, 1.000000000000000000, 1.000000000000000000, 1.000000000000000000, 1.000000000000000000, 1.000000000000000000, 1.000000000000000000, 1.000000000000000000, 1.000000000000000000, 1.000000000000000000, 1.000000000000000000, 1.000000000000000000, 1.000000000000000000, 1.000000000000000000, 1.000000000000000000, 1.000000000000000000, 1.000000000000000000, 1.000000000000000000, 1.000000000000000000),
 ( 0.3333333333333333703, 0.3333333333333333703, 0.3333333333333333703, 0.3333333333333333703, 0.3333333333333333703, 0.3333333333333333703, 0.3333333333333333703, 0.3333333333333333703, 0.3333333333333333703, 0.3333333333333333703, 0.3333333333333333703, 0.3333333333333333703, 0.3333333333333333703, 0.3333333333333333703, 0.3333333333333333703, 0.3333333333333333703, 0.3333333333333333703, 0.3333333333333333703, 0.3333333333333333703, 0.3333333333333333703, 0.3333333333333333703, 0.3333333333333333703, 0.3333333333333333703, 0.3333333333333333703, 0.3333333333333333703, 0.3333333333333333703, 0.3333333333333333703, 0.3333333333333333703, 0.3333333333333333703, 0.3333333333333333703),
 ( 0.3333333333333333703, 0.3333333333333333703, 0.3333333333333333703, 0.3333333333333333703, 0.3333333333333333703, 0.3333333333333333703, 0.3333333333333333703, 0.3333333333333333703, 0.3333333333333333703, 0.3333333333333333703, 0.3333333333333333703, 0.3333333333333333703, 0.3333333333333333703, 0.3333333333333333703, 0.3333333333333333703, 0.3333333333333333703, 0.3333333333333333703, 0.3333333333333333703, 0.3333333333333333703, 0.3333333333333333703, 0.3333333333333333703, 0.3333333333333333703, 0.3333333333333333703, 0.3333333333333333703, 0.3333333333333333703, 0.3333333333333333703, 0.3333333333333333703, 0.3333333333333333703, 0.3333333333333333703, 0.3333333333333333703),
 ( 1.000000000000000000, 1.000000000000000000, 1.000000000000000000, 1.000000000000000000, 1.000000000000000000, 1.000000000000000000, 1.000000000000000000, 1.000000000000000000, 1.000000000000000000, 1.000000000000000000, 1.000000000000000000, 1.000000000000000000, 1.000000000000000000, 1.000000000000000000, 1.000000000000000000, 1.000000000000000000, 1.000000000000000000, 1.000000000000000000, 1.000000000000000000, 1.000000000000000000, 1.000000000000000000, 1.000000000000000000, 1.000000000000000000, 1.000000000000000000, 1.000000000000000000, 1.000000000000000000, 1.000000000000000000, 1.000000000000000000, 1.000000000000000000, 1.000000000000000000),
 ( 0.3333333333333333703, 0.3333333333333333703, 0.3333333333333333703, 0.3333333333333333703, 0.3333333333333333703, 0.3333333333333333703, 0.3333333333333333703, 0.3333333333333333703, 0.3333333333333333703, 0.3333333333333333703, 0.3333333333333333703, 0.3333333333333333703, 0.3333333333333333703, 0.3333333333333333703, 0.3333333333333333703, 0.3333333333333333703, 0.3333333333333333703, 0.3333333333333333703, 0.3333333333333333703, 0.3333333333333333703, 0.3333333333333333703, 0.3333333333333333703, 0.3333333333333333703, 0.3333333333333333703, 0.3333333333333333703, 0.3333333333333333703, 0.3333333333333333703, 0.3333333333333333703, 0.3333333333333333703, 0.3333333333333333703),
 ( 0.3333333333333333703, 0.3333333333333333703, 0.3333333333333333703, 0.3333333333333333703, 0.3333333333333333703, 0.3333333333333333703, 0.3333333333333333703, 0.3333333333333333703, 0.3333333333333333703, 0.3333333333333333703, 0.3333333333333333703, 0.3333333333333333703, 0.3333333333333333703, 0.3333333333333333703, 0.3333333333333333703, 0.3333333333333333703, 0.3333333333333333703, 0.3333333333333333703, 0.3333333333333333703, 0.3333333333333333703, 0.3333333333333333703, 0.3333333333333333703, 0.3333333333333333703, 0.3333333333333333703, 0.3333333333333333703, 0.3333333333333333703, 0.3333333333333333703, 0.3333333333333333703, 0.3333333333333333703, 0.3333333333333333703),
 ( 1.000000000000000000, 1.000000000000000000, 1.000000000000000000, 1.000000000000000000, 1.000000000000000000, 1.000000000000000000, 1.000000000000000000, 1.000000000000000000, 1.000000000000000000, 1.000000000000000000, 1.000000000000000000, 1.000000000000000000, 1.000000000000000000, 1.000000000000000000, 1.000000000000000000, 1.000000000000000000, 1.000000000000000000, 1.000000000000000000, 1.000000000000000000, 1.000000000000000000, 1.000000000000000000, 1.000000000000000000, 1.000000000000000000, 1.000000000000000000, 1.000000000000000000, 1.000000000000000000, 1.000000000000000000, 1.000000000000000000, 1.000000000000000000, 1.000000000000000000) ) ) 
 REPRESENTATION_ITEM ( '' )  SURFACE ( )  );
#85248 = CARTESIAN_POINT ( 'NONE',  ( -0.6823417656250003738, 8.963541667008065872, 1.181850606188754593 ) ) ;
#85250 = ORIENTED_EDGE ( 'NONE', *, *, #99914, .F. ) ;
#85251 = CARTESIAN_POINT ( 'NONE',  ( 3.809155001108742056, 1.613891119516493999, -1.025466636117925212 ) ) ;
#85252 = CARTESIAN_POINT ( 'NONE',  ( -4.471491734408701291, 4.111161866431900513, 1.214306433183764966E-14 ) ) ;
#85253 = CARTESIAN_POINT ( 'NONE',  ( 8.959240580532112475, 9.346868853575953651, -0.7998128361456221525 ) ) ;
#85254 = CARTESIAN_POINT ( 'NONE',  ( 6.883263157960362477, -0.004191378316371896506, 2.053658919477070910 ) ) ;
#85255 = CARTESIAN_POINT ( 'NONE',  ( -0.6801582343750438575, 0.1302083336747333897, -1.178068619123883165 ) ) ;
#85256 = CARTESIAN_POINT ( 'NONE',  ( 3.809477975315569864, 7.388215371269402532, -0.7216878364870197293 ) ) ;
#85257 = CARTESIAN_POINT ( 'NONE',  ( 10.99370838174331233, -6.893137084989840346, -0.3821126922044815744 ) ) ;
#85258 = CARTESIAN_POINT ( 'NONE',  ( 8.126472743488658779, 14.19519224714456840, -8.830242308825365427 ) ) ;
#85259 = CARTESIAN_POINT ( 'NONE',  ( -9.606148981167452305, -6.583980363594983842, 0.4355862708380028314 ) ) ;
#85260 = ORIENTED_EDGE ( 'NONE', *, *, #83213, .F. ) ;
#85261 = CARTESIAN_POINT ( 'NONE',  ( -1.737500000000000266, -2.158333333333331439, -3.009438278150923907 ) ) ;
#85262 = EDGE_CURVE ( 'NONE', #53136, #150774, #178153, .T. ) ;
#85263 = CARTESIAN_POINT ( 'NONE',  ( 3.391731324245280010, -0.7611128710301139355, 1.708892184765831157 ) ) ;
#85264 = CARTESIAN_POINT ( 'NONE',  ( -6.717278222822391953, -7.473374494058216300, 6.830415307812263137 ) ) ;
#85265 = CIRCLE ( 'NONE', #61008, 6.200000000000000178 ) ;
#85266 = CARTESIAN_POINT ( 'NONE',  ( 0.000000000000000000, 8.500000000000000000, 0.000000000000000000 ) ) ;
#85267 = CARTESIAN_POINT ( 'NONE',  ( -6.073689629242158716, 9.069426419882418600, -1.082531754730538864 ) ) ;
#85269 = CARTESIAN_POINT ( 'NONE',  ( 0.05278957052760185897, 0.3289079202175131389, 1.883742972368242174 ) ) ;
#85268 = MECHANICAL_DESIGN_GEOMETRIC_PRESENTATION_REPRESENTATION (  '', ( #74926 ), #81873 ) ;
#85270 = CARTESIAN_POINT ( 'NONE',  ( 3.635557746758808495, 7.393234471193928847, -0.7998128361456291469 ) ) ;
#85271 = CARTESIAN_POINT ( 'NONE',  ( 0.6550501802922055195, 1.640498656168420943, -1.089389633329050033 ) ) ;
#85272 = CARTESIAN_POINT ( 'NONE',  ( 1.353138909097661768, 0.1455122274086443901, -2.011206940682720212 ) ) ;
#85273 = CARTESIAN_POINT ( 'NONE',  ( -8.890396042259075315, 11.39521468743417998, -1.599625672291263179 ) ) ;
#85274 = CARTESIAN_POINT ( 'NONE',  ( 5.668190738965027897, 8.770583741171307679, -1.199719254218452047 ) ) ;
#85275 =( NAMED_UNIT ( * ) PLANE_ANGLE_UNIT ( ) SI_UNIT ( $, .RADIAN. ) );
#85276 = CARTESIAN_POINT ( 'NONE',  ( 1.394752248596371702, 1.789971953256053627, -1.264032476404143512 ) ) ;
#85277 = CARTESIAN_POINT ( 'NONE',  ( 6.692070433991195166, -0.7751425012093198230, 1.651373049820707317 ) ) ;
#85278 = CARTESIAN_POINT ( 'NONE',  ( -3.785751206713858785, 5.439795712631356750, 1.599625672291267398 ) ) ;
#85279 = EDGE_CURVE ( 'NONE', #158010, #202349, #48679, .T. ) ;
#85280 = CARTESIAN_POINT ( 'NONE',  ( 4.529832720741620022, 7.338536369956936589, -1.082531754730548412 ) ) ;
#85281 = CARTESIAN_POINT ( 'NONE',  ( 10.09812548408005384, 10.67556790771522124, -0.7998128361456281477 ) ) ;
#85282 = CARTESIAN_POINT ( 'NONE',  ( 4.542145155778077203, 5.257923088951247159, -1.199719254218452047 ) ) ;
#85283 = CARTESIAN_POINT ( 'NONE',  ( 2.905190055078214595, 6.611415174225076186, 0.7998128361456271485 ) ) ;
#85284 = EDGE_LOOP ( 'NONE', ( #163882, #187306, #112248, #125825, #38294, #67961, #67644 ) ) ;
#85286 = CARTESIAN_POINT ( 'NONE',  ( 0.8736902326584498057, 0.3905749221770152269, -1.974679160882378826 ) ) ;
#85285 = CARTESIAN_POINT ( 'NONE',  ( 3.491602800004707241, -1.839307750763185645, -0.08696504193297231733 ) ) ;
#85287 = CARTESIAN_POINT ( 'NONE',  ( 2.196985159075715011, -1.500492831465898513, -1.741107174271120384 ) ) ;
#85289 = CARTESIAN_POINT ( 'NONE',  ( 0.7778919621034340315, -0.9889961724188134351, -1.576189065804904477 ) ) ;
#85288 = CARTESIAN_POINT ( 'NONE',  ( 4.365362273920252889, 4.195270195769483124, 0.7216878364870317197 ) ) ;
#85290 = CARTESIAN_POINT ( 'NONE',  ( -3.475000000000000533, -0.6999999999999992895, 0.000000000000000000 ) ) ;
#85291 = CARTESIAN_POINT ( 'NONE',  ( -5.199715606040888005, 6.025088614257851027, -1.199719254218446718 ) ) ;
#85292 = DIRECTION ( 'NONE',  ( 1.000000000000000000, -5.391474854832587087E-16, 0.000000000000000000 ) ) ;
#85293 = CARTESIAN_POINT ( 'NONE',  ( 4.341997288149157086, -1.180789491531178292, -1.504210074635865757 ) ) ;
#85294 = CARTESIAN_POINT ( 'NONE',  ( -8.459397779922852578, 11.95671561229694824, 1.199719254218453823 ) ) ;
#85295 = CARTESIAN_POINT ( 'NONE',  ( 6.321627859881460587, 6.858947107989728842, -0.6823232096292205506 ) ) ;
#85296 = CARTESIAN_POINT ( 'NONE',  ( -7.268579750702168774, 7.652633595340216921, -0.7216878364870338292 ) ) ;
#85298 = CARTESIAN_POINT ( 'NONE',  ( 2.342468781959532453, 0.4075140148256419792, 1.825566309089213579 ) ) ;
#85297 = CARTESIAN_POINT ( 'NONE',  ( 4.230081496780574213, 2.050754116127400106, 0.4060544076584340356 ) ) ;
#85299 = CARTESIAN_POINT ( 'NONE',  ( 8.026063749610047537, 10.38682701267698150, -1.443375672974057666 ) ) ;
#85300 = CARTESIAN_POINT ( 'NONE',  ( 1.364683531249992088, 5.696875000341418804, 1.214306433183764966E-14 ) ) ;
#85301 = CARTESIAN_POINT ( 'NONE',  ( 3.298151293307958642, 1.369808456162135091, -1.073517941977668588 ) ) ;
#85302 = CARTESIAN_POINT ( 'NONE',  ( 3.497113557321089861, 6.167384019261527683, -1.199719254218446718 ) ) ;
#85304 = CARTESIAN_POINT ( 'NONE',  ( 4.761938266897790761, 6.578680616179308771, 1.599625672291267398 ) ) ;
#85303 = CARTESIAN_POINT ( 'NONE',  ( -1.500000000000015099, 11.51041666734946567, -0.8660254037844309360 ) ) ;
#85305 = CARTESIAN_POINT ( 'NONE',  ( 3.984733165684080092, -0.1715787546078418324, -1.716317334075837975 ) ) ;
#85306 = CARTESIAN_POINT ( 'NONE',  ( -7.874588291438845644, 8.081441182967111558, -0.7998128361456291469 ) ) ;
#85307 = CARTESIAN_POINT ( 'NONE',  ( 3.790727848299980440, 1.850687065220711469, -1.173560875862532660 ) ) ;
#85308 = CARTESIAN_POINT ( 'NONE',  ( 6.721333373144884327, -0.1645177889858795151, 2.170883633896856679 ) ) ;
#85309 = CARTESIAN_POINT ( 'NONE',  ( 0.4019237886466816012, 8.676335450315372455, -1.499999999999998668 ) ) ;
#85310 =( BOUNDED_CURVE ( )  B_SPLINE_CURVE ( 2, ( #151580, #98558, #135336, #16204, #66011, #83349, #18349 ),
 .UNSPECIFIED., .F., .T. ) 
 B_SPLINE_CURVE_WITH_KNOTS ( ( 3, 2, 2, 3 ),
 ( 0.1607142857142856152, 0.1666666666666666297, 0.1726190476190476719, 0.1785714285714287142 ),
 .UNSPECIFIED. ) 
 CURVE ( )  GEOMETRIC_REPRESENTATION_ITEM ( )  RATIONAL_B_SPLINE_CURVE ( ( 1.000000000000002442, 0.8660254037844361541, 1.000000000000000000, 0.8660254037844387076, 1.000000000000000000, 0.8660254037844355990, 1.000000000000003109 ) ) 
 REPRESENTATION_ITEM ( '' )  );
#85311 = CARTESIAN_POINT ( 'NONE',  ( 9.578932859269645661, -9.985077769980609474, -0.1209251627559674580 ) ) ;
#85312 = CARTESIAN_POINT ( 'NONE',  ( 3.467796559821629820, -0.4283512159202977343, 2.128237193570106101 ) ) ;
#85313 = CARTESIAN_POINT ( 'NONE',  ( 2.262075381241589245, 0.7800679334904643270, 1.650788133108482825 ) ) ;
#85314 = CARTESIAN_POINT ( 'NONE',  ( -1.420000000000021911, 6.216000000000048153, 2.921333333333346882 ) ) ;
#85315 = CARTESIAN_POINT ( 'NONE',  ( 6.157425464982741126, 2.025529447029483343, -0.6166105444416707382 ) ) ;
#85316 = EDGE_CURVE ( 'NONE', #149695, #179985, #114447, .T. ) ;
#85317 = ORIENTED_EDGE ( 'NONE', *, *, #23681, .F. ) ;
#85319 = CARTESIAN_POINT ( 'NONE',  ( -1.364683531249997417, 3.071875000341423245, 1.214306433183764966E-14 ) ) ;
#85318 = CARTESIAN_POINT ( 'NONE',  ( 5.847306917912500346, 0.6688746937079934618, -2.192647164702413498 ) ) ;
#85320 = CARTESIAN_POINT ( 'NONE',  ( 9.215791728987056786, 11.77484298861683598, -1.599625672291262513 ) ) ;
#85321 = CARTESIAN_POINT ( 'NONE',  ( 1.295735140135088281, 1.957893036122235531, -0.8148005001323217478 ) ) ;
#85322 = CARTESIAN_POINT ( 'NONE',  ( -4.934804725694224459, 6.780358151441803649, -1.443375672974053447 ) ) ;
#85323 = CARTESIAN_POINT ( 'NONE',  ( 3.768803514918948938, 4.459654191235965293, -1.082531754730543083 ) ) ;
#85324 = CARTESIAN_POINT ( 'NONE',  ( -5.544921637864838715, 6.531792001339513654, -1.082531754730543971 ) ) ;
#85326 = CARTESIAN_POINT ( 'NONE',  ( -0.7500000000000179856, 12.57291666734946389, 1.299038105676658228 ) ) ;
#85325 = CARTESIAN_POINT ( 'NONE',  ( -1.902435570468859805, 0.6170404364503311312, 0.9487424039605132364 ) ) ;
#85328 = VERTEX_POINT ( 'NONE', #153043 ) ;
#85327 = CARTESIAN_POINT ( 'NONE',  ( 1.190412498926897600, 1.327076764020938882, 1.781161496267854361 ) ) ;
#85329 = CARTESIAN_POINT ( 'NONE',  ( 5.906875006520014182, -1.122496024291631755, -1.674889250513518446 ) ) ;
#85331 = CARTESIAN_POINT ( 'NONE',  ( 3.889554661416291026, -1.907601829641421887, 0.7848441205193229520 ) ) ;
#85330 = CARTESIAN_POINT ( 'NONE',  ( 5.684946482831785275, 5.526859072925533134, -0.7998128361456231517 ) ) ;
#85333 = CARTESIAN_POINT ( 'NONE',  ( -0.2409995289980038091, 6.947781193150415646, -2.595509233728268583 ) ) ;
#85332 = CARTESIAN_POINT ( 'NONE',  ( 7.015418140428412386, 7.149352350113456822, 0.7998128361456331437 ) ) ;
#85334 = ADVANCED_FACE ( 'NONE', ( #67487 ), #65942, .T. ) ;
#85335 = CARTESIAN_POINT ( 'NONE',  ( 6.713222337422018349, 7.861122810861019161, -1.199719254218452047 ) ) ;
#85336 = CARTESIAN_POINT ( 'NONE',  ( 3.285556943750000514, -2.063541666188710266, 1.896917185911906500 ) ) ;
#85337 = CARTESIAN_POINT ( 'NONE',  ( 0.1329588055935760349, 7.629137130509077380, -2.445925914280167923 ) ) ;
#85338 = CARTESIAN_POINT ( 'NONE',  ( 0.4629771330677232011, 0.2027323353172970355, -2.080777175944429125 ) ) ;
#85339 = CARTESIAN_POINT ( 'NONE',  ( 5.238907797441370029, 2.013986022392059816, -0.1017483359899013229 ) ) ;
#85340 = CARTESIAN_POINT ( 'NONE',  ( 4.845164456061270997, 0.5726227986864868003, -1.750029900461601340 ) ) ;
#85341 = EDGE_CURVE ( 'NONE', #22516, #3330, #6168, .T. ) ;
#85342 = CARTESIAN_POINT ( 'NONE',  ( 4.981731378017507872, 7.899438143407371271, -1.199719254218452047 ) ) ;
#85343 = CARTESIAN_POINT ( 'NONE',  ( 1.201696739578085982, -1.724958192343982510, -0.005827584801694830549 ) ) ;
#85344 = CARTESIAN_POINT ( 'NONE',  ( 0.02267320670834571672, 0.3494893071277604402, 1.985867805234131644 ) ) ;
#85345 = CARTESIAN_POINT ( 'NONE',  ( 1.143681411288837824, 0.9377895679426456743, 2.098875006570381618 ) ) ;
#85346 = CARTESIAN_POINT ( 'NONE',  ( -6.735703387890906946, 6.752742128827836865, -0.7998128361456291469 ) ) ;
#85347 = CARTESIAN_POINT ( 'NONE',  ( 1.089599759544016999, 1.994953948513054742, -1.067007742874733545 ) ) ;
#85348 = CARTESIAN_POINT ( 'NONE',  ( 3.369845833479632180, 2.054674681345913800, -0.4616683548303905926 ) ) ;
#85349 = CARTESIAN_POINT ( 'NONE',  ( -5.581116510680924847, 6.540332679663050541, -1.199719254218453823 ) ) ;
#85350 = CARTESIAN_POINT ( 'NONE',  ( 6.564118927310645724, 10.80988918183778225, -0.7998128361456291469 ) ) ;
#85351 = CARTESIAN_POINT ( 'NONE',  ( 6.333067150914808430, 8.481940657524365434, 1.443375672974063439 ) ) ;
#85352 = CARTESIAN_POINT ( 'NONE',  ( 0.000000000000000000, 0.000000000000000000, -1.999999999999999556 ) ) ;
#85353 = CARTESIAN_POINT ( 'NONE',  ( -6.423865854776591000, 6.388931673527803667, 1.040834085586084257E-14 ) ) ;
#85354 = CARTESIAN_POINT ( 'NONE',  ( 7.090551149822739596, 8.335026431957096804, 1.082531754730558626 ) ) ;
#85355 = CARTESIAN_POINT ( 'NONE',  ( 5.079507498475252625, 6.736975590279616455, 1.417308049988776020 ) ) ;
#85356 = CARTESIAN_POINT ( 'NONE',  ( -2.625475302540713152, 6.214804952939456228, -0.7998128361456281477 ) ) ;
#85357 = CARTESIAN_POINT ( 'NONE',  ( 5.431947826915617838, -2.167270271666811077, 0.4867340719418070671 ) ) ;
#85358 = CARTESIAN_POINT ( 'NONE',  ( 3.011879173929287390, -1.080601074572758558, -1.906429682232862577 ) ) ;
#85359 = CARTESIAN_POINT ( 'NONE',  ( -3.764360206088648297, 7.543504007078730922, -0.7998128361456281477 ) ) ;
#85360 = CARTESIAN_POINT ( 'NONE',  ( -2.810282979782591006, 6.500690253046801814, 0.000000000000000000 ) ) ;
#85361 = CARTESIAN_POINT ( 'NONE',  ( 5.600043156098196917, 0.7966083592686534764, -1.793046234938546757 ) ) ;
#85362 = CARTESIAN_POINT ( 'NONE',  ( -1.364683531250014514, 1.988541667008086655, -0.7879004041258289570 ) ) ;
#85363 = CARTESIAN_POINT ( 'NONE',  ( 6.610000000000014531, 2.942932264094192174, 2.732153830519419291 ) ) ;
#85365 = VERTEX_POINT ( 'NONE', #84837 ) ;
#85364 = CARTESIAN_POINT ( 'NONE',  ( -3.782361668532609134, 7.356579680022602652, 1.040834085586084257E-14 ) ) ;
#85366 = CARTESIAN_POINT ( 'NONE',  ( 4.640951271726033056, 2.030106984047326701, 0.6129599860185754867 ) ) ;
#85367 = CARTESIAN_POINT ( 'NONE',  ( -5.750066545971566079, 8.762142499391876171, 1.082531754730550855 ) ) ;
#85368 = VERTEX_POINT ( 'NONE', #2488 ) ;
#85370 = CARTESIAN_POINT ( 'NONE',  ( 6.614160618316515361, -1.014195557614630205, -1.909021090911746654 ) ) ;
#85369 = CARTESIAN_POINT ( 'NONE',  ( -4.990809943606269172, 8.836712344267034780, -0.7216878364870338292 ) ) ;
#85371 = CARTESIAN_POINT ( 'NONE',  ( 4.157546660884947620, 8.002221537674429896, 1.040834085586084257E-14 ) ) ;
#85372 = CARTESIAN_POINT ( 'NONE',  ( 5.003375819710620398, -1.831856422778654681, 0.1858995714831001289 ) ) ;
#85373 = CARTESIAN_POINT ( 'NONE',  ( 0.000000000000000000, 7.000000000000000000, 0.000000000000000000 ) ) ;
#85374 = CARTESIAN_POINT ( 'NONE',  ( 1.364683531249988535, 3.426041667008085323, 0.7879004041258500513 ) ) ;
#85375 = CARTESIAN_POINT ( 'NONE',  ( 1.381927130872797838, -0.2546507840628647878, -1.721584071012570050 ) ) ;
#85376 = CARTESIAN_POINT ( 'NONE',  ( 11.49978884755350172, 12.35729178837194375, 3.429452816445248242 ) ) ;
#85377 = CARTESIAN_POINT ( 'NONE',  ( -1.364683531250014514, -0.6989583329919100141, -0.7879004041258359514 ) ) ;
#85378 = CYLINDRICAL_SURFACE ( 'NONE', #163701, 0.08000000000000020983 ) ;
#85379 = CARTESIAN_POINT ( 'NONE',  ( 5.524359596833869013, 1.291058806671550485, -1.733668313432787933 ) ) ;
#85380 = CARTESIAN_POINT ( 'NONE',  ( -3.460355519985875983, 5.060167411448709629, 1.599625672291267398 ) ) ;
#85381 = CARTESIAN_POINT ( 'NONE',  ( -7.998947441938374148, 8.434452891790657603, 1.040834085586084257E-14 ) ) ;
#85382 = CARTESIAN_POINT ( 'NONE',  ( 4.504844740329728481, 1.672958716126593082, -1.369014088531981255 ) ) ;
#85383 = CARTESIAN_POINT ( 'NONE',  ( 1.364683531249988535, 2.905208333674754506, -0.7879004041258239610 ) ) ;
#85384 = CARTESIAN_POINT ( 'NONE',  ( 4.745367521161733215, -1.522072814771213922, -1.252777155790285590 ) ) ;
#85385 = CARTESIAN_POINT ( 'NONE',  ( 3.567500862290486019, 1.367785175758473581, -1.065411925293987760 ) ) ;
#85386 = CARTESIAN_POINT ( 'NONE',  ( 1.013517375116283592, -2.137022957946862700, 0.4851717564131745597 ) ) ;
#85387 = CARTESIAN_POINT ( 'NONE',  ( 2.485774399949276070, 2.109797628256422364, -0.9350972159218959856 ) ) ;
#85388 = CARTESIAN_POINT ( 'NONE',  ( 4.991509756128800213, 1.524171611017493655, 1.387147876433484806 ) ) ;
#85389 = CARTESIAN_POINT ( 'NONE',  ( 6.374560617330069512, -0.09999853314933374038, -1.939619642457596660 ) ) ;
#85390 = CARTESIAN_POINT ( 'NONE',  ( -5.870317324592805086, 9.792527945426188651, -0.7216878364870197293 ) ) ;
#85391 = CARTESIAN_POINT ( 'NONE',  ( -5.991777542596674166, 5.955104985976372944, 0.000000000000000000 ) ) ;
#85392 = DIRECTION ( 'NONE',  ( -0.5131086435338325646, -0.8583236685137316524, 4.218847493575600376E-15 ) ) ;
#85393 = CARTESIAN_POINT ( 'NONE',  ( 1.002577532868035526, -1.966644254196001196, 0.4445047019146358691 ) ) ;
#85394 = CARTESIAN_POINT ( 'NONE',  ( -5.680503174001480637, 9.571078103069643461, 0.7216878364870458196 ) ) ;
#85395 = CARTESIAN_POINT ( 'NONE',  ( 3.803933094734159415, -0.6430795383850876901, 2.110982628114480786 ) ) ;
#85396 = CARTESIAN_POINT ( 'NONE',  ( -3.285556943750000514, -1.976041666188710577, -1.896917185911906500 ) ) ;
#85397 = CARTESIAN_POINT ( 'NONE',  ( 1.270090995528074362, -0.8302864195119415980, -1.665510012463662148 ) ) ;
#85398 = CARTESIAN_POINT ( 'NONE',  ( 1.355395447572484313, 3.764859155812621871, -0.6425755019599879159 ) ) ;
#85399 = CARTESIAN_POINT ( 'NONE',  ( -7.720982897393583677, -6.134628647623485698, 7.834948825496934610 ) ) ;
#85400 = CARTESIAN_POINT ( 'NONE',  ( 2.744865908132018362, 2.962146155648302415, -2.500000000000000888 ) ) ;
#85403 = CIRCLE ( 'NONE', #19682, 1.600000000000005196 ) ;
#85402 = CARTESIAN_POINT ( 'NONE',  ( 6.825078400183575589, -0.005632053428735600553, 2.144262460745151255 ) ) ;
#85401 = CARTESIAN_POINT ( 'NONE',  ( -5.577377183731011101, 7.510248947172004641, -1.348340355397449342 ) ) ;
#85404 = CARTESIAN_POINT ( 'NONE',  ( 6.193280126971262511, -0.6156851667328180344, 1.735278506779000640 ) ) ;
#85405 = ORIENTED_EDGE ( 'NONE', *, *, #193355, .F. ) ;
#85406 = CARTESIAN_POINT ( 'NONE',  ( 2.887629844759795450, 1.456389637235107948, 1.458414562493230759 ) ) ;
#85407 = CARTESIAN_POINT ( 'NONE',  ( -1.360316468750007779, 2.390625000341400685, -1.734723475976807094E-15 ) ) ;
#85408 = CARTESIAN_POINT ( 'NONE',  ( -5.585069213825653023, 8.603332285183535433, -1.199719254218440723 ) ) ;
#85409 = CARTESIAN_POINT ( 'NONE',  ( 2.227218753574769838, 1.805135905798272100, 0.9059672028350268524 ) ) ;
#85411 = EDGE_CURVE ( 'NONE', #157333, #178508, #172766, .T. ) ;
#85410 = CARTESIAN_POINT ( 'NONE',  ( -1.402160292154681736E-14, -0.5374999999999753308, 1.732050807568877637 ) ) ;
#85412 = CARTESIAN_POINT ( 'NONE',  ( 3.174580523894166006, 6.855427711185178019, 0.7998128361456341429 ) ) ;
#85413 = CARTESIAN_POINT ( 'NONE',  ( 2.289980725320222010, -0.8822103741390595610, 1.862666789336121509 ) ) ;
#85415 = CARTESIAN_POINT ( 'NONE',  ( -0.6823417656250039265, 12.81770833367473017, -1.181850606188755259 ) ) ;
#85414 = CARTESIAN_POINT ( 'NONE',  ( -5.219525951136881226, 5.191794485855505847, -0.7216878364870058515 ) ) ;
#85416 = CARTESIAN_POINT ( 'NONE',  ( 4.645640190976921602, 8.571663989448405019, 1.040834085586084257E-14 ) ) ;
#85417 = CARTESIAN_POINT ( 'NONE',  ( -0.2409995289980246258, 7.629137130509076492, -2.600476469121239198 ) ) ;
#85418 = CARTESIAN_POINT ( 'NONE',  ( 5.250674450588199704, 0.6379336648693231249, 2.112661011922472021 ) ) ;
#85419 = CARTESIAN_POINT ( 'NONE',  ( 6.038177310039780643, 8.137902509836795417, -1.599625672291283607 ) ) ;
#85420 = CARTESIAN_POINT ( 'NONE',  ( 1.124558466181435179, 1.288545020775376804, -1.735378439385642180 ) ) ;
#85421 = CARTESIAN_POINT ( 'NONE',  ( -4.934804725694224459, 6.780358151441803649, -1.443375672974053447 ) ) ;
#85422 = CARTESIAN_POINT ( 'NONE',  ( 2.413296319342159713, -1.879803466158457059, 0.7303082167480907660 ) ) ;
#85423 = CARTESIAN_POINT ( 'NONE',  ( 2.249760294480507294, -2.253934603285558502, -0.4491563171437322199 ) ) ;
#85424 = CARTESIAN_POINT ( 'NONE',  ( -4.281741921268227280, 3.985524603254129605, 0.2951291498071085262 ) ) ;
#85425 = CARTESIAN_POINT ( 'NONE',  ( 0.4263524580605422276, 1.788790299270696993, 0.5473224044415525569 ) ) ;
#85426 = CARTESIAN_POINT ( 'NONE',  ( 1.843739406749228538, 8.920000000000001705, -0.7749999999999996891 ) ) ;
#85427 = CARTESIAN_POINT ( 'NONE',  ( 1.938157646728836614, 1.849873822469105145, 0.2772664081076986475 ) ) ;
#85428 =( GEOMETRIC_REPRESENTATION_CONTEXT ( 3 ) GLOBAL_UNCERTAINTY_ASSIGNED_CONTEXT ( ( #102698 ) ) GLOBAL_UNIT_ASSIGNED_CONTEXT ( ( #111481, #147129, #12821 ) ) REPRESENTATION_CONTEXT ( 'NONE', 'WORKASPACE' ) );
#85429 = CARTESIAN_POINT ( 'NONE',  ( 3.116422982138194353, 1.968445132739887748, 0.4370783100892047801 ) ) ;
#85431 = CARTESIAN_POINT ( 'NONE',  ( 11.44786932348564079, 13.79999999999998295, 3.303370173849796032 ) ) ;
#85430 = CARTESIAN_POINT ( 'NONE',  ( -1.201851678989727383E-14, 2.571875000341417472, 1.575800808251672791 ) ) ;
#85433 = CARTESIAN_POINT ( 'NONE',  ( 5.303390785913836503, 1.721067984382893545, 1.213575365270858075 ) ) ;
#85432 = CARTESIAN_POINT ( 'NONE',  ( -6.690058733339450114, 9.892486724616283311, 1.199719254218452047 ) ) ;
#85434 = CARTESIAN_POINT ( 'NONE',  ( 5.635385404774530649, 9.726366738878972740, 0.7998128361456462443 ) ) ;
#85435 = CARTESIAN_POINT ( 'NONE',  ( -6.191269702934848240, 10.37489842006599616, 0.000000000000000000 ) ) ;
#85436 = CARTESIAN_POINT ( 'NONE',  ( 3.867349521082877217, 7.341814853893565918, 0.5856213828667733434 ) ) ;
#85437 = CARTESIAN_POINT ( 'NONE',  ( 5.748308766347858700, 0.9917722086787251756, -1.759414076857076514 ) ) ;
#85438 = CARTESIAN_POINT ( 'NONE',  ( 1.499999999999987121, -0.4645833326505149907, 0.8660254037844524744 ) ) ;
#85439 = CARTESIAN_POINT ( 'NONE',  ( 0.3563950589157930393, -2.062029646941070382, -0.05432448973826872057 ) ) ;
#85440 = CARTESIAN_POINT ( 'NONE',  ( 8.812436659202669276, 10.34389285956704363, -1.082531754730543083 ) ) ;
#85441 = CARTESIAN_POINT ( 'NONE',  ( 5.006703865196457492, 9.063181286029688977, 0.000000000000000000 ) ) ;
#85442 = CARTESIAN_POINT ( 'NONE',  ( 6.574778147984297938, 6.635272358928617997, -0.7998128361456481317 ) ) ;
#85443 = CARTESIAN_POINT ( 'NONE',  ( -1.364683531250000748, 0.8218750003414210248, 0.000000000000000000 ) ) ;
#85445 = CARTESIAN_POINT ( 'NONE',  ( 8.845566791370190529, 3.603011019375345736, 7.955782632700100443 ) ) ;
#85444 = CARTESIAN_POINT ( 'NONE',  ( 5.713835393516482952, 5.630839145382857680, 0.7998128361456352531 ) ) ;
#85446 = CARTESIAN_POINT ( 'NONE',  ( 8.554831740098663317, 9.082984572977682802, 0.7216878364870458196 ) ) ;
#85448 = FACE_OUTER_BOUND ( 'NONE', #134192, .T. ) ;
#85447 = CARTESIAN_POINT ( 'NONE',  ( 3.174467775116470936, -1.067885509202262773, -1.890316989176257234 ) ) ;
#85450 = CARTESIAN_POINT ( 'NONE',  ( 1.698526806778306586, 1.531337151408303621, 1.022036240780115346 ) ) ;
#85449 = CARTESIAN_POINT ( 'NONE',  ( -3.768803514918943609, 7.340761834139994058, 0.7216878364870317197 ) ) ;
#85451 = CARTESIAN_POINT ( 'NONE',  ( 0.6823417656249882723, 2.926041667008084879, -1.181850606188754593 ) ) ;
#85452 = CARTESIAN_POINT ( 'NONE',  ( 4.177398808104064720, 1.432170664236757540, 1.658919600136643524 ) ) ;
#85453 = CARTESIAN_POINT ( 'NONE',  ( 6.883263157960367806, 2.959656548886806071, 2.506466465954690914 ) ) ;
#85454 = CARTESIAN_POINT ( 'NONE',  ( 5.225545412997908201, -2.150153479602398221, 0.7043797957921889008 ) ) ;
#85455 = CARTESIAN_POINT ( 'NONE',  ( -5.357443255694392725, 9.402100898285455699, 0.000000000000000000 ) ) ;
#85456 = CARTESIAN_POINT ( 'NONE',  ( -1.364683531250010295, 5.592708333674750953, 0.7879004041258379498 ) ) ;
#85457 = CARTESIAN_POINT ( 'NONE',  ( 4.915098833515745724, 8.004322973991836676, -0.9888141558981374812 ) ) ;
#85458 = CARTESIAN_POINT ( 'NONE',  ( 1.499999999999997113, 13.64583333333332860, -0.8660254037844378194 ) ) ;
#85459 = CARTESIAN_POINT ( 'NONE',  ( -6.631346530415505036, 7.869564052640446228, 1.082531754730549078 ) ) ;
#85460 = CARTESIAN_POINT ( 'NONE',  ( 3.282482588284323821, 6.843663763058119187, 0.7216878364870257245 ) ) ;
#85461 = CARTESIAN_POINT ( 'NONE',  ( 5.993352163831329626, 1.341162022463908032, 1.154712335393495160 ) ) ;
#85462 = CARTESIAN_POINT ( 'NONE',  ( 8.471147050440139381, 8.777426401801974976, -0.7998128361456281477 ) ) ;
#85463 = CARTESIAN_POINT ( 'NONE',  ( 2.046058472223175162, 0.8067420340923843192, -1.945513702063914163 ) ) ;
#85465 = CARTESIAN_POINT ( 'NONE',  ( -0.7500000000000006661, 2.108333333333357817, -1.299038105676652011 ) ) ;
#85464 = CARTESIAN_POINT ( 'NONE',  ( 0.6823417656249934904, 11.94270833367473017, 1.181850606188764807 ) ) ;
#85466 = CARTESIAN_POINT ( 'NONE',  ( 1.521857752106166695, 1.940948540861246352, -0.3334180107718246466 ) ) ;
#85467 = CARTESIAN_POINT ( 'NONE',  ( 0.09234973940512071489, -0.4041859633337717694, -1.833079292876439670 ) ) ;
#85468 = CARTESIAN_POINT ( 'NONE',  ( 0.8011316787140990714, -1.684513426579350659, 1.005393624328714264 ) ) ;
#85470 = ORIENTED_EDGE ( 'NONE', *, *, #140696, .T. ) ;
#85469 = CARTESIAN_POINT ( 'NONE',  ( 0.2285749388857594433, 1.317234250586714284, -1.386657971642536014 ) ) ;
#85471 = CARTESIAN_POINT ( 'NONE',  ( 5.490689023854504747, 9.349628261231513804, 1.040834085586084257E-14 ) ) ;
#85472 = CIRCLE ( 'NONE', #47458, 1.500000000000000222 ) ;
#85473 = CARTESIAN_POINT ( 'NONE',  ( 1.364683531249986537, 0.1760416670080860446, 0.7879004041258500513 ) ) ;
#85474 = EDGE_CURVE ( 'NONE', #50054, #46947, #71762, .T. ) ;
#85475 = CARTESIAN_POINT ( 'NONE',  ( 6.368025811218641863, 0.9635043244729593059, 1.603280169136585220 ) ) ;
#85476 = CARTESIAN_POINT ( 'NONE',  ( 2.758194185376297902, 5.305311418659259814, 1.199719254218452047 ) ) ;
#85477 = CARTESIAN_POINT ( 'NONE',  ( 8.846456096353175980, 0.9706168436483472162, 7.965384846859531187 ) ) ;
#85478 = VERTEX_POINT ( 'NONE', #189801 ) ;
#85479 = CARTESIAN_POINT ( 'NONE',  ( 5.911005882915713272, -1.635593682349820499, 1.269112435710928688 ) ) ;
#85480 = CARTESIAN_POINT ( 'NONE',  ( -1.225000000000014300, 2.750000000000002665, -3.469446951953614189E-14 ) ) ;
#85481 = CARTESIAN_POINT ( 'NONE',  ( -4.245111494410291897, 7.006361605903701495, 1.082531754730549967 ) ) ;
#85482 = CARTESIAN_POINT ( 'NONE',  ( 0.8710647801728804707, -0.9715519045938938447, 3.328597978068449148 ) ) ;
#85483 = CARTESIAN_POINT ( 'NONE',  ( -1.402160292154681736E-14, 0.08750000000001964540, -1.732050807568870754 ) ) ;
#85484 = CARTESIAN_POINT ( 'NONE',  ( 8.938903350111612411, 9.323142084752035430, -0.7998128361456221525 ) ) ;
#85485 = CARTESIAN_POINT ( 'NONE',  ( -8.666686507633592385, 11.13422023037111330, 1.599625672291269396 ) ) ;
#85486 = CARTESIAN_POINT ( 'NONE',  ( 7.191674137406095291, 7.354984346587396082, 0.000000000000000000 ) ) ;
#85487 = CARTESIAN_POINT ( 'NONE',  ( 1.364683531249986537, 0.6552083336747522857, -0.7879004041258239610 ) ) ;
#85488 = CARTESIAN_POINT ( 'NONE',  ( 0.7499999999999885647, 0.8166666666666877461, -1.299038105676652899 ) ) ;
#85490 = CARTESIAN_POINT ( 'NONE',  ( 5.172599298813543633, 5.993452922492633839, -1.199719254218452047 ) ) ;
#85489 = CARTESIAN_POINT ( 'NONE',  ( 5.529730448059603454, 1.891198321494348633, -0.5216162335564683561 ) ) ;
#85491 = CARTESIAN_POINT ( 'NONE',  ( 3.602888598310006074, 0.9090057795711030675, -1.799647124144133858 ) ) ;
#85492 = CARTESIAN_POINT ( 'NONE',  ( 2.237376970375870577, 0.5068087052534899772, -1.847417656071285608 ) ) ;
#85493 = CARTESIAN_POINT ( 'NONE',  ( -1.874158809982213958, 3.299964346911606228, -0.4000000000000374922 ) ) ;
#85494 = CARTESIAN_POINT ( 'NONE',  ( 0.4510473619779230003, -1.854578567552306767, -1.167393260480112493 ) ) ;
#85495 = FACE_OUTER_BOUND ( 'NONE', #208163, .T. ) ;
#85496 = CARTESIAN_POINT ( 'NONE',  ( 2.758895227446885645, -1.625506345271657604, -0.9254698705311248386 ) ) ;
#85497 = CARTESIAN_POINT ( 'NONE',  ( -1.500000000000001332, -0.8187499993171781787, 0.000000000000000000 ) ) ;
#85498 = CARTESIAN_POINT ( 'NONE',  ( -6.347188469492005325, 10.55680364771601809, -0.7998128361456291469 ) ) ;
#85500 = CARTESIAN_POINT ( 'NONE',  ( 4.183301248788100501, 1.701634275673917784, 1.259637755991403374 ) ) ;
#85499 = CARTESIAN_POINT ( 'NONE',  ( -5.910991785878175975, 6.958873840688411860, -1.082531754730544860 ) ) ;
#85501 = LINE ( 'NONE', #102828, #128801 ) ;
#85502 = CARTESIAN_POINT ( 'NONE',  ( 6.478973898625433492, 1.930320082341809629, 0.7489585856828018251 ) ) ;
#85504 = CARTESIAN_POINT ( 'NONE',  ( 6.720655732516649827, 4.686306134629722564, 2.836255308917837947 ) ) ;
#85503 = CARTESIAN_POINT ( 'NONE',  ( 0.8024204784428441428, 1.580594792060415088, -1.368634514759473397 ) ) ;
#85506 = ORIENTED_EDGE ( 'NONE', *, *, #59177, .T. ) ;
#85505 = CARTESIAN_POINT ( 'NONE',  ( 6.792070425361753649, -0.7769146798779454910, 1.650438213995283565 ) ) ;
#85507 = ADVANCED_FACE ( 'NONE', ( #23013 ), #140022, .F. ) ;
#85508 = CARTESIAN_POINT ( 'NONE',  ( 6.401421083946654100, 10.62007503124645957, -0.7998128361456291469 ) ) ;
#85509 = DIRECTION ( 'NONE',  ( -5.578564026256490882E-16, -1.000000000000000000, -9.066213480720158442E-32 ) ) ;
#85510 = SURFACE_STYLE_USAGE ( .BOTH. , #115943 ) ;
#85511 = CARTESIAN_POINT ( 'NONE',  ( 7.253248993186735660, 7.564471368247083660, 0.7216878364870317197 ) ) ;
#85512 = CARTESIAN_POINT ( 'NONE',  ( -1.402160292154681736E-14, 12.98437500034139980, 1.575800808251682339 ) ) ;
#85514 = CARTESIAN_POINT ( 'NONE',  ( 0.04710954650594124937, -1.657193159602200927, 0.7319819781744562048 ) ) ;
#85513 = CARTESIAN_POINT ( 'NONE',  ( 6.801350335910821165, 7.963938809097990124, 1.199719254218452047 ) ) ;
#85515 = CARTESIAN_POINT ( 'NONE',  ( -8.076906825439122528, 10.44614393447756129, -1.599625672291263179 ) ) ;
#85516 = CARTESIAN_POINT ( 'NONE',  ( 5.087333953625774008, 6.958308917361963886, 1.599625672291267398 ) ) ;
#85517 = CARTESIAN_POINT ( 'NONE',  ( 5.040599249230596435, 9.102725900736217568, 0.7998128361456341429 ) ) ;
#85518 = CARTESIAN_POINT ( 'NONE',  ( 0.4265819271708388150, -6.701306620465361519, 10.99180900346492251 ) ) ;
#85519 = CARTESIAN_POINT ( 'NONE',  ( -11.55950211276791251, 11.37999999999998302, 3.221476510067112109 ) ) ;
#85520 = CARTESIAN_POINT ( 'NONE',  ( 4.695201269034174452, 4.372156323494968966, 1.214306433183764966E-14 ) ) ;
#85521 = ORIENTED_EDGE ( 'NONE', *, *, #87621, .T. ) ;
#85522 = CARTESIAN_POINT ( 'NONE',  ( 5.712517600013328867, 1.944077172375497486, 0.5350714256760413789 ) ) ;
#85523 = CARTESIAN_POINT ( 'NONE',  ( 0.5574859923395922845, -1.816599148028580579, 1.093606109393664427 ) ) ;
#85524 = CARTESIAN_POINT ( 'NONE',  ( -0.1394461523060883668, 1.988389203256015536, -2.694605331112149393 ) ) ;
#85525 = CARTESIAN_POINT ( 'NONE',  ( 1.288855427156948835E-16, 3.400000000000000355, 1.925000000000005818 ) ) ;
#85526 = CARTESIAN_POINT ( 'NONE',  ( -4.989037340148921196, 5.883260320670900434, 1.082531754730560403 ) ) ;
#85527 = CARTESIAN_POINT ( 'NONE',  ( 9.924205255523292024, 10.68058700763975466, -0.7216878364870257245 ) ) ;
#85528 = CARTESIAN_POINT ( 'NONE',  ( 3.344544815957225747, -1.939504806627976752, -0.3411970713738179395 ) ) ;
#85529 = CARTESIAN_POINT ( 'NONE',  ( 0.9266185682500321930, -0.9568284065921551784, -1.892426592148554132 ) ) ;
#85530 = CARTESIAN_POINT ( 'NONE',  ( -4.771579997005698459, 7.654261532226910525, -1.199719254218452047 ) ) ;
#85531 = CARTESIAN_POINT ( 'NONE',  ( 0.9311234436981512541, -2.159380368602565881, -3.475000000000000977 ) ) ;
#85532 = CARTESIAN_POINT ( 'NONE',  ( -9.499606442108985860, -9.580649465752454574, 0.08647222121308685561 ) ) ;
#85533 = CARTESIAN_POINT ( 'NONE',  ( 5.648420989521034663, -1.729380818958951460, 1.345873388983606533 ) ) ;
#85534 = CARTESIAN_POINT ( 'NONE',  ( -1.872228381520322449, 3.300000000000011369, -0.3999999999999993006 ) ) ;
#85535 = CARTESIAN_POINT ( 'NONE',  ( 4.647439542507147081, -1.488915335790324201, -1.222320866314072774 ) ) ;
#85536 = CARTESIAN_POINT ( 'NONE',  ( -8.342344591110322227, 8.627156865917170236, -0.7998128361456291469 ) ) ;
#85537 = CARTESIAN_POINT ( 'NONE',  ( -0.1296875068448125057, 2.889142263448498227, -2.315371602238533555 ) ) ;
#85538 = CARTESIAN_POINT ( 'NONE',  ( 1.137671262558290763, -1.993743905544292927, 0.9465009238469669350 ) ) ;
#85539 = ADVANCED_FACE ( 'NONE', ( #206048 ), #152561, .T. ) ;
#85540 = SURFACE_STYLE_FILL_AREA ( #186230 ) ;
#85541 = ORIENTED_EDGE ( 'NONE', *, *, #35731, .T. ) ;
#85542 = CARTESIAN_POINT ( 'NONE',  ( 3.431622278034673901, 7.017660067766835930, -1.734723475976807094E-15 ) ) ;
#85543 = CARTESIAN_POINT ( 'NONE',  ( 5.858249334120006147, -1.969629310164786373, -0.003746551262697600092 ) ) ;
#85544 = CARTESIAN_POINT ( 'NONE',  ( 0.3978616433950994957, -0.6552777965449173569, -1.828281909955962181 ) ) ;
#85545 = CIRCLE ( 'NONE', #130484, 0.09999999999999982514 ) ;
#85546 = CARTESIAN_POINT ( 'NONE',  ( 6.872461156203343080, -0.5239007177601956444, 2.246970456009795836 ) ) ;
#85548 = CARTESIAN_POINT ( 'NONE',  ( 4.082723863713003887, 1.765846151219726101, 0.5873946967244033646 ) ) ;
#85547 = CARTESIAN_POINT ( 'NONE',  ( -5.257529707049291900, 9.355811434857983500, 0.7998128361456291469 ) ) ;
#85549 = CARTESIAN_POINT ( 'NONE',  ( 6.068156270568149324, 9.237210194708310951, 1.199719254218452047 ) ) ;
#85550 = CYLINDRICAL_SURFACE ( 'NONE', #174755, 1.500000000000000222 ) ;
#85551 = CARTESIAN_POINT ( 'NONE',  ( -8.030507057996002729, 8.263346410617135263, 1.040834085586084257E-14 ) ) ;
#85552 = CARTESIAN_POINT ( 'NONE',  ( -3.851925040058345573, 5.587274861525073355, -1.443375672974078761 ) ) ;
#85553 = CARTESIAN_POINT ( 'NONE',  ( 0.6443834720083198020, 0.6415979653194536780, 2.095529601600601755 ) ) ;
#85554 = CARTESIAN_POINT ( 'NONE',  ( 4.039966587192257208, 6.696749537490852333, 1.082531754730558626 ) ) ;
#85555 = VERTEX_POINT ( 'NONE', #41452 ) ;
#85556 = CARTESIAN_POINT ( 'NONE',  ( 9.260383576709811493, -9.448429295179890275, -0.1616405965916348220 ) ) ;
#85557 = CARTESIAN_POINT ( 'NONE',  ( 2.449293598294706414E-16, 8.920000000000001705, 2.000000000000000000 ) ) ;
#85559 = EDGE_CURVE ( 'NONE', #211752, #129544, #180105, .T. ) ;
#85558 = CARTESIAN_POINT ( 'NONE',  ( 0.9612317138737861422, 0.3586375672061762887, -1.789940867121169843 ) ) ;
#85560 = CARTESIAN_POINT ( 'NONE',  ( -5.623934791570306402, 5.455678766453782913, 0.7998128361456341429 ) ) ;
#85561 = CARTESIAN_POINT ( 'NONE',  ( 2.513978358999646723, -1.617321061556979300, 0.6262005117416250544 ) ) ;
#85562 = CARTESIAN_POINT ( 'NONE',  ( 0.000000000000000000, 15.00000000000000000, -11.68000000000000149 ) ) ;
#85563 = CARTESIAN_POINT ( 'NONE',  ( 6.509000000000010111, 6.037005099786168394, 2.594901386363585694 ) ) ;
#85564 = FACE_OUTER_BOUND ( 'NONE', #156710, .T. ) ;
#85565 = CARTESIAN_POINT ( 'NONE',  ( 5.584540971669589737, -1.782103179330214449, -0.3958202769075992444 ) ) ;
#85566 = CARTESIAN_POINT ( 'NONE',  ( 3.133595828963112950, 1.864314371477162169, -0.6108997337519045390 ) ) ;
#85567 = CARTESIAN_POINT ( 'NONE',  ( -0.6125000000000105915, -0.7291666659838408338, -1.060881119635976200 ) ) ;
#85568 = CARTESIAN_POINT ( 'NONE',  ( -7.479294296233107708, 11.87759377891399204, 0.7998128361456481317 ) ) ;
#85569 = CARTESIAN_POINT ( 'NONE',  ( 4.788000803920411386, 8.737751371215816576, 1.040834085586084257E-14 ) ) ;
#85570 = CARTESIAN_POINT ( 'NONE',  ( 4.565154201998150363, -1.702539431995837349, 1.263830167178958463 ) ) ;
#85571 = CARTESIAN_POINT ( 'NONE',  ( 5.657495238652423097, 9.822437888394988548, 0.000000000000000000 ) ) ;
#85572 = CARTESIAN_POINT ( 'NONE',  ( -9.755255220232635693, 11.33988483081495957, -1.199719254218441611 ) ) ;
#85573 = VECTOR ( 'NONE', #162110, 1000.000000000000000 ) ;
#85574 = CARTESIAN_POINT ( 'NONE',  ( 2.799741537105740363, -1.531010120401912200, -1.393694001666223814 ) ) ;
#85576 = CARTESIAN_POINT ( 'NONE',  ( 1.364683531249988757, -0.05312499965857975237, 0.000000000000000000 ) ) ;
#85575 = CARTESIAN_POINT ( 'NONE',  ( 6.827182134110198142, 0.003888933837258023996, 1.810856214465889069 ) ) ;
#85578 = VERTEX_POINT ( 'NONE', #58743 ) ;
#85577 = CARTESIAN_POINT ( 'NONE',  ( 4.635507155980078231, -0.1095829440264598081, 2.218699120425669413 ) ) ;
#85579 = CARTESIAN_POINT ( 'NONE',  ( 2.374040334453372925, -0.3969776081079456898, -2.264039395722910353 ) ) ;
#85580 = CARTESIAN_POINT ( 'NONE',  ( 9.259855728453651125, 9.905512559391842942, 1.040834085586084257E-14 ) ) ;
#85582 = CARTESIAN_POINT ( 'NONE',  ( -1.642778471875000035, -2.967708332855374831, -2.845375778867859751 ) ) ;
#85581 = CARTESIAN_POINT ( 'NONE',  ( 3.444653546323793947, 6.176457016423196222, 1.199719254218451159 ) ) ;
#85583 = EDGE_CURVE ( 'NONE', #140333, #6177, #104027, .T. ) ;
#85584 = DIRECTION ( 'NONE',  ( 0.000000000000000000, 1.000000000000000000, 0.000000000000000000 ) ) ;
#85585 = CARTESIAN_POINT ( 'NONE',  ( 6.720655732516647163, 0.005566325962592238996, 1.826293863978686982 ) ) ;
#85586 = CARTESIAN_POINT ( 'NONE',  ( -0.3536970929470897307, -9.200718514870397158, 9.493915151247904305 ) ) ;
#85587 = EDGE_CURVE ( 'NONE', #179285, #132336, #131738, .T. ) ;
#85588 = CARTESIAN_POINT ( 'NONE',  ( 4.218947473185084007, 1.474887410857337100, -1.217315437338606365 ) ) ;
#85589 = CARTESIAN_POINT ( 'NONE',  ( 3.475000000000000533, -1.195833333333332194, -2.006292185433951047 ) ) ;
#85590 = CARTESIAN_POINT ( 'NONE',  ( 3.557352906045672114, 0.4196458916515317661, -1.672789571874600645 ) ) ;
#85591 = CARTESIAN_POINT ( 'NONE',  ( 3.151577601795185757, 1.966304690962265234, -0.4465026806126579095 ) ) ;
#85592 = CARTESIAN_POINT ( 'NONE',  ( 3.534061846033216714, -1.878541635090751560, 1.324563465849286859 ) ) ;
#85593 = CARTESIAN_POINT ( 'NONE',  ( -11.45842088241054135, 12.50693529122955283, -3.566211699757781073 ) ) ;
#85594 = CARTESIAN_POINT ( 'NONE',  ( 6.428360055892773595, 1.214212339677790409, -1.720619796903441578 ) ) ;
#85595 = CARTESIAN_POINT ( 'NONE',  ( -6.631346530859867805, 6.909194838857525944, 0.000000000000000000 ) ) ;
#85596 = ORIENTED_EDGE ( 'NONE', *, *, #59134, .T. ) ;
#85597 = CARTESIAN_POINT ( 'NONE',  ( 4.463939829769240752, 0.8331255105114807602, 1.561325262609781772 ) ) ;
#85599 = CARTESIAN_POINT ( 'NONE',  ( 0.4106429779945898195, 1.576260533944493503, -1.664518642746879662 ) ) ;
#85598 = CARTESIAN_POINT ( 'NONE',  ( 7.038618024149998043, 8.240751112043669835, -1.199719254218452047 ) ) ;
#85600 = CARTESIAN_POINT ( 'NONE',  ( 6.562460610575872266, -1.685528226061007162, -0.7412392050258274079 ) ) ;
#85601 = CARTESIAN_POINT ( 'NONE',  ( 0.5998553420608258024, 4.283167794419532548, 0.2583637543479620491 ) ) ;
#85602 = B_SPLINE_CURVE_WITH_KNOTS ( 'NONE', 3,
 ( #26653, #109047, #157745, #193427 ),
 .UNSPECIFIED., .F., .F.,
 ( 4, 4 ),
 ( 0.001235641190896560925, 0.001582017824277167153 ),
 .UNSPECIFIED. ) ;
#85603 = SURFACE_STYLE_USAGE ( .BOTH. , #16316 ) ;
#85604 = CARTESIAN_POINT ( 'NONE',  ( -8.086512275908061653, 8.398962174839683215, 0.000000000000000000 ) ) ;
#85605 = CARTESIAN_POINT ( 'NONE',  ( -3.956095110007852622E-14, -1.015624999658570893, 1.570758158831770279 ) ) ;
#85606 = FACE_OUTER_BOUND ( 'NONE', #202048, .T. ) ;
#85607 = CARTESIAN_POINT ( 'NONE',  ( 0.2566020104313873618, -2.170709068928804886, -0.05254486697847670501 ) ) ;
#85608 = CARTESIAN_POINT ( 'NONE',  ( 1.147673126774436225, 1.985868168208399842, -0.3494872464938902357 ) ) ;
#85609 = CIRCLE ( 'NONE', #189509, 11.00000000000000000 ) ;
#85610 = CARTESIAN_POINT ( 'NONE',  ( -1.402160292154681736E-14, 0.2437500006828163535, 1.732050807568877637 ) ) ;
#85611 = CARTESIAN_POINT ( 'NONE',  ( 5.953728026056397837, 0.5566793334266966209, -1.844321365346488273 ) ) ;
#85612 = CARTESIAN_POINT ( 'NONE',  ( -1.402160292154681736E-14, 12.17187500034140335, 1.575800808251682339 ) ) ;
#85613 = CARTESIAN_POINT ( 'NONE',  ( 1.160717840558170622, 2.219164385786871030, 0.1022553982447590853 ) ) ;
#85615 = ORIENTED_EDGE ( 'NONE', *, *, #3232, .F. ) ;
#85614 = CARTESIAN_POINT ( 'NONE',  ( 8.757677159423465696, 12.30470822171437284, 1.199719254218450271 ) ) ;
#85617 = CARTESIAN_POINT ( 'NONE',  ( -7.815970093360414158E-14, 8.210952333604092601, -2.038660652713623733 ) ) ;
#85616 = CARTESIAN_POINT ( 'NONE',  ( -8.912450614902597934, 3.507114751586604129, -8.024806578263023127 ) ) ;
#85618 = CARTESIAN_POINT ( 'NONE',  ( 11.78331023100045627, 9.799999999999998934, -1.800000000000001155 ) ) ;
#85619 = CARTESIAN_POINT ( 'NONE',  ( 9.053093885623066939, 11.58502883802551153, -1.599625672291262513 ) ) ;
#85620 = CARTESIAN_POINT ( 'NONE',  ( -10.91804383151480629, -9.900000000000005684, 0.1905751639681794174 ) ) ;
#85621 = DIRECTION ( 'NONE',  ( 0.000000000000000000, 1.000000000000000000, 0.000000000000000000 ) ) ;
#85622 = CARTESIAN_POINT ( 'NONE',  ( 4.827569786946327213, 0.8888792617508225469, -1.496182039812316678 ) ) ;
#85624 = CARTESIAN_POINT ( 'NONE',  ( 2.014041202081144011, 1.956828179156915315, -0.1411808619533050091 ) ) ;
#85623 = CIRCLE ( 'NONE', #61365, 0.08000000000000020983 ) ;
#85626 = CARTESIAN_POINT ( 'NONE',  ( -0.6823417656250003738, 2.030208333674753174, -1.181850606188749264 ) ) ;
#85625 = CARTESIAN_POINT ( 'NONE',  ( 5.169736645512481132, 4.925780929386339935, 0.7998128361456341429 ) ) ;
#85627 = FACE_OUTER_BOUND ( 'NONE', #61029, .T. ) ;
#85628 = CARTESIAN_POINT ( 'NONE',  ( -1.500000000000022204, 7.388542872122518368, 4.154462424328226433 ) ) ;
#85629 = CARTESIAN_POINT ( 'NONE',  ( 6.391066755906244623, 0.1909826923555627554, 1.952524381009380861 ) ) ;
#85630 = CARTESIAN_POINT ( 'NONE',  ( -6.835281999583978418, 11.12624609948998966, -0.7998128361456291469 ) ) ;
#85631 = CARTESIAN_POINT ( 'NONE',  ( -4.731432421044883263, 5.582721248382882528, -1.082531754730543971 ) ) ;
#85632 = CARTESIAN_POINT ( 'NONE',  ( 5.313685493615880162, -1.282986534165726944, -1.555701818360885280 ) ) ;
#85633 = CARTESIAN_POINT ( 'NONE',  ( 1.235668275047563380, -2.044475609799735416, 0.9693208282701860634 ) ) ;
#85634 = ORIENTED_EDGE ( 'NONE', *, *, #201285, .F. ) ;
#85635 = CARTESIAN_POINT ( 'NONE',  ( -1.402160292154681736E-14, -0.6312499993171797330, -1.732050807568870754 ) ) ;
#85636 = CARTESIAN_POINT ( 'NONE',  ( 2.038157526861613889, 1.849479306444936411, 0.2792354855166642724 ) ) ;
#85637 = CARTESIAN_POINT ( 'NONE',  ( 1.142726939315736656, 0.7017603364856840331, 1.586018014115580188 ) ) ;
#85638 = CARTESIAN_POINT ( 'NONE',  ( 4.792620198997869174, 1.822056328612733145, -1.217503271791681163 ) ) ;
#85639 = CARTESIAN_POINT ( 'NONE',  ( 5.913149109437923379, 2.031366086520134395, 1.094794683655570644 ) ) ;
#85640 = CARTESIAN_POINT ( 'NONE',  ( 1.094684877246233201, -0.5000429121475665761, -1.999180680717755898 ) ) ;
#85641 = CARTESIAN_POINT ( 'NONE',  ( 3.451055654028605701, 0.4708835965685866376, -1.883881102318455847 ) ) ;
#85642 = AXIS2_PLACEMENT_3D ( 'NONE', #212174, #192724, #44378 ) ;
#85643 = CARTESIAN_POINT ( 'NONE',  ( -3.863710589770277259, 6.491117540498504646, 1.082531754730560403 ) ) ;
#85644 = CARTESIAN_POINT ( 'NONE',  ( 5.501189692264965458, 1.528658022856645315, 1.077728667985423661 ) ) ;
#85645 = CARTESIAN_POINT ( 'NONE',  ( 4.009017875521604601, 7.583074288825860876, 0.2480677224083651655 ) ) ;
#85646 = CARTESIAN_POINT ( 'NONE',  ( 0.4031117941524774984, 0.2875473383168804520, 1.709643368666772467 ) ) ;
#85647 = CARTESIAN_POINT ( 'NONE',  ( -1.360316468750040642, 1.161458333674751486, 0.7853790794158861388 ) ) ;
#85648 = CARTESIAN_POINT ( 'NONE',  ( 4.799454022740247794, 1.388487131293577592, -1.462444391756134943 ) ) ;
#85649 = CARTESIAN_POINT ( 'NONE',  ( -3.538314903042294457, 6.111489239315849531, 1.082531754730560403 ) ) ;
#85650 = CARTESIAN_POINT ( 'NONE',  ( 9.759171643738394408, 10.28012176064996197, 0.000000000000000000 ) ) ;
#85652 = CARTESIAN_POINT ( 'NONE',  ( 7.761717428875247293, -5.600320323339640360, -7.717216217110713039 ) ) ;
#85651 = CARTESIAN_POINT ( 'NONE',  ( 2.666400811807769777, -1.259032629953384719, 1.322343945743660543 ) ) ;
#85653 = CARTESIAN_POINT ( 'NONE',  ( -3.623772196602547346, 7.449761006003425834, 0.000000000000000000 ) ) ;
#85654 = CARTESIAN_POINT ( 'NONE',  ( -5.492988512192097161, 6.437516681426083132, 1.199719254218452935 ) ) ;
#85655 = CARTESIAN_POINT ( 'NONE',  ( -9.812993378609343509, 5.211864641514284635, 6.299721592320037367 ) ) ;
#85656 = VERTEX_POINT ( 'NONE', #207118 ) ;
#85657 = CARTESIAN_POINT ( 'NONE',  ( -4.597623488365601752, 8.377994813152914944, 0.7216878364870267237 ) ) ;
#85658 = UNCERTAINTY_MEASURE_WITH_UNIT (LENGTH_MEASURE( 1.000000000000000082E-05 ), #35766, 'distance_accuracy_value', 'NONE');
#85659 = DIRECTION ( 'NONE',  ( 0.000000000000000000, 0.000000000000000000, 1.000000000000000000 ) ) ;
#85660 = CARTESIAN_POINT ( 'NONE',  ( 2.970157261343746136, 6.585292010301047938, 0.4235207732182846851 ) ) ;
#85661 = CARTESIAN_POINT ( 'NONE',  ( 5.830724911194343996, 1.354916080449189764, -1.497948107757952174 ) ) ;
#85663 = ORIENTED_EDGE ( 'NONE', *, *, #13041, .T. ) ;
#85662 = CARTESIAN_POINT ( 'NONE',  ( 6.445936322256165418, -1.448296609194921647, -1.684281199878513657 ) ) ;
#85664 = CARTESIAN_POINT ( 'NONE',  ( -6.343235766347277149, 8.493804042195527870, -1.599625672291271394 ) ) ;
#85665 = CARTESIAN_POINT ( 'NONE',  ( 4.306686350635271054, 8.176217842383143974, -0.7998128361456221525 ) ) ;
#85666 = CARTESIAN_POINT ( 'NONE',  ( 5.102442524761234388, -0.6923759778164092493, -1.941246359495584883 ) ) ;
#85667 = CARTESIAN_POINT ( 'NONE',  ( 4.940077362011475515, -1.704937458037486531, -1.076318853994034930 ) ) ;
#85668 = VERTEX_POINT ( 'NONE', #123840 ) ;
#85669 = ORIENTED_EDGE ( 'NONE', *, *, #209595, .F. ) ;
#85670 = CARTESIAN_POINT ( 'NONE',  ( 10.10176665042273392, 1.000000000000000888, 6.279211784079129721 ) ) ;
#85671 = LINE ( 'NONE', #200468, #82483 ) ;
#85673 = ORIENTED_EDGE ( 'NONE', *, *, #107653, .T. ) ;
#85672 = CARTESIAN_POINT ( 'NONE',  ( -5.444481204339554736, 8.509589284108232121, 1.199719254218454489 ) ) ;
#85674 = CARTESIAN_POINT ( 'NONE',  ( 4.607021725950278146, 8.475092030744066918, 0.2235605714990263060 ) ) ;
#85675 = CARTESIAN_POINT ( 'NONE',  ( 5.079453798366286854, 1.392331892589277142, -1.458333960840517696 ) ) ;
#85676 = CARTESIAN_POINT ( 'NONE',  ( 4.118977087773854961, -1.761250088754966692, 0.5364436722887636622 ) ) ;
#85677 = CARTESIAN_POINT ( 'NONE',  ( -3.332481584934697150, 7.719208080883564804, 2.450691333334236166 ) ) ;
#85678 = CARTESIAN_POINT ( 'NONE',  ( 1.928779914882609914, 1.326332282235458848, -1.888294200376864573 ) ) ;
#85679 = CARTESIAN_POINT ( 'NONE',  ( 5.657495238652423097, 9.822437888394988548, 0.000000000000000000 ) ) ;
#85680 = CARTESIAN_POINT ( 'NONE',  ( 4.516967039858135635, 1.974289957696921949, 0.8805908171375662619 ) ) ;
#85681 = CARTESIAN_POINT ( 'NONE',  ( 8.178592977541601527, 10.56477777859713463, 1.599625672291281386 ) ) ;
#85683 = CARTESIAN_POINT ( 'NONE',  ( 2.747280062631300535, 0.2910806042949847239, -1.995268371848608835 ) ) ;
#85682 = CARTESIAN_POINT ( 'NONE',  ( 0.3451281418221859854, 0.6079892978090885025, -1.844522312511005957 ) ) ;
#85684 = CARTESIAN_POINT ( 'NONE',  ( -5.331380718671772101, 7.243030143248949670, -1.599625672291256295 ) ) ;
#85685 = CARTESIAN_POINT ( 'NONE',  ( 2.680963302752255029, 0.4759847170802535832, -0.1021121987831403316 ) ) ;
#85686 = CARTESIAN_POINT ( 'NONE',  ( 3.151090109352538082, -1.528452604574185525, -1.078222621661927061 ) ) ;
#85687 = CARTESIAN_POINT ( 'NONE',  ( 0.4914017305483203701, 1.457842971892213235, 1.327161884117057600 ) ) ;
#85689 = FILL_AREA_STYLE ('',( #139804 ) ) ;
#85688 = CARTESIAN_POINT ( 'NONE',  ( -0.7500000000000006661, -0.6104166659838470288, -1.299038105676652011 ) ) ;
#85690 = CARTESIAN_POINT ( 'NONE',  ( 2.227434312139275896, 0.001603268854937638837, 2.207063162490217056 ) ) ;
#85691 = CARTESIAN_POINT ( 'NONE',  ( 4.913904330310220558, 4.697586238308844919, 0.000000000000000000 ) ) ;
#85692 = CARTESIAN_POINT ( 'NONE',  ( 3.867100128395839942, 5.534702787927018974, -1.599625672291255185 ) ) ;
#85693 = CARTESIAN_POINT ( 'NONE',  ( -5.135841261478327979, 4.886236314679810455, 0.7998128361456341429 ) ) ;
#85694 = CARTESIAN_POINT ( 'NONE',  ( -6.224601922005509991, 10.27613631906616476, 0.7216878364870267237 ) ) ;
#85695 = CARTESIAN_POINT ( 'NONE',  ( 6.737195113697223903, -1.761045485681483669, 0.8863934713586976155 ) ) ;
#85696 = CARTESIAN_POINT ( 'NONE',  ( 6.252564486485036710, 0.7173172151448119482, 2.193443857502775263 ) ) ;
#85697 = CARTESIAN_POINT ( 'NONE',  ( 0.8890225878602634468, 0.1407106197201784259, 1.956863499422318631 ) ) ;
#85698 = CARTESIAN_POINT ( 'NONE',  ( 3.907127581704954888, -1.689070986467123836, 1.183507789072274496 ) ) ;
#85699 = CARTESIAN_POINT ( 'NONE',  ( 4.690757960648213931, 8.416375354157496602, 0.7216878364870438212 ) ) ;
#85700 = CARTESIAN_POINT ( 'NONE',  ( 5.559725510055676168, 8.644040974110419384, 1.199719254218451159 ) ) ;
#85701 = ORIENTED_EDGE ( 'NONE', *, *, #164027, .T. ) ;
#85702 = CARTESIAN_POINT ( 'NONE',  ( 6.751597309481075726, 10.82068792779586985, 1.040834085586084257E-14 ) ) ;
#85703 = CARTESIAN_POINT ( 'NONE',  ( 1.364683531249988535, 4.717708333674756283, -0.7879004041258300672 ) ) ;
#85704 = CARTESIAN_POINT ( 'NONE',  ( -1.499999999999997780, 4.931250000682820378, 1.214306433183764966E-14 ) ) ;
#85705 = CARTESIAN_POINT ( 'NONE',  ( 4.975479186090852046, 6.827811688571220117, 1.443375672974062551 ) ) ;
#85706 = CARTESIAN_POINT ( 'NONE',  ( 6.461400869420954152, 1.801464151850284301, 1.211653227174382952 ) ) ;
#85707 = CARTESIAN_POINT ( 'NONE',  ( 1.931788062848141441E-13, 7.054063922337705073, -3.955400951015614730 ) ) ;
#85709 = CARTESIAN_POINT ( 'NONE',  ( 6.515202330376022921, -1.784155196879381622, 0.4545711315065634195 ) ) ;
#85708 = DIRECTION ( 'NONE',  ( 0.000000000000000000, 0.000000000000000000, -1.000000000000000000 ) ) ;
#85710 = FACE_OUTER_BOUND ( 'NONE', #79193, .T. ) ;
#85711 = LINE ( 'NONE', #132379, #163860 ) ;
#85712 = CARTESIAN_POINT ( 'NONE',  ( 0.8252170375972631700, -1.778153878779257901, 0.5809004490327505099 ) ) ;
#85714 = EDGE_CURVE ( 'NONE', #102475, #183550, #17564, .T. ) ;
#85713 = CARTESIAN_POINT ( 'NONE',  ( -5.193604695876673283, 6.642107527433549485, 1.420026453975403724 ) ) ;
#85715 = CARTESIAN_POINT ( 'NONE',  ( -2.788906526875773208E-15, 11.71875000068279604, -1.499999999999998446 ) ) ;
#85716 = CARTESIAN_POINT ( 'NONE',  ( 5.943507298343291723, 7.226397084328657350, -1.228854570503196575 ) ) ;
#85717 = CARTESIAN_POINT ( 'NONE',  ( 1.364683531249990311, 5.176041667008085767, 0.7879004041258500513 ) ) ;
#85718 = CARTESIAN_POINT ( 'NONE',  ( 1.154776974461441341, 0.3738248154092556064, 1.875208037630435864 ) ) ;
#85719 = CARTESIAN_POINT ( 'NONE',  ( 3.432247180620687566, 1.726460203109028591, 0.3886401920838201685 ) ) ;
#85721 = CARTESIAN_POINT ( 'NONE',  ( 1.189939518123926510, 1.139724415472416652, 1.535358521287055300 ) ) ;
#85720 = AXIS2_PLACEMENT_3D ( 'NONE', #132225, #177751, #48817 ) ;
#85723 = CARTESIAN_POINT ( 'NONE',  ( 4.077677060472849391, -0.7296757366501721576, 1.771397967703478793 ) ) ;
#85722 = CARTESIAN_POINT ( 'NONE',  ( -2.277406616971334508, 5.600798786534425311, 1.040834085586084257E-14 ) ) ;
#85724 = B_SPLINE_CURVE_WITH_KNOTS ( 'NONE', 3,
 ( #76545, #75490, #123275, #191351 ),
 .UNSPECIFIED., .F., .F.,
 ( 4, 4 ),
 ( 0.000000000000000000, 0.0005559729156925552647 ),
 .UNSPECIFIED. ) ;
#85725 = DIRECTION ( 'NONE',  ( -3.497202527569253358E-15, 0.000000000000000000, -1.000000000000000000 ) ) ;
#85726 = CARTESIAN_POINT ( 'NONE',  ( 5.863713558449636487, -0.4802757262234845226, 1.909948281557447114 ) ) ;
#85728 = ADVANCED_FACE ( 'NONE', ( #190859 ), #26229, .T. ) ;
#85727 = CARTESIAN_POINT ( 'NONE',  ( 0.8617730121942971389, -1.675286201960282995, -1.300076073212981242 ) ) ;
#85729 = CARTESIAN_POINT ( 'NONE',  ( 0.3617799047494585918, -7.723163706540469242, -10.97113338213670808 ) ) ;
#85730 = CARTESIAN_POINT ( 'NONE',  ( 4.100366707588389836, -0.5864361863821172527, -1.776433678864146382 ) ) ;
#85732 = EDGE_LOOP ( 'NONE', ( #125835, #154499, #84180, #49586 ) ) ;
#85731 = CARTESIAN_POINT ( 'NONE',  ( 5.848237035817564156, 1.723274176396558888, 0.07769637638467204177 ) ) ;
#85734 = CARTESIAN_POINT ( 'NONE',  ( 2.901081683644319842, 5.368050483351580304, 1.082531754730548412 ) ) ;
#85733 = CARTESIAN_POINT ( 'NONE',  ( 3.844505992619148937, 2.196175933995975438, 0.2170506636963928093 ) ) ;
#85735 = CARTESIAN_POINT ( 'NONE',  ( 0.6823417656249917140, 4.155208333674755394, 1.181850606188765695 ) ) ;
#85736 = CARTESIAN_POINT ( 'NONE',  ( 1.275913394178169957, -2.012872700982801355, 0.4499014461352250360 ) ) ;
#85738 = EDGE_CURVE ( 'NONE', #36822, #15524, #211136, .T. ) ;
#85737 = CARTESIAN_POINT ( 'NONE',  ( 8.260995669428309540, 8.532249790621511565, 0.7998128361456481317 ) ) ;
#85740 = AXIS2_PLACEMENT_3D ( 'NONE', #13233, #66212, #95589 ) ;
#85739 = CARTESIAN_POINT ( 'NONE',  ( -9.775592450653132204, 11.36361159963886891, -1.199719254218441611 ) ) ;
#85741 = CARTESIAN_POINT ( 'NONE',  ( 0.000000000000000000, 0.000000000000000000, -1.500000000000000222 ) ) ;
#85742 = CARTESIAN_POINT ( 'NONE',  ( 11.94105721839855505, 11.02698343341124243, -1.187919402540330127 ) ) ;
#85743 = CARTESIAN_POINT ( 'NONE',  ( -7.346809171966848240, -6.836568542494916301, -8.002408263929963184 ) ) ;
#85745 = VECTOR ( 'NONE', #211089, 1000.000000000000000 ) ;
#85744 = AXIS2_PLACEMENT_3D ( 'NONE', #101515, #151349, #49561 ) ;
#85746 = ORIENTED_EDGE ( 'NONE', *, *, #179232, .F. ) ;
#85747 = CARTESIAN_POINT ( 'NONE',  ( 3.139188941651628539, -0.1496422021231707811, -2.064996656166856237 ) ) ;
#85748 = CARTESIAN_POINT ( 'NONE',  ( -1.201851678989727383E-14, 4.337500000000023448, -1.732050807568863648 ) ) ;
#85749 = CARTESIAN_POINT ( 'NONE',  ( 4.635998460869027227, 7.496083073400806818, -1.199719254218452047 ) ) ;
#85750 = CARTESIAN_POINT ( 'NONE',  ( -6.374142478797011790, 6.840173217398676897, -0.5947513654121737714 ) ) ;
#85751 = CARTESIAN_POINT ( 'NONE',  ( 1.418624149192078576, -0.7290977765982089576, -1.883658722702468591 ) ) ;
#85752 = SURFACE_STYLE_USAGE ( .BOTH. , #202676 ) ;
#85753 = EDGE_LOOP ( 'NONE', ( #114125, #14889, #172070, #104177 ) ) ;
#85755 = CARTESIAN_POINT ( 'NONE',  ( 7.944714827928043732, 10.29191993738131927, 1.443375672974076540 ) ) ;
#85754 = CARTESIAN_POINT ( 'NONE',  ( 0.07479286986305544449, 2.888457405263197941, -2.344396930208477947 ) ) ;
#85756 = CARTESIAN_POINT ( 'NONE',  ( 6.309922681198771421, -1.704675833164914778, 1.076154833852351000 ) ) ;
#85757 = CARTESIAN_POINT ( 'NONE',  ( 6.245329893291753365, 0.3200292219377436354, -1.888624904781693870 ) ) ;
#85758 = CARTESIAN_POINT ( 'NONE',  ( 6.639320575229230137, 7.629137130509035636, 2.603262396134010892 ) ) ;
#85759 = CARTESIAN_POINT ( 'NONE',  ( 4.282901435897610298, 1.957309562236182021, -0.9860176978964061423 ) ) ;
#85760 = CARTESIAN_POINT ( 'NONE',  ( -1.499999999999997780, 2.931250000682818158, 1.214306433183764966E-14 ) ) ;
#85761 = CARTESIAN_POINT ( 'NONE',  ( 3.937688585161042809, -1.828529804631402023, 0.5600222464785462595 ) ) ;
#85762 = CARTESIAN_POINT ( 'NONE',  ( -5.066996723205291708, 6.934582148538044777, 1.599625672291267398 ) ) ;
#85763 = CARTESIAN_POINT ( 'NONE',  ( 4.812781342726870193, 4.717259109377208048, 0.7216878364870317197 ) ) ;
#85765 = CARTESIAN_POINT ( 'NONE',  ( 0.5621253344089729431, -1.117812357707391069, 1.678020072846800659 ) ) ;
#85764 = CARTESIAN_POINT ( 'NONE',  ( -10.60211293576223213, 11.47147930125185589, 1.040834085586084257E-14 ) ) ;
#85766 = CARTESIAN_POINT ( 'NONE',  ( 0.6823417656249934904, 10.50520833367472839, 1.181850606188764807 ) ) ;
#85768 = CARTESIAN_POINT ( 'NONE',  ( -5.061990249855848667, 6.999017606288844284, -1.599625672291271394 ) ) ;
#85767 = CARTESIAN_POINT ( 'NONE',  ( 6.567925981381852907, -1.350348970527824211, 1.726830949945204363 ) ) ;
#85770 = ORIENTED_EDGE ( 'NONE', *, *, #166482, .T. ) ;
#85769 = CARTESIAN_POINT ( 'NONE',  ( 4.383650571098846704, 1.127723038421009738, 1.305118705121767420 ) ) ;
#85771 = FACE_OUTER_BOUND ( 'NONE', #186979, .T. ) ;
#85772 = CARTESIAN_POINT ( 'NONE',  ( 8.118635056484817980, 8.366162408854107113, 0.7998128361456481317 ) ) ;
#85773 = CARTESIAN_POINT ( 'NONE',  ( 5.335297142177534369, 6.183267073083954735, -1.199719254218452047 ) ) ;
#85774 = CARTESIAN_POINT ( 'NONE',  ( -11.33772463945036968, 12.59088423488573660, -3.600000000000000977 ) ) ;
#85775 = CARTESIAN_POINT ( 'NONE',  ( 0.7835587076311965049, -1.864072139945194717, 0.6119401183290391621 ) ) ;
#85776 = CARTESIAN_POINT ( 'NONE',  ( -1.734723475976807094E-15, 4.518467169708414666, -11.92000000000000171 ) ) ;
#85777 = CARTESIAN_POINT ( 'NONE',  ( 5.542585869888291938, 5.360771691158120689, -0.7998128361456211532 ) ) ;
#85778 = CARTESIAN_POINT ( 'NONE',  ( 0.07536363704237906969, 4.084105538841027894, -2.698926661290324880 ) ) ;
#85779 = VERTEX_POINT ( 'NONE', #191918 ) ;
#85780 = AXIS2_PLACEMENT_3D ( 'NONE', #196875, #65772, #167583 ) ;
#85781 = CARTESIAN_POINT ( 'NONE',  ( 0.4359508081057527629, -6.362962251423731175, 9.827407719474875236 ) ) ;
#85782 = ORIENTED_EDGE ( 'NONE', *, *, #157408, .F. ) ;
#85783 = CARTESIAN_POINT ( 'NONE',  ( 4.301270310059371660, 1.616194109774160559, -0.8183029847002845081 ) ) ;
#85784 = ORIENTED_EDGE ( 'NONE', *, *, #50690, .F. ) ;
#85785 = CARTESIAN_POINT ( 'NONE',  ( 5.006703865196457492, 9.063181286029688977, 0.000000000000000000 ) ) ;
#85786 = CARTESIAN_POINT ( 'NONE',  ( -5.436182321379713578, 6.108390213082993903, 1.083092214668917919 ) ) ;
#85787 = CARTESIAN_POINT ( 'NONE',  ( 5.180233172056982305, 0.8977705535664436409, 1.573279850597033347 ) ) ;
#85788 = CARTESIAN_POINT ( 'NONE',  ( 6.495764994278795612, 9.632124022417032805, 1.082531754730549078 ) ) ;
#85789 = CARTESIAN_POINT ( 'NONE',  ( -6.770610912236888268, -7.154544010627095219, -6.663994888585867749 ) ) ;
#85790 = CARTESIAN_POINT ( 'NONE',  ( 5.430853319176391025, 6.270791292598644873, -1.030804022418196464 ) ) ;
#85791 = AXIS2_PLACEMENT_3D ( 'NONE', #69504, #104176, #137750 ) ;
#85793 = CARTESIAN_POINT ( 'NONE',  ( -8.012344526598182026E-15, 15.29687500034140157, -1.575800808251669460 ) ) ;
#85792 = CARTESIAN_POINT ( 'NONE',  ( 6.725070007137362360, -1.702231675683645973, -0.7527390810756880990 ) ) ;
#85794 = CARTESIAN_POINT ( 'NONE',  ( 2.618635445852790511, 0.2369565241663183774, 1.900835938982778472 ) ) ;
#85795 = CARTESIAN_POINT ( 'NONE',  ( -6.726126798029754106, -7.621055083280781517, -6.709229400517475739 ) ) ;
#85796 = CARTESIAN_POINT ( 'NONE',  ( -10.52284260640670688, 5.420240069097000735, -5.071998063130033430 ) ) ;
#85797 = CARTESIAN_POINT ( 'NONE',  ( 0.7499999999999902300, 5.597916667349482900, -1.299038105676658228 ) ) ;
#85798 = CARTESIAN_POINT ( 'NONE',  ( 4.367134876933267407, 8.109091433148536865, 0.000000000000000000 ) ) ;
#85799 = CARTESIAN_POINT ( 'NONE',  ( 7.131225611108100715, 7.422110755822004968, 0.7216878364870317197 ) ) ;
#85800 = CARTESIAN_POINT ( 'NONE',  ( -4.464712657601869417, 4.103252943490596216, 0.7998128361456341429 ) ) ;
#85801 = CARTESIAN_POINT ( 'NONE',  ( 0.8136072859011161951, -0.3160970183575459447, 2.138355382504661506 ) ) ;
#85802 = CARTESIAN_POINT ( 'NONE',  ( -6.720001414228860881, 7.869031733802326123, -1.199719254218452047 ) ) ;
#85803 = CARTESIAN_POINT ( 'NONE',  ( 4.908934136599710563, 7.884784371745123366, 1.199719254218451159 ) ) ;
#85804 = CARTESIAN_POINT ( 'NONE',  ( 1.342497868159111984, 0.3520595052693386018, 1.791136884925909056 ) ) ;
#85805 = CARTESIAN_POINT ( 'NONE',  ( -4.391951695823077984, 7.211361847513815704, 1.199719254218464037 ) ) ;
#85806 = CARTESIAN_POINT ( 'NONE',  ( 2.414841169274529520, 1.629557050654990791, 0.8231356554938076275 ) ) ;
#85807 = EDGE_CURVE ( 'NONE', #190182, #169714, #129655, .T. ) ;
#85808 = CARTESIAN_POINT ( 'NONE',  ( -3.028993686180034839, 2.741750000184234981, 2.499999999999998224 ) ) ;
#85809 = CARTESIAN_POINT ( 'NONE',  ( 2.039183100597967258, 0.003605121848727563250, 1.912571728241836633 ) ) ;
#85810 = CARTESIAN_POINT ( 'NONE',  ( 3.191813391966125124, -1.320872291013975630, -1.461159636213595459 ) ) ;
#85811 = CARTESIAN_POINT ( 'NONE',  ( 3.913568440338021315, -1.001196544591560933, -1.663976088286099886 ) ) ;
#85812 = CARTESIAN_POINT ( 'NONE',  ( -3.654804927335652209, 6.421633627603656080, 1.199719254218452935 ) ) ;
#85814 = CARTESIAN_POINT ( 'NONE',  ( 4.728832233812888752, 1.460412846248357210, -1.537820402542383169 ) ) ;
#85813 = CARTESIAN_POINT ( 'NONE',  ( 6.210516883511641772, 9.403297576475722508, 1.199719254218452047 ) ) ;
#85815 = DIRECTION ( 'NONE',  ( 0.000000000000000000, 1.000000000000000000, 0.000000000000000000 ) ) ;
#85816 = CARTESIAN_POINT ( 'NONE',  ( 7.397945374551106568, 11.78268670361832093, -0.7998128361456291469 ) ) ;
#85817 = CARTESIAN_POINT ( 'NONE',  ( 6.062205217752669739, 6.048677139763619870, -0.4177986087803304271 ) ) ;
#85818 = CARTESIAN_POINT ( 'NONE',  ( -1.230728480726500429, 3.101239941806485767, -0.7749999999999918066 ) ) ;
#85819 = COLOUR_RGB ( '', 0.66274510, 0.83137255, 0.94901961) ;
#85820 = CARTESIAN_POINT ( 'NONE',  ( 7.523848900940885542, 7.742521570711348389, 0.7998128361456291469 ) ) ;
#85821 = CARTESIAN_POINT ( 'NONE',  ( 11.97929049433705551, 12.30000000000000071, -0.7046979865771820783 ) ) ;
#85823 = EDGE_CURVE ( 'NONE', #50845, #119003, #157254, .T. ) ;
#85822 = CARTESIAN_POINT ( 'NONE',  ( 4.406759617291758246, 1.409692282476209924, -1.160130723419292353 ) ) ;
#85824 = FACE_OUTER_BOUND ( 'NONE', #21693, .T. ) ;
#85825 = CARTESIAN_POINT ( 'NONE',  ( -9.815740026613967828, 10.55404424057886636, -0.7216878364870267237 ) ) ;
#85826 = CARTESIAN_POINT ( 'NONE',  ( -5.672142842012183550, 7.433492730264275927, 1.337035701138490351 ) ) ;
#85827 = LINE ( 'NONE', #135657, #77713 ) ;
#85828 = CARTESIAN_POINT ( 'NONE',  ( 5.049604242677837362, 0.5861553263475408615, -1.776501995420045832 ) ) ;
#85829 = CARTESIAN_POINT ( 'NONE',  ( 8.586391356156291010, 8.911878091804165791, 0.7998128361456481317 ) ) ;
#85830 = CARTESIAN_POINT ( 'NONE',  ( 3.404829243095872648, 1.518349439661485389, -1.185654278882039669 ) ) ;
#85831 = CARTESIAN_POINT ( 'NONE',  ( 6.860214158839045950, -1.961385418603446062, 0.04497666117601883257 ) ) ;
#85832 = AXIS2_PLACEMENT_3D ( 'NONE', #205364, #56998, #123171 ) ;
#85833 = CARTESIAN_POINT ( 'NONE',  ( 4.487912541323413329, 5.194651705420806564, 1.199719254218462483 ) ) ;
#85834 = CARTESIAN_POINT ( 'NONE',  ( 0.6823417656249969321, 9.588541667008065872, -1.181850606188757036 ) ) ;
#85835 = CARTESIAN_POINT ( 'NONE',  ( -5.982172092127739482, 8.002286745614243912, -1.599625672291263179 ) ) ;
#85836 = CARTESIAN_POINT ( 'NONE',  ( 4.518945272056516416, 4.166524327021037699, 0.7998128361456341429 ) ) ;
#85837 = CARTESIAN_POINT ( 'NONE',  ( -7.553827861469316396, 8.841829255582865699, -1.199719254218452047 ) ) ;
#85838 =( BOUNDED_CURVE ( )  B_SPLINE_CURVE ( 2, ( #89332, #6964, #22137 ),
 .UNSPECIFIED., .F., .T. ) 
 B_SPLINE_CURVE_WITH_KNOTS ( ( 3, 3 ),
 ( 0.000000000000000000, 0.002781257751169551561 ),
 .UNSPECIFIED. ) 
 CURVE ( )  GEOMETRIC_REPRESENTATION_ITEM ( )  RATIONAL_B_SPLINE_CURVE ( ( 1.000000000000000000, 0.9105717077957582450, 0.9405305184076298008 ) ) 
 REPRESENTATION_ITEM ( '' )  );
#85839 = CARTESIAN_POINT ( 'NONE',  ( 1.353279953590967644, 0.1518699462816820722, -2.111824974118434728 ) ) ;
#85840 = CARTESIAN_POINT ( 'NONE',  ( -1.873515663034590606, 3.299988112486754943, -0.4000000000000374922 ) ) ;
#85841 = DIRECTION ( 'NONE',  ( 0.000000000000000000, 0.000000000000000000, -1.000000000000000000 ) ) ;
#85842 = CARTESIAN_POINT ( 'NONE',  ( 6.280147189154119403, -1.145143509460907039, -1.724508502191648862 ) ) ;
#85844 = CARTESIAN_POINT ( 'NONE',  ( 4.202513864555980305, 7.333163887849894813, -0.8510647575735978965 ) ) ;
#85843 = CARTESIAN_POINT ( 'NONE',  ( 0.4679805871025365382, -1.733519288248483559, -0.6209854868195128219 ) ) ;
#85845 = CARTESIAN_POINT ( 'NONE',  ( 6.012345284929816458, -2.165844811509042511, 0.7704031996330994447 ) ) ;
#85846 = CARTESIAN_POINT ( 'NONE',  ( 5.124618876285529367, 7.962177208099690873, -1.082531754730549078 ) ) ;
#85847 = CARTESIAN_POINT ( 'NONE',  ( 3.933273961740296087, 6.642551151122080277, 1.082531754730549078 ) ) ;
#85848 = CARTESIAN_POINT ( 'NONE',  ( 1.342159615362942704, 2.289816521768207380, 0.1084569774388414870 ) ) ;
#85850 = EDGE_CURVE ( 'NONE', #97759, #141934, #183101, .T. ) ;
#85849 = CARTESIAN_POINT ( 'NONE',  ( -1.256902978990764641, 3.300000000000025580, 0.5473114391985675065 ) ) ;
#85851 = CARTESIAN_POINT ( 'NONE',  ( -4.586401103172829785, 8.572828063668767484, 0.7998128361456281477 ) ) ;
#85852 = CARTESIAN_POINT ( 'NONE',  ( 6.105412738798914773, -1.926975682693391700, 0.2402159021005992046 ) ) ;
#85853 = ORIENTED_EDGE ( 'NONE', *, *, #190367, .F. ) ;
#85854 = CARTESIAN_POINT ( 'NONE',  ( 8.568389893712330618, 9.098802418860289620, 1.040834085586084257E-14 ) ) ;
#85855 = EDGE_CURVE ( 'NONE', #15686, #141689, #78304, .T. ) ;
#85856 = CARTESIAN_POINT ( 'NONE',  ( 0.8439947366445134103, -1.280256340399921200, -1.553649900018534202 ) ) ;
#85857 = CARTESIAN_POINT ( 'NONE',  ( 6.385953923436008317, -2.015982004707029596, 0.05432014494890363698 ) ) ;
#85859 = CARTESIAN_POINT ( 'NONE',  ( 0.000000000000000000, 8.500000000000000000, 0.000000000000000000 ) ) ;
#85858 = CARTESIAN_POINT ( 'NONE',  ( -7.340850106795412167, 10.65174332698158643, 1.199719254218453823 ) ) ;
#85860 = LINE ( 'NONE', #18707, #5613 ) ;
#85862 = CARTESIAN_POINT ( 'NONE',  ( 1.428175943150990390, 1.704372189200783705, 0.4766478552604267449 ) ) ;
#85861 = CARTESIAN_POINT ( 'NONE',  ( 3.099644000116580589, -2.088226275799191622, 0.1030096337034935861 ) ) ;
#85863 = DIRECTION ( 'NONE',  ( -0.000000000000000000, 1.000000000000000000, -0.000000000000000000 ) ) ;
#85865 = CARTESIAN_POINT ( 'NONE',  ( 4.295090358266894448, 1.839821235612853600, 1.367129665020486273 ) ) ;
#85864 = CARTESIAN_POINT ( 'NONE',  ( -11.01510031751075758, 5.354170659035768942, -4.767690450682862568 ) ) ;
#85866 = CARTESIAN_POINT ( 'NONE',  ( 3.204748380415303188, -0.3384778632026878564, 1.706898776778777993 ) ) ;
#85867 = CARTESIAN_POINT ( 'NONE',  ( 9.083072846151447166, 12.68433652289702884, 1.199719254218450271 ) ) ;
#85868 = CARTESIAN_POINT ( 'NONE',  ( 6.059568310664962709, 6.034194215389424798, 0.7998128361456350310 ) ) ;
#85869 = CARTESIAN_POINT ( 'NONE',  ( 3.584998556975723005, 1.101681934899124915, -1.338793912720330770 ) ) ;
#85870 = CARTESIAN_POINT ( 'NONE',  ( 4.070888617658403597, 1.538033944094893579, -1.532718761138168517 ) ) ;
#85871 = CARTESIAN_POINT ( 'NONE',  ( 4.039439701867726384, 6.800097854565950506, 1.199719254218462483 ) ) ;
#85872 = CARTESIAN_POINT ( 'NONE',  ( 4.100796195634116792, 1.845626398921360822, 0.8128187495666516771 ) ) ;
#85873 = CARTESIAN_POINT ( 'NONE',  ( 3.406250000000002220, 1.895863743164009740, -0.7852924748301655100 ) ) ;
#85874 = CIRCLE ( 'NONE', #61759, 0.07999999999999998779 ) ;
#85875 = CARTESIAN_POINT ( 'NONE',  ( -0.7500000000000215383, 3.972916667349481123, 1.299038105676671107 ) ) ;
#85876 = CARTESIAN_POINT ( 'NONE',  ( 1.676654808981252520, -1.828468026129226542, -0.6065514213326441695 ) ) ;
#85878 = B_SPLINE_CURVE_WITH_KNOTS ( 'NONE', 3,
 ( #156064, #170164, #87860, #71581, #73737, #139834 ),
 .UNSPECIFIED., .F., .F.,
 ( 4, 2, 4 ),
 ( 0.000000000000000000, 0.0003258677429877279035, 0.0006517354859754558071 ),
 .UNSPECIFIED. ) ;
#85877 = CARTESIAN_POINT ( 'NONE',  ( -0.7500000000000179856, 9.072916667349467446, 1.299038105676658228 ) ) ;
#85879 = CARTESIAN_POINT ( 'NONE',  ( 5.906509255234578148, -2.210603606603298132, -0.2184946463264207661 ) ) ;
#85880 = ORIENTED_EDGE ( 'NONE', *, *, #2314, .F. ) ;
#85881 = CARTESIAN_POINT ( 'NONE',  ( -0.1108833634137009749, 4.092508091048022933, -2.451885048449681914 ) ) ;
#85882 = CARTESIAN_POINT ( 'NONE',  ( -1.499999999999997780, 1.900000000000019673, 0.000000000000000000 ) ) ;
#85883 = CARTESIAN_POINT ( 'NONE',  ( 5.937581207780954884, 9.014596278131406848, -1.199719254218440723 ) ) ;
#85884 = CARTESIAN_POINT ( 'NONE',  ( 5.138177029454852551, 5.096887410559856946, 0.7216878364870317197 ) ) ;
#85885 = CARTESIAN_POINT ( 'NONE',  ( 3.285556943750000070, -2.384374999522043126, 0.000000000000000000 ) ) ;
#85886 = CARTESIAN_POINT ( 'NONE',  ( 0.3291711827644402399, 1.527175228150777331, -1.613279532339807476 ) ) ;
#85887 = CARTESIAN_POINT ( 'NONE',  ( 6.180128940399614912, -1.088687182605744042, -1.631870318916525120 ) ) ;
#85888 = CARTESIAN_POINT ( 'NONE',  ( 9.097157885089661278, 9.715698408800516717, 1.040834085586084257E-14 ) ) ;
#85889 = CARTESIAN_POINT ( 'NONE',  ( 6.484567079770447329, -6.583980363594976737, 7.100579091573052004 ) ) ;
#85890 = CARTESIAN_POINT ( 'NONE',  ( 0.2280961430754513408, -1.329988288769240024, -1.704746276402234528 ) ) ;
#85891 = CARTESIAN_POINT ( 'NONE',  ( 5.123001941117305336, 7.070197912760590064, 1.599625672291268286 ) ) ;
#85893 = AXIS2_PLACEMENT_3D ( 'NONE', #13280, #212535, #129268 ) ;
#85892 = CONICAL_SURFACE ( 'NONE', #206950, 1.540450515248283025, 0.7853981633974428389 ) ;
#85894 = CARTESIAN_POINT ( 'NONE',  ( -5.994113311017573054, 6.165756082374834079, 0.7216878364870257245 ) ) ;
#85895 = CARTESIAN_POINT ( 'NONE',  ( 4.053227687556320014, 1.744102858319864113, -1.100964799198749455 ) ) ;
#85896 = CARTESIAN_POINT ( 'NONE',  ( -5.311043488251275591, 7.219303374425030562, -1.599625672291256295 ) ) ;
#85897 = B_SPLINE_CURVE_WITH_KNOTS ( 'NONE', 3,
 ( #32072, #164207, #128598, #81880, #180455, #147964, #144804, #63509 ),
 .UNSPECIFIED., .F., .F.,
 ( 4, 2, 2, 4 ),
 ( 0.000000000000000000, 0.0003954713701971478341, 0.0005932070552957217783, 0.0007909427403942956682 ),
 .UNSPECIFIED. ) ;
#85898 = CARTESIAN_POINT ( 'NONE',  ( -1.201851678989727383E-14, 3.618750000682816381, -1.732050807568863648 ) ) ;
#85899 = CARTESIAN_POINT ( 'NONE',  ( -1.402160292154681736E-14, -1.178124999658576311, 1.575800808251672791 ) ) ;
#85900 = CARTESIAN_POINT ( 'NONE',  ( 5.589076619078012342, 1.650032040524500143, -0.8810306647013477210 ) ) ;
#85901 = CARTESIAN_POINT ( 'NONE',  ( 4.219182763733449804, 1.701723821253621427, 0.3326838626578206282 ) ) ;
#85902 = CARTESIAN_POINT ( 'NONE',  ( 2.805909833680774845, 1.258924587927259253, -1.202001966437598268 ) ) ;
#85903 = CARTESIAN_POINT ( 'NONE',  ( 2.314399336204819857, 1.494381390340574489, -1.738437040929841082 ) ) ;
#85904 = CARTESIAN_POINT ( 'NONE',  ( -1.364683531250012516, 4.551041667008082214, -0.7879004041258300672 ) ) ;
#85905 = CARTESIAN_POINT ( 'NONE',  ( 6.216366674833015971, 1.951045902775162322, 0.7519257042096252341 ) ) ;
#85906 = CARTESIAN_POINT ( 'NONE',  ( 6.720655732516681802, 0.002698097948229584257, 1.926293798961112858 ) ) ;
#85907 = CARTESIAN_POINT ( 'NONE',  ( 0.000000000000000000, -0.4330127018922214077, 0.000000000000000000 ) ) ;
#85908 = CARTESIAN_POINT ( 'NONE',  ( 1.916638904718031000, -1.319229391439219246, -1.525043083973671498 ) ) ;
#85909 = CARTESIAN_POINT ( 'NONE',  ( 0.02373106683711476844, -1.352142385343929387, -1.725327757841052856 ) ) ;
#85910 = CARTESIAN_POINT ( 'NONE',  ( 7.209650745910531455, 13.96317866693702925, -9.185143276789457190 ) ) ;
#85911 = CARTESIAN_POINT ( 'NONE',  ( -7.395082721250053837, 10.71501471051202614, -1.199719254218446718 ) ) ;
#85912 = CARTESIAN_POINT ( 'NONE',  ( 6.063521013809720195, 8.097193820909906137, 1.599625672291281386 ) ) ;
#85913 = CARTESIAN_POINT ( 'NONE',  ( 2.473420802178166067, -1.846219560914775570, -1.042883725575906029 ) ) ;
#85914 = CARTESIAN_POINT ( 'NONE',  ( -0.6823417656250246877, -0.1989583329919109023, 1.181850606188755259 ) ) ;
#85915 = CARTESIAN_POINT ( 'NONE',  ( 5.145057536039753465, -1.563975785779356587, 0.9416349707431559413 ) ) ;
#85916 = EDGE_CURVE ( 'NONE', #150426, #107948, #86531, .T. ) ;
#85917 = EDGE_LOOP ( 'NONE', ( #130528, #94894, #109271, #54787 ) ) ;
#85918 = CARTESIAN_POINT ( 'NONE',  ( -7.632314129850253259, 7.869064337772231355, 0.7998128361456341429 ) ) ;
#85919 =( NAMED_UNIT ( * ) PLANE_ANGLE_UNIT ( ) SI_UNIT ( $, .RADIAN. ) );
#85920 = CARTESIAN_POINT ( 'NONE',  ( 6.170369307550816806, 9.252495721234380355, 1.082531754730549967 ) ) ;
#85921 = CARTESIAN_POINT ( 'NONE',  ( -1.737499999999997824, -4.097916665710750195, 3.009438278150925683 ) ) ;
#85922 = CARTESIAN_POINT ( 'NONE',  ( -5.530836599371015794, 8.540060901653093950, 1.199719254218452047 ) ) ;
#85923 = CARTESIAN_POINT ( 'NONE',  ( 1.670181813679386007, 2.014099715005359670, -0.1526998803580876252 ) ) ;
#85924 = CARTESIAN_POINT ( 'NONE',  ( 0.2882880397960294605, -0.9922573751702695732, 1.857558580286112981 ) ) ;
#85925 = CARTESIAN_POINT ( 'NONE',  ( 8.920375002787457319, 12.49452237230570084, 1.199719254218450271 ) ) ;
#85926 = CARTESIAN_POINT ( 'NONE',  ( 4.346440162718026912, -1.840208154270198015, -0.2762933559420696072 ) ) ;
#85927 = CARTESIAN_POINT ( 'NONE',  ( 8.727698198895078363, 11.20540053684285553, -1.599625672291257406 ) ) ;
#85928 = CARTESIAN_POINT ( 'NONE',  ( 11.97929049433705373, 13.88000000000000078, -0.7046979865771834106 ) ) ;
#85929 = EDGE_LOOP ( 'NONE', ( #7781, #724, #134375, #67258 ) ) ;
#85930 = CARTESIAN_POINT ( 'NONE',  ( -4.548924232584923288, 5.265832011892554121, -1.199719254218446718 ) ) ;
#85931 =( BOUNDED_SURFACE ( )  B_SPLINE_SURFACE ( 3, 3, ( 
 ( #75665, #141772, #59407, #37830, #103908, #71368, #78841, #176368, #192588, #97257, #46369, #43189, #160109, #175311, #13835, #112488, #93002, #162248, #27975, #163311, #113560, #212029, #208838, #62594, #147076, #94069, #109302, #44243, #110364, #63672, #213097, #11712, #146018, #126625, #29048, #194730, #178498, #77786, #125563, #79910, #14892, #31184 ),
 ( #143907, #80987, #209900, #129826, #144961, #61538, #195808, #191524, #127704, #76715, #60468, #193664, #47444, #12766, #177430, #45307, #26898, #30108, #159046, #111426, #210966, #128757, #96199, #179563, #10639, #142831, #95131, #161180, #35425, #1840, #51702, #198972, #130870, #197919, #83104, #32237, #102573, #152393, #20236, #86321, #49546, #118883 ),
 ( #167573, #33294, #181667, #200053, #84183, #64727, #115672, #17027, #182742, #98309, #149184, #50617, #166503, #151335, #67899, #34360, #99378, #760, #165431, #131910, #66827, #132970, #116742, #48503, #100433, #15958, #117825, #18095, #150271, #65764, #2904, #36495, #134043, #82041, #148135, #183815, #135095, #101503, #19172, #85246, #114622, #68976 ),
 ( #201108, #52749, #184869, #168633, #164373, #196865, #180613, #214136, #192067, #158529, #208321, #141254, #70039, #140169, #25313, #185935, #44803, #94620, #176913, #28529, #206191, #61024, #175860, #9070, #109846, #189949, #123981, #142311, #26378, #3971, #57819, #173735, #125046, #37570, #91414, #207262, #108776, #93546, #156400, #107709, #10126, #76201 ),
 ( #191001, #59952, #126107, #43732, #27448, #7988, #159590, #119960, #143381, #136155, #74077, #106625, #127185, #58892, #157475, #42668, #11189, #77269, #209380, #193153, #174802, #110907, #202172, #53830, #172654, #24229, #92491, #41598, #75144, #90331, #81541, #78336, #195302, #210462, #49055, #147623, #128259, #197414, #211525, #132468, #148684, #32796 ),
 ( #212595, #115176, #63160, #13335, #111988, #181171, #213642, #252, #129325, #66324, #62100, #98870, #14386, #161743, #96758, #164922, #179056, #95689, #46932, #64233, #162809, #182226, #160663, #177990, #80478, #16515, #79409, #113050, #198471, #33849, #48006, #146577, #114124, #130376, #194221, #45866, #50116, #145526, #180116, #29603, #30675, #82598 ),
 ( #196366, #31741, #97814, #163878, #116236, #15453, #12259, #65268, #144458, #131414, #100977, #99930, #83661, #168127, #187565, #154016, #5582, #149751, #152942, #2390, #135638, #84738, #167066, #184359, #165992, #86875, #70591, #68468, #67390, #151888, #54382, #134595, #18658, #51179, #120520, #4518, #71662, #150827, #103130, #69531, #200596, #52243 ) ),
 .UNSPECIFIED., .T., .F., .T. ) 
 B_SPLINE_SURFACE_WITH_KNOTS ( ( 4, 3, 4 ),
 ( 4, 2, 2, 2, 2, 2, 2, 2, 2, 2, 2, 2, 2, 2, 2, 2, 2, 2, 2, 2, 4 ),
 ( 0.000000000000000000, 0.5000000000000000000, 1.000000000000000000 ),
 ( 0.2451329569378435380, 0.2471230096987881431, 0.2491130624597327203, 0.2530931679816219027, 0.2610533790254002673, 0.2769738011129569966, 0.3088146452880705106, 0.3724963336382974832, 0.4043793557688165619, 0.4362623778993356405, 0.5000489545690223192, 0.5638291548596064962, 0.5957026119297792466, 0.6275760689999518860, 0.6912196958168144167, 0.7230415092252455711, 0.7389524159294611483, 0.7469078692815689369, 0.7508855959576228312, 0.7528744592956497783, 0.7548633226336768365 ),
 .UNSPECIFIED. ) 
 GEOMETRIC_REPRESENTATION_ITEM ( )  RATIONAL_B_SPLINE_SURFACE ( (
 ( 1.000000000000000000, 1.000000000000000000, 1.000000000000000000, 1.000000000000000000, 1.000000000000000000, 1.000000000000000000, 1.000000000000000000, 1.000000000000000000, 1.000000000000000000, 1.000000000000000000, 1.000000000000000000, 1.000000000000000000, 1.000000000000000000, 1.000000000000000000, 1.000000000000000000, 1.000000000000000000, 1.000000000000000000, 1.000000000000000000, 1.000000000000000000, 1.000000000000000000, 1.000000000000000000, 1.000000000000000000, 1.000000000000000000, 1.000000000000000000, 1.000000000000000000, 1.000000000000000000, 1.000000000000000000, 1.000000000000000000, 1.000000000000000000, 1.000000000000000000, 1.000000000000000000, 1.000000000000000000, 1.000000000000000000, 1.000000000000000000, 1.000000000000000000, 1.000000000000000000, 1.000000000000000000, 1.000000000000000000, 1.000000000000000000, 1.000000000000000000, 1.000000000000000000, 1.000000000000000000),
 ( 0.3333333333333333703, 0.3333333333333333703, 0.3333333333333333703, 0.3333333333333333703, 0.3333333333333333703, 0.3333333333333333703, 0.3333333333333333703, 0.3333333333333333703, 0.3333333333333333703, 0.3333333333333333703, 0.3333333333333333703, 0.3333333333333333703, 0.3333333333333333703, 0.3333333333333333703, 0.3333333333333333703, 0.3333333333333333703, 0.3333333333333333703, 0.3333333333333333703, 0.3333333333333333703, 0.3333333333333333703, 0.3333333333333333703, 0.3333333333333333703, 0.3333333333333333703, 0.3333333333333333703, 0.3333333333333333703, 0.3333333333333333703, 0.3333333333333333703, 0.3333333333333333703, 0.3333333333333333703, 0.3333333333333333703, 0.3333333333333333703, 0.3333333333333333703, 0.3333333333333333703, 0.3333333333333333703, 0.3333333333333333703, 0.3333333333333333703, 0.3333333333333333703, 0.3333333333333333703, 0.3333333333333333703, 0.3333333333333333703, 0.3333333333333333703, 0.3333333333333333703),
 ( 0.3333333333333333703, 0.3333333333333333703, 0.3333333333333333703, 0.3333333333333333703, 0.3333333333333333703, 0.3333333333333333703, 0.3333333333333333703, 0.3333333333333333703, 0.3333333333333333703, 0.3333333333333333703, 0.3333333333333333703, 0.3333333333333333703, 0.3333333333333333703, 0.3333333333333333703, 0.3333333333333333703, 0.3333333333333333703, 0.3333333333333333703, 0.3333333333333333703, 0.3333333333333333703, 0.3333333333333333703, 0.3333333333333333703, 0.3333333333333333703, 0.3333333333333333703, 0.3333333333333333703, 0.3333333333333333703, 0.3333333333333333703, 0.3333333333333333703, 0.3333333333333333703, 0.3333333333333333703, 0.3333333333333333703, 0.3333333333333333703, 0.3333333333333333703, 0.3333333333333333703, 0.3333333333333333703, 0.3333333333333333703, 0.3333333333333333703, 0.3333333333333333703, 0.3333333333333333703, 0.3333333333333333703, 0.3333333333333333703, 0.3333333333333333703, 0.3333333333333333703),
 ( 1.000000000000000000, 1.000000000000000000, 1.000000000000000000, 1.000000000000000000, 1.000000000000000000, 1.000000000000000000, 1.000000000000000000, 1.000000000000000000, 1.000000000000000000, 1.000000000000000000, 1.000000000000000000, 1.000000000000000000, 1.000000000000000000, 1.000000000000000000, 1.000000000000000000, 1.000000000000000000, 1.000000000000000000, 1.000000000000000000, 1.000000000000000000, 1.000000000000000000, 1.000000000000000000, 1.000000000000000000, 1.000000000000000000, 1.000000000000000000, 1.000000000000000000, 1.000000000000000000, 1.000000000000000000, 1.000000000000000000, 1.000000000000000000, 1.000000000000000000, 1.000000000000000000, 1.000000000000000000, 1.000000000000000000, 1.000000000000000000, 1.000000000000000000, 1.000000000000000000, 1.000000000000000000, 1.000000000000000000, 1.000000000000000000, 1.000000000000000000, 1.000000000000000000, 1.000000000000000000),
 ( 0.3333333333333333703, 0.3333333333333333703, 0.3333333333333333703, 0.3333333333333333703, 0.3333333333333333703, 0.3333333333333333703, 0.3333333333333333703, 0.3333333333333333703, 0.3333333333333333703, 0.3333333333333333703, 0.3333333333333333703, 0.3333333333333333703, 0.3333333333333333703, 0.3333333333333333703, 0.3333333333333333703, 0.3333333333333333703, 0.3333333333333333703, 0.3333333333333333703, 0.3333333333333333703, 0.3333333333333333703, 0.3333333333333333703, 0.3333333333333333703, 0.3333333333333333703, 0.3333333333333333703, 0.3333333333333333703, 0.3333333333333333703, 0.3333333333333333703, 0.3333333333333333703, 0.3333333333333333703, 0.3333333333333333703, 0.3333333333333333703, 0.3333333333333333703, 0.3333333333333333703, 0.3333333333333333703, 0.3333333333333333703, 0.3333333333333333703, 0.3333333333333333703, 0.3333333333333333703, 0.3333333333333333703, 0.3333333333333333703, 0.3333333333333333703, 0.3333333333333333703),
 ( 0.3333333333333333703, 0.3333333333333333703, 0.3333333333333333703, 0.3333333333333333703, 0.3333333333333333703, 0.3333333333333333703, 0.3333333333333333703, 0.3333333333333333703, 0.3333333333333333703, 0.3333333333333333703, 0.3333333333333333703, 0.3333333333333333703, 0.3333333333333333703, 0.3333333333333333703, 0.3333333333333333703, 0.3333333333333333703, 0.3333333333333333703, 0.3333333333333333703, 0.3333333333333333703, 0.3333333333333333703, 0.3333333333333333703, 0.3333333333333333703, 0.3333333333333333703, 0.3333333333333333703, 0.3333333333333333703, 0.3333333333333333703, 0.3333333333333333703, 0.3333333333333333703, 0.3333333333333333703, 0.3333333333333333703, 0.3333333333333333703, 0.3333333333333333703, 0.3333333333333333703, 0.3333333333333333703, 0.3333333333333333703, 0.3333333333333333703, 0.3333333333333333703, 0.3333333333333333703, 0.3333333333333333703, 0.3333333333333333703, 0.3333333333333333703, 0.3333333333333333703),
 ( 1.000000000000000000, 1.000000000000000000, 1.000000000000000000, 1.000000000000000000, 1.000000000000000000, 1.000000000000000000, 1.000000000000000000, 1.000000000000000000, 1.000000000000000000, 1.000000000000000000, 1.000000000000000000, 1.000000000000000000, 1.000000000000000000, 1.000000000000000000, 1.000000000000000000, 1.000000000000000000, 1.000000000000000000, 1.000000000000000000, 1.000000000000000000, 1.000000000000000000, 1.000000000000000000, 1.000000000000000000, 1.000000000000000000, 1.000000000000000000, 1.000000000000000000, 1.000000000000000000, 1.000000000000000000, 1.000000000000000000, 1.000000000000000000, 1.000000000000000000, 1.000000000000000000, 1.000000000000000000, 1.000000000000000000, 1.000000000000000000, 1.000000000000000000, 1.000000000000000000, 1.000000000000000000, 1.000000000000000000, 1.000000000000000000, 1.000000000000000000, 1.000000000000000000, 1.000000000000000000) ) ) 
 REPRESENTATION_ITEM ( '' )  SURFACE ( )  );
#85932 = CARTESIAN_POINT ( 'NONE',  ( -7.049349804101573191, 10.31165964050546258, -1.199719254218440723 ) ) ;
#85933 = CARTESIAN_POINT ( 'NONE',  ( 5.602125774977974260, -1.825872481414937853, 0.004271240736861136277 ) ) ;
#85935 = CARTESIAN_POINT ( 'NONE',  ( -4.010472434439474654, 7.801430412234481082, -0.4134458547365611469 ) ) ;
#85934 = CARTESIAN_POINT ( 'NONE',  ( -6.129167961829681488, 9.308390501180058507, -1.199719254218452047 ) ) ;
#85936 = CARTESIAN_POINT ( 'NONE',  ( 1.364683531249986981, -1.115624999658580752, 0.000000000000000000 ) ) ;
#85937 = CARTESIAN_POINT ( 'NONE',  ( 1.405166929871915604, 0.3316955492517637549, 1.701605581617445129 ) ) ;
#85938 = CARTESIAN_POINT ( 'NONE',  ( 0.3568325553494673397, 1.722114113718915984, -0.2502821355834724537 ) ) ;
#85940 = CARTESIAN_POINT ( 'NONE',  ( 6.954969614130424027, 11.05795561655343384, 1.040834085586084257E-14 ) ) ;
#85939 = CARTESIAN_POINT ( 'NONE',  ( 6.094374174207308315, -2.295927367373576722, -0.2327322904458818675 ) ) ;
#85941 = CARTESIAN_POINT ( 'NONE',  ( 5.388439706788500594, 5.251210844200210559, 0.7998128361456352531 ) ) ;
#85942 = CARTESIAN_POINT ( 'NONE',  ( 1.634131612217240681, 1.018193428692963698, -1.791617596397138801 ) ) ;
#85943 = CARTESIAN_POINT ( 'NONE',  ( 5.120175567455225618, 9.125288595339771547, -0.7998128361456281477 ) ) ;
#85944 = CARTESIAN_POINT ( 'NONE',  ( 0.4915642615439493879, 1.928455281639355867, 0.5879340682083398217 ) ) ;
#85945 = CARTESIAN_POINT ( 'NONE',  ( 0.001026545178762920067, 7.078193277237624592, -2.121339347286375965 ) ) ;
#85946 = CARTESIAN_POINT ( 'NONE',  ( -6.720001414228860881, 7.869031733802326123, -1.199719254218452047 ) ) ;
#85947 = CARTESIAN_POINT ( 'NONE',  ( 0.09253734621218495660, -0.4319466259074012937, -1.930967020758065589 ) ) ;
#85949 = CARTESIAN_POINT ( 'NONE',  ( -5.289089323106922258, 9.184704953684462936, 0.7216878364870267237 ) ) ;
#85948 = CARTESIAN_POINT ( 'NONE',  ( 3.902528505893249733, -1.892296425594198750, -0.2755589300712790735 ) ) ;
#85950 = CARTESIAN_POINT ( 'NONE',  ( 5.602238545945851023, -2.207063162045197924, -0.003355105161521875021 ) ) ;
#85951 = CARTESIAN_POINT ( 'NONE',  ( -4.957638175832625493E-14, 2.375000000682783163, 1.414508159514561436 ) ) ;
#85952 = CARTESIAN_POINT ( 'NONE',  ( 3.834746474454188013E-15, 10.56250000000000178, 1.500000000000001554 ) ) ;
#85953 = CARTESIAN_POINT ( 'NONE',  ( 3.567203813726949058, 7.175838526074521440, 0.7216878364870257245 ) ) ;
#85954 = CARTESIAN_POINT ( 'NONE',  ( -3.634994581795317536, 7.254927755487573293, 0.000000000000000000 ) ) ;
#85955 = CARTESIAN_POINT ( 'NONE',  ( 0.01237536129615121258, -2.019283296508204817, -0.04721428876065454638 ) ) ;
#85956 = CARTESIAN_POINT ( 'NONE',  ( 3.100898361104642120, -0.6683016296473989204, -2.208703637169514788 ) ) ;
#85957 = CARTESIAN_POINT ( 'NONE',  ( 4.404711838702720428, 0.5211615849865286476, 1.891323523724611766 ) ) ;
#85958 = CARTESIAN_POINT ( 'NONE',  ( 0.4440980561614649158, -0.9299495107331550159, 1.727370323332158897 ) ) ;
#85959 = CARTESIAN_POINT ( 'NONE',  ( 1.734723475976807094E-15, 15.00041888085534758, 12.17999951260719982 ) ) ;
#85960 = CARTESIAN_POINT ( 'NONE',  ( -9.386399775572158433, 15.51845911145272083, 7.476390437876971440 ) ) ;
#85961 = CARTESIAN_POINT ( 'NONE',  ( 6.368375356916068597, -1.978549699825098429, -0.3886382054163611821 ) ) ;
#85962 = CARTESIAN_POINT ( 'NONE',  ( -7.309817376062285099, 11.67987070538135264, 0.000000000000000000 ) ) ;
#85963 = CARTESIAN_POINT ( 'NONE',  ( -0.02968770228140016343, 0.003472272166151618711, -1.826291111852257343 ) ) ;
#85964 = B_SPLINE_CURVE_WITH_KNOTS ( 'NONE', 3,
 ( #87959, #120539, #99945, #185443, #67406, #151902, #100996, #84756, #166010, #37063, #17595, #150843, #186516, #2405, #103145, #68484 ),
 .UNSPECIFIED., .F., .F.,
 ( 4, 3, 3, 3, 3, 4 ),
 ( 0.000000000000000000, 6.763659418792606948E-06, 1.351747408346288389E-05, 2.025570936575419461E-05, 2.697948549281416054E-05, 3.136114954460949742E-05 ),
 .UNSPECIFIED. ) ;
#85965 = CARTESIAN_POINT ( 'NONE',  ( 3.098652014986380543, 2.154143853245940043, 0.2703130112568508103 ) ) ;
#85966 = CARTESIAN_POINT ( 'NONE',  ( 0.4461838333975313153, 2.877219473291478646, 1.949594826320503849 ) ) ;
#85967 = CARTESIAN_POINT ( 'NONE',  ( 0.5629301599625028407, 0.6213668382478373386, 2.027498709647377773 ) ) ;
#85968 = CARTESIAN_POINT ( 'NONE',  ( 1.499999999999989120, 2.035416667349480679, 0.8660254037844524744 ) ) ;
#85969 = CARTESIAN_POINT ( 'NONE',  ( 8.380911511541880188, 12.92948053010758258, 0.7998128361456462443 ) ) ;
#85970 = CARTESIAN_POINT ( 'NONE',  ( 1.886825320689233809, 2.480000000000016858, 2.459652456995882641 ) ) ;
#85971 = CARTESIAN_POINT ( 'NONE',  ( 6.454497976780569246, 6.866128686250288382, -0.6735470152485992790 ) ) ;
#85972 = CIRCLE ( 'NONE', #68627, 0.04999999999999985706 ) ;
#85973 = CARTESIAN_POINT ( 'NONE',  ( 1.704443381354688203, -0.7389896827423731995, -1.923919429860524888 ) ) ;
#85975 = FACE_OUTER_BOUND ( 'NONE', #46093, .T. ) ;
#85974 = CARTESIAN_POINT ( 'NONE',  ( -10.17947440576205054, 10.77047498301088346, 0.7998128361456462443 ) ) ;
#85976 = CARTESIAN_POINT ( 'NONE',  ( 0.6823417656249882723, 1.676041667008083769, -1.181850606188749264 ) ) ;
#85977 = DIRECTION ( 'NONE',  ( 0.000000000000000000, 1.000000000000000000, 0.000000000000000000 ) ) ;
#85978 = EDGE_LOOP ( 'NONE', ( #44412, #6603, #115593, #27985, #103134, #55412, #111147 ) ) ;
#85979 = CARTESIAN_POINT ( 'NONE',  ( 4.424404876070213710, -0.8207606565990737124, -1.727334472114170794 ) ) ;
#85980 = CARTESIAN_POINT ( 'NONE',  ( 11.86239285000045918, 12.22000000000000064, -1.812080536912753059 ) ) ;
#85981 = CARTESIAN_POINT ( 'NONE',  ( -2.578021764892882040, 6.159442492350315490, 0.7998128361456341429 ) ) ;
#85982 = CARTESIAN_POINT ( 'NONE',  ( 1.441375510584298913, -1.705046834049932292, 0.6123784311264174329 ) ) ;
#85984 = CARTESIAN_POINT ( 'NONE',  ( 0.8486862992652006721, -1.733348825135153648, -0.8160025691017428473 ) ) ;
#85983 = CARTESIAN_POINT ( 'NONE',  ( 1.500000000000001110, 7.388542872122531691, -4.154462424328188241 ) ) ;
#85985 = TOROIDAL_SURFACE ( 'NONE', #200065, 12.18000000000000149, 0.5000000000000008882 ) ;
#85986 = CARTESIAN_POINT ( 'NONE',  ( 2.031770498437397876, 1.981864486777328294, -0.5989037013024376410 ) ) ;
#85987 = CARTESIAN_POINT ( 'NONE',  ( -1.364683531250014514, -0.1572916663252435232, 0.7879004041258379498 ) ) ;
#85988 = EDGE_CURVE ( 'NONE', #68165, #21223, #88135, .T. ) ;
#85989 = CARTESIAN_POINT ( 'NONE',  ( 0.9187500235564357576, 1.820693165844145867, 0.7566030219750378150 ) ) ;
#85990 = CARTESIAN_POINT ( 'NONE',  ( 5.373632986646971865, 1.856140760046654403, -0.5156676092323666527 ) ) ;
#85992 = CARTESIAN_POINT ( 'NONE',  ( 6.469672735924913987, 6.762149564967588233, 0.2594904213018677797 ) ) ;
#85991 = CARTESIAN_POINT ( 'NONE',  ( 6.498651167236064730, -0.5841124237929047336, -2.128106146270396071 ) ) ;
#85993 = CARTESIAN_POINT ( 'NONE',  ( -0.6823417656250003738, 1.467708333674752730, -1.181850606188749264 ) ) ;
#85994 = CARTESIAN_POINT ( 'NONE',  ( 3.666515279890161239, -0.8333913613888814798, -1.886988505759807921 ) ) ;
#85995 = CARTESIAN_POINT ( 'NONE',  ( -6.847031270101295419, 7.946956888995021728, -1.199719254218446718 ) ) ;
#85996 = CARTESIAN_POINT ( 'NONE',  ( 8.209625708274705502, 9.536650400197368427, 1.199719254218462483 ) ) ;
#85997 = CARTESIAN_POINT ( 'NONE',  ( 0.000000000000000000, 5.868705557303649734, -4.125226524755057689 ) ) ;
#85998 = CARTESIAN_POINT ( 'NONE',  ( 6.518772930072240790, 6.499656594706071822, -0.7998128361456281477 ) ) ;
#86000 = CARTESIAN_POINT ( 'NONE',  ( -1.500000000000011324, 4.170833333333359150, 0.8660254037844403729 ) ) ;
#85999 = CARTESIAN_POINT ( 'NONE',  ( 5.350649881110917327, 0.6085095821539068250, 2.016136239840255140 ) ) ;
#86001 = CARTESIAN_POINT ( 'NONE',  ( 6.883263157960362477, -0.004191378316371896506, 2.053658919477070910 ) ) ;
#86002 = CARTESIAN_POINT ( 'NONE',  ( 0.6823417656249882723, 1.738541667008083991, -1.181850606188749264 ) ) ;
#86003 = CARTESIAN_POINT ( 'NONE',  ( 4.411504763889100289, -0.3743020017868465832, 2.128795073437335095 ) ) ;
#86004 = CARTESIAN_POINT ( 'NONE',  ( 4.389322685995568740, -0.002182162029157329840, -2.019862493239577894 ) ) ;
#86005 = FILL_AREA_STYLE ('',( #136901 ) ) ;
#86006 = ADVANCED_FACE ( 'NONE', ( #21676 ), #106220, .T. ) ;
#86009 = CARTESIAN_POINT ( 'NONE',  ( 6.344852701515477200, 6.504675694630598137, -0.7216878364870257245 ) ) ;
#86008 = CARTESIAN_POINT ( 'NONE',  ( -1.642778471875000035, -3.667708332855373676, -2.845375778867859751 ) ) ;
#86007 = DIRECTION ( 'NONE',  ( 0.000000000000000000, -1.000000000000000000, 0.000000000000000000 ) ) ;
#86010 = CARTESIAN_POINT ( 'NONE',  ( -6.493429226302317225, 6.540365283632955773, 0.7998128361456341429 ) ) ;
#86011 = CARTESIAN_POINT ( 'NONE',  ( 2.958220528980558761, -1.197304571117228100, 1.622486353517027968 ) ) ;
#86012 = CARTESIAN_POINT ( 'NONE',  ( -9.691380875670077444, 10.20103253123691189, 0.7998128361456462443 ) ) ;
#86014 = CARTESIAN_POINT ( 'NONE',  ( -4.281882426504885153, 7.413440659835691449, -1.046679656837728789 ) ) ;
#86013 = CARTESIAN_POINT ( 'NONE',  ( -5.440899717785814715, 5.242137847038546461, 0.7998128361456341429 ) ) ;
#86015 = CARTESIAN_POINT ( 'NONE',  ( 1.500000000000001332, 12.62499999999999645, 0.000000000000000000 ) ) ;
#86016 = CARTESIAN_POINT ( 'NONE',  ( 2.093795543908758994, 0.9691415390508362204, -11.71227324440729411 ) ) ;
#86017 = CARTESIAN_POINT ( 'NONE',  ( 3.834746474454188013E-15, 12.56250000000000000, 1.500000000000001554 ) ) ;
#86019 = CARTESIAN_POINT ( 'NONE',  ( 4.534779904478015489, -1.617806963314952773, 1.203370736114671269 ) ) ;
#86018 = CARTESIAN_POINT ( 'NONE',  ( -8.487040972030346353, 9.003895343564625620, 1.040834085586084257E-14 ) ) ;
#86020 = CARTESIAN_POINT ( 'NONE',  ( 0.7499999999999902300, 4.816666666666684193, -1.299038105676658228 ) ) ;
#86021 = CARTESIAN_POINT ( 'NONE',  ( 1.048929499675733235, -1.357256335890437926, -1.064349854222715885 ) ) ;
#86022 = CARTESIAN_POINT ( 'NONE',  ( 5.363132282657546490, 8.414682208812571673, -1.199719254218452047 ) ) ;
#86024 = CARTESIAN_POINT ( 'NONE',  ( 3.834746474454188013E-15, 10.59375000068279604, 1.500000000000001554 ) ) ;
#86023 = CARTESIAN_POINT ( 'NONE',  ( 7.456621297836072415, 9.722477485607340597, 1.443375672974076540 ) ) ;
#86025 = CARTESIAN_POINT ( 'NONE',  ( -11.04592006821611427, 7.049318325634454041, 4.577072995540873102 ) ) ;
#86026 = CARTESIAN_POINT ( 'NONE',  ( 5.729731410239141454, -1.186140735684092284, -1.446405967604667886 ) ) ;
#86027 = CARTESIAN_POINT ( 'NONE',  ( -0.09313581672419719848, -0.4459848746838651623, -1.970588110806646753 ) ) ;
#86028 = VECTOR ( 'NONE', #156729, 1000.000000000000114 ) ;
#86029 = CARTESIAN_POINT ( 'NONE',  ( -7.065207446052813367, 8.375735120883982532, -1.082531754730549967 ) ) ;
#86030 = ORIENTED_EDGE ( 'NONE', *, *, #21279, .F. ) ;
#86031 = CARTESIAN_POINT ( 'NONE',  ( 10.35806617071623315, 11.18675807536486566, 0.000000000000000000 ) ) ;
#86032 = CARTESIAN_POINT ( 'NONE',  ( 0.3511856949766634095, 0.1948183440376727305, -2.006963311255556714 ) ) ;
#86033 = CARTESIAN_POINT ( 'NONE',  ( 3.973948422136968084, 5.729635473950147606, -1.443375672974068769 ) ) ;
#86034 = DIRECTION ( 'NONE',  ( 5.578564026256490882E-16, 1.000000000000000000, 9.066213480720158442E-32 ) ) ;
#86035 = CARTESIAN_POINT ( 'NONE',  ( 8.609064354553323639, 10.10662517080946543, -1.082531754730543083 ) ) ;
#86036 = CARTESIAN_POINT ( 'NONE',  ( 5.750629710490689384, 9.860818428881154674, -0.7998128361456291469 ) ) ;
#86038 = CARTESIAN_POINT ( 'NONE',  ( 0.2861690844194793026, -0.6482510287857257136, -1.802810126718904504 ) ) ;
#86037 = CARTESIAN_POINT ( 'NONE',  ( -4.554649539187067830, 7.401175998105142817, 1.199719254218464037 ) ) ;
#86039 = AXIS2_PLACEMENT_3D ( 'NONE', #102513, #22295, #120987 ) ;
#86040 = CARTESIAN_POINT ( 'NONE',  ( -11.94105721237522921, 10.07259215598210567, -1.187919463087249605 ) ) ;
#86041 = DIRECTION ( 'NONE',  ( -1.000000000000000000, 1.014813233446432150E-15, 1.972152263052529514E-31 ) ) ;
#86042 = CARTESIAN_POINT ( 'NONE',  ( -1.364683531250000748, -0.6781249996585803075, 0.000000000000000000 ) ) ;
#86044 = EDGE_LOOP ( 'NONE', ( #41863, #183779, #156686, #68615 ) ) ;
#86043 = CARTESIAN_POINT ( 'NONE',  ( 4.690757960648234359, 4.574898496952131133, 0.7216878364870317197 ) ) ;
#86045 = CARTESIAN_POINT ( 'NONE',  ( -3.541704441667874903, 5.155074486744371853, -1.599625672291256295 ) ) ;
#86046 = CARTESIAN_POINT ( 'NONE',  ( 4.083022661009271914, -0.2092679848491978134, -2.151539631373246220 ) ) ;
#86047 = CARTESIAN_POINT ( 'NONE',  ( -5.804299160426229953, 8.825413882922319431, -1.082531754730549967 ) ) ;
#86048 = CARTESIAN_POINT ( 'NONE',  ( 6.861835142292147083, 7.178098218861903135, 0.7216878364870328300 ) ) ;
#86049 = CARTESIAN_POINT ( 'NONE',  ( 1.160570123509139906, 2.118417766304943495, 0.09849428607798524360 ) ) ;
#86050 = CARTESIAN_POINT ( 'NONE',  ( 6.821331453475777629, -0.1281762050449504198, 1.796388512460028286 ) ) ;
#86051 = EDGE_CURVE ( 'NONE', #62971, #184258, #71320, .T. ) ;
#86052 = CARTESIAN_POINT ( 'NONE',  ( 2.671113287583181339, 0.1005484070672260644, -1.968930098583418387 ) ) ;
#86053 = CARTESIAN_POINT ( 'NONE',  ( 4.869353489999923568, -1.618680692612521455, -1.018082601613921723 ) ) ;
#86054 = ORIENTED_EDGE ( 'NONE', *, *, #93974, .T. ) ;
#86055 = CARTESIAN_POINT ( 'NONE',  ( -1.360316468750033980, 2.906250000341399797, -3.469446951953614189E-14 ) ) ;
#86056 = CARTESIAN_POINT ( 'NONE',  ( 5.775830853014204180, -1.921903692836058886, 0.4298591908668251138 ) ) ;
#86057 = CARTESIAN_POINT ( 'NONE',  ( 0.8142755762143333298, 1.794035260217427874, 0.7438321904150380082 ) ) ;
#86058 = EDGE_LOOP ( 'NONE', ( #151666, #27358, #14388 ) ) ;
#86059 = CARTESIAN_POINT ( 'NONE',  ( -4.228163802615396705, 6.026220084508304708, -1.599625672291271394 ) ) ;
#86060 = CARTESIAN_POINT ( 'NONE',  ( -6.102578539926875933, 10.13377570664109051, 0.7216878364870267237 ) ) ;
#86062 = CARTESIAN_POINT ( 'NONE',  ( 5.356880090730857802, 8.303424968277756335, 1.082531754730548412 ) ) ;
#86061 = CARTESIAN_POINT ( 'NONE',  ( 7.091078035147269532, 8.231678114882006625, 1.199719254218462483 ) ) ;
#86064 = ORIENTED_EDGE ( 'NONE', *, *, #15231, .F. ) ;
#86063 = CARTESIAN_POINT ( 'NONE',  ( 5.426388453851806126, -0.8635988772061551355, -1.706256623820540108 ) ) ;
#86065 = CARTESIAN_POINT ( 'NONE',  ( 3.158999515626020216, -1.670948785577108797, 1.441709373268922123 ) ) ;
#86066 = CARTESIAN_POINT ( 'NONE',  ( 1.606762454812577179, -0.7948807482080816333, -2.058825234118460745 ) ) ;
#86067 = AXIS2_PLACEMENT_3D ( 'NONE', #199403, #164796, #16388 ) ;
#86068 = CARTESIAN_POINT ( 'NONE',  ( 0.2999999999999859446, 3.322650755865473204, -0.5865692111442881718 ) ) ;
#86069 = CARTESIAN_POINT ( 'NONE',  ( 0.3285747216504387724, 1.318609938922534530, -1.385187620709791512 ) ) ;
#86070 = CARTESIAN_POINT ( 'NONE',  ( 0.07661050522435490506, 0.2583762315121455599, -1.746200777818290195 ) ) ;
#86071 = CARTESIAN_POINT ( 'NONE',  ( 0.000000000000000000, 6.999999999999999112, 0.000000000000000000 ) ) ;
#86072 = CARTESIAN_POINT ( 'NONE',  ( -0.5707974126488067901, 6.595910036604164084, 3.427880048805499236 ) ) ;
#86073 = CARTESIAN_POINT ( 'NONE',  ( 2.910663983731573090, 0.6951178490613962868, 1.950330170896700022 ) ) ;
#86074 = CARTESIAN_POINT ( 'NONE',  ( -5.599681137644054729, 6.491715067794862293, 1.199719254218450271 ) ) ;
#86075 = CARTESIAN_POINT ( 'NONE',  ( -4.839221724899702259, 8.104102677821947154, -0.8803655321611182361 ) ) ;
#86077 = CARTESIAN_POINT ( 'NONE',  ( 0.2862814217290919894, -1.017545141758866789, 1.907252267444502269 ) ) ;
#86076 = CARTESIAN_POINT ( 'NONE',  ( -2.767835915484202047, 6.380892334706859792, -0.7998128361456281477 ) ) ;
#86078 = CARTESIAN_POINT ( 'NONE',  ( 2.894263506066748093, -0.6386881658498286818, -2.096408367471907841 ) ) ;
#86079 = CARTESIAN_POINT ( 'NONE',  ( -0.2190597442376090720, -0.9782633227147815580, 3.454112556983322424 ) ) ;
#86080 = CARTESIAN_POINT ( 'NONE',  ( 3.106226591306694651, 6.638031766584184368, 0.000000000000000000 ) ) ;
#86081 = CARTESIAN_POINT ( 'NONE',  ( -9.348561386512724170, 4.000007913748541810, -7.001914023932275910 ) ) ;
#86082 = CARTESIAN_POINT ( 'NONE',  ( 0.6823417656249934904, 13.25520833367473195, 1.181850606188764807 ) ) ;
#86083 = CARTESIAN_POINT ( 'NONE',  ( -5.119085517611572378, 8.129960982925583224, 1.199719254218452935 ) ) ;
#86084 = CIRCLE ( 'NONE', #200322, 0.08000000000000020983 ) ;
#86085 = CARTESIAN_POINT ( 'NONE',  ( 6.293613488329289574, 1.277945636399902440, -1.172455961997687535 ) ) ;
#86086 = CARTESIAN_POINT ( 'NONE',  ( -3.928111819657352566, 5.605883094398769195, 1.599625672291267398 ) ) ;
#86087 = CARTESIAN_POINT ( 'NONE',  ( 3.414952709633051864, -1.570776679111930640, 1.348709175982481856 ) ) ;
#86088 = CARTESIAN_POINT ( 'NONE',  ( 4.165693581912960575, 1.384238758890417031, 1.602101081018918904 ) ) ;
#86089 = CARTESIAN_POINT ( 'NONE',  ( 6.745345117998789775, 7.828323044875442172, 1.199719254218462483 ) ) ;
#86090 = CARTESIAN_POINT ( 'NONE',  ( -1.001543065824772872E-14, 5.071875000341421469, 1.575800808251672791 ) ) ;
#86091 = CARTESIAN_POINT ( 'NONE',  ( 3.168761922233914952, 1.429703897159577464, -1.354768240434875759 ) ) ;
#86092 = CARTESIAN_POINT ( 'NONE',  ( 1.212987991671743204, 1.561712320281399835, -1.103468303573502673 ) ) ;
#86093 = CARTESIAN_POINT ( 'NONE',  ( 4.734495095973747070, 0.3888400998970488187, 2.258902165976091059 ) ) ;
#86095 = ADVANCED_FACE ( 'NONE', ( #42256 ), #23833, .F. ) ;
#86094 = CARTESIAN_POINT ( 'NONE',  ( 3.422296110638739286, 1.157362003623555236, -1.411967061744797469 ) ) ;
#86096 = B_SPLINE_CURVE_WITH_KNOTS ( 'NONE', 3,
 ( #78786, #144908, #194673, #145966 ),
 .UNSPECIFIED., .F., .F.,
 ( 4, 4 ),
 ( 0.000000000000000000, 0.002006572499523605075 ),
 .UNSPECIFIED. ) ;
#86097 = CARTESIAN_POINT ( 'NONE',  ( 4.553559489343365740, 6.405848385690952718, -1.599625672291269396 ) ) ;
#86098 = CARTESIAN_POINT ( 'NONE',  ( 6.629573926958101993, 6.836850457647000390, -0.7216878364870257245 ) ) ;
#86099 = CARTESIAN_POINT ( 'NONE',  ( -7.691553217654356622, 7.867900263551875994, -0.7998128361456291469 ) ) ;
#86100 =( BOUNDED_CURVE ( )  B_SPLINE_CURVE ( 2, ( #208380, #93609, #61084, #161798, #76262, #162864, #43794, #211579, #175918 ),
 .UNSPECIFIED., .F., .T. ) 
 B_SPLINE_CURVE_WITH_KNOTS ( ( 3, 2, 2, 2, 3 ),
 ( 0.6718749999999998890, 0.6770833333333333703, 0.6875000000000000000, 0.6979166666666666297, 0.7031250001592646015 ),
 .UNSPECIFIED. ) 
 CURVE ( )  GEOMETRIC_REPRESENTATION_ITEM ( )  RATIONAL_B_SPLINE_CURVE ( ( 0.9330127018922192983, 0.9330127018922178550, 1.000000000000000000, 0.8660254037844387076, 1.000000000000000000, 0.8660254037844387076, 1.000000000000000000, 0.9330126998438279529, 0.9330127018922194093 ) ) 
 REPRESENTATION_ITEM ( '' )  );
#86101 = ADVANCED_FACE ( 'NONE', ( #144047 ), #50481, .F. ) ;
#86102 = CARTESIAN_POINT ( 'NONE',  ( 4.289318580081720178, -0.004264002974461738975, -2.013376228308662252 ) ) ;
#86103 = CARTESIAN_POINT ( 'NONE',  ( 3.203904402660478379, 0.7104733393662396868, -1.828749470067204896 ) ) ;
#86104 = CARTESIAN_POINT ( 'NONE',  ( -6.659026002606323047, 10.92061410301605662, 0.000000000000000000 ) ) ;
#86105 = CARTESIAN_POINT ( 'NONE',  ( -5.925076824372040640, 6.871343368977510302, 1.199719254218450271 ) ) ;
#86107 = EDGE_CURVE ( 'NONE', #182913, #211538, #84565, .T. ) ;
#86106 = CARTESIAN_POINT ( 'NONE',  ( 0.1755611466353291517, 1.991966693188641280, -2.657903234774192658 ) ) ;
#86109 = CARTESIAN_POINT ( 'NONE',  ( 5.664868940362820737, -1.601528614980719967, -0.7536287887903775351 ) ) ;
#86108 = CARTESIAN_POINT ( 'NONE',  ( 0.3102505407175432661, 1.438864707272140775, -1.517118456267575022 ) ) ;
#86110 = CARTESIAN_POINT ( 'NONE',  ( 10.99643026930483991, -5.229832900979420884, -0.2868663046952705242 ) ) ;
#86111 = CARTESIAN_POINT ( 'NONE',  ( 2.449409141518565480, 0.5832169002529237201, -2.112351429719904861 ) ) ;
#86112 = CARTESIAN_POINT ( 'NONE',  ( 6.351467175048743918, 1.735110083250133162, -0.1355937802150069815 ) ) ;
#86113 = AXIS2_PLACEMENT_3D ( 'NONE', #196503, #114258, #180254 ) ;
#86114 = CARTESIAN_POINT ( 'NONE',  ( 5.750629710490689384, 9.860818428881154674, -0.7998128361456291469 ) ) ;
#86115 = CARTESIAN_POINT ( 'NONE',  ( 0.1333692844072802142, 0.2389375359408679178, -2.087895146362698906 ) ) ;
#86116 = CARTESIAN_POINT ( 'NONE',  ( 0.7852881911578631913, 1.155166132482473351, 1.281103752909551030 ) ) ;
#86117 = CARTESIAN_POINT ( 'NONE',  ( 0.8377433530848135135, 0.8832496248250313320, -2.005872107257236969 ) ) ;
#86118 = CARTESIAN_POINT ( 'NONE',  ( 2.965657822035951963, 0.3232568108629539361, -2.182957019552448141 ) ) ;
#86119 = CARTESIAN_POINT ( 'NONE',  ( 0.6202906599508707375, 2.147645164210740365, -0.3171128231679083975 ) ) ;
#86120 = DIRECTION ( 'NONE',  ( -0.000000000000000000, -1.000000000000000000, -0.000000000000000000 ) ) ;
#86121 = CARTESIAN_POINT ( 'NONE',  ( 1.481820193039787403, -0.7077492718140475647, 1.995708955693164199 ) ) ;
#86122 = CARTESIAN_POINT ( 'NONE',  ( 6.727182134110200273, -0.004969159814478123736, 2.189081792362323586 ) ) ;
#86123 = CARTESIAN_POINT ( 'NONE',  ( 5.684577344524033293, -1.879503395548718148, -0.4217397607521166103 ) ) ;
#86124 = EDGE_LOOP ( 'NONE', ( #58512, #25110, #168751, #10752 ) ) ;
#86125 = AXIS2_PLACEMENT_3D ( 'NONE', #25030, #91130, #9850 ) ;
#86127 = CARTESIAN_POINT ( 'NONE',  ( -1.364683531250000748, -0.9281249996585805295, 0.000000000000000000 ) ) ;
#86126 = CARTESIAN_POINT ( 'NONE',  ( 1.365189820700737577, 0.1628935585381158235, -2.286633867385555519 ) ) ;
#86128 = CARTESIAN_POINT ( 'NONE',  ( 2.998324526916512411, 6.649795714711241423, 0.000000000000000000 ) ) ;
#86129 = CARTESIAN_POINT ( 'NONE',  ( 5.524057522564145728, 8.532151978711786100, 1.199719254218462483 ) ) ;
#86130 = CARTESIAN_POINT ( 'NONE',  ( 3.475417139410865275, -1.959577385150832907, -1.046020024706290297 ) ) ;
#86131 = CARTESIAN_POINT ( 'NONE',  ( -8.026063749610061748, 9.426457798375635022, -1.082531754730543971 ) ) ;
#86132 = FILL_AREA_STYLE ('',( #37376 ) ) ;
#86133 = CARTESIAN_POINT ( 'NONE',  ( 4.839897650398541806, 8.590371658866210680, 1.040834085586084257E-14 ) ) ;
#86134 = CARTESIAN_POINT ( 'NONE',  ( -7.334597914868727919, 10.54048608644677465, -1.082531754730543083 ) ) ;
#86135 = EDGE_CURVE ( 'NONE', #80335, #9969, #161325, .T. ) ;
#86136 = CARTESIAN_POINT ( 'NONE',  ( 5.397554552016212703, 8.350878506444006533, 1.082531754730547524 ) ) ;
#86137 = CARTESIAN_POINT ( 'NONE',  ( 1.635388916632842360, 0.6352005984417673501, 1.913803229121699534 ) ) ;
#86139 = CARTESIAN_POINT ( 'NONE',  ( 0.6728087625662204641, 1.424998530877854552, -1.491364779339200641 ) ) ;
#86138 = CARTESIAN_POINT ( 'NONE',  ( 7.832860060393120882, 10.16142270859057462, 1.599625672291281386 ) ) ;
#86140 = CARTESIAN_POINT ( 'NONE',  ( 4.370663978927065152, 5.060324124126029943, 1.009771797811723326 ) ) ;
#86141 = CARTESIAN_POINT ( 'NONE',  ( 4.529832720297257254, 8.298905583739861314, 0.000000000000000000 ) ) ;
#86142 = CARTESIAN_POINT ( 'NONE',  ( -0.006632162239710717895, -1.840811702136424088, -0.04651623371411393176 ) ) ;
#86143 = FILL_AREA_STYLE_COLOUR ( '', #19403 ) ;
#86144 = CARTESIAN_POINT ( 'NONE',  ( -1.201851678989727383E-14, 2.821875000341418804, 1.575800808251672791 ) ) ;
#86145 = CARTESIAN_POINT ( 'NONE',  ( 2.618099050500310998, 1.159573672392331112, -1.336980558935680241 ) ) ;
#86146 = CARTESIAN_POINT ( 'NONE',  ( 1.652970434142877920, 1.038994816082598804, 1.728001345923817267 ) ) ;
#86147 = CARTESIAN_POINT ( 'NONE',  ( 6.497592319816168249, -1.739837010378456617, 0.05289828334312414448 ) ) ;
#86148 = CARTESIAN_POINT ( 'NONE',  ( 5.038769576086907342, -1.967128976631225434, 1.176836258767649745 ) ) ;
#86149 = CARTESIAN_POINT ( 'NONE',  ( 3.380630241506640932, 1.664009615612583204, -0.7882418170854917916 ) ) ;
#86150 = CARTESIAN_POINT ( 'NONE',  ( 9.420217803396747414, 9.884675613584706255, 0.7998128361456462443 ) ) ;
#86151 = CARTESIAN_POINT ( 'NONE',  ( 4.243042751400435186, -1.588269943899191183, 0.8999137264355041577 ) ) ;
#86152 = CARTESIAN_POINT ( 'NONE',  ( 4.711564657724523819, 1.930417226389494090, 0.5826574956761670920 ) ) ;
#86153 = CARTESIAN_POINT ( 'NONE',  ( -9.365985188942097750, 9.821404230054264772, 0.7998128361456462443 ) ) ;
#86155 = CARTESIAN_POINT ( 'NONE',  ( -7.095713291905736853, 9.371694488680407886, 1.599625672291269396 ) ) ;
#86154 = CARTESIAN_POINT ( 'NONE',  ( 3.485499699327331502, 2.046305154993263375, -0.9654624412855338234 ) ) ;
#86156 = CARTESIAN_POINT ( 'NONE',  ( 6.821333371289608927, -0.1635999628400324479, 2.070553102365073173 ) ) ;
#86157 = CARTESIAN_POINT ( 'NONE',  ( -1.500000000000039524, 4.202083334016153415, 0.8660254037844240527 ) ) ;
#86158 = CARTESIAN_POINT ( 'NONE',  ( 3.965334771736851671, 1.774175476309115984, 1.066894043611272824 ) ) ;
#86159 = CARTESIAN_POINT ( 'NONE',  ( 4.552840656090682891, 4.206068941727564514, 1.214306433183764966E-14 ) ) ;
#86160 = CARTESIAN_POINT ( 'NONE',  ( -0.6801582343750282034, 1.963541667008045222, 1.178068619123803451 ) ) ;
#86161 = SHAPE_DEFINITION_REPRESENTATION ( #128549, #188305 ) ;
#86163 = CARTESIAN_POINT ( 'NONE',  ( 2.051278105266049590, -1.547248087829168339, -1.147608674410576901 ) ) ;
#86162 = CARTESIAN_POINT ( 'NONE',  ( -7.655550293210764856, 12.08322577538792331, 0.000000000000000000 ) ) ;
#86164 = UNCERTAINTY_MEASURE_WITH_UNIT (LENGTH_MEASURE( 1.000000000000000082E-05 ), #137126, 'distance_accuracy_value', 'NONE');
#86165 = CARTESIAN_POINT ( 'NONE',  ( 4.879410147971470657, 4.944948943068641967, -0.7687999843507594688 ) ) ;
#86166 = CARTESIAN_POINT ( 'NONE',  ( 0.2210688645036896216, -1.757681936009440893, -0.8888059845142733950 ) ) ;
#86167 = CARTESIAN_POINT ( 'NONE',  ( 5.248414861821569133, 6.256143772614186638, -1.082531754730548412 ) ) ;
#86168 = CARTESIAN_POINT ( 'NONE',  ( 5.892592298951464969, 5.976936425253049912, 0.01597356071081010298 ) ) ;
#86169 = CARTESIAN_POINT ( 'NONE',  ( -5.796211742350026341, 6.069872996917573538, -0.5622600474562855499 ) ) ;
#86170 = CARTESIAN_POINT ( 'NONE',  ( -3.846762897975357198, 5.510976019103107859, -1.599625672291256295 ) ) ;
#86171 = CARTESIAN_POINT ( 'NONE',  ( 0.6334296782557496952, 2.055416226174343386, 0.8430641771750585489 ) ) ;
#86172 = CARTESIAN_POINT ( 'NONE',  ( 3.557739748072580088, 0.5135893094758836597, -2.042235538380641202 ) ) ;
#86173 = CARTESIAN_POINT ( 'NONE',  ( -5.912237504011027767, 9.055304967058290799, 1.199719254218454489 ) ) ;
#86174 = CARTESIAN_POINT ( 'NONE',  ( 6.154511665599609493, 9.267681812253174556, 1.199719254218462483 ) ) ;
#86175 = CARTESIAN_POINT ( 'NONE',  ( 1.029495724655055344, 1.794938190532389788, -0.4914328765713778524 ) ) ;
#86176 = CARTESIAN_POINT ( 'NONE',  ( 5.289652487626049115, 9.323011668872403845, 0.7998128361456462443 ) ) ;
#86177 = CARTESIAN_POINT ( 'NONE',  ( 4.147904930777053245, 6.926640621626830807, -1.199719254218452047 ) ) ;
#86178 = CARTESIAN_POINT ( 'NONE',  ( -7.783789588021474692, 8.253711738879413673, 0.7216878364870317197 ) ) ;
#86179 = CARTESIAN_POINT ( 'NONE',  ( -7.537970219518075332, 10.77775377520434574, -1.082531754730543971 ) ) ;
#86181 = CARTESIAN_POINT ( 'NONE',  ( 1.441811196653530747, -1.994930912159533332, 0.7194735443712959588 ) ) ;
#86180 = AXIS2_PLACEMENT_3D ( 'NONE', #46728, #62946, #61893 ) ;
#86182 = CARTESIAN_POINT ( 'NONE',  ( -7.910256278930404505, 8.193330178365746619, -0.7998128361456362523 ) ) ;
#86184 = CARTESIAN_POINT ( 'NONE',  ( 4.264078424595136418, -1.956757550135434620, 0.1421211968542570592 ) ) ;
#86183 = CARTESIAN_POINT ( 'NONE',  ( -1.225000000000019407, 1.250000000000028866, -1.734723475976807094E-14 ) ) ;
#86185 = CARTESIAN_POINT ( 'NONE',  ( 2.870174731959000525, 1.155358403710282866, 1.826860881501219280 ) ) ;
#86186 = CARTESIAN_POINT ( 'NONE',  ( 2.208333698829296310, 1.645431377724184463, 0.8263914577605266931 ) ) ;
#86187 = CARTESIAN_POINT ( 'NONE',  ( -4.073306942994160629, 7.542743630792291043, -0.4897309385070089394 ) ) ;
#86188 = CARTESIAN_POINT ( 'NONE',  ( 4.962738864268898098, 0.1657098081031352088, -1.732421123976911836 ) ) ;
#86189 = CARTESIAN_POINT ( 'NONE',  ( -9.117697077653634352, 15.00000000001154987, -7.299999999986293453 ) ) ;
#86190 = CARTESIAN_POINT ( 'NONE',  ( 6.046573322014824114, 7.117052299514516456, -1.082531754730543083 ) ) ;
#86191 = CARTESIAN_POINT ( 'NONE',  ( -9.997720234198379075, 5.662301760159435204, -5.943093865039206669 ) ) ;
#86192 = CARTESIAN_POINT ( 'NONE',  ( 2.237400686453533183, -1.931180590798301955, 0.9714560045831142077 ) ) ;
#86193 = CARTESIAN_POINT ( 'NONE',  ( 2.899767358622063806, 0.2439914025648345919, 2.001204936777578602 ) ) ;
#86194 = LINE ( 'NONE', #3838, #172568 ) ;
#86195 = CARTESIAN_POINT ( 'NONE',  ( 1.727627455807039691, -2.035446057602477321, 0.7283451284763039490 ) ) ;
#86196 = CARTESIAN_POINT ( 'NONE',  ( 3.977382581243666504, 1.856787152588537548, -0.6629638669850937971 ) ) ;
#86197 = CARTESIAN_POINT ( 'NONE',  ( 6.509000000000033204, 1.287336644856639456, 2.017667062298739822 ) ) ;
#86198 = CARTESIAN_POINT ( 'NONE',  ( 3.632312094575868677, 0.2880498525525148623, 1.920478541846024179 ) ) ;
#86200 = ORIENTED_EDGE ( 'NONE', *, *, #149058, .T. ) ;
#86199 = DIRECTION ( 'NONE',  ( 0.8594130494132222742, -0.03761243564701257508, -0.5098965730253202100 ) ) ;
#86201 = CARTESIAN_POINT ( 'NONE',  ( -3.919715807682309094, 6.626733304721049933, 1.082531754730549967 ) ) ;
#86202 = CARTESIAN_POINT ( 'NONE',  ( -0.1110810684432622653, 5.724789179085956192, -2.391029204513066553 ) ) ;
#86203 = CARTESIAN_POINT ( 'NONE',  ( 5.248941747146098180, 6.152795455539095570, -1.199719254218452047 ) ) ;
#86204 = CARTESIAN_POINT ( 'NONE',  ( -5.978219388983010418, 5.939287140093762574, -0.7998128361456362523 ) ) ;
#86206 = ORIENTED_EDGE ( 'NONE', *, *, #128408, .T. ) ;
#86205 = CARTESIAN_POINT ( 'NONE',  ( -5.986807348886189040, 9.142303119412650503, -1.199719254218452047 ) ) ;
#86207 = CARTESIAN_POINT ( 'NONE',  ( -10.10046125205659173, 10.88621900359527572, -0.7216878364870267237 ) ) ;
#86208 = CARTESIAN_POINT ( 'NONE',  ( 0.1127427399064059588, -0.9454589178800475446, -1.991880357201977425 ) ) ;
#86209 = CARTESIAN_POINT ( 'NONE',  ( 2.960184520039609524, -4.109567588314592790, -1.425549731837409961 ) ) ;
#86210 = CARTESIAN_POINT ( 'NONE',  ( 3.801568999928582659, -1.482573837031101016, -1.284759613706359271 ) ) ;
#86211 = CARTESIAN_POINT ( 'NONE',  ( 7.476431642932036326, 10.80992178580769014, 1.199719254218460707 ) ) ;
#86212 = CARTESIAN_POINT ( 'NONE',  ( 1.266250242576156815, 1.862016182229693673, -0.7743172429433077264 ) ) ;
#86213 = EDGE_LOOP ( 'NONE', ( #209007, #14144, #105405, #70850 ) ) ;
#86214 = CARTESIAN_POINT ( 'NONE',  ( 3.011064194431464003, 0.05668958241028876355, 2.116758953476727267 ) ) ;
#86215 = CARTESIAN_POINT ( 'NONE',  ( 1.499999999999987121, 1.535416667349486453, 0.8660254037844524744 ) ) ;
#86217 = CARTESIAN_POINT ( 'NONE',  ( -5.717788096661253761, 7.693838750903348789, 1.599625672291269396 ) ) ;
#86216 = DIRECTION ( 'NONE',  ( 5.578564026256504688E-16, 1.000000000000000000, 9.066213480720158442E-32 ) ) ;
#86218 = CARTESIAN_POINT ( 'NONE',  ( 2.712652182946372559, -0.1802803596865458491, 1.832282175343015407 ) ) ;
#86219 = EDGE_LOOP ( 'NONE', ( #69282, #144710, #197279, #11202 ) ) ;
#86220 = CARTESIAN_POINT ( 'NONE',  ( -9.020252271793614440, 9.418049160047695878, 0.7998128361456462443 ) ) ;
#86221 = CARTESIAN_POINT ( 'NONE',  ( 0.2999999999999511391, 3.322650755865479866, 0.5865692111442165624 ) ) ;
#86222 = CARTESIAN_POINT ( 'NONE',  ( 4.201511661969238531, 1.892856375164463367, -0.9562558712687405649 ) ) ;
#86223 = DIRECTION ( 'NONE',  ( 0.000000000000000000, 0.000000000000000000, 1.000000000000000000 ) ) ;
#86224 = CARTESIAN_POINT ( 'NONE',  ( 7.287671262545424966, 8.461036880179857889, -1.199719254218451159 ) ) ;
#86225 = CARTESIAN_POINT ( 'NONE',  ( 5.096976104305405819, 1.715636550957209794, -1.141348886549067077 ) ) ;
#86226 = AXIS2_PLACEMENT_3D ( 'NONE', #46035, #178159, #147792 ) ;
#86228 = CARTESIAN_POINT ( 'NONE',  ( 2.419273308677453826, -1.061688697878185206, -1.504126257600538974 ) ) ;
#86227 = CARTESIAN_POINT ( 'NONE',  ( -8.050844288416501016, 8.287073179441051707, 1.040834085586084257E-14 ) ) ;
#86229 = CARTESIAN_POINT ( 'NONE',  ( 9.423080456697809026, 10.95234760669099749, -1.199719254218446718 ) ) ;
#86230 = FACE_BOUND ( 'NONE', #123787, .T. ) ;
#86231 = CARTESIAN_POINT ( 'NONE',  ( -7.553827861469316396, 8.841829255582865699, -1.199719254218452047 ) ) ;
#86232 = CYLINDRICAL_SURFACE ( 'NONE', #70115, 1.500000000000000222 ) ;
#86233 = CARTESIAN_POINT ( 'NONE',  ( 2.719571217284349363, -0.2154062111461417517, 2.196339928330424129 ) ) ;
#86234 = CARTESIAN_POINT ( 'NONE',  ( 4.710415318105323657, -0.9616676431317521256, -2.047968690232481848 ) ) ;
#86235 = CARTESIAN_POINT ( 'NONE',  ( -6.399085315970132193, 10.40942393536641397, -0.7216878364870278340 ) ) ;
#86236 = CARTESIAN_POINT ( 'NONE',  ( 5.203285271772914555, 1.593979872821064570, -0.8609055379997750945 ) ) ;
#86237 = CARTESIAN_POINT ( 'NONE',  ( 4.522610612662866458, 0.3335214923718023416, 1.886305606834618231 ) ) ;
#86238 = CARTESIAN_POINT ( 'NONE',  ( 0.6823417656249899377, 4.238541667008085767, -1.181850606188754593 ) ) ;
#86239 = ADVANCED_FACE ( 'NONE', ( #195957 ), #78989, .F. ) ;
#86240 = CARTESIAN_POINT ( 'NONE',  ( 3.414874914781691473, 1.781649806626634858, 0.8443359948157087569 ) ) ;
#86241 = CARTESIAN_POINT ( 'NONE',  ( 5.506679003988666388, 1.415762158562785533, -1.222804595763474333 ) ) ;
#86242 = MECHANICAL_DESIGN_GEOMETRIC_PRESENTATION_REPRESENTATION (  '', ( #158924 ), #24073 ) ;
#86243 = CARTESIAN_POINT ( 'NONE',  ( 5.283604245000163679, -1.767202373759840572, 0.5838029059755837080 ) ) ;
#86244 = CARTESIAN_POINT ( 'NONE',  ( 0.6823417656249899377, 5.176041667008086655, -1.181850606188754593 ) ) ;
#86245 = CARTESIAN_POINT ( 'NONE',  ( 0.6554828803995507158, 1.942095732595986890, -0.5424746339172461518 ) ) ;
#86247 = CARTESIAN_POINT ( 'NONE',  ( 1.875742097524640384, 2.014971663898405652, -0.6126918839576761533 ) ) ;
#86246 = CARTESIAN_POINT ( 'NONE',  ( -2.887523529586332405, 5.352232636950553513, 1.082531754730560403 ) ) ;
#86248 = CARTESIAN_POINT ( 'NONE',  ( 10.23370702021670020, 10.83374636654133383, 0.7998128361456462443 ) ) ;
#86250 = CARTESIAN_POINT ( 'NONE',  ( -10.47775378526269918, 11.11846759242831872, -0.7998128361456221525 ) ) ;
#86249 = CARTESIAN_POINT ( 'NONE',  ( -1.364683531250010295, 4.842708333674756283, 0.7879004041258379498 ) ) ;
#86251 = CARTESIAN_POINT ( 'NONE',  ( 2.971057270251746818, -1.603071526910588629, 1.388259434452358665 ) ) ;
#86252 = CARTESIAN_POINT ( 'NONE',  ( 3.563261906135759993, 6.332667919118538435, -2.420000000000000373 ) ) ;
#86253 = CARTESIAN_POINT ( 'NONE',  ( 0.9494800659552645739, -1.824215446917340389, 0.8674010940010259407 ) ) ;
#86254 = CARTESIAN_POINT ( 'NONE',  ( 0.6823417656249899377, 2.592708333674753618, 1.181850606188767472 ) ) ;
#86255 = CARTESIAN_POINT ( 'NONE',  ( -3.145128448690323264, 4.692402494937224056, -1.443375672974059665 ) ) ;
#86256 = CARTESIAN_POINT ( 'NONE',  ( 5.118366684358879759, 5.930181538962194132, 1.199719254218462483 ) ) ;
#86257 = ORIENTED_EDGE ( 'NONE', *, *, #80161, .F. ) ;
#86258 = CARTESIAN_POINT ( 'NONE',  ( 1.985828983967323325, 1.489073237690191176, 1.567133960648490199 ) ) ;
#86259 = DIRECTION ( 'NONE',  ( 0.000000000000000000, 1.000000000000000000, 0.000000000000000000 ) ) ;
#86262 = CARTESIAN_POINT ( 'NONE',  ( 6.639320575229281651, -0.0007625845807879281287, 2.103388539994067497 ) ) ;
#86261 = DIRECTION ( 'NONE',  ( 1.000000000000000000, 0.000000000000000000, 0.000000000000000000 ) ) ;
#86260 = CARTESIAN_POINT ( 'NONE',  ( 3.074666975249065626, 6.809138247757705820, 0.000000000000000000 ) ) ;
#86263 = CARTESIAN_POINT ( 'NONE',  ( 10.66990370383054731, 11.55056853066490952, 0.7216878364870317197 ) ) ;
#86264 = CARTESIAN_POINT ( 'NONE',  ( -7.827294160508087906, -6.717993526550283256, 7.547439985188244549 ) ) ;
#86265 = CARTESIAN_POINT ( 'NONE',  ( -8.188761592974046266, 10.57664116326830595, -1.443375672974059665 ) ) ;
#86266 = CARTESIAN_POINT ( 'NONE',  ( 0.4159077360078728969, -1.177411712353953588, -1.848246096435968600 ) ) ;
#86267 = DIRECTION ( 'NONE',  ( -0.000000000000000000, 1.000000000000000000, -0.000000000000000000 ) ) ;
#86269 = CARTESIAN_POINT ( 'NONE',  ( 1.364683531249997417, 11.48437500034139802, 2.602085213965210642E-15 ) ) ;
#86268 = CARTESIAN_POINT ( 'NONE',  ( 1.253188901120566134, -1.782426524439745030, 1.393456103103172250 ) ) ;
#86270 = CARTESIAN_POINT ( 'NONE',  ( -7.808606406466886973, 11.19745900993164511, 1.199719254218453823 ) ) ;
#86271 = CARTESIAN_POINT ( 'NONE',  ( -3.917943204224914933, 6.554388924028945240, -1.082531754730548412 ) ) ;
#86273 = CIRCLE ( 'NONE', #210735, 0.07999999999999996003 ) ;
#86272 = CARTESIAN_POINT ( 'NONE',  ( -0.6823417656250212460, 1.863541667008083991, 1.181850606188755259 ) ) ;
#86274 = CARTESIAN_POINT ( 'NONE',  ( -1.500000000000039524, 4.420833333333351156, 0.8660254037844240527 ) ) ;
#86275 = CARTESIAN_POINT ( 'NONE',  ( 0.7500000000000006661, 10.16666666666667140, -1.299038105676657340 ) ) ;
#86276 = CARTESIAN_POINT ( 'NONE',  ( 4.547283022377748729, -1.335744037758682667, -1.091317429222604884 ) ) ;
#86277 = CARTESIAN_POINT ( 'NONE',  ( 4.203910148689107729, 7.062256385849379647, -1.199719254218448494 ) ) ;
#86278 = CARTESIAN_POINT ( 'NONE',  ( 1.756752346989236768, -1.514669478205426190, -0.9150583790542564655 ) ) ;
#86279 = CARTESIAN_POINT ( 'NONE',  ( 2.719391910328097683, 1.701792079550172421, 1.075097526896612088 ) ) ;
#86280 = CARTESIAN_POINT ( 'NONE',  ( 5.614374367772542840, -0.9875226594672004143, -1.973556357105679115 ) ) ;
#86281 = ORIENTED_EDGE ( 'NONE', *, *, #50401, .T. ) ;
#86283 = CARTESIAN_POINT ( 'NONE',  ( 3.955335691828856692, -1.755346444749112722, 0.9990557238469994772 ) ) ;
#86282 = CIRCLE ( 'NONE', #155394, 1.249999999999999778 ) ;
#86284 = CARTESIAN_POINT ( 'NONE',  ( -7.761116589180078407, 8.019333873657032541, 0.000000000000000000 ) ) ;
#86286 = CARTESIAN_POINT ( 'NONE',  ( 4.411732571322396268, -1.242743209197882059, -1.587826168943158089 ) ) ;
#86285 = CARTESIAN_POINT ( 'NONE',  ( 5.127636373287420390, -0.3106611864900839515, 2.097473367668806876 ) ) ;
#86288 = ORIENTED_EDGE ( 'NONE', *, *, #110858, .T. ) ;
#86287 = CARTESIAN_POINT ( 'NONE',  ( 4.429823666617582312, -1.775263289385048848, 0.3600210208860327721 ) ) ;
#86289 = ORIENTED_EDGE ( 'NONE', *, *, #136321, .F. ) ;
#86290 = CARTESIAN_POINT ( 'NONE',  ( 2.201827603038747139, -1.870314503716500099, 0.04339327950253490246 ) ) ;
#86291 = CARTESIAN_POINT ( 'NONE',  ( -11.97181073603049839, 11.37999999999999901, -0.8318477717169578955 ) ) ;
#86292 = CARTESIAN_POINT ( 'NONE',  ( 1.740342883905017013, 1.098329146349947827, -1.565357986077076990 ) ) ;
#86293 = CARTESIAN_POINT ( 'NONE',  ( 6.385527162356455122, 10.39360608948380538, 1.056142170575426150E-14 ) ) ;
#86294 = CARTESIAN_POINT ( 'NONE',  ( -10.20559888102932256, 5.000029895416906456, -7.525687786258633771 ) ) ;
#86295 = DIRECTION ( 'NONE',  ( 0.6123724356957872539, 0.7071067811865541231, -0.3535533905932732313 ) ) ;
#86296 = B_SPLINE_CURVE_WITH_KNOTS ( 'NONE', 3,
 ( #188150, #39781, #111245, #143725, #62420, #63492, #61363, #131730, #144790, #94949 ),
 .UNSPECIFIED., .F., .F.,
 ( 4, 1, 1, 1, 1, 1, 1, 4 ),
 ( 0.000000000000000000, 0.09090790722575105287, 0.1825853934691276381, 0.2551728700554835028, 0.3603391217242263855, 0.5205903519787860034, 0.7335386666926504429, 0.9999999999999998890 ),
 .UNSPECIFIED. ) ;
#86297 = CARTESIAN_POINT ( 'NONE',  ( -1.364683531249997417, 2.571875000341422357, 1.214306433183764966E-14 ) ) ;
#86298 = CARTESIAN_POINT ( 'NONE',  ( 0.08795244648929222142, 1.102731429460445334, 1.562230693318837238 ) ) ;
#86299 = CARTESIAN_POINT ( 'NONE',  ( 5.939880696562888751, 7.062853913145737295, -1.082531754730548412 ) ) ;
#86300 = CARTESIAN_POINT ( 'NONE',  ( 1.187862215860764126, -1.241893603568875903, -1.518774446641702580 ) ) ;
#86301 = CARTESIAN_POINT ( 'NONE',  ( 6.735557395310444981E-16, 7.999999999999992895, -5.500000000000002665 ) ) ;
#86302 = CARTESIAN_POINT ( 'NONE',  ( -5.367048706163331850, 7.354919138647580290, -1.599625672291271394 ) ) ;
#86303 = CARTESIAN_POINT ( 'NONE',  ( 3.691739789689612472, 1.995538565534977549, -0.7177698711837015022 ) ) ;
#86304 = CARTESIAN_POINT ( 'NONE',  ( 10.09812548408005384, 10.67556790771522124, -0.7998128361456281477 ) ) ;
#86305 = CARTESIAN_POINT ( 'NONE',  ( 5.255133876903111734, -1.663856106090171538, -1.057019077474026680 ) ) ;
#86306 = CARTESIAN_POINT ( 'NONE',  ( 1.364683531249986537, 0.8635416670080893198, 0.7879004041258500513 ) ) ;
#86307 = ORIENTED_EDGE ( 'NONE', *, *, #164010, .T. ) ;
#86308 = CARTESIAN_POINT ( 'NONE',  ( 1.634521315757204940, 0.6676430208681031209, 2.009258352967583150 ) ) ;
#86309 = CARTESIAN_POINT ( 'NONE',  ( 10.37552651436754836, 9.126834862229522116, 6.082233718396662603 ) ) ;
#86310 = CARTESIAN_POINT ( 'NONE',  ( 2.348173244826061268, -0.8873571809006628452, 1.870714752860686447 ) ) ;
#86311 = CARTESIAN_POINT ( 'NONE',  ( 3.542423274920540432, 7.354853930707762721, -1.734723475976807094E-15 ) ) ;
#86312 = CARTESIAN_POINT ( 'NONE',  ( 6.333594036239346359, 7.418223126147930557, 1.199719254218453823 ) ) ;
#86313 = ORIENTED_EDGE ( 'NONE', *, *, #203350, .F. ) ;
#86315 = CARTESIAN_POINT ( 'NONE',  ( 4.867540842506059562, 5.637551390133895168, -1.199719254218452047 ) ) ;
#86314 = CARTESIAN_POINT ( 'NONE',  ( 5.156232390734752258, -1.514662699498746878, 1.441270160984737370 ) ) ;
#86318 = VERTEX_POINT ( 'NONE', #214278 ) ;
#86317 = CARTESIAN_POINT ( 'NONE',  ( 1.348006360704995910, 0.8929448326314154416, -1.575985355173844527 ) ) ;
#86316 = CARTESIAN_POINT ( 'NONE',  ( 2.942213871598580166, 1.811567870905493205, 0.2252638538085757203 ) ) ;
#86319 = CARTESIAN_POINT ( 'NONE',  ( 6.691986956589398794, -0.9478133180038283978, 1.990996264204819122 ) ) ;
#86320 = DIRECTION ( 'NONE',  ( -0.9782075119097819460, 0.1245777785625464124, 0.1661037047500602826 ) ) ;
#86321 = CARTESIAN_POINT ( 'NONE',  ( 10.14216661378989848, 13.64382096325071458, 7.299002950830796088 ) ) ;
#86322 = CARTESIAN_POINT ( 'NONE',  ( 5.139771110516938357, -1.557344429106276573, -1.563758303505815794 ) ) ;
#86323 = CARTESIAN_POINT ( 'NONE',  ( 0.6823417656249934904, 9.005208333674726617, 1.181850606188764807 ) ) ;
#86324 = ORIENTED_EDGE ( 'NONE', *, *, #126186, .F. ) ;
#86325 = CARTESIAN_POINT ( 'NONE',  ( 4.389254143344611947, -0.003399479254035177832, -1.912461472815998320 ) ) ;
#86326 = CARTESIAN_POINT ( 'NONE',  ( -2.948008335967658322, 5.526761261015804116, 1.199719254218462483 ) ) ;
#86327 = PRESENTATION_LAYER_ASSIGNMENT (  '', '', ( #41519 ) ) ;
#86328 = CARTESIAN_POINT ( 'NONE',  ( 7.934546212495622086, 10.28005655271014795, -1.599625672291262513 ) ) ;
#86329 = CARTESIAN_POINT ( 'NONE',  ( 6.549288556030709252, 1.803345607721940524, -1.016871928424131877 ) ) ;
#86330 = CARTESIAN_POINT ( 'NONE',  ( -0.4019237886466933696, 10.33258545099817027, 1.500000000000005995 ) ) ;
#86331 = CARTESIAN_POINT ( 'NONE',  ( 4.595850884908202261, 7.345281218159464665, -1.082531754730549078 ) ) ;
#86332 = CARTESIAN_POINT ( 'NONE',  ( 6.093348126157794198, -0.7399906200981146709, 2.062998119606203939 ) ) ;
#86333 = FACE_OUTER_BOUND ( 'NONE', #194049, .T. ) ;
#86334 = CARTESIAN_POINT ( 'NONE',  ( -0.9037479196795165093, 15.51845925029282114, -11.99999999996284750 ) ) ;
#86335 = ORIENTED_EDGE ( 'NONE', *, *, #199147, .F. ) ;
#86336 = CARTESIAN_POINT ( 'NONE',  ( -0.9311234436981447038, -2.171869630441516374, -3.475000000000004086 ) ) ;
#86337 = CARTESIAN_POINT ( 'NONE',  ( 3.971829172498120286, 1.036919360001643531, 1.556626693588740062 ) ) ;
#86338 = CARTESIAN_POINT ( 'NONE',  ( -1.642778471875000035, -2.005208332855376696, -2.845375778867859751 ) ) ;
#86339 = DIRECTION ( 'NONE',  ( 0.7592566023653005702, -0.6507913734559639396, 0.000000000000000000 ) ) ;
#86340 = CARTESIAN_POINT ( 'NONE',  ( -8.026063749610061748, 9.426457798375635022, -1.082531754730543971 ) ) ;
#86341 = CARTESIAN_POINT ( 'NONE',  ( 5.032011289327418702, 5.899709921417326974, 1.199719254218452935 ) ) ;
#86342 = CARTESIAN_POINT ( 'NONE',  ( 5.555090253297246150, 7.504024600312024340, 1.599625672291267398 ) ) ;
#86343 = CARTESIAN_POINT ( 'NONE',  ( 0.6374758831957715310, 1.839649526063956042, -0.7036667969960698210 ) ) ;
#86344 = EDGE_CURVE ( 'NONE', #195087, #201525, #43165, .T. ) ;
#86345 = CARTESIAN_POINT ( 'NONE',  ( 1.581657880887325174, -0.6766953518495041342, 1.899626397962331126 ) ) ;
#86346 = CARTESIAN_POINT ( 'NONE',  ( -8.784793466650835825, 12.33634391347959713, 1.199719254218462483 ) ) ;
#86347 = CARTESIAN_POINT ( 'NONE',  ( 6.879836604291781121, 6.991173891287354003, -0.7998128361456341429 ) ) ;
#86348 = DIRECTION ( 'NONE',  ( 1.000000000000000000, -0.000000000000000000, -0.000000000000000000 ) ) ;
#86349 = CARTESIAN_POINT ( 'NONE',  ( 1.728746526384251858, 0.2170652002222578369, 2.180672313318913869 ) ) ;
#86350 = CARTESIAN_POINT ( 'NONE',  ( 6.410779360540267646, 1.349177972556347971, -1.230185023894624141 ) ) ;
#86351 = CARTESIAN_POINT ( 'NONE',  ( -2.272963308585411735, 5.803540959991587478, 0.7998128361456341429 ) ) ;
#86352 = CARTESIAN_POINT ( 'NONE',  ( 5.234856708652227297, 7.200695141551334721, 1.443375672974065660 ) ) ;
#86353 = CARTESIAN_POINT ( 'NONE',  ( 8.398386088661320414, 11.88553530582519357, -1.199719254218446718 ) ) ;
#86354 = CARTESIAN_POINT ( 'NONE',  ( 4.162516854595432747, 4.815023404238158555, 1.199719254218464037 ) ) ;
#86355 = CARTESIAN_POINT ( 'NONE',  ( 5.858531774880875176, 9.849054480754103835, -0.7216878364870458196 ) ) ;
#86356 = VERTEX_POINT ( 'NONE', #180760 ) ;
#86358 = CARTESIAN_POINT ( 'NONE',  ( 0.9791529934419791470, -1.820790759202662423, -0.8588917989246074303 ) ) ;
#86357 = CARTESIAN_POINT ( 'NONE',  ( 4.124425300631988200, 0.09459923933386081563, 1.838956108544815171 ) ) ;
#86359 = CARTESIAN_POINT ( 'NONE',  ( 1.669710354559012622, -0.8274895997400324443, -2.144421126502197517 ) ) ;
#86361 = CARTESIAN_POINT ( 'NONE',  ( 1.375590602687895458, -1.817075280682054927, 0.4009801126106312674 ) ) ;
#86360 = CARTESIAN_POINT ( 'NONE',  ( 2.724825686666657809, 6.122787701178987518, 0.000000000000000000 ) ) ;
#86362 = CARTESIAN_POINT ( 'NONE',  ( 1.737499999999999378, -0.4666666666666673402, -3.009438278150925683 ) ) ;
#86363 = CARTESIAN_POINT ( 'NONE',  ( -4.928552533767591726, 5.708731696605642725, 1.199719254218462483 ) ) ;
#86364 = CARTESIAN_POINT ( 'NONE',  ( 4.582993027900885252, 6.853944465854098667, -1.265546273303337133 ) ) ;
#86365 = CARTESIAN_POINT ( 'NONE',  ( 4.025576834063953946, -0.3218090080209669024, 1.884953445776993863 ) ) ;
#86366 = B_SPLINE_CURVE_WITH_KNOTS ( 'NONE', 3,
 ( #154988, #122581, #138749, #105189, #153926, #23897, #190661, #171226, #90003, #206919 ),
 .UNSPECIFIED., .F., .F.,
 ( 4, 2, 2, 2, 4 ),
 ( 0.000000000000000000, 0.0002334048330869030008, 0.0004668096661738060016, 0.0007002144992607089481, 0.0009336193323476120031 ),
 .UNSPECIFIED. ) ;
#86367 = CARTESIAN_POINT ( 'NONE',  ( -8.435144125996554720, 12.99275191363802229, 0.7998128361456341429 ) ) ;
#86369 = EDGE_CURVE ( 'NONE', #40348, #123271, #214128, .T. ) ;
#86368 = CARTESIAN_POINT ( 'NONE',  ( 6.457572779797339457, 6.769951385671206801, 0.3193968722623799494 ) ) ;
#86370 = CARTESIAN_POINT ( 'NONE',  ( -2.823841133396259639, 6.516508098929413961, -0.7998128361456481317 ) ) ;
#86372 = CARTESIAN_POINT ( 'NONE',  ( 2.412791964582483129, 1.669947582624079274, 0.8431454209596804805 ) ) ;
#86371 = CARTESIAN_POINT ( 'NONE',  ( 4.265234282975380431, 2.027484720304991495, -0.5098422324811486828 ) ) ;
#86373 = CARTESIAN_POINT ( 'NONE',  ( 8.432808358020025707, 9.900993174853955026, 1.082531754730558626 ) ) ;
#86374 = CARTESIAN_POINT ( 'NONE',  ( 0.6823417656249917140, 5.155208333674749177, 1.181850606188765695 ) ) ;
#86375 = CARTESIAN_POINT ( 'NONE',  ( 3.139928233896288390, 0.4259470162499751633, 1.687361108405739385 ) ) ;
#86376 = VECTOR ( 'NONE', #99325, 1000.000000000000000 ) ;
#86377 = CARTESIAN_POINT ( 'NONE',  ( 5.359550796103802028, 5.147230771742885125, -0.7998128361456231517 ) ) ;
#86379 = CARTESIAN_POINT ( 'NONE',  ( 4.568734577680872988, 6.353276312092901890, -1.443375672974051449 ) ) ;
#86378 = CARTESIAN_POINT ( 'NONE',  ( 5.985929146193681660, 5.992403464881949304, 0.1705357982419167806 ) ) ;
#86380 = CARTESIAN_POINT ( 'NONE',  ( 3.615580125028591052, -1.699004861347377604, 0.2966152939984505466 ) ) ;
#86381 = CARTESIAN_POINT ( 'NONE',  ( 3.527062600443749307, -2.024233912922444478, 0.8403589366152917073 ) ) ;
#86382 = CARTESIAN_POINT ( 'NONE',  ( 5.936183876523434932, 1.091049494364674466, -1.918236432931222257 ) ) ;
#86383 = CARTESIAN_POINT ( 'NONE',  ( 6.983263157960362122, 2.430545403621493072, 2.435370848939223620 ) ) ;
#86384 = CARTESIAN_POINT ( 'NONE',  ( 3.362351297888244606, -2.168775535925556053, 0.1018362995675748534 ) ) ;
#86385 = CARTESIAN_POINT ( 'NONE',  ( 1.805030607383810715, 1.517133602069477893, 1.015288170653723343 ) ) ;
#86386 = CARTESIAN_POINT ( 'NONE',  ( 1.850000000000000089, 4.013456704145457099E-20, 0.5999999999999969802 ) ) ;
#86387 = CARTESIAN_POINT ( 'NONE',  ( 4.909417703775454278, -2.009542366629351484, 0.6670832617777838758 ) ) ;
#86388 = VERTEX_POINT ( 'NONE', #912 ) ;
#86390 = CARTESIAN_POINT ( 'NONE',  ( 1.364683531249988757, 2.446875000341415696, 1.214306433183764966E-14 ) ) ;
#86389 = CARTESIAN_POINT ( 'NONE',  ( 4.810265146351084375, 1.581823803905563430, -1.659390399702101337 ) ) ;
#86391 = CARTESIAN_POINT ( 'NONE',  ( 6.720655732516641834, 2.102516797890502165, 2.037305422295607293 ) ) ;
#86392 = CARTESIAN_POINT ( 'NONE',  ( 9.673906298550626559, 11.24497775551929557, 1.199719254218452047 ) ) ;
#86393 = CARTESIAN_POINT ( 'NONE',  ( 0.7859742890132662696, 2.042544534415400737, -0.5693509180391894686 ) ) ;
#86394 = CARTESIAN_POINT ( 'NONE',  ( -3.795919822146277767, 7.372397525905215687, -0.7216878364870267237 ) ) ;
#86395 = AXIS2_PLACEMENT_3D ( 'NONE', #199887, #51532, #35254 ) ;
#86396 = CYLINDRICAL_SURFACE ( 'NONE', #191345, 0.07999999999999998779 ) ;
#86397 = CARTESIAN_POINT ( 'NONE',  ( -4.568734577680875653, 8.274014740695587733, -0.7216878364870257245 ) ) ;
#86398 = ADVANCED_FACE ( 'NONE', ( #201252 ), #48646, .T. ) ;
#86400 = CARTESIAN_POINT ( 'NONE',  ( -1.500000000000008216, 11.53125000068279427, 3.469446951953614189E-15 ) ) ;
#86399 = CARTESIAN_POINT ( 'NONE',  ( -10.99962150373186631, -9.919999999999998153, 0.09125116240079726715 ) ) ;
#86401 = ORIENTED_EDGE ( 'NONE', *, *, #45059, .T. ) ;
#86402 = CARTESIAN_POINT ( 'NONE',  ( 5.379529795981254914, -0.4926393568372189335, -1.955173248319847845 ) ) ;
#86404 = CARTESIAN_POINT ( 'NONE',  ( 4.329007229187351591, -1.922695762783795947, -0.7470244877981512266 ) ) ;
#86403 = CARTESIAN_POINT ( 'NONE',  ( 5.606460214450851964, 6.499623990736163037, 1.199719254218462483 ) ) ;
#86406 = CARTESIAN_POINT ( 'NONE',  ( -0.2408018239684096284, 1.329574536483958846, -2.350731018214331947 ) ) ;
#86405 = CARTESIAN_POINT ( 'NONE',  ( 6.343235766347262938, 8.493804042195527870, -1.599625672291281386 ) ) ;
#86407 = CARTESIAN_POINT ( 'NONE',  ( 6.821687566331318564, 7.987665577921906568, 1.199719254218452935 ) ) ;
#86408 = CARTESIAN_POINT ( 'NONE',  ( 3.285556943749998737, -1.305208332855376296, -1.896917185911906500 ) ) ;
#86409 = CARTESIAN_POINT ( 'NONE',  ( 1.123270288250308280, 2.922697346350005887, 0.7749999999993786304 ) ) ;
#86410 = CARTESIAN_POINT ( 'NONE',  ( 0.6036074345479571779, -2.080388865039545454, 0.2067186989125231189 ) ) ;
#86411 = CARTESIAN_POINT ( 'NONE',  ( 5.186172726741035355, 1.650080556555008293, 1.158690440749516881 ) ) ;
#86412 = CARTESIAN_POINT ( 'NONE',  ( 4.265079090171526310, 1.784866007061826298, -0.4516350764028759235 ) ) ;
#86413 = CARTESIAN_POINT ( 'NONE',  ( 7.006866460164219212, 7.069099046480051385, -0.7998128361456281477 ) ) ;
#86414 = CARTESIAN_POINT ( 'NONE',  ( 1.096240241049123210, -0.4132495022837120446, -1.674402075930980338 ) ) ;
#86415 = FACE_OUTER_BOUND ( 'NONE', #29119, .T. ) ;
#86416 = CARTESIAN_POINT ( 'NONE',  ( 0.7569315055401154568, 2.213468045025353881, -0.6199256774504552370 ) ) ;
#86417 = CARTESIAN_POINT ( 'NONE',  ( -5.038826645773246682, 9.030381520044109322, 0.7998128361456481317 ) ) ;
#86418 = CARTESIAN_POINT ( 'NONE',  ( 1.687200700035433876, -0.3313812920804170559, -2.237873883018532073 ) ) ;
#86419 = CARTESIAN_POINT ( 'NONE',  ( 2.596425589483622787, -2.100489730888196238, -0.1540555546653120389 ) ) ;
#86420 = CARTESIAN_POINT ( 'NONE',  ( -5.808742468812186033, 5.741564066561132940, 0.000000000000000000 ) ) ;
#86421 = APPLICATION_CONTEXT ( 'automotive_design' ) ;
#86422 = CARTESIAN_POINT ( 'NONE',  ( 5.764187864104357573, 9.876636274763768597, 1.040834085586084257E-14 ) ) ;
#86423 = CARTESIAN_POINT ( 'NONE',  ( 5.844973620822835336, 7.912498205750389424, 1.443375672974064550 ) ) ;
#86424 =( LENGTH_UNIT ( ) NAMED_UNIT ( * ) SI_UNIT ( .MILLI., .METRE. ) );
#86425 = CARTESIAN_POINT ( 'NONE',  ( -5.768104287610143821, 8.816873204598778102, -1.199719254218440723 ) ) ;
#86426 = CARTESIAN_POINT ( 'NONE',  ( 5.111060722227499298, 8.906728576000002562, -0.7216878364870267237 ) ) ;
#86427 = CARTESIAN_POINT ( 'NONE',  ( 4.972575192752072937, 6.823350471033509557, 1.425105271486303282 ) ) ;
#86428 = CARTESIAN_POINT ( 'NONE',  ( -5.271422797614987665, 5.044414773505913274, -0.7998128361456221525 ) ) ;
#86429 = CARTESIAN_POINT ( 'NONE',  ( 5.590131909697702461, 1.323030080273413844, 1.784280720909060758 ) ) ;
#86430 = CARTESIAN_POINT ( 'NONE',  ( 1.904481915951491189, 1.622449043516610123, -1.473309109067892697 ) ) ;
#86431 = CARTESIAN_POINT ( 'NONE',  ( -5.087333953625788219, 6.958308917361963886, 1.599625672291267398 ) ) ;
#86432 = CARTESIAN_POINT ( 'NONE',  ( -4.995253251992230581, 4.792493313604505367, 0.000000000000000000 ) ) ;
#86433 = CARTESIAN_POINT ( 'NONE',  ( 5.828557447170540584, -1.245780601409246957, 1.515539014345569147 ) ) ;
#86434 = CARTESIAN_POINT ( 'NONE',  ( -1.402160292154681736E-14, 2.446875000341416584, -1.575800808251660134 ) ) ;
#86435 = CARTESIAN_POINT ( 'NONE',  ( -2.278026279638522666, 5.601521726312811644, -0.03298406423010708660 ) ) ;
#86436 = CARTESIAN_POINT ( 'NONE',  ( -5.016153647376219382, 6.875265226737464985, 1.443375672974064550 ) ) ;
#86437 = CARTESIAN_POINT ( 'NONE',  ( 4.096021571020786567, 1.387573888390711385, 1.603661410755026440 ) ) ;
#86438 = CARTESIAN_POINT ( 'NONE',  ( -5.966997003790217136, 9.975597247814986801, -0.7216878364870338292 ) ) ;
#86439 = EDGE_LOOP ( 'NONE', ( #174598, #115994, #136300, #103385 ) ) ;
#86441 = CARTESIAN_POINT ( 'NONE',  ( 6.543834100630380846, 0.8322713294773576020, -1.995267709627518427 ) ) ;
#86440 = CARTESIAN_POINT ( 'NONE',  ( -5.424670859243583720, 8.382514198209223721, 1.082531754730550855 ) ) ;
#86442 = CARTESIAN_POINT ( 'NONE',  ( 5.144429221381498607, 8.089252293998699272, -1.199719254218452047 ) ) ;
#86443 = CARTESIAN_POINT ( 'NONE',  ( 4.915489835137424102, -0.9894786724786635013, -1.552603174752004600 ) ) ;
#86444 = CARTESIAN_POINT ( 'NONE',  ( 3.486133158594716510E-16, 0.8750000006828204668, 1.224999999999968336 ) ) ;
#86445 = CARTESIAN_POINT ( 'NONE',  ( -1.201851678989727383E-14, 2.384375000341416584, 1.575800808251672791 ) ) ;
#86446 = CARTESIAN_POINT ( 'NONE',  ( 1.135833342500572440, 0.3383711564543417927, 1.707032442944929729 ) ) ;
#86447 = LINE ( 'NONE', #70167, #129247 ) ;
#86448 = CARTESIAN_POINT ( 'NONE',  ( -0.1437412632283050218, 3.385453691495572404, 2.075078668430507367 ) ) ;
#86449 = CARTESIAN_POINT ( 'NONE',  ( -1.123270288250342919, 2.846052654332832610, 0.7749999999993751887 ) ) ;
#86450 = VECTOR ( 'NONE', #14922, 1000.000000000000227 ) ;
#86451 = CARTESIAN_POINT ( 'NONE',  ( 5.278265135069068137, -1.204163492603943064, 1.795060720813673738 ) ) ;
#86452 = CARTESIAN_POINT ( 'NONE',  ( -4.569261463005423352, 5.289558780716470565, -1.199719254218446718 ) ) ;
#86453 = CARTESIAN_POINT ( 'NONE',  ( -7.849807752188049825, 8.260456587081938196, 0.7216878364870578100 ) ) ;
#86454 = B_SPLINE_CURVE_WITH_KNOTS ( 'NONE', 3,
 ( #41298, #107406, #142008, #177680, #125808, #190702 ),
 .UNSPECIFIED., .F., .F.,
 ( 4, 2, 4 ),
 ( 0.000000000000000000, 0.0003844267940947831432, 0.0007688535881895662864 ),
 .UNSPECIFIED. ) ;
#86455 = CARTESIAN_POINT ( 'NONE',  ( 4.223607183596161718, -2.069420184152844566, 0.6248923283326962563 ) ) ;
#86456 = CARTESIAN_POINT ( 'NONE',  ( 1.364683531249988535, 3.155208333674756283, -0.7879004041258239610 ) ) ;
#86457 = CARTESIAN_POINT ( 'NONE',  ( 5.237557467868056094, -1.392094792763297617, -1.396070155715684269 ) ) ;
#86458 = CARTESIAN_POINT ( 'NONE',  ( 3.497127502780640107, 1.691016411901521854, 0.3820211100199251697 ) ) ;
#86459 = CARTESIAN_POINT ( 'NONE',  ( 0.4686481397476391364, -2.065551408369214137, -0.7328327568804984260 ) ) ;
#86460 = CARTESIAN_POINT ( 'NONE',  ( 1.888135564707097425, 1.592107727680527329, 1.670599446388189913 ) ) ;
#86461 = CARTESIAN_POINT ( 'NONE',  ( 4.042301887969748542, 2.050516515953205055, 0.2056252831919377910 ) ) ;
#86462 = CARTESIAN_POINT ( 'NONE',  ( 0.1111347575282967681, -1.904682588250571573, 0.3777756254830581528 ) ) ;
#86463 = CARTESIAN_POINT ( 'NONE',  ( -6.629573926958124197, 9.717958100551031819, 1.082531754730548412 ) ) ;
#86464 = CARTESIAN_POINT ( 'NONE',  ( -5.119085517611572378, 8.129960982925583224, 1.199719254218452935 ) ) ;
#86465 = CARTESIAN_POINT ( 'NONE',  ( -2.103486388414573138, 5.605817886458954291, 1.040834085586084257E-14 ) ) ;
#86466 = CARTESIAN_POINT ( 'NONE',  ( -5.354544322754380303, 5.211666229493680191, 0.7998128361456281477 ) ) ;
#86467 = CARTESIAN_POINT ( 'NONE',  ( -7.009202228140755331, 8.240119356661432803, -1.082531754730543083 ) ) ;
#86468 = CARTESIAN_POINT ( 'NONE',  ( 2.872332416675418276, 1.179501869419818494, 1.864919306664609921 ) ) ;
#86469 = CARTESIAN_POINT ( 'NONE',  ( -3.285556943750000070, -2.296874999522042327, 0.000000000000000000 ) ) ;
#86470 = CARTESIAN_POINT ( 'NONE',  ( 0.3735836145450521228, -1.826584228078181660, 0.3550381321636967846 ) ) ;
#86471 = CARTESIAN_POINT ( 'NONE',  ( -0.1290005225502676156, 1.324981729379502537, -2.425680704180297464 ) ) ;
#86472 = DIRECTION ( 'NONE',  ( -0.000000000000000000, -1.000000000000000000, 0.000000000000000000 ) ) ;
#86473 = CARTESIAN_POINT ( 'NONE',  ( -9.499262961676867789, -8.008893676012023732, 0.1288460037566295513 ) ) ;
#86475 = CARTESIAN_POINT ( 'NONE',  ( 6.825078400183551608, 0.5660753733540256905, 2.196387875007102419 ) ) ;
#86474 = CARTESIAN_POINT ( 'NONE',  ( -5.233950224509621663, 7.808013953112580730, -1.290304472045332496 ) ) ;
#86476 = CARTESIAN_POINT ( 'NONE',  ( 6.492148756324659153, -0.4961259030743305209, -1.772972609911625419 ) ) ;
#86477 = VERTEX_POINT ( 'NONE', #99520 ) ;
#86478 = CARTESIAN_POINT ( 'NONE',  ( 3.186453599190769648, -2.030135695866011503, -0.3537577654625714274 ) ) ;
#86479 = CARTESIAN_POINT ( 'NONE',  ( 0.6801582343749883464, 2.473958333674766585, 1.178068619123824323 ) ) ;
#86480 = CARTESIAN_POINT ( 'NONE',  ( -5.096975683733680818, 8.033889833409558534, -1.199719254218452047 ) ) ;
#86481 = CARTESIAN_POINT ( 'NONE',  ( 2.526040989133854886, -1.997384215488164694, 0.2984307725432763236 ) ) ;
#86482 = CARTESIAN_POINT ( 'NONE',  ( 3.147464216666835402, 6.823792019419957278, -0.7998128361456291469 ) ) ;
#86483 = CARTESIAN_POINT ( 'NONE',  ( 2.026313557074521210, 1.187556641299570614, -1.684123726253353492 ) ) ;
#86485 = CARTESIAN_POINT ( 'NONE',  ( -0.6823417656250003738, 13.40104166700806232, 1.181850606188754593 ) ) ;
#86484 = CARTESIAN_POINT ( 'NONE',  ( -10.52942622947605145, 3.950194995956630262, -5.760434021238635793 ) ) ;
#86486 = CARTESIAN_POINT ( 'NONE',  ( 7.006866460164219212, 7.069099046480051385, -0.7998128361456281477 ) ) ;
#86487 = MECHANICAL_DESIGN_GEOMETRIC_PRESENTATION_REPRESENTATION (  '', ( #58814 ), #107581 ) ;
#86488 = CARTESIAN_POINT ( 'NONE',  ( 6.178787966740411086, 5.309377612921773348, 2.438151698554704261 ) ) ;
#86489 = CARTESIAN_POINT ( 'NONE',  ( 5.936183876523434932, 1.091049494364674466, -1.918236432931222257 ) ) ;
#86490 = CARTESIAN_POINT ( 'NONE',  ( 1.985828983967323325, 1.489073237690191176, 1.567133960648490199 ) ) ;
#86491 = CARTESIAN_POINT ( 'NONE',  ( -4.365362273920257330, 6.116008624372160973, 1.443375672974064550 ) ) ;
#86492 = CARTESIAN_POINT ( 'NONE',  ( 1.305875433988498813, -1.124247956386617009, -1.673852571057245830 ) ) ;
#86493 = CARTESIAN_POINT ( 'NONE',  ( 2.320019640604139788, -1.777541238149564107, 1.457059784348129217 ) ) ;
#86494 = ADVANCED_FACE ( 'NONE', ( #199116 ), #3048, .F. ) ;
#86495 = CARTESIAN_POINT ( 'NONE',  ( -0.1004607481840987110, 6.432248552227529004, 3.209664736303321497 ) ) ;
#86496 = CARTESIAN_POINT ( 'NONE',  ( 1.930226670627054109, 8.999999999999998224, -0.7749999999999996891 ) ) ;
#86497 = CARTESIAN_POINT ( 'NONE',  ( 2.096370420935515178, -0.4963513585865795275, -1.803540123670114736 ) ) ;
#86498 = CARTESIAN_POINT ( 'NONE',  ( 3.696500153570709379, 1.422608671726926177, -1.429447704489300364 ) ) ;
#86500 = CARTESIAN_POINT ( 'NONE',  ( 11.41381675112453387, 13.39999999999998259, 3.704697986577180302 ) ) ;
#86499 = CARTESIAN_POINT ( 'NONE',  ( 1.364683531249986537, 1.405208333674755838, -0.7879004041258239610 ) ) ;
#86502 = CARTESIAN_POINT ( 'NONE',  ( 5.039724086851991913, -1.488677873513370331, -1.490019843855681536 ) ) ;
#86501 = CARTESIAN_POINT ( 'NONE',  ( -7.771848369131641121, 10.09024240211882351, -1.599625672291263179 ) ) ;
#86503 = CARTESIAN_POINT ( 'NONE',  ( 6.109920781252839994, 10.27999134477033216, 1.040834085586084257E-14 ) ) ;
#86505 = CARTESIAN_POINT ( 'NONE',  ( -8.538937818508475885, 8.856515631215026829, 1.040834085586084257E-14 ) ) ;
#86504 = CARTESIAN_POINT ( 'NONE',  ( 5.357406976055401948, 6.279338222599979424, 1.199719254218452935 ) ) ;
#86506 = CARTESIAN_POINT ( 'NONE',  ( -0.3525790917593719653, -6.713792789267393424, -9.484899655072640101 ) ) ;
#86507 = CARTESIAN_POINT ( 'NONE',  ( 5.783464979101770709, 0.1443126057797445849, -2.014664192723765623 ) ) ;
#86508 = CARTESIAN_POINT ( 'NONE',  ( -1.364683531249997417, 5.509375000341417916, 1.214306433183764966E-14 ) ) ;
#86509 = ADVANCED_FACE ( 'NONE', ( #82186 ), #68043, .T. ) ;
#86510 = CARTESIAN_POINT ( 'NONE',  ( 0.3739784900498700493, -2.023488180542520887, 0.3987778971655773219 ) ) ;
#86511 = CARTESIAN_POINT ( 'NONE',  ( 8.649738815838679429, 10.15407870897571563, -1.082531754730543083 ) ) ;
#86512 = CARTESIAN_POINT ( 'NONE',  ( 6.547661840756936691, 6.603636667163397256, 0.7998128361456352531 ) ) ;
#86513 = CARTESIAN_POINT ( 'NONE',  ( -0.6823417656250246877, -0.8864583329919115684, 1.181850606188755259 ) ) ;
#86515 = CARTESIAN_POINT ( 'NONE',  ( -7.712474369503325988, -6.289226506789196591, 7.712474369503350857 ) ) ;
#86514 = CARTESIAN_POINT ( 'NONE',  ( 3.881377115262159894, 7.750300077773022878, 0.7998128361456271485 ) ) ;
#86516 = CARTESIAN_POINT ( 'NONE',  ( 6.765155463094740362, 10.83650577367847667, 0.7216878364870438212 ) ) ;
#86518 = CARTESIAN_POINT ( 'NONE',  ( -7.013428937081431336, 5.939655416065873439, -2.436399677959149024 ) ) ;
#86517 = CARTESIAN_POINT ( 'NONE',  ( 2.910768570555821277, 0.7291657262279130913, 2.045214924614814578 ) ) ;
#86520 = CARTESIAN_POINT ( 'NONE',  ( 2.366542893654680402, 0.08848056876738576160, -1.839231530397527736 ) ) ;
#86519 = CARTESIAN_POINT ( 'NONE',  ( -4.256897045010916258, 7.910204285913967404, 0.7216878364870317197 ) ) ;
#86521 = CARTESIAN_POINT ( 'NONE',  ( -1.364683531250012516, 3.488541667008085767, -0.7879004041258300672 ) ) ;
#86522 = CARTESIAN_POINT ( 'NONE',  ( 4.564136437409766600, -1.431273618155091576, 1.659743667367798103 ) ) ;
#86523 = CARTESIAN_POINT ( 'NONE',  ( 6.883263157960391787, 1.253787318140922480, 2.167784446185747171 ) ) ;
#86524 = CARTESIAN_POINT ( 'NONE',  ( 4.452213415057678425, 2.262087339288323840, -0.05152095106783493444 ) ) ;
#86525 = CARTESIAN_POINT ( 'NONE',  ( -6.891622154448065807, 6.934647356477856128, 1.040834085586084257E-14 ) ) ;
#86526 = DIRECTION ( 'NONE',  ( 0.9840714016191985936, 0.1066641999242542993, -0.1422189332323393063 ) ) ;
#86527 = CARTESIAN_POINT ( 'NONE',  ( 5.441225816562971218, 7.512442699629209741, -1.249814574298679926 ) ) ;
#86528 = CARTESIAN_POINT ( 'NONE',  ( -6.009258394948636914E-15, 13.43749999999999822, -1.732050807568875195 ) ) ;
#86529 = CARTESIAN_POINT ( 'NONE',  ( -6.604230223188181093, 6.877559146573883453, 0.7216878364870317197 ) ) ;
#86530 = CARTESIAN_POINT ( 'NONE',  ( 6.048345925472191631, 7.189396680206621149, 1.082531754730549967 ) ) ;
#86531 =( BOUNDED_CURVE ( )  B_SPLINE_CURVE ( 2, ( #209228, #143239, #47856, #212436, #113968, #44645, #12112, #64078, #15300, #195149, #130221, #30523, #60873, #162655, #161593, #179965, #29452, #176758, #97662, #163719, #13182, #63001, #45716, #145377, #81388, #144312, #111834, #131271, #109700, #213493, #65115, #210310, #43584, #178908, #175705, #27295, #93402, #159439, #11037, #61946, #128105, #194063, #177838, #79260, #211375, #46783, #70434, #98713, #199377, #18504, #133372, #150671, #167968, #51024, #164772, #118216, #197259, #100826, #17424, #169029, #198314, #166911, #3304, #82440, #67238, #69374, #84584, #83507, #184202, #49955, #102971, #35825, #116074, #99773, #149590, #182064, #66163, #16362, #19574, #101903, #1173, #148530, #201504, #85647, #53150, #33696, #165838, #151734, #20626, #134440, #135482, #119280, #97, #185266, #2232, #36889, #183149, #132308, #86715, #152784, #68309, #32636, #117145, #34752, #200443, #52089, #4364, #48899, #115019, #181015, #121438, #170090, #204703, #58485, #37971, #205788, #136550, #25970, #202571, #158133, #55288, #173322, #7578, #22752, #73663, #153860, #54223, #56353, #6509, #137620, #140841, #187407, #188479, #39038, #5429, #190598, #74736, #203637, #107298, #171163, #40109 ),
 .UNSPECIFIED., .F., .T. ) 
 B_SPLINE_CURVE_WITH_KNOTS ( ( 3, 2, 2, 2, 2, 2, 2, 2, 2, 2, 2, 2, 2, 2, 2, 2, 2, 2, 2, 2, 2, 2, 2, 2, 2, 2, 2, 2, 2, 2, 2, 2, 2, 2, 2, 2, 2, 2, 2, 2, 2, 2, 2, 2, 2, 2, 2, 2, 2, 2, 2, 2, 2, 2, 2, 2, 2, 2, 2, 2, 2, 2, 2, 2, 2, 2, 2, 2, 2, 2, 3 ),
 ( 0.000000000000000000, 0.01041666666666666609, 0.02083333333333333218, 0.03125000000000000000, 0.04166666666666666435, 0.05208333333333334259, 0.06250000000000000000, 0.07291666666666667129, 0.08333333333333332871, 0.09375000000000000000, 0.1041666666666666852, 0.1145833333333333148, 0.1250000000000000000, 0.1354166666666666574, 0.1458333333333333426, 0.1562500000000000000, 0.1666666666666666574, 0.1770833333333333426, 0.1875000000000000000, 0.1979166666666666574, 0.2083333333333333703, 0.2187499999999999722, 0.2291666666666666297, 0.2395833333333333426, 0.2500000000000000000, 0.2604166666666666852, 0.2708333333333333148, 0.2812500000000000000, 0.2916666666666666852, 0.3020833333333333148, 0.3125000000000000000, 0.3229166666666666852, 0.3333333333333333148, 0.3437500000000000000, 0.3541666666666666852, 0.3645833333333333148, 0.3750000000000000000, 0.3854166666666666852, 0.3958333333333333148, 0.4062500000000000000, 0.4166666666666667407, 0.4270833333333333148, 0.4374999999999999445, 0.4479166666666666852, 0.4583333333333332593, 0.4687500000000000000, 0.4791666666666666852, 0.4895833333333333148, 0.5000000000000000000, 0.5104166666666666297, 0.5208333333333333703, 0.5312500000000000000, 0.5416666666666666297, 0.5520833333333333703, 0.5625000000000000000, 0.5729166666666666297, 0.5833333333333333703, 0.5937500000000000000, 0.6041666666666666297, 0.6145833333333333703, 0.6250000000000000000, 0.6354166666666666297, 0.6458333333333333703, 0.6562500000000000000, 0.6666666666666666297, 0.6770833333333333703, 0.6875000000000000000, 0.6979166666666666297, 0.7083333333333333703, 0.7187500000000000000, 0.7227386901363775928 ),
 .UNSPECIFIED. ) 
 CURVE ( )  GEOMETRIC_REPRESENTATION_ITEM ( )  RATIONAL_B_SPLINE_CURVE ( ( 1.000000000000000000, 0.8660254037844387076, 1.000000000000000000, 0.8660254037844387076, 1.000000000000000000, 0.8660254037844387076, 1.000000000000000000, 0.8660254037844387076, 1.000000000000000000, 0.8660254037844387076, 1.000000000000000000, 0.8660254037844387076, 1.000000000000000000, 0.8660254037844387076, 1.000000000000000000, 0.8660254037844387076, 1.000000000000000000, 0.8660254037844387076, 1.000000000000000000, 0.8660254037844387076, 1.000000000000000000, 0.8660254037844387076, 1.000000000000000000, 0.8660254037844387076, 1.000000000000000000, 0.8660254037844387076, 1.000000000000000000, 0.8660254037844387076, 1.000000000000000000, 0.8660254037844387076, 1.000000000000000000, 0.8660254037844387076, 1.000000000000000000, 0.8660254037844387076, 1.000000000000000000, 0.8660254037844387076, 1.000000000000000000, 0.8660254037844387076, 1.000000000000000000, 0.8660254037844387076, 1.000000000000000000, 0.8660254037844387076, 1.000000000000000000, 0.8660254037844387076, 1.000000000000000000, 0.8660254037844387076, 1.000000000000000000, 0.8660254037844387076, 1.000000000000000000, 0.8660254037844387076, 1.000000000000000000, 0.8660254037844387076, 1.000000000000000000, 0.8660254037844387076, 1.000000000000000000, 0.8660254037844387076, 1.000000000000000000, 0.8660254037844387076, 1.000000000000000000, 0.8660254037844387076, 1.000000000000000000, 0.8660254037844387076, 1.000000000000000000, 0.8660254037844387076, 1.000000000000000000, 0.8660254037844387076, 1.000000000000000000, 0.8660254037844387076, 1.000000000000000000, 0.8660254037844387076, 1.000000000000000000, 0.8660254037844387076, 1.000000000000000000, 0.8660254037844387076, 1.000000000000000000, 0.8660254037844387076, 1.000000000000000000, 0.8660254037844387076, 1.000000000000000000, 0.8660254037844387076, 1.000000000000000000, 0.8660254037844387076, 1.000000000000000000, 0.8660254037844387076, 1.000000000000000000, 0.8660254037844387076, 1.000000000000000000, 0.8660254037844387076, 1.000000000000000000, 0.8660254037844387076, 1.000000000000000000, 0.8660254037844387076, 1.000000000000000000, 0.8660254037844387076, 1.000000000000000000, 0.8660254037844387076, 1.000000000000000000, 0.8660254037844387076, 1.000000000000000000, 0.8660254037844387076, 1.000000000000000000, 0.8660254037844387076, 1.000000000000000000, 0.8660254037844387076, 1.000000000000000000, 0.8660254037844387076, 1.000000000000000000, 0.8660254037844387076, 1.000000000000000000, 0.8660254037844387076, 1.000000000000000000, 0.8660254037844387076, 1.000000000000000000, 0.8660254037844387076, 1.000000000000000000, 0.8660254037844387076, 1.000000000000000000, 0.8660254037844387076, 1.000000000000000000, 0.8660254037844387076, 1.000000000000000000, 0.8660254037844387076, 1.000000000000000000, 0.8660254037844387076, 1.000000000000000000, 0.8660254037844387076, 1.000000000000000000, 0.8660254037844387076, 1.000000000000000000, 0.8660254037844387076, 1.000000000000000000, 0.8660254037844387076, 1.000000000000000000, 0.8660254037844387076, 1.000000000000000000, 0.8660254037844387076, 1.000000000000000000, 0.8660254037844387076, 1.000000000000000000, 0.9486992175567839913, 0.9366860366981510921 ) ) 
 REPRESENTATION_ITEM ( '' )  );
#86532 = CARTESIAN_POINT ( 'NONE',  ( 5.096827573163183800, 1.471272477087566699, -0.9831756853606200552 ) ) ;
#86533 = CARTESIAN_POINT ( 'NONE',  ( 7.096803341749390981, 10.36702210109460154, -1.199719254218441611 ) ) ;
#86534 = CARTESIAN_POINT ( 'NONE',  ( 1.940588816512535120, 2.082954711654343427, 0.3096100588686269695 ) ) ;
#86537 = EDGE_CURVE ( 'NONE', #179011, #49626, #191853, .T. ) ;
#86536 = CARTESIAN_POINT ( 'NONE',  ( 1.499999999999989120, 2.025000000000019895, 1.214306433183764966E-14 ) ) ;
#86535 = CARTESIAN_POINT ( 'NONE',  ( -1.364683531250014514, 11.33854166700806410, -0.7879004041258335089 ) ) ;
#86538 = CARTESIAN_POINT ( 'NONE',  ( 2.523828315609038864, 1.932092998399935091, -0.3813574256018251729 ) ) ;
#86539 = DIRECTION ( 'NONE',  ( 0.000000000000000000, 1.000000000000000000, 0.000000000000000000 ) ) ;
#86540 = CARTESIAN_POINT ( 'NONE',  ( 8.915975476025575830, 3.467171072964057910, 8.027980377473637574 ) ) ;
#86542 = EDGE_LOOP ( 'NONE', ( #108396, #7455, #156740, #148132 ) ) ;
#86541 = CARTESIAN_POINT ( 'NONE',  ( 5.941655795435678122, -1.702662506596404279, 0.6190658298997688824 ) ) ;
#86543 = CARTESIAN_POINT ( 'NONE',  ( 5.666945020832167224, 8.594891043404107478, 1.082531754730558626 ) ) ;
#86544 = CARTESIAN_POINT ( 'NONE',  ( 0.6823417656249882723, -0.2614583329919109578, -1.181850606188749264 ) ) ;
#86545 = AXIS2_PLACEMENT_3D ( 'NONE', #179962, #31586, #97660 ) ;
#86546 = CARTESIAN_POINT ( 'NONE',  ( 5.436355746168001879, 1.843147576875401983, 0.3187000444574567548 ) ) ;
#86547 = CARTESIAN_POINT ( 'NONE',  ( 4.241003122976366058, 3.842258486427521103, -0.7998128361456211532 ) ) ;
#86548 = EDGE_LOOP ( 'NONE', ( #4966, #109113, #116495, #130229, #129193 ) ) ;
#86549 = CARTESIAN_POINT ( 'NONE',  ( 5.981320602565292077, -0.05662044862421274083, 2.069665677200482445 ) ) ;
#86550 = CARTESIAN_POINT ( 'NONE',  ( -1.224999999999995204, 3.000000000000002665, -1.387778780781445676E-14 ) ) ;
#86551 = CARTESIAN_POINT ( 'NONE',  ( -4.123088111887291518, 7.824370207261548416, 0.000000000000000000 ) ) ;
#86552 = CARTESIAN_POINT ( 'NONE',  ( 2.494940289813108780, 3.038492715500545227, -11.73777120880564873 ) ) ;
#86553 = CARTESIAN_POINT ( 'NONE',  ( 0.7499999999999867883, 0.3166666666666873020, -1.299038105676652899 ) ) ;
#86554 = CARTESIAN_POINT ( 'NONE',  ( 6.642605195691581699, 9.837124264027149678, 1.199719254218462483 ) ) ;
#86555 = CARTESIAN_POINT ( 'NONE',  ( -9.826962411806732689, 10.35921099006301382, -0.7998128361456291469 ) ) ;
#86556 = CARTESIAN_POINT ( 'NONE',  ( 5.611095471209277541, 7.639640364534566075, 1.599625672291268286 ) ) ;
#86557 = ADVANCED_FACE ( 'NONE', ( #147217 ), #100436, .F. ) ;
#86558 = CARTESIAN_POINT ( 'NONE',  ( -1.364683531250014514, 0.2385416670080863499, -0.7879004041258359514 ) ) ;
#86559 = EDGE_CURVE ( 'NONE', #182627, #175466, #157437, .T. ) ;
#86560 = CARTESIAN_POINT ( 'NONE',  ( -1.402160292154681736E-14, 1.087500000000024336, -1.732050807568863648 ) ) ;
#86562 = CARTESIAN_POINT ( 'NONE',  ( 5.847644326195776010, 5.716673223516856694, -0.7998128361456281477 ) ) ;
#86561 = CARTESIAN_POINT ( 'NONE',  ( 5.406682003534418079, 0.5678430586343993225, 1.877905798087247335 ) ) ;
#86563 = CARTESIAN_POINT ( 'NONE',  ( 3.304064382408095302, -1.779354530013575131, 0.9478943420064069869 ) ) ;
#86564 = CARTESIAN_POINT ( 'NONE',  ( 2.184663254350202255, 1.535933850207292783, -1.144682215256398239 ) ) ;
#86565 = CARTESIAN_POINT ( 'NONE',  ( 11.01135777277262306, 13.39999999999998259, 1.399999999999998579 ) ) ;
#86566 = CARTESIAN_POINT ( 'NONE',  ( 0.09952931447375359952, -0.5783855404800625211, 2.113812074898171023 ) ) ;
#86567 = PLANE ( 'NONE',  #132350 ) ;
#86568 = CARTESIAN_POINT ( 'NONE',  ( 2.301827437220682171, -1.870247568056710774, 0.04138213060620592881 ) ) ;
#86569 = CARTESIAN_POINT ( 'NONE',  ( -0.6823417656250212460, 4.551041667008086655, 1.181850606188767472 ) ) ;
#86570 = CARTESIAN_POINT ( 'NONE',  ( -8.128276786592724790, 9.441743324901704426, -1.199719254218446718 ) ) ;
#86572 = CARTESIAN_POINT ( 'NONE',  ( 4.112992273575425628, 0.1058706520744826102, 2.114715381611050660 ) ) ;
#86571 = CARTESIAN_POINT ( 'NONE',  ( -5.775410249741523394, 5.840326167560965231, 0.7216878364870317197 ) ) ;
#86573 = LINE ( 'NONE', #152636, #87132 ) ;
#86574 = CARTESIAN_POINT ( 'NONE',  ( 5.617656447048144486, 0.4075009240860455462, -2.029694874052537568 ) ) ;
#86576 = CARTESIAN_POINT ( 'NONE',  ( -5.317937133690677776, 6.974616996837226246, -1.245902666257096669 ) ) ;
#86575 = CARTESIAN_POINT ( 'NONE',  ( 0.9254645587078378366, -1.329342062510083355, -1.613690532076578199 ) ) ;
#86578 = VERTEX_POINT ( 'NONE', #138431 ) ;
#86577 = CARTESIAN_POINT ( 'NONE',  ( 6.211906940382025510, -1.811394037990306627, 0.2264786762415857968 ) ) ;
#86579 = CARTESIAN_POINT ( 'NONE',  ( 8.613507663383630941, 8.943513783569379427, -0.7998128361456221525 ) ) ;
#86580 = DIRECTION ( 'NONE',  ( -5.551115123125766062E-17, 0.000000000000000000, 1.000000000000000000 ) ) ;
#86581 = CARTESIAN_POINT ( 'NONE',  ( -10.39320420135713263, 4.932286138528427344, 5.331284845095887626 ) ) ;
#86582 = CARTESIAN_POINT ( 'NONE',  ( 6.927853306458743532, 9.105581495667113501, 1.443375672974076540 ) ) ;
#86583 = CARTESIAN_POINT ( 'NONE',  ( -1.364683531250014514, 12.90104166700806410, -0.7879004041258335089 ) ) ;
#86585 = CARTESIAN_POINT ( 'NONE',  ( 0.6096459265214678735, -0.6533943968328138618, 1.689718745909152053 ) ) ;
#86584 = CARTESIAN_POINT ( 'NONE',  ( 7.367930134383754215, 7.560616343061329125, -0.7998128361456341429 ) ) ;
#86586 = CARTESIAN_POINT ( 'NONE',  ( -8.694856585065634746, 9.038420858865048757, 0.7998128361456462443 ) ) ;
#86587 =( BOUNDED_CURVE ( )  B_SPLINE_CURVE ( 3, ( #146174, #160262, #213259, #28128 ),
 .UNSPECIFIED., .F., .T. ) 
 B_SPLINE_CURVE_WITH_KNOTS ( ( 4, 4 ),
 ( 0.4999999999999970579, 1.000000000000000000 ),
 .UNSPECIFIED. ) 
 CURVE ( )  GEOMETRIC_REPRESENTATION_ITEM ( )  RATIONAL_B_SPLINE_CURVE ( ( 1.000000000000003997, 0.3333333333333334259, 0.3333333333333294846, 1.000000000000000222 ) ) 
 REPRESENTATION_ITEM ( '' )  );
#86588 = CARTESIAN_POINT ( 'NONE',  ( 5.144429221381498607, 8.089252293998699272, -1.199719254218452047 ) ) ;
#86589 = CARTESIAN_POINT ( 'NONE',  ( 7.334597915313080918, 9.580116872663850813, 1.040834085586084257E-14 ) ) ;
#86590 = CARTESIAN_POINT ( 'NONE',  ( 9.499700864329909678, -7.154544010627095219, 0.07538891330675402680 ) ) ;
#86591 = CARTESIAN_POINT ( 'NONE',  ( 4.532503425670185493, 4.182342172903648070, 1.214306433183764966E-14 ) ) ;
#86592 = ORIENTED_EDGE ( 'NONE', *, *, #161158, .F. ) ;
#86593 = AXIS2_PLACEMENT_3D ( 'NONE', #14669, #209665, #93833 ) ;
#86594 = CARTESIAN_POINT ( 'NONE',  ( 6.257435441360899908, 1.928747933193178721, -0.5880367767025842518 ) ) ;
#86595 = CARTESIAN_POINT ( 'NONE',  ( 0.3113914200543760336, 1.760583737686383321, -1.181573663439142052 ) ) ;
#86596 = CARTESIAN_POINT ( 'NONE',  ( -2.996969800987126842, 6.406095355250562839, -0.7225173797624391270 ) ) ;
#86597 = CARTESIAN_POINT ( 'NONE',  ( 0.1405533004714279999, 2.862415582289945526, -2.767767315042678700 ) ) ;
#86598 = FACE_OUTER_BOUND ( 'NONE', #76468, .T. ) ;
#86599 = CARTESIAN_POINT ( 'NONE',  ( -4.202664430556263930, 5.926194473780837413, 1.443375672974064550 ) ) ;
#86600 = CARTESIAN_POINT ( 'NONE',  ( 10.39874063200158893, 11.23421161353111586, 0.000000000000000000 ) ) ;
#86601 = CARTESIAN_POINT ( 'NONE',  ( 3.696117419531047776, 0.8894436365228419739, -1.757264023730123581 ) ) ;
#86602 = CARTESIAN_POINT ( 'NONE',  ( 4.376577478760902196, -0.4445230835841383898, -1.966641233467445016 ) ) ;
#86603 = CARTESIAN_POINT ( 'NONE',  ( -7.691553217654356622, 7.867900263551875994, -0.7998128361456291469 ) ) ;
#86604 = CARTESIAN_POINT ( 'NONE',  ( 3.475000000000000533, -1.895833333333332815, -2.006292185433951047 ) ) ;
#86605 = DIRECTION ( 'NONE',  ( 0.000000000000000000, 1.000000000000000000, -0.000000000000000000 ) ) ;
#86606 = CARTESIAN_POINT ( 'NONE',  ( 5.226606370275341362, 0.1587857941063846590, 2.185760735149797185 ) ) ;
#86607 = CARTESIAN_POINT ( 'NONE',  ( 2.959893420002459585, 1.917249785004307316, -0.1873479421724104088 ) ) ;
#86608 = CARTESIAN_POINT ( 'NONE',  ( -7.263417608619167076, 9.497073181520933716, -1.599625672291263179 ) ) ;
#86609 = CARTESIAN_POINT ( 'NONE',  ( -0.02948999725178608200, 2.884818527723536530, -2.415019744152223868 ) ) ;
#86610 = CARTESIAN_POINT ( 'NONE',  ( 0.4917504562595223505, 10.46609003534429760, -2.500000000000000444 ) ) ;
#86611 = CARTESIAN_POINT ( 'NONE',  ( -0.4914377447849399561, 7.519435632882157883, 2.014015809874911245 ) ) ;
#86612 = EDGE_LOOP ( 'NONE', ( #69232, #31671, #36432, #206982 ) ) ;
#86613 = CARTESIAN_POINT ( 'NONE',  ( 3.933273961740296087, 6.642551151122080277, 1.082531754730549078 ) ) ;
#86614 = CARTESIAN_POINT ( 'NONE',  ( 4.803538196489102852, -1.519661447750167982, -1.252675939642827529 ) ) ;
#86616 = CARTESIAN_POINT ( 'NONE',  ( 3.721343298090164620, 1.727675083452884897, 1.033047338021097383 ) ) ;
#86615 = CARTESIAN_POINT ( 'NONE',  ( 0.3627036604622800864, 0.1893831815216796277, -1.932784825206189661 ) ) ;
#86617 = CARTESIAN_POINT ( 'NONE',  ( 5.712396407272276377, -1.806953704233695612, -1.420304717212710122 ) ) ;
#86619 = CARTESIAN_POINT ( 'NONE',  ( 3.942128412476927135, -0.9204884114761485714, 1.617296529409748773 ) ) ;
#86618 = CARTESIAN_POINT ( 'NONE',  ( -6.071018923869249129, 10.30488218781460574, 0.7998128361456291469 ) ) ;
#86620 = CARTESIAN_POINT ( 'NONE',  ( 5.905458427204159477, 9.047396044116986502, 1.199719254218452047 ) ) ;
#86621 = CARTESIAN_POINT ( 'NONE',  ( -10.40319425600960201, -5.787668213791931748, 0.4366904681730437443 ) ) ;
#86622 = LINE ( 'NONE', #53051, #192309 ) ;
#86623 = CARTESIAN_POINT ( 'NONE',  ( -7.718669524881690336, 7.899535955317097624, 0.7998128361456462443 ) ) ;
#86624 = ADVANCED_FACE ( 'NONE', ( #136296 ), #108749, .T. ) ;
#86625 = CARTESIAN_POINT ( 'NONE',  ( -3.526529353330355221, 6.168015774643768268, -1.082531754730546636 ) ) ;
#86626 = CARTESIAN_POINT ( 'NONE',  ( 0.3456114054924685486, 0.6817542107791437767, -2.082909237240769151 ) ) ;
#86627 = CARTESIAN_POINT ( 'NONE',  ( 4.514501963670558560, 8.210743357683563559, 1.040834085586084257E-14 ) ) ;
#86628 = VERTEX_POINT ( 'NONE', #182429 ) ;
#86629 = DIRECTION ( 'NONE',  ( -0.000000000000000000, -0.000000000000000000, 1.000000000000000000 ) ) ;
#86630 = CARTESIAN_POINT ( 'NONE',  ( 6.760415694340460783E-18, 5.633679745283718603E-18, 0.4330127018937082184 ) ) ;
#86631 = CARTESIAN_POINT ( 'NONE',  ( 0.1877650043593872553, -0.8638833939697135866, 1.608357707688967242 ) ) ;
#86632 = CARTESIAN_POINT ( 'NONE',  ( -3.574546055497324737, 7.322054164722185732, 0.7998128361456341429 ) ) ;
#86633 = STYLED_ITEM ( 'NONE', ( #207115 ), #166452 ) ;
#86634 = CARTESIAN_POINT ( 'NONE',  ( 2.760114697247218807, 1.645750434341390900, -0.5467383172713826678 ) ) ;
#86635 = CARTESIAN_POINT ( 'NONE',  ( -3.486133158594716510E-16, 2.687500000000001332, -1.225000000000008749 ) ) ;
#86636 = CARTESIAN_POINT ( 'NONE',  ( -1.499999999999997780, 3.400000000000021227, 1.214306433183764966E-14 ) ) ;
#86637 = CARTESIAN_POINT ( 'NONE',  ( 5.496661139185262002, -0.4475443406098400523, -1.769863040007889410 ) ) ;
#86638 = CARTESIAN_POINT ( 'NONE',  ( 2.817183829107517745, -1.704460984269994039, -0.9711623693852902139 ) ) ;
#86639 = CARTESIAN_POINT ( 'NONE',  ( 1.224999999999961009, -0.7916666659838317299, -0.7072540797572958171 ) ) ;
#86640 = CARTESIAN_POINT ( 'NONE',  ( -8.666686507633592385, 11.13422023037111330, 1.599625672291269396 ) ) ;
#86641 = CARTESIAN_POINT ( 'NONE',  ( 8.260995669428309540, 8.532249790621511565, 0.7998128361456481317 ) ) ;
#86642 = CARTESIAN_POINT ( 'NONE',  ( 4.776102292387626846, 2.097323840013893381, -0.3118266106481304423 ) ) ;
#86643 = CARTESIAN_POINT ( 'NONE',  ( 7.614839552730775729, 8.913009562054615031, 1.199719254218452047 ) ) ;
#86644 = CARTESIAN_POINT ( 'NONE',  ( -8.513630394377489807, 12.01998699582738972, -1.199719254218446718 ) ) ;
#86645 = CARTESIAN_POINT ( 'NONE',  ( 1.393514648303464165, -1.873246724434135313, 0.8816542684770898308 ) ) ;
#86647 = CARTESIAN_POINT ( 'NONE',  ( 1.364683531249986537, -0.2822916663252520997, -0.7879004041258309554 ) ) ;
#86646 = CARTESIAN_POINT ( 'NONE',  ( -11.86687215968023601, 11.10942212305781851, 1.056395335932115209 ) ) ;
#86649 = ORIENTED_EDGE ( 'NONE', *, *, #88601, .T. ) ;
#86648 = CARTESIAN_POINT ( 'NONE',  ( 5.127666992232062348, -0.3272401999867382560, 2.196937980255990741 ) ) ;
#86650 = CARTESIAN_POINT ( 'NONE',  ( 2.989241104188970155, -2.295904969233518500, 0.1156830036863568528 ) ) ;
#86651 = CARTESIAN_POINT ( 'NONE',  ( 8.595506201384008449, 11.05117653974661529, 1.443375672974076540 ) ) ;
#86653 = CARTESIAN_POINT ( 'NONE',  ( 3.285556943750000514, -3.113541666188709645, 1.896917185911906500 ) ) ;
#86652 = CARTESIAN_POINT ( 'NONE',  ( 6.034787771858531435, 10.05468647722803865, 0.000000000000000000 ) ) ;
#86654 = CARTESIAN_POINT ( 'NONE',  ( 1.224999999999989209, 1.604166666666679619, 0.7072540797572898219 ) ) ;
#86655 = FILL_AREA_STYLE ('',( #116020 ) ) ;
#86656 = ORIENTED_EDGE ( 'NONE', *, *, #187873, .T. ) ;
#86657 = LINE ( 'NONE', #150612, #52916 ) ;
#86658 = CARTESIAN_POINT ( 'NONE',  ( 3.392734571251673881, -1.844325299564765652, -0.5055192353106837677 ) ) ;
#86659 = CARTESIAN_POINT ( 'NONE',  ( -11.78331023100045627, 13.79999999999999893, -1.800000000000001155 ) ) ;
#86660 = CARTESIAN_POINT ( 'NONE',  ( 3.821100691872282518, -0.1266977344972844144, 1.720184112200423332 ) ) ;
#86661 = CARTESIAN_POINT ( 'NONE',  ( 3.538296236868877731, 0.7303062672313584969, 1.879804216660937666 ) ) ;
#86662 = CARTESIAN_POINT ( 'NONE',  ( 4.026267332373588914, -1.999701941076356349, 1.133592428816285080 ) ) ;
#86663 = DIRECTION ( 'NONE',  ( 0.000000000000000000, 0.000000000000000000, 1.000000000000000000 ) ) ;
#86664 = CARTESIAN_POINT ( 'NONE',  ( 6.305314546112477103, 1.749969596565099650, 1.171488565500600654 ) ) ;
#86665 = CARTESIAN_POINT ( 'NONE',  ( -4.963693636378939011, 8.805076652501815815, 0.7216878364870267237 ) ) ;
#86666 = VERTEX_POINT ( 'NONE', #51390 ) ;
#86667 = CARTESIAN_POINT ( 'NONE',  ( 4.323360031453548302, -1.693909316728856806, 0.5125324126216290743 ) ) ;
#86669 = CARTESIAN_POINT ( 'NONE',  ( 0.6040055286682350921, -2.280654241543427663, 0.2304348961432670095 ) ) ;
#86668 = CARTESIAN_POINT ( 'NONE',  ( 5.826972158823246595, 10.02016096192762085, -0.7998128361456481317 ) ) ;
#86670 = B_SPLINE_CURVE_WITH_KNOTS ( 'NONE', 3,
 ( #52060, #54190, #134410, #86685, #170061, #200414, #101872, #135451, #152753, #116047, #184175, #132277, #167939, #85617 ),
 .UNSPECIFIED., .F., .F.,
 ( 4, 2, 2, 2, 2, 2, 4 ),
 ( 6.159050845453070644E-06, 0.0002195312228445668514, 0.0004329033948436806448, 0.0008596477388419082859, 0.001073019910841021890, 0.001286392082840135927, 0.001713136426838359665 ),
 .UNSPECIFIED. ) ;
#86671 = CARTESIAN_POINT ( 'NONE',  ( 0.005214030526056419486, -0.7400075616556491820, -1.574097848898856622 ) ) ;
#86672 = CARTESIAN_POINT ( 'NONE',  ( 0.6500572981163011965, 4.350074487569242976, 0.06817653764027256647 ) ) ;
#86673 = CARTESIAN_POINT ( 'NONE',  ( 5.244143516318892750, 0.6338322011035132375, 2.097776330851252258 ) ) ;
#86674 = CARTESIAN_POINT ( 'NONE',  ( -4.516801452008150086, 5.298631777878131111, 1.199719254218452935 ) ) ;
#86675 = CARTESIAN_POINT ( 'NONE',  ( -0.6801582343750229853, -0.3697916663252601155, -1.178068619123890270 ) ) ;
#86676 = CARTESIAN_POINT ( 'NONE',  ( 9.492899823913848678, -8.233137084989849086, -0.3774118403930767363 ) ) ;
#86677 = CARTESIAN_POINT ( 'NONE',  ( 0.6257148180217129152, 0.2125798311119214690, -2.160765367999056608 ) ) ;
#86678 = CARTESIAN_POINT ( 'NONE',  ( 1.112517963266421939, 1.944731545904467396, 0.5331650539944567946 ) ) ;
#86679 = CARTESIAN_POINT ( 'NONE',  ( -1.602468905319636405E-14, -1.131249999317182064, -1.732050807568870754 ) ) ;
#86680 = CARTESIAN_POINT ( 'NONE',  ( 4.441968003317652958, 0.8225352836801721468, -1.742211325687251788 ) ) ;
#86681 = CARTESIAN_POINT ( 'NONE',  ( 0.6823417656249934904, 12.19270833367473017, 1.181850606188764807 ) ) ;
#86682 = CARTESIAN_POINT ( 'NONE',  ( 1.652877544743835969, 2.198119390704804665, 0.3199964322739051736 ) ) ;
#86684 = VERTEX_POINT ( 'NONE', #132666 ) ;
#86683 = CARTESIAN_POINT ( 'NONE',  ( 0.000000000000000000, 0.5000000000000004441, -3.475000000000000089 ) ) ;
#86685 = CARTESIAN_POINT ( 'NONE',  ( 0.2656570211550720595, 7.171539594011578700, -2.094714161149643594 ) ) ;
#86686 = CARTESIAN_POINT ( 'NONE',  ( 0.000000000000000000, 3.000000000000002665, 8.049999999999993605 ) ) ;
#86687 = CARTESIAN_POINT ( 'NONE',  ( 3.837121167867449945, 4.435395103055503441, 1.199719254218464037 ) ) ;
#86688 = DIRECTION ( 'NONE',  ( -0.9999980456341538426, 0.000000000000000000, -0.001977050295958626691 ) ) ;
#86689 = CARTESIAN_POINT ( 'NONE',  ( -8.014278199453791274, 8.522615118883788199, 1.530808498934192557E-16 ) ) ;
#86690 = CARTESIAN_POINT ( 'NONE',  ( 4.757210230733205591, 1.720523950154304371, -0.2617468875206073742 ) ) ;
#86691 = CARTESIAN_POINT ( 'NONE',  ( 2.101936620064443151, 0.7537240185569763495, -1.811501260397870405 ) ) ;
#86693 = CARTESIAN_POINT ( 'NONE',  ( -1.201851678989727383E-14, 2.634375000341417916, 1.575800808251672791 ) ) ;
#86692 = CARTESIAN_POINT ( 'NONE',  ( 4.310602774141044868, 7.116454772218158809, -1.199719254218452047 ) ) ;
#86694 = ADVANCED_FACE ( 'NONE', ( #198671 ), #164081, .F. ) ;
#86695 = CARTESIAN_POINT ( 'NONE',  ( -5.887541547804238995, 6.014758725225416214, 0.2650624260464862214 ) ) ;
#86696 = CARTESIAN_POINT ( 'NONE',  ( 9.028840231696797503, 12.62106513936658203, -1.199719254218446718 ) ) ;
#86697 = CARTESIAN_POINT ( 'NONE',  ( 0.2212323960570794501, -1.841704181501323312, -0.9290775759197547057 ) ) ;
#86698 = CARTESIAN_POINT ( 'NONE',  ( -9.020252271793614440, 9.418049160047695878, 0.7998128361456462443 ) ) ;
#86699 = PRESENTATION_LAYER_ASSIGNMENT (  '', '', ( #121419 ) ) ;
#86700 = CARTESIAN_POINT ( 'NONE',  ( -3.578989363883261277, 7.119311991265024453, 1.040834085586084257E-14 ) ) ;
#86701 = CARTESIAN_POINT ( 'NONE',  ( 0.9016947886714383742, 1.851236229948808543, 1.300475659685183416 ) ) ;
#86703 = ORIENTED_EDGE ( 'NONE', *, *, #114761, .T. ) ;
#86702 = CARTESIAN_POINT ( 'NONE',  ( -4.367698041896780126, 8.247398148854895084, 0.7998128361456481317 ) ) ;
#86704 = CARTESIAN_POINT ( 'NONE',  ( -1.500000000000015099, 0.1604166673494879791, -0.8660254037844383745 ) ) ;
#86705 = CARTESIAN_POINT ( 'NONE',  ( 1.475632603725419489, 1.109822327618605442, 1.505604422130282227 ) ) ;
#86706 = CARTESIAN_POINT ( 'NONE',  ( 0.6153164582703105623, 0.1250789957258427176, 1.729716150945133535 ) ) ;
#86707 = CARTESIAN_POINT ( 'NONE',  ( 4.036819321710017228, -1.906298169312226953, 1.081085072550565407 ) ) ;
#86708 = CARTESIAN_POINT ( 'NONE',  ( 5.842881032528668861, 0.4426140756379555730, 2.264596805331307472 ) ) ;
#86709 = CARTESIAN_POINT ( 'NONE',  ( 0.7782833776110262836, -1.145455985629862505, 1.713024904945841254 ) ) ;
#86710 = CARTESIAN_POINT ( 'NONE',  ( 3.046748965309022505, -1.587984067068026528, -1.117546226756223726 ) ) ;
#86711 = CARTESIAN_POINT ( 'NONE',  ( -4.907688418022547516, 4.827984030555475314, 1.214306433183764966E-14 ) ) ;
#86712 = CARTESIAN_POINT ( 'NONE',  ( 5.764887228985436707, -1.690807747980655584, -0.8004016547063924625 ) ) ;
#86713 = CARTESIAN_POINT ( 'NONE',  ( 0.3667533499403192732, 13.35836302003387743, -1.335730745167230893 ) ) ;
#86714 = CARTESIAN_POINT ( 'NONE',  ( 5.234856708652235291, 5.279956712948652431, 0.7216878364870338292 ) ) ;
#86715 = CARTESIAN_POINT ( 'NONE',  ( -0.6801582343750282034, 0.8489583336747236197, -1.178068619123876282 ) ) ;
#86716 = CARTESIAN_POINT ( 'NONE',  ( 4.922500090287251773, -1.427935867408920645, -1.423962988533589158 ) ) ;
#86717 = CARTESIAN_POINT ( 'NONE',  ( -4.297571505407598025, 5.076550180139354218, 1.082531754730558626 ) ) ;
#86718 = CARTESIAN_POINT ( 'NONE',  ( -5.631432701629818460, 7.663367133358481631, 1.599625672291263179 ) ) ;
#86719 = CARTESIAN_POINT ( 'NONE',  ( 9.447334110624092673, 9.916311305349925220, -0.7998128361456281477 ) ) ;
#86721 = LINE ( 'NONE', #105129, #132742 ) ;
#86720 = CARTESIAN_POINT ( 'NONE',  ( 1.576486190600217663, -1.733098801405801304, -0.5742540608338757568 ) ) ;
#86722 = CARTESIAN_POINT ( 'NONE',  ( -4.610654757099099221, 7.536791762327691657, 1.199719254218452935 ) ) ;
#86723 = CARTESIAN_POINT ( 'NONE',  ( -1.387778780781445676E-14, -5.907420853759282053, -10.91970695577495398 ) ) ;
#86724 = CARTESIAN_POINT ( 'NONE',  ( -10.14895191633106819, 4.000000000000000888, 7.601392964450660372 ) ) ;
#86725 = EDGE_LOOP ( 'NONE', ( #154569, #100035, #41332, #132631, #132417, #125052, #153336, #48162 ) ) ;
#86726 = CARTESIAN_POINT ( 'NONE',  ( -6.604230223188181093, 6.877559146573883453, 0.7216878364870317197 ) ) ;
#86727 = CARTESIAN_POINT ( 'NONE',  ( -4.627410500965859264, 4.293067094081919777, 0.7998128361456341429 ) ) ;
#86728 = CARTESIAN_POINT ( 'NONE',  ( -9.622536337397040285, 12.24937836509514710, 1.599625672291281386 ) ) ;
#86729 = CARTESIAN_POINT ( 'NONE',  ( 5.514321518048907578, -2.019862493962302441, 0.002152582845403941403 ) ) ;
#86731 = EDGE_LOOP ( 'NONE', ( #22509, #124055, #5511, #28084 ) ) ;
#86730 = CARTESIAN_POINT ( 'NONE',  ( 6.481102860290734569, -2.029466250747449685, -0.9033904549611364576 ) ) ;
#86732 = CARTESIAN_POINT ( 'NONE',  ( -6.882699257592852504, 8.058845884393651460, -1.199719254218452047 ) ) ;
#86733 = CARTESIAN_POINT ( 'NONE',  ( 4.761938266897790761, 6.578680616179308771, 1.599625672291267398 ) ) ;
#86734 = AXIS2_PLACEMENT_3D ( 'NONE', #63443, #194501, #144736 ) ;
#86735 = CARTESIAN_POINT ( 'NONE',  ( 5.366112562010656895, 1.013659120426290361, 1.794278544449072088 ) ) ;
#86736 = CARTESIAN_POINT ( 'NONE',  ( 4.061172775696818782, -1.158689426361030561, 1.650081270007992318 ) ) ;
#86737 = ORIENTED_EDGE ( 'NONE', *, *, #21894, .F. ) ;
#86738 = VERTEX_POINT ( 'NONE', #35112 ) ;
#86739 = CARTESIAN_POINT ( 'NONE',  ( 2.920214025141053327, 6.445393704534057022, 0.4458799699700779495 ) ) ;
#86740 = CARTESIAN_POINT ( 'NONE',  ( 4.701980345841006326, 4.380065246436280368, 0.7998128361456341429 ) ) ;
#86742 = EDGE_LOOP ( 'NONE', ( #139844, #191414, #125049, #27051 ) ) ;
#86741 = CARTESIAN_POINT ( 'NONE',  ( -6.903036488013351679, 8.082572653217566128, -1.199719254218452047 ) ) ;
#86743 = CARTESIAN_POINT ( 'NONE',  ( 4.617922728991994852, 8.461530327540957686, 0.3091873533234041904 ) ) ;
#86744 = CARTESIAN_POINT ( 'NONE',  ( 4.323592178502837058, -1.495822217463145476, 1.351947993609707632 ) ) ;
#86745 = CARTESIAN_POINT ( 'NONE',  ( 3.714658492009088153, -0.1339090230784936997, 1.836323816731308067 ) ) ;
#86746 = DIRECTION ( 'NONE',  ( 0.000000000000000000, 0.000000000000000000, -1.000000000000000000 ) ) ;
#86747 = CARTESIAN_POINT ( 'NONE',  ( 1.629934303081633340, -2.171740791250169611, 0.7807429155501348639 ) ) ;
#86748 = CARTESIAN_POINT ( 'NONE',  ( 5.820193082016415609, 10.01225203898631655, 0.000000000000000000 ) ) ;
#86749 = EDGE_CURVE ( 'NONE', #104869, #39666, #84726, .T. ) ;
#86750 = CARTESIAN_POINT ( 'NONE',  ( 4.956408742875526130, 0.8222144862577386304, 1.999314050312686053 ) ) ;
#86752 = CARTESIAN_POINT ( 'NONE',  ( 6.936968151686458306, 11.24487994360957188, 0.7998128361456462443 ) ) ;
#86751 = CARTESIAN_POINT ( 'NONE',  ( 3.397672961473942266, -1.985868886743065609, 0.3494831190506141883 ) ) ;
#86753 = CARTESIAN_POINT ( 'NONE',  ( 0.2923913620977801053, 1.614019350141202569, -1.079779171115168523 ) ) ;
#86754 = CARTESIAN_POINT ( 'NONE',  ( -5.949330478298285207, 5.835307067636438028, 0.7998128361456341429 ) ) ;
#86755 = CIRCLE ( 'NONE', #83172, 0.08000000000000020983 ) ;
#86756 = CARTESIAN_POINT ( 'NONE',  ( -6.777498110814238252, 15.51954974125004760, 9.912810906811193590 ) ) ;
#86757 = DIRECTION ( 'NONE',  ( 0.000000000000000000, 0.000000000000000000, 1.000000000000000000 ) ) ;
#86758 = CARTESIAN_POINT ( 'NONE',  ( 2.289737743334671283, -0.8020533187339595749, 1.690132462187944107 ) ) ;
#86759 = CARTESIAN_POINT ( 'NONE',  ( 0.5265599218138971027, 1.885207356905926668, 0.5763402985480212681 ) ) ;
#86761 = CARTESIAN_POINT ( 'NONE',  ( -6.074935347375019390, 9.245119117649618801, 1.199719254218452047 ) ) ;
#86760 = CARTESIAN_POINT ( 'NONE',  ( 1.499999999999987121, -0.4645833326505149907, 0.8660254037844524744 ) ) ;
#86762 = CARTESIAN_POINT ( 'NONE',  ( 1.155211076828046579, -1.737760091701185505, 1.360235214042208263 ) ) ;
#86763 = EDGE_LOOP ( 'NONE', ( #94330, #97182, #79423, #99705 ) ) ;
#86764 = DIRECTION ( 'NONE',  ( 0.000000000000000000, 1.000000000000000000, 0.000000000000000000 ) ) ;
#86765 = CARTESIAN_POINT ( 'NONE',  ( 3.354752944377597856, 6.001296637494123232, -1.199719254218446718 ) ) ;
#86766 = CARTESIAN_POINT ( 'NONE',  ( -4.273844736805832767, 6.009238164405336313, 1.599625672291267398 ) ) ;
#86767 = CARTESIAN_POINT ( 'NONE',  ( -1.040834085586084257E-14, -8.763419982614969683, -10.56339547890105202 ) ) ;
#86768 = CARTESIAN_POINT ( 'NONE',  ( 5.963742398600946792, 1.942370021616221409, -0.3365726279523760800 ) ) ;
#86769 = CARTESIAN_POINT ( 'NONE',  ( 6.604155123031994812, -2.307348207032692944, 0.04906353339812623282 ) ) ;
#86771 = EDGE_CURVE ( 'NONE', #144299, #83007, #17780, .T. ) ;
#86770 = CARTESIAN_POINT ( 'NONE',  ( 6.566864649055507819, 1.378042638564499489, -1.251022615016267103 ) ) ;
#86772 = CARTESIAN_POINT ( 'NONE',  ( 3.924720150778399752, -1.388762634255924500, 1.525101558930273660 ) ) ;
#86773 = CARTESIAN_POINT ( 'NONE',  ( 5.829642864196168617, 6.863966765392747860, 1.082531754730558626 ) ) ;
#86774 = CARTESIAN_POINT ( 'NONE',  ( 6.367489420273535039, 7.457767740854454708, -1.199719254218452047 ) ) ;
#86775 = ORIENTED_EDGE ( 'NONE', *, *, #5273, .T. ) ;
#86776 = CARTESIAN_POINT ( 'NONE',  ( 6.927853306458731986, 11.02631992426980112, 0.7216878364870438212 ) ) ;
#86777 = CARTESIAN_POINT ( 'NONE',  ( -1.201851678989727383E-14, 3.384375000341421469, 1.575800808251672791 ) ) ;
#86778 = CARTESIAN_POINT ( 'NONE',  ( -10.53033573153658153, 3.951415937214838525, -5.758770635485034539 ) ) ;
#86779 = CARTESIAN_POINT ( 'NONE',  ( 3.999292125906894313, 7.609665213625947722, 0.7216878364870317197 ) ) ;
#86780 = CARTESIAN_POINT ( 'NONE',  ( 6.742638747055813120, -2.127943412135436585, -0.4303581323979056017 ) ) ;
#86782 = CARTESIAN_POINT ( 'NONE',  ( 4.862772069579198941, 0.1752732939881325724, -1.832877676746891726 ) ) ;
#86781 = DIRECTION ( 'NONE',  ( 0.000000000000000000, 1.000000000000000000, 0.000000000000000000 ) ) ;
#86783 = CARTESIAN_POINT ( 'NONE',  ( -2.421437874748401775, 3.696394713403113208, 11.55257195323929231 ) ) ;
#86784 = DIRECTION ( 'NONE',  ( 0.8003905296791066215, 0.000000000000000000, -0.5994789404140892231 ) ) ;
#86785 = CARTESIAN_POINT ( 'NONE',  ( 0.7021627906659901885, -0.6242572379067250488, -1.763460184394528341 ) ) ;
#86786 = CARTESIAN_POINT ( 'NONE',  ( -4.211465482254622472, 7.549728682704877514, 0.9859626088348661943 ) ) ;
#86787 = CARTESIAN_POINT ( 'NONE',  ( -0.1476870296772063995, 2.615815853600972130, 2.075651118116234706 ) ) ;
#86788 = CARTESIAN_POINT ( 'NONE',  ( 5.646014316602349759, 7.456765758048159221, -1.329534273556526758 ) ) ;
#86789 = CARTESIAN_POINT ( 'NONE',  ( 0.6625817696367036769, 0.5554855734208345996, 1.829800363923417716 ) ) ;
#86790 =( GEOMETRIC_REPRESENTATION_CONTEXT ( 3 ) GLOBAL_UNCERTAINTY_ASSIGNED_CONTEXT ( ( #52515 ) ) GLOBAL_UNIT_ASSIGNED_CONTEXT ( ( #196720, #32088, #147983 ) ) REPRESENTATION_CONTEXT ( 'NONE', 'WORKASPACE' ) );
#86791 = CARTESIAN_POINT ( 'NONE',  ( 1.480939207288126669, 1.637052324538622816, -0.6731226676765161843 ) ) ;
#86792 = STYLED_ITEM ( 'NONE', ( #137643 ), #70312 ) ;
#86793 = CARTESIAN_POINT ( 'NONE',  ( 6.551439491213440824, -1.797098368391306655, 0.9074013689854224518 ) ) ;
#86795 = CARTESIAN_POINT ( 'NONE',  ( 4.763251566037994600, 1.785832754541897049, -0.6935334960865118248 ) ) ;
#86794 = CARTESIAN_POINT ( 'NONE',  ( -9.612894607289142357, 11.17379744904754801, -1.199719254218441611 ) ) ;
#86796 = MECHANICAL_DESIGN_GEOMETRIC_PRESENTATION_REPRESENTATION (  '', ( #180192 ), #52166 ) ;
#86797 = CARTESIAN_POINT ( 'NONE',  ( -5.346851039111044201, 6.199209027673978412, 7.500000000000000000 ) ) ;
#86798 = CARTESIAN_POINT ( 'NONE',  ( 4.932068866601894364, 1.132370341068598796, 1.611282302955379553 ) ) ;
#86799 = CARTESIAN_POINT ( 'NONE',  ( 6.345964425358009642, -1.322526734765665513, -1.526637064097993157 ) ) ;
#86800 = CARTESIAN_POINT ( 'NONE',  ( -3.460355519985875983, 5.060167411448709629, 1.599625672291267398 ) ) ;
#86801 = CARTESIAN_POINT ( 'NONE',  ( 4.328871119428026049, 0.09166491666120352155, 1.868520897946590598 ) ) ;
#86803 = VERTEX_POINT ( 'NONE', #101183 ) ;
#86802 = CARTESIAN_POINT ( 'NONE',  ( 5.707552393076498198, -0.4128270653469527374, 1.674615006835003639 ) ) ;
#86805 = CARTESIAN_POINT ( 'NONE',  ( 4.039966587192267866, 4.776011108888172707, 1.082531754730560403 ) ) ;
#86804 = CARTESIAN_POINT ( 'NONE',  ( 3.580891165198408110, -2.126768340858419926, -0.5889919780145411732 ) ) ;
#86806 = CARTESIAN_POINT ( 'NONE',  ( -1.364683531250010295, 3.842708333674751398, 0.7879004041258379498 ) ) ;
#86807 = CARTESIAN_POINT ( 'NONE',  ( 0.7661727470247855498, -2.052889565338772204, 0.2005107248105562623 ) ) ;
#86808 = CARTESIAN_POINT ( 'NONE',  ( 7.461064606222022277, 7.598996883547496139, 1.040834085586084257E-14 ) ) ;
#86809 = CARTESIAN_POINT ( 'NONE',  ( -8.585337585951595685, 11.03931315507545108, -1.599625672291263179 ) ) ;
#86810 = CARTESIAN_POINT ( 'NONE',  ( -5.969155412111654790, 15.44727373956653693, -10.36857180707296244 ) ) ;
#86811 = CARTESIAN_POINT ( 'NONE',  ( -3.419573553597315296, -0.02497503617633969886, -0.3927721855967285514 ) ) ;
#86812 = CARTESIAN_POINT ( 'NONE',  ( -1.579999999999998073, 6.280000000000042881, -2.579999999999995630 ) ) ;
#86813 = ORIENTED_EDGE ( 'NONE', *, *, #151561, .T. ) ;
#86814 = CARTESIAN_POINT ( 'NONE',  ( 3.279797552538410876, -1.996039814156633785, 0.5495672325947635883 ) ) ;
#86815 = CARTESIAN_POINT ( 'NONE',  ( -1.500000000000011324, 4.629166666666689522, -0.8660254037844313801 ) ) ;
#86816 = CARTESIAN_POINT ( 'NONE',  ( 4.123651276850781144, 7.962676922967908411, -0.7998128361456221525 ) ) ;
#86817 = CARTESIAN_POINT ( 'NONE',  ( -6.569648045741773856, 6.787758985223060648, 0.3860807628459517749 ) ) ;
#86819 = ADVANCED_FACE ( 'NONE', ( #131618 ), #144778, .T. ) ;
#86818 = CARTESIAN_POINT ( 'NONE',  ( 1.207682226051248753, 1.530763495831432452, 1.317637323925124671 ) ) ;
#86820 = CARTESIAN_POINT ( 'NONE',  ( 1.734723475976807094E-15, -3.469446951953614189E-15, 0.2936757779752607878 ) ) ;
#86821 = EDGE_CURVE ( 'NONE', #166004, #26662, #18819, .T. ) ;
#86823 = CARTESIAN_POINT ( 'NONE',  ( 7.592202833972727660, 11.80139437303613015, -0.7216878364870267237 ) ) ;
#86822 = CARTESIAN_POINT ( 'NONE',  ( 0.07499057489267992038, 0.7202342490539682673, -2.037914685249627045 ) ) ;
#86824 = CARTESIAN_POINT ( 'NONE',  ( 6.169296033003512925, -0.7230314695168098549, -1.882185070641306801 ) ) ;
#86825 = CARTESIAN_POINT ( 'NONE',  ( 5.348823992091742419, -1.734843432642660721, -0.8128511771108116735 ) ) ;
#86826 = FACE_BOUND ( 'NONE', #55845, .T. ) ;
#86827 = CARTESIAN_POINT ( 'NONE',  ( 4.054362073078698891, -1.623213109359676443, 1.472610181411205144 ) ) ;
#86828 = CARTESIAN_POINT ( 'NONE',  ( -1.500000000000011324, 3.452083334016151639, 0.8660254037844403729 ) ) ;
#86829 = CARTESIAN_POINT ( 'NONE',  ( 1.951281838316549777, -1.706683157587106425, 0.8630329916254892986 ) ) ;
#86830 = CARTESIAN_POINT ( 'NONE',  ( -4.660252114795309097, 6.460046772059735432, -1.599625672291256295 ) ) ;
#86831 = CARTESIAN_POINT ( 'NONE',  ( 4.324687812634892659, 5.108185871904570519, 1.082531754730560403 ) ) ;
#86833 = CARTESIAN_POINT ( 'NONE',  ( 1.370720498019749378, -0.2986500928384462350, -1.994069080148860973 ) ) ;
#86832 = SURFACE_STYLE_FILL_AREA ( #5540 ) ;
#86834 = CARTESIAN_POINT ( 'NONE',  ( 0.6823417656249969321, 11.33854166700806765, -1.181850606188757036 ) ) ;
#86836 = CARTESIAN_POINT ( 'NONE',  ( -4.308458954092677651, 8.248562223075252220, -0.7998128361456362523 ) ) ;
#86835 = CARTESIAN_POINT ( 'NONE',  ( 6.515165533258342023, -2.126321577054360201, 0.5302794918828001025 ) ) ;
#86838 = ORIENTED_EDGE ( 'NONE', *, *, #78041, .F. ) ;
#86837 = CARTESIAN_POINT ( 'NONE',  ( 3.469487465715580310, 1.682841854137674398, -0.3771888234031828824 ) ) ;
#86839 = CARTESIAN_POINT ( 'NONE',  ( -0.1405533004718676759, 6.947778977978678050, -2.315285900534403307 ) ) ;
#86840 = CARTESIAN_POINT ( 'NONE',  ( 6.584456157731144899, 10.83361595066169514, -0.7998128361456291469 ) ) ;
#86841 = CARTESIAN_POINT ( 'NONE',  ( 3.337278367258157630, 7.045241861776501580, 0.7998128361456341429 ) ) ;
#86842 = LINE ( 'NONE', #103095, #54092 ) ;
#86843 = CARTESIAN_POINT ( 'NONE',  ( 1.521847698614446687, 1.933392594956625521, -0.3320675068423510345 ) ) ;
#86844 = CARTESIAN_POINT ( 'NONE',  ( 3.673896439623286714, 4.156855427197417185, 2.420000000000023022 ) ) ;
#86845 = CARTESIAN_POINT ( 'NONE',  ( 3.357615597678655917, 7.068968630600412695, 0.7998128361456321445 ) ) ;
#86846 = CARTESIAN_POINT ( 'NONE',  ( 0.07536363704233395300, 5.720741966631408104, -2.738263776839637398 ) ) ;
#86847 = ORIENTED_EDGE ( 'NONE', *, *, #180401, .F. ) ;
#86848 = CARTESIAN_POINT ( 'NONE',  ( 0.4350533241460359801, -6.938200158402027640, 9.251576347356904151 ) ) ;
#86849 = B_SPLINE_CURVE_WITH_KNOTS ( 'NONE', 3,
 ( #157540, #156470, #109914, #8058 ),
 .UNSPECIFIED., .F., .F.,
 ( 4, 4 ),
 ( 7.552443772458755810E-16, 0.0003455271673302856279 ),
 .UNSPECIFIED. ) ;
#86850 = VERTEX_POINT ( 'NONE', #153147 ) ;
#86851 = CARTESIAN_POINT ( 'NONE',  ( 3.387185712204858312, 0.04143215291275677975, -1.811162278692766581 ) ) ;
#86852 = ORIENTED_EDGE ( 'NONE', *, *, #147049, .T. ) ;
#86853 = CARTESIAN_POINT ( 'NONE',  ( 9.459838494033030898, 12.05956421450382088, 1.599625672291281386 ) ) ;
#86854 = CARTESIAN_POINT ( 'NONE',  ( 4.598150373690133463, 5.393538853173795111, -1.199719254218452047 ) ) ;
#86855 = CARTESIAN_POINT ( 'NONE',  ( 4.652869415276386533, 0.3145016728411016982, 1.783790502623605834 ) ) ;
#86856 = CARTESIAN_POINT ( 'NONE',  ( 7.309254211098760834, 8.660456346770972758, 1.082531754730549967 ) ) ;
#86857 =( NAMED_UNIT ( * ) PLANE_ANGLE_UNIT ( ) SI_UNIT ( $, .RADIAN. ) );
#86858 = CARTESIAN_POINT ( 'NONE',  ( 5.827790676886797527, 6.016211147664318304, -0.4261259532085531765 ) ) ;
#86860 = CARTESIAN_POINT ( 'NONE',  ( -1.364683531250010295, 15.13020833367473017, 0.7879004041258445001 ) ) ;
#86859 = CARTESIAN_POINT ( 'NONE',  ( 5.652756593210860103, -0.4525561148686143009, -1.805067620203390177 ) ) ;
#86861 = CARTESIAN_POINT ( 'NONE',  ( 2.706530202829552145, 1.804627309565815185, 0.6429686382581675241 ) ) ;
#86862 = DIRECTION ( 'NONE',  ( 0.000000000000000000, 1.000000000000000000, 0.000000000000000000 ) ) ;
#86863 = CARTESIAN_POINT ( 'NONE',  ( -10.91675076000969113, 4.673595418013491987, -4.467283485442433921 ) ) ;
#86864 = B_SPLINE_CURVE_WITH_KNOTS ( 'NONE', 3,
 ( #143252, #127045, #208187, #9994, #4896, #92358 ),
 .UNSPECIFIED., .F., .F.,
 ( 4, 2, 4 ),
 ( 0.001616326159039276067, 0.001719602896561277672, 0.001822879634083279061 ),
 .UNSPECIFIED. ) ;
#86865 = CARTESIAN_POINT ( 'NONE',  ( 9.499671278040523248, -9.915617081696053603, -0.07902916658836418862 ) ) ;
#86866 = CARTESIAN_POINT ( 'NONE',  ( 6.480434237652124452, 8.583592582059388576, 1.443375672974076540 ) ) ;
#86867 = CARTESIAN_POINT ( 'NONE',  ( -2.754277761870538299, 6.365074488824250309, 1.040834085586084257E-14 ) ) ;
#86868 = CARTESIAN_POINT ( 'NONE',  ( 11.89942855770814312, 12.30000000000000071, -0.7000000000000009548 ) ) ;
#86869 = CARTESIAN_POINT ( 'NONE',  ( -4.762657100150483380, 8.778460060142702304, 0.000000000000000000 ) ) ;
#86870 = CARTESIAN_POINT ( 'NONE',  ( 1.816468492311611893, 1.951142502984483107, 0.7513475392508098816 ) ) ;
#86871 = CARTESIAN_POINT ( 'NONE',  ( 5.692444392891300886, 7.734547439830227411, -1.599625672291281386 ) ) ;
#86872 = CARTESIAN_POINT ( 'NONE',  ( 6.827182134110199030, 0.001020705822914885546, 1.910856149448316721 ) ) ;
#86873 = CARTESIAN_POINT ( 'NONE',  ( -5.362413449404877852, 6.214902764849178141, -1.199719254218446718 ) ) ;
#86874 = CARTESIAN_POINT ( 'NONE',  ( 2.274178591966895091, -1.125271047149905890, 1.437439779654096750 ) ) ;
#86875 = CARTESIAN_POINT ( 'NONE',  ( 11.72719273365024506, 8.694648967210921953, 4.374500150831954315 ) ) ;
#86876 = CARTESIAN_POINT ( 'NONE',  ( 2.338023529656753752, -1.104205016203146705, -1.561194055274425452 ) ) ;
#86877 = CARTESIAN_POINT ( 'NONE',  ( 1.978894816976022097, 1.836590731562221412, 0.7118427970769640734 ) ) ;
#86878 = CARTESIAN_POINT ( 'NONE',  ( 3.685046248344743258, 1.408799512439436352, 1.336988689110546913 ) ) ;
#86879 = ORIENTED_EDGE ( 'NONE', *, *, #195623, .F. ) ;
#86880 = CARTESIAN_POINT ( 'NONE',  ( -3.804741806807946602, 4.044702255324862605, -0.8707498557368220649 ) ) ;
#86881 = CARTESIAN_POINT ( 'NONE',  ( -3.657667580636712934, 7.489305620709952649, -0.7998128361456481317 ) ) ;
#86883 = CARTESIAN_POINT ( 'NONE',  ( 4.693665235656380830, 1.977662049654808740, -0.7657889336421249693 ) ) ;
#86882 = CARTESIAN_POINT ( 'NONE',  ( 3.074666975249065626, 6.809138247757705820, 0.000000000000000000 ) ) ;
#86884 = CARTESIAN_POINT ( 'NONE',  ( -6.615342224808818727, 6.750480251133849308, 0.3470571717737805373 ) ) ;
#86885 = CARTESIAN_POINT ( 'NONE',  ( 9.908311333488716954, 10.45411806535867782, 0.7998128361456462443 ) ) ;
#86886 = CARTESIAN_POINT ( 'NONE',  ( 5.966167892564917530, 6.109520806784549229, 0.6870465322655286977 ) ) ;
#86887 = DIRECTION ( 'NONE',  ( 0.000000000000000000, 0.000000000000000000, -1.000000000000000000 ) ) ;
#86888 = ORIENTED_EDGE ( 'NONE', *, *, #126196, .T. ) ;
#86889 = TOROIDAL_SURFACE ( 'NONE', #111078, 12.17999999982603576, 0.5000000000000008882 ) ;
#86890 = CARTESIAN_POINT ( 'NONE',  ( 6.387826650694035990, 7.481494509678370264, -1.199719254218452047 ) ) ;
#86891 = CARTESIAN_POINT ( 'NONE',  ( -15.75000000000000000, 10.19999999999999929, 1.099999999999996758 ) ) ;
#86892 = CARTESIAN_POINT ( 'NONE',  ( 3.826616632296374831, 1.734130841282412128, 0.5711148077138239465 ) ) ;
#86893 = CARTESIAN_POINT ( 'NONE',  ( -3.189213936345698830, 2.817530495244580102, 2.450448857954578230 ) ) ;
#86894 = CARTESIAN_POINT ( 'NONE',  ( -9.544576954340667996, 11.19805653722800365, 1.082531754730558626 ) ) ;
#86895 = CARTESIAN_POINT ( 'NONE',  ( -4.599258460307840579, 8.480642220064158465, 0.2485357878534207865 ) ) ;
#86896 = CARTESIAN_POINT ( 'NONE',  ( 0.000000000000000000, 2.499999999999998668, 0.000000000000000000 ) ) ;
#86897 = CARTESIAN_POINT ( 'NONE',  ( 4.785944050937030347, -0.8815013282119155136, 1.649949660215948688 ) ) ;
#86898 = CARTESIAN_POINT ( 'NONE',  ( 7.426115451983150706, 9.686887332112256388, -1.599625672291262513 ) ) ;
#86899 = CARTESIAN_POINT ( 'NONE',  ( 1.998540859798603408, -0.5134167636005394497, -1.856760371892735906 ) ) ;
#86900 = CARTESIAN_POINT ( 'NONE',  ( 0.7035002141062960401, 2.800000000000067768, 1.266925154657448038 ) ) ;
#86901 = VECTOR ( 'NONE', #103354, 1000.000000000000114 ) ;
#86902 = CARTESIAN_POINT ( 'NONE',  ( 2.706824224222692088, 6.309712028235118453, 0.7998128361456362523 ) ) ;
#86903 = CARTESIAN_POINT ( 'NONE',  ( -1.364683531250000748, 8.671875000341403350, 0.000000000000000000 ) ) ;
#86904 = CARTESIAN_POINT ( 'NONE',  ( -7.400052914960538963, 7.527816577075747695, 1.040834085586084257E-14 ) ) ;
#86905 = CARTESIAN_POINT ( 'NONE',  ( 4.202137545231717120, 6.989912005157271402, 1.199719254218462483 ) ) ;
#86906 = CARTESIAN_POINT ( 'NONE',  ( -4.299344108864949554, 8.030002203735486788, -0.7216878364870338292 ) ) ;
#86907 = CARTESIAN_POINT ( 'NONE',  ( 1.441172756004579947, -1.817888344413360668, -1.085095524780084864 ) ) ;
#86908 = CARTESIAN_POINT ( 'NONE',  ( -0.3282377607281271592, 0.5111645503674250302, -1.225000000000009859 ) ) ;
#86909 = CARTESIAN_POINT ( 'NONE',  ( -1.378728738066235859, 3.613591550242559070, -0.5908528300941767730 ) ) ;
#86910 = CARTESIAN_POINT ( 'NONE',  ( 5.911005882915712384, -1.635593682349820721, 1.269112435710928688 ) ) ;
#86912 = CARTESIAN_POINT ( 'NONE',  ( 4.221210552267129046, 7.311159377000789661, -0.8807526815687096722 ) ) ;
#86911 = CARTESIAN_POINT ( 'NONE',  ( 0.5382993156314471728, -1.579489783069366604, 0.9460463261394758128 ) ) ;
#86913 = CARTESIAN_POINT ( 'NONE',  ( 6.574781987728091970, -0.9847942639734930115, 2.074158207377621910 ) ) ;
#86914 = CARTESIAN_POINT ( 'NONE',  ( 4.528060117284222308, 8.226561203566173930, 0.7216878364870438212 ) ) ;
#86916 = CARTESIAN_POINT ( 'NONE',  ( 0.1245482448182331087, 6.487495393664095111, 3.100011470320013895 ) ) ;
#86915 = CARTESIAN_POINT ( 'NONE',  ( 3.418064124421011041, 7.001842221884225559, -0.7216878364870338292 ) ) ;
#86917 = CARTESIAN_POINT ( 'NONE',  ( 1.131297326486919497, -2.070297854115164871, 0.9843215409001818683 ) ) ;
#86918 = CARTESIAN_POINT ( 'NONE',  ( -0.04698948850442342950, -9.984793193541563028, -9.579582872750561862 ) ) ;
#86919 = CARTESIAN_POINT ( 'NONE',  ( -5.315678745009726924, 8.359319748223434487, -1.199719254218453823 ) ) ;
#86920 = CARTESIAN_POINT ( 'NONE',  ( 6.316353394666050391, 1.812894500769960837, 0.6965700268309078513 ) ) ;
#86921 = ORIENTED_EDGE ( 'NONE', *, *, #111248, .F. ) ;
#86922 = CARTESIAN_POINT ( 'NONE',  ( 9.205623113554628034, 9.842241175342985926, 0.7216878364870458196 ) ) ;
#86923 = ORIENTED_EDGE ( 'NONE', *, *, #54763, .T. ) ;
#86924 = CARTESIAN_POINT ( 'NONE',  ( 5.994389040191065554, -1.017321598621454548, 1.619163160827830517 ) ) ;
#86925 = CARTESIAN_POINT ( 'NONE',  ( 0.000000000000000000, 15.50000000000019362, 0.000000000000000000 ) ) ;
#86927 = CARTESIAN_POINT ( 'NONE',  ( 7.654042494670958593E-16, 3.799999999999998046, -6.250000000000000000 ) ) ;
#86926 = CARTESIAN_POINT ( 'NONE',  ( -8.341290820905609138, 10.75459192918846618, 1.599625672291269396 ) ) ;
#86928 = CARTESIAN_POINT ( 'NONE',  ( 9.481348452320371933, -9.006862915010128035, -0.5950054837411746789 ) ) ;
#86930 = CARTESIAN_POINT ( 'NONE',  ( 1.551229123295729373, 0.5181449431543529993, -1.692289574110398931 ) ) ;
#86929 = CARTESIAN_POINT ( 'NONE',  ( 3.275413508211636238, 1.326730841477074208, 1.615706224610208519 ) ) ;
#86931 = CARTESIAN_POINT ( 'NONE',  ( 11.35605497252127449, 9.985818540483530015, 3.553547709190206572 ) ) ;
#86932 = MANIFOLD_SOLID_BREP ( 'Fillet3', #101943 ) ;
#86934 = CARTESIAN_POINT ( 'NONE',  ( 4.629038687585553369, -2.096899809942855075, 0.9264041093646653291 ) ) ;
#86933 = CARTESIAN_POINT ( 'NONE',  ( 3.790386463472274148, 6.579812086429759788, 1.199719254218452047 ) ) ;
#86935 = CARTESIAN_POINT ( 'NONE',  ( 3.468456934111513235, 0.04105959252117792613, -1.740014521098575351 ) ) ;
#86936 = CARTESIAN_POINT ( 'NONE',  ( 10.71502147350184231, 11.39527989537399755, 0.000000000000000000 ) ) ;
#86937 = CARTESIAN_POINT ( 'NONE',  ( 6.412080304620305427, 6.445458208337293549, -0.7998128361456481317 ) ) ;
#86938 = CARTESIAN_POINT ( 'NONE',  ( 3.022450238936627009, 1.725798670860735351, -0.1664453034943418896 ) ) ;
#86939 = CARTESIAN_POINT ( 'NONE',  ( 3.578747896202236323, 1.379726198893852729, -1.676393335895840497 ) ) ;
#86940 = CARTESIAN_POINT ( 'NONE',  ( 3.960953433486789521, 7.772862772376584850, -0.7998128361456221525 ) ) ;
#86941 = CARTESIAN_POINT ( 'NONE',  ( 4.628138809701114020, 2.011451458044950069, 0.1435230606586651581 ) ) ;
#86942 = CARTESIAN_POINT ( 'NONE',  ( 2.031250000000000888, -0.7852924748300881275, -1.895863743164043491 ) ) ;
#86943 = CARTESIAN_POINT ( 'NONE',  ( -1.500000000000013101, 2.702083334016155636, 0.8660254037844403729 ) ) ;
#86944 = CARTESIAN_POINT ( 'NONE',  ( 2.573164103464478991, 0.09656903795818297387, -1.924097065980167942 ) ) ;
#86945 = CARTESIAN_POINT ( 'NONE',  ( -0.6823417656250039265, 15.31770833367473372, -1.181850606188755259 ) ) ;
#86946 = CARTESIAN_POINT ( 'NONE',  ( 5.062811918942510481, 0.6453760322048059939, 2.125560002649288460 ) ) ;
#86947 = ORIENTED_EDGE ( 'NONE', *, *, #171813, .F. ) ;
#86948 = CARTESIAN_POINT ( 'NONE',  ( -1.500000000000013101, 2.129166666666693519, -0.8660254037844313801 ) ) ;
#86949 = CARTESIAN_POINT ( 'NONE',  ( 5.099838337034727331, 9.101561826515851550, -0.7998128361456281477 ) ) ;
#86950 = CARTESIAN_POINT ( 'NONE',  ( 5.653386866774156694, 5.697965554099049257, -0.7216878364870207285 ) ) ;
#86951 = DIRECTION ( 'NONE',  ( 0.000000000000000000, 0.000000000000000000, -1.000000000000000000 ) ) ;
#86952 = EDGE_CURVE ( 'NONE', #131029, #141526, #70797, .T. ) ;
#86953 = CARTESIAN_POINT ( 'NONE',  ( 1.155278206730834256, 0.4382352071879510036, 2.177490050429623736 ) ) ;
#86954 = CARTESIAN_POINT ( 'NONE',  ( 5.793401095800717826, -1.774274828963496198, 0.8374297333502839225 ) ) ;
#86955 = CARTESIAN_POINT ( 'NONE',  ( 8.649738815838679429, 10.15407870897571563, -1.082531754730543083 ) ) ;
#86956 = ADVANCED_FACE ( 'NONE', ( #188844 ), #209319, .T. ) ;
#86957 = CARTESIAN_POINT ( 'NONE',  ( -0.2916131387015714060, 3.292968587997009422, 2.053236966640526351 ) ) ;
#86958 = CARTESIAN_POINT ( 'NONE',  ( 6.661402789601885033, 0.3967159107356016401, -2.227235065690711835 ) ) ;
#86959 = CARTESIAN_POINT ( 'NONE',  ( -5.153507786970275006, 7.105788066255672497, -1.443375672974066548 ) ) ;
#86960 = CARTESIAN_POINT ( 'NONE',  ( 2.893094712532847890, 0.2500570216604477980, 2.047387263510790145 ) ) ;
#86961 = CARTESIAN_POINT ( 'NONE',  ( -4.578903193113314174, 6.365139696764064325, 1.599625672291267398 ) ) ;
#86962 = CARTESIAN_POINT ( 'NONE',  ( 1.499999999999989120, 4.577083334016148974, -0.8660254037844323793 ) ) ;
#86963 = CARTESIAN_POINT ( 'NONE',  ( 0.6823417656249899377, 5.488541667008087543, -1.181850606188754593 ) ) ;
#86964 = CARTESIAN_POINT ( 'NONE',  ( 5.184763189090160651, -0.2277032997176874074, -1.856539885857370953 ) ) ;
#86965 = CARTESIAN_POINT ( 'NONE',  ( 3.603937110245566178, -0.1228517400825197836, 1.729840182746833266 ) ) ;
#86966 = CARTESIAN_POINT ( 'NONE',  ( 3.755166387800693339, 1.726757624646685807, -0.2173075579294906912 ) ) ;
#86967 = CARTESIAN_POINT ( 'NONE',  ( 1.224644656679523713, 2.210950556192964989, 0.6053773189644614527 ) ) ;
#86968 = CARTESIAN_POINT ( 'NONE',  ( 1.364683531249990311, 3.696875000341416584, 1.214306433183764966E-14 ) ) ;
#86969 = CARTESIAN_POINT ( 'NONE',  ( 5.021074897447791230, -1.984789774362485604, 0.6572858584967393725 ) ) ;
#86970 = CARTESIAN_POINT ( 'NONE',  ( 6.703083108286362446, -0.4264415456523527603, 1.901745634116110084 ) ) ;
#86971 = CARTESIAN_POINT ( 'NONE',  ( 0.000000000000000000, -0.2000000000000057288, 6.399999999999999467 ) ) ;
#86972 = CARTESIAN_POINT ( 'NONE',  ( 1.283827520628720187, 1.646837967535810021, -1.163270716046126196 ) ) ;
#86973 = CARTESIAN_POINT ( 'NONE',  ( 0.1819133275808570704, -1.029140439971199417, 1.934768540691175431 ) ) ;
#86974 = CARTESIAN_POINT ( 'NONE',  ( 9.599742726594369557, 13.73983281947659840, -8.263962686181493211 ) ) ;
#86975 = CARTESIAN_POINT ( 'NONE',  ( -8.690940161559884913, 10.09818392903003748, 1.199719254218462483 ) ) ;
#86976 = CARTESIAN_POINT ( 'NONE',  ( 4.821896187954575197, 8.777295985922343391, 0.7998128361456462443 ) ) ;
#86977 = CARTESIAN_POINT ( 'NONE',  ( 2.631617588254760776, -0.2053842346896698201, 2.110501108333342035 ) ) ;
#86978 = CARTESIAN_POINT ( 'NONE',  ( 1.364683531249988757, -0.8656249996585805295, 0.000000000000000000 ) ) ;
#86979 = CARTESIAN_POINT ( 'NONE',  ( 4.951681858558426796, 0.5695450498939165218, -1.734646904759745700 ) ) ;
#86980 = ORIENTED_EDGE ( 'NONE', *, *, #186000, .T. ) ;
#86981 = CARTESIAN_POINT ( 'NONE',  ( -5.121948170912633991, 9.197632976031879792, -0.7998128361456362523 ) ) ;
#86982 = CARTESIAN_POINT ( 'NONE',  ( 1.642778471875001811, -0.7802083328553761632, 2.845375778867859751 ) ) ;
#86983 = CARTESIAN_POINT ( 'NONE',  ( -7.802881099864745984, 9.062115023719057305, -1.199719254218446718 ) ) ;
#86984 = CARTESIAN_POINT ( 'NONE',  ( 2.584245202030683419, 1.084020786718616680, 1.704056320703779992 ) ) ;
#86985 = CARTESIAN_POINT ( 'NONE',  ( 0.08314155087942810829, -0.1569203414564980525, -2.071771216027401774 ) ) ;
#86986 = CARTESIAN_POINT ( 'NONE',  ( -3.471769853551161411, 6.208092708188416076, 1.199719254218452935 ) ) ;
#86987 = CARTESIAN_POINT ( 'NONE',  ( 4.328838875689292820, -1.735142615721802395, -0.6730405439913983434 ) ) ;
#86988 = CARTESIAN_POINT ( 'NONE',  ( 7.879259827836241570, 12.34422023245099176, 1.040834085586084257E-14 ) ) ;
#86989 = CARTESIAN_POINT ( 'NONE',  ( 3.173948600550551724, 6.437700466846534297, 0.6171826442077615882 ) ) ;
#86990 = CARTESIAN_POINT ( 'NONE',  ( -4.874319919312905647, 5.645460313075203018, -1.199719254218446718 ) ) ;
#86991 = CARTESIAN_POINT ( 'NONE',  ( -8.182509401047415309, 9.505014708432145909, 1.199719254218462483 ) ) ;
#86992 = CARTESIAN_POINT ( 'NONE',  ( 5.426323838365306074, 1.084245000580752238, -1.468710674947353967 ) ) ;
#86994 = CARTESIAN_POINT ( 'NONE',  ( -4.103765016252827635, 7.679818082383993882, -0.7602138238151506799 ) ) ;
#86993 = CARTESIAN_POINT ( 'NONE',  ( -7.262327558775498737, 8.501745569106741840, 1.199719254218452047 ) ) ;
#86995 = CARTESIAN_POINT ( 'NONE',  ( 1.364683531249988757, -0.8656249996585805295, 0.000000000000000000 ) ) ;
#86996 = CARTESIAN_POINT ( 'NONE',  ( 1.633743589071215974, 0.1333172958793479579, -1.728787957231948447 ) ) ;
#86997 = CARTESIAN_POINT ( 'NONE',  ( 0.09317796543232242934, -1.739829294281483474, -0.04824335600969902743 ) ) ;
#86999 = CARTESIAN_POINT ( 'NONE',  ( 8.920901888112002354, 9.510066412326583674, 0.7216878364870438212 ) ) ;
#86998 = CARTESIAN_POINT ( 'NONE',  ( 5.602268381685036935, -2.307868969066428022, -0.005371834822459965395 ) ) ;
#87000 = CARTESIAN_POINT ( 'NONE',  ( 4.577813143269636065, 5.369812084349879555, -1.199719254218450271 ) ) ;
#87001 = CARTESIAN_POINT ( 'NONE',  ( 1.950533276942335137, 0.6436621796281314367, 1.957774297735858759 ) ) ;
#87002 = CARTESIAN_POINT ( 'NONE',  ( 5.198661835836162481, 8.152523677529138979, 1.199719254218462483 ) ) ;
#87003 = CARTESIAN_POINT ( 'NONE',  ( 6.714253291261501388, -1.839887274036870357, -1.377324995421406628 ) ) ;
#87004 = CARTESIAN_POINT ( 'NONE',  ( 9.100780844468317810, 14.29763700255456449, -7.752528009982434298 ) ) ;
#87005 = CARTESIAN_POINT ( 'NONE',  ( -5.101610940492132151, 9.173906207207963348, -0.7998128361456362523 ) ) ;
#87006 = VECTOR ( 'NONE', #71818, 1000.000000000000114 ) ;
#87007 = CARTESIAN_POINT ( 'NONE',  ( 6.473518811298506925, 1.789458955665638618, -0.5451884755478533240 ) ) ;
#87009 = CARTESIAN_POINT ( 'NONE',  ( -2.823841133396259639, 6.516508098929413961, -0.7998128361456481317 ) ) ;
#87008 = CARTESIAN_POINT ( 'NONE',  ( 3.322422747544371280, -0.7792853099402965444, -1.746611395919236642 ) ) ;
#87010 = CARTESIAN_POINT ( 'NONE',  ( 4.600333186373093852, -2.206333364838486411, -0.05604163552313382035 ) ) ;
#87011 = CARTESIAN_POINT ( 'NONE',  ( -1.225000000000040057, 2.333333334016198801, 0.7072540797572637317 ) ) ;
#87012 = CARTESIAN_POINT ( 'NONE',  ( 0.4019237886466816012, 10.67633545031537246, -1.499999999999998668 ) ) ;
#87013 = CARTESIAN_POINT ( 'NONE',  ( 4.136646265500957043, 5.919449624541475607, -1.443375672974068769 ) ) ;
#87014 = CARTESIAN_POINT ( 'NONE',  ( -6.427974226210522168, 6.671927150099951298, 0.000000000000000000 ) ) ;
#87015 = CARTESIAN_POINT ( 'NONE',  ( 6.094406630213895504, -1.134638919006492275, 1.791192486788994120 ) ) ;
#87016 = ORIENTED_EDGE ( 'NONE', *, *, #20202, .T. ) ;
#87017 = CARTESIAN_POINT ( 'NONE',  ( 3.733692867724636599, -2.133222801268436442, 0.8804087197434546930 ) ) ;
#87019 = EDGE_CURVE ( 'NONE', #37648, #178928, #193473, .T. ) ;
#87018 = CARTESIAN_POINT ( 'NONE',  ( 3.437899435096212208, 1.242623406730450908, 1.518177208742684803 ) ) ;
#87020 = CARTESIAN_POINT ( 'NONE',  ( -3.962726036944197450, 7.845207153068689543, -0.7998128361456481317 ) ) ;
#87021 = CARTESIAN_POINT ( 'NONE',  ( 0.3562053913853078790, -1.961198556353323186, -0.05404869553313899899 ) ) ;
#87022 = CARTESIAN_POINT ( 'NONE',  ( 0.000000000000000000, 14.55305236562705318, 0.000000000000000000 ) ) ;
#87023 = CARTESIAN_POINT ( 'NONE',  ( -9.333041836230234978, 15.44694763438833540, 7.472413793097425483 ) ) ;
#87024 = ORIENTED_EDGE ( 'NONE', *, *, #62930, .F. ) ;
#87025 = CARTESIAN_POINT ( 'NONE',  ( 5.665250009225348826, 1.861346387706263261, -0.7762253298396750711 ) ) ;
#87026 = CARTESIAN_POINT ( 'NONE',  ( -7.808606406466886973, 11.19745900993164511, 1.199719254218453823 ) ) ;
#87027 = PLANE ( 'NONE',  #210080 ) ;
#87028 = CARTESIAN_POINT ( 'NONE',  ( 3.081114545232612301, 2.042771114613873173, 0.7355539269583191153 ) ) ;
#87029 = CARTESIAN_POINT ( 'NONE',  ( 1.419999999999990603, 6.200000000000045475, 2.580000000000000515 ) ) ;
#87030 = CARTESIAN_POINT ( 'NONE',  ( 0.4223351350958382544, -2.109807164369668087, 0.2139620856976830743 ) ) ;
#87031 = CARTESIAN_POINT ( 'NONE',  ( -1.499999999999997780, 1.681250000682817047, 0.000000000000000000 ) ) ;
#87032 = CARTESIAN_POINT ( 'NONE',  ( 8.367353357928214663, 12.91366268422496688, 1.040834085586084257E-14 ) ) ;
#87033 = CARTESIAN_POINT ( 'NONE',  ( 11.86145016429273191, 10.90000000000000036, -1.100000000000002087 ) ) ;
#87034 = CARTESIAN_POINT ( 'NONE',  ( 5.753927575595171540, 7.371122731025397279, 1.306365966420112601 ) ) ;
#87035 = CARTESIAN_POINT ( 'NONE',  ( 1.247419646546283234, -1.622699693697586820, -1.270148745232473564 ) ) ;
#87036 = AXIS2_PLACEMENT_3D ( 'NONE', #89263, #172643, #71898 ) ;
#87038 = LINE ( 'NONE', #34018, #166007 ) ;
#87037 = CARTESIAN_POINT ( 'NONE',  ( -8.967828540435322182, 12.54988483289483980, 1.199719254218462483 ) ) ;
#87039 = CARTESIAN_POINT ( 'NONE',  ( -1.364683531250012516, 2.238541667008087988, -0.7879004041258289570 ) ) ;
#87040 = CARTESIAN_POINT ( 'NONE',  ( 1.500000000000016209, 5.504166666666685082, 0.8660254037844364872 ) ) ;
#87041 = EDGE_CURVE ( 'NONE', #3254, #174147, #203806, .T. ) ;
#87042 = ORIENTED_EDGE ( 'NONE', *, *, #68949, .T. ) ;
#87043 = CARTESIAN_POINT ( 'NONE',  ( 4.283787348595206268, 1.854039900284172315, -0.4678174759695231666 ) ) ;
#87044 = CARTESIAN_POINT ( 'NONE',  ( 7.388267364804250725, 7.584343111885245570, -0.7998128361456341429 ) ) ;
#87045 = CARTESIAN_POINT ( 'NONE',  ( -4.776550190716183586, 4.467063398790632966, 1.214306433183764966E-14 ) ) ;
#87046 = CARTESIAN_POINT ( 'NONE',  ( 0.2811518721992244951, 0.1772043297433387177, -1.802849762578159876 ) ) ;
#87048 = CARTESIAN_POINT ( 'NONE',  ( 0.9892949506953198080, -0.4622125203353181222, 1.859009271263431184 ) ) ;
#87047 = CARTESIAN_POINT ( 'NONE',  ( 1.499999999999990674, 8.226475397238111498, -3.114076396432628346 ) ) ;
#87049 = CARTESIAN_POINT ( 'NONE',  ( 1.697802635435996743, -1.498143435978617877, -1.429203828351800487 ) ) ;
#87050 = CARTESIAN_POINT ( 'NONE',  ( -0.6823417656250003738, 0.5302083336747518416, -1.181850606188749264 ) ) ;
#87051 = COLOUR_RGB ( '', 0.31764706, 0.68627451, 0.89019608) ;
#87052 = CARTESIAN_POINT ( 'NONE',  ( 0.08089089327990153788, -0.1352431037574420292, -1.940231264204687722 ) ) ;
#87053 = CARTESIAN_POINT ( 'NONE',  ( 3.088313589057069208, -1.798746773638896457, -0.3115406389907551810 ) ) ;
#87055 = CARTESIAN_POINT ( 'NONE',  ( 6.479309170914094196, 6.755949689298615723, 0.1985876171829506487 ) ) ;
#87054 = CARTESIAN_POINT ( 'NONE',  ( 0.1183777584694784279, -2.261842813846013822, 0.4569907027171058456 ) ) ;
#87056 = CARTESIAN_POINT ( 'NONE',  ( -1.364683531250000748, 1.009375000341421247, 0.000000000000000000 ) ) ;
#87057 = CARTESIAN_POINT ( 'NONE',  ( 4.475086314992714698, 1.884572246790953365, 0.8388810360253369236 ) ) ;
#87058 = CARTESIAN_POINT ( 'NONE',  ( -7.074657228232555717, 7.148188275893099686, 1.040834085586084257E-14 ) ) ;
#87059 = CARTESIAN_POINT ( 'NONE',  ( 8.046927864910717432, 9.346836249606042202, 1.199719254218462483 ) ) ;
#87060 = CARTESIAN_POINT ( 'NONE',  ( -1.040834085586084257E-14, -7.246166700194011767, -9.579665964935651701 ) ) ;
#87061 = CARTESIAN_POINT ( 'NONE',  ( 6.193377243344257543, 6.120028293523423812, -0.7998128361456281477 ) ) ;
#87063 = CARTESIAN_POINT ( 'NONE',  ( 1.499999999999990896, 3.775000000000021227, 1.214306433183764966E-14 ) ) ;
#87062 = CARTESIAN_POINT ( 'NONE',  ( 5.420966337283807945, 1.944620675078809757, 0.8088979906116978702 ) ) ;
#87064 = CARTESIAN_POINT ( 'NONE',  ( 5.969205681473694902, 1.824102622056431811, 0.9793482939001868504 ) ) ;
#87065 = CARTESIAN_POINT ( 'NONE',  ( -1.364683531250000748, 1.571875000341421691, 0.000000000000000000 ) ) ;
#87066 = CARTESIAN_POINT ( 'NONE',  ( 4.270900206319126369, -2.015198044118733822, -0.7823990653590962019 ) ) ;
#87068 = EDGE_CURVE ( 'NONE', #32739, #176773, #173859, .T. ) ;
#87067 = CARTESIAN_POINT ( 'NONE',  ( 4.740881522827352867, 1.933304458870839238, 0.5843455605825734755 ) ) ;
#87069 = EDGE_CURVE ( 'NONE', #71735, #21539, #167775, .T. ) ;
#87072 = CARTESIAN_POINT ( 'NONE',  ( 6.155038550924155416, 6.283225852274053835, 0.7216878364870317197 ) ) ;
#87071 = CARTESIAN_POINT ( 'NONE',  ( 1.001543065824772753E-15, -3.171874999522042327, 3.793834371823811669 ) ) ;
#87070 = CARTESIAN_POINT ( 'NONE',  ( -2.324088772396477673E-16, 1.562500000000000666, 1.224999999999980549 ) ) ;
#87073 = CARTESIAN_POINT ( 'NONE',  ( -6.466312919074983512, 6.508729591867735031, -0.7998128361456362523 ) ) ;
#87074 = CARTESIAN_POINT ( 'NONE',  ( 2.044158018538293042, 0.8666093899718421145, 1.820985203412978093 ) ) ;
#87075 = CARTESIAN_POINT ( 'NONE',  ( -8.317037166979361018, 11.79062823052953668, 1.199719254218453823 ) ) ;
#87077 = CARTESIAN_POINT ( 'NONE',  ( -1.123270288250315163, 3.047697346350006331, -0.7749999999993613109 ) ) ;
#87076 = CARTESIAN_POINT ( 'NONE',  ( -3.846762897975357198, 5.510976019103107859, -1.599625672291256295 ) ) ;
#87078 = CARTESIAN_POINT ( 'NONE',  ( 3.834746474454188013E-15, 12.56250000000000178, 1.500000000000001554 ) ) ;
#87079 = CARTESIAN_POINT ( 'NONE',  ( -11.86145016429273191, 11.00587876334730453, 1.099999999999996758 ) ) ;
#87080 = CARTESIAN_POINT ( 'NONE',  ( -10.89183333199790304, 4.909323612238608803, -5.036858318171157478 ) ) ;
#87082 = CARTESIAN_POINT ( 'NONE',  ( 4.552361342037492875, -1.314984614574012944, 1.528753174698034067 ) ) ;
#87081 = CARTESIAN_POINT ( 'NONE',  ( -7.605760987142072160, 10.85684300409898384, 1.082531754730549967 ) ) ;
#87083 = CARTESIAN_POINT ( 'NONE',  ( 1.499999999999989120, 5.254166666666684193, 0.8660254037844524744 ) ) ;
#87084 = CARTESIAN_POINT ( 'NONE',  ( 1.364683531249996529, 14.77604166700806410, 0.7879004041258405033 ) ) ;
#87085 = CARTESIAN_POINT ( 'NONE',  ( 6.821331452548096586, -0.1252896706360993595, 1.696280295671446448 ) ) ;
#87086 = CARTESIAN_POINT ( 'NONE',  ( 6.547661840756936691, 6.603636667163397256, 0.7998128361456352531 ) ) ;
#87088 = CARTESIAN_POINT ( 'NONE',  ( 7.075376061485196821, 9.347967719856493218, 1.599625672291268286 ) ) ;
#87087 = CARTESIAN_POINT ( 'NONE',  ( 7.782016984564049444, 11.06247500109133064, 1.082531754730557072 ) ) ;
#87089 = CARTESIAN_POINT ( 'NONE',  ( -11.40611951520848955, 7.885036337628656078, 3.737597762133503920 ) ) ;
#87090 = CARTESIAN_POINT ( 'NONE',  ( 5.325416506339426981, -1.776575524504429016, 0.5857008802128694791 ) ) ;
#87091 = CARTESIAN_POINT ( 'NONE',  ( 0.2232913631893228001, 1.752491241892171647, 0.9904617665423065542 ) ) ;
#87092 = CYLINDRICAL_SURFACE ( 'NONE', #92084, 0.07999999999999993228 ) ;
#87093 = CIRCLE ( 'NONE', #173713, 0.08000000000000019595 ) ;
#87094 = FACE_OUTER_BOUND ( 'NONE', #90649, .T. ) ;
#87095 = ORIENTED_EDGE ( 'NONE', *, *, #98624, .F. ) ;
#87096 = CARTESIAN_POINT ( 'NONE',  ( 0.9136856707930467447, -1.281379520587552889, -1.556895127150646374 ) ) ;
#87097 = CARTESIAN_POINT ( 'NONE',  ( 0.9842725786804270571, -1.148342222048874595, 1.401147620581437048 ) ) ;
#87098 = CARTESIAN_POINT ( 'NONE',  ( 4.868786560638889149, 6.773613302202437403, 1.443375672974065660 ) ) ;
#87099 = DIRECTION ( 'NONE',  ( 0.000000000000000000, -1.000000000000000000, 0.000000000000000000 ) ) ;
#87100 = CARTESIAN_POINT ( 'NONE',  ( 7.253248993186720561, 10.44557901115111065, 1.082531754730558626 ) ) ;
#87101 = CARTESIAN_POINT ( 'NONE',  ( 8.125414133291656071, 8.374071331795406081, -0.7998128361456291469 ) ) ;
#87103 = CARTESIAN_POINT ( 'NONE',  ( 5.923430108280006934, -1.391030039757386039, -1.317302766908773126 ) ) ;
#87102 = CARTESIAN_POINT ( 'NONE',  ( -4.934277840369690971, 7.844075682818238526, -1.199719254218452047 ) ) ;
#87104 = DIRECTION ( 'NONE',  ( 0.000000000000000000, -1.000000000000000000, 0.000000000000000000 ) ) ;
#87105 = DIRECTION ( 'NONE',  ( 0.000000000000000000, 0.000000000000000000, -1.000000000000000000 ) ) ;
#87106 =( BOUNDED_CURVE ( )  B_SPLINE_CURVE ( 2, ( #198985, #136167, #166519, #19186, #168647, #201125, #85261, #86336, #119974 ),
 .UNSPECIFIED., .F., .T. ) 
 B_SPLINE_CURVE_WITH_KNOTS ( ( 3, 2, 2, 2, 3 ),
 ( 0.4791666666666666852, 0.4861111111111111049, 0.5000000000000000000, 0.5138888888888888395, 0.5208333333333333703 ),
 .UNSPECIFIED. ) 
 CURVE ( )  GEOMETRIC_REPRESENTATION_ITEM ( )  RATIONAL_B_SPLINE_CURVE ( ( 0.9330127018922194093, 0.9330127018922196314, 1.000000000000000000, 0.8660254037844387076, 1.000000000000000000, 0.8660254037844387076, 1.000000000000000000, 0.9330127018922187432, 0.9330127018922192983 ) ) 
 REPRESENTATION_ITEM ( '' )  );
#87107 = CARTESIAN_POINT ( 'NONE',  ( -10.99620347397582876, -6.863457517656843088, 0.2978015046999314408 ) ) ;
#87109 = ORIENTED_EDGE ( 'NONE', *, *, #77660, .T. ) ;
#87108 = FACE_OUTER_BOUND ( 'NONE', #167978, .T. ) ;
#87110 = CARTESIAN_POINT ( 'NONE',  ( -3.110706179331648169, 5.716575411607132118, 1.199719254218462483 ) ) ;
#87111 = CARTESIAN_POINT ( 'NONE',  ( 3.168983506954273999, -1.996715753333128118, -0.8287754370841573515 ) ) ;
#87112 = CARTESIAN_POINT ( 'NONE',  ( -7.756673280794142755, 8.222076047114187602, -0.7216878364870338292 ) ) ;
#87113 = CARTESIAN_POINT ( 'NONE',  ( 5.234856708652215751, 9.121433570154021453, 0.7216878364870317197 ) ) ;
#87114 = CARTESIAN_POINT ( 'NONE',  ( 0.9496594531581278309, -1.914679731917130479, 0.9119059213342149972 ) ) ;
#87115 = CARTESIAN_POINT ( 'NONE',  ( 5.842758758449526191, 0.3585452818064547853, 1.789846783968067845 ) ) ;
#87116 = CARTESIAN_POINT ( 'NONE',  ( 1.915242260480106706, -0.2453889982298693984, 1.955985308386765542 ) ) ;
#87117 = CARTESIAN_POINT ( 'NONE',  ( 4.254103502353132171, 0.8128351696983120434, -1.731171583500931366 ) ) ;
#87118 = ORIENTED_EDGE ( 'NONE', *, *, #159948, .T. ) ;
#87119 = LINE ( 'NONE', #4762, #173911 ) ;
#87121 = EDGE_CURVE ( 'NONE', #137371, #44957, #141724, .T. ) ;
#87120 = CARTESIAN_POINT ( 'NONE',  ( 6.285607346219458158, -1.855037422363578381, 0.6622139934589140742 ) ) ;
#87122 = CARTESIAN_POINT ( 'NONE',  ( 0.1111347575282967681, -1.904682588250571573, 0.3777756254830581528 ) ) ;
#87123 = ORIENTED_EDGE ( 'NONE', *, *, #74132, .T. ) ;
#87124 = CARTESIAN_POINT ( 'NONE',  ( -3.474632506852224356, 7.275764701294714420, -0.7998128361456481317 ) ) ;
#87126 = CARTESIAN_POINT ( 'NONE',  ( -0.4170821662629227156, 3.033599471985643170, 0.4170821662629036752 ) ) ;
#87125 = CARTESIAN_POINT ( 'NONE',  ( -6.943184063974175757, 9.193743722760251202, -1.443375672974066548 ) ) ;
#87128 = CARTESIAN_POINT ( 'NONE',  ( 4.868786560638878491, 8.694351730805124134, 0.7216878364870317197 ) ) ;
#87127 = CARTESIAN_POINT ( 'NONE',  ( 8.782984583554449998, 9.141236857102018831, 1.040834085586084257E-14 ) ) ;
#87130 = ORIENTED_EDGE ( 'NONE', *, *, #50115, .F. ) ;
#87129 = CARTESIAN_POINT ( 'NONE',  ( 5.268181577278353345, 1.909906527651853425, -0.09793718704654422180 ) ) ;
#87131 = CARTESIAN_POINT ( 'NONE',  ( 0.3060867131535296992, -0.5861141839358529060, 2.127432003918772629 ) ) ;
#87132 = VECTOR ( 'NONE', #18358, 1000.000000000000114 ) ;
#87133 = CARTESIAN_POINT ( 'NONE',  ( -5.623259694695312838, 5.814328530587530075, 0.3973859538428151650 ) ) ;
#87134 = CARTESIAN_POINT ( 'NONE',  ( -0.1108833634136767443, 0.0002062650063822807356, -1.896853557917008271 ) ) ;
#87135 = CARTESIAN_POINT ( 'NONE',  ( -0.7500000000000006661, 8.708333333333332149, -1.299038105676657340 ) ) ;
#87136 = CARTESIAN_POINT ( 'NONE',  ( -4.918597572616692837, 8.113217865663214567, 1.086842401077245279 ) ) ;
#87137 = CARTESIAN_POINT ( 'NONE',  ( -6.634380621478864093, -6.684699875907221589, -6.783773251375836644 ) ) ;
#87138 = CARTESIAN_POINT ( 'NONE',  ( 2.594261239525695206, 0.9781076984213372683, -1.824767828009652204 ) ) ;
#87139 = CARTESIAN_POINT ( 'NONE',  ( -4.843287188579803448, 6.673587691474970107, -1.599625672291256295 ) ) ;
#87140 = CARTESIAN_POINT ( 'NONE',  ( -4.693116838625758014, 8.272874032808440248, 0.5769273507626712094 ) ) ;
#87142 = CARTESIAN_POINT ( 'NONE',  ( 0.2335756976950612018, -1.975703151049061024, 0.8776370805363906680 ) ) ;
#87141 = CARTESIAN_POINT ( 'NONE',  ( -4.603156847039612920, 5.329103395422994716, 1.199719254218462483 ) ) ;
#87143 = CARTESIAN_POINT ( 'NONE',  ( -11.81293272228161229, 8.718537709414365011, -2.131821593364598755 ) ) ;
#87144 = LINE ( 'NONE', #90363, #158278 ) ;
#87145 = CARTESIAN_POINT ( 'NONE',  ( -0.6823417656250039265, 13.38020833367473195, -1.181850606188755259 ) ) ;
#87147 = CARTESIAN_POINT ( 'NONE',  ( -5.306037014901836990, 7.283738832175834510, 1.599625672291263179 ) ) ;
#87146 = CARTESIAN_POINT ( 'NONE',  ( 6.825078400183553384, 0.5907600490881077526, 1.908621492364571903 ) ) ;
#87148 = CARTESIAN_POINT ( 'NONE',  ( 5.836466137708809399, 0.4949425091341461136, -1.662031903658898413 ) ) ;
#87149 = TOROIDAL_SURFACE ( 'NONE', #128691, 12.18000000000000149, 0.5000000000000008882 ) ;
#87150 = CARTESIAN_POINT ( 'NONE',  ( -4.451154503988200339, 4.087435097607984957, 1.214306433183764966E-14 ) ) ;
#87151 = CARTESIAN_POINT ( 'NONE',  ( 3.537997267176114846, 1.309675639058418550, 1.603382541711120268 ) ) ;
#87152 = CARTESIAN_POINT ( 'NONE',  ( 4.851218673320928154, 0.2063579389092398131, -2.107127644889031703 ) ) ;
#87153 = CARTESIAN_POINT ( 'NONE',  ( 7.800018446563675489, 7.994443030612759848, -0.7998128361456281477 ) ) ;
#87154 = CARTESIAN_POINT ( 'NONE',  ( 1.364683531249988535, 4.405208333674754506, -0.7879004041258300672 ) ) ;
#87155 = CARTESIAN_POINT ( 'NONE',  ( 2.448051270322794348, -0.8465065455745772738, 1.778409512993859076 ) ) ;
#87156 = CARTESIAN_POINT ( 'NONE',  ( 1.230557176020010912, 1.282188879665364656, -1.419081615486268433 ) ) ;
#87157 = CARTESIAN_POINT ( 'NONE',  ( 4.470831859796895458, 0.002540009476469616122, -2.292435214262526166 ) ) ;
#87158 = CARTESIAN_POINT ( 'NONE',  ( 2.156629195875509719, -1.411784796728832170, 1.157573153174975111 ) ) ;
#87159 = CARTESIAN_POINT ( 'NONE',  ( 5.890091390494168522, 5.836471141856793388, 0.000000000000000000 ) ) ;
#87160 = CARTESIAN_POINT ( 'NONE',  ( 6.616015773344440021, 6.821032611764393572, 1.040834085586084257E-14 ) ) ;
#87161 = CARTESIAN_POINT ( 'NONE',  ( -8.179646747746328828, 8.437342715325849341, -0.7998128361456291469 ) ) ;
#87162 = EDGE_CURVE ( 'NONE', #68014, #120459, #79902, .T. ) ;
#87163 = CARTESIAN_POINT ( 'NONE',  ( 3.885024706246028803, -1.880017414580990032, -0.7205730073996403640 ) ) ;
#87164 = CARTESIAN_POINT ( 'NONE',  ( 3.467582345443523728, -0.3871886708083654427, 1.922995549214156608 ) ) ;
#87165 = CARTESIAN_POINT ( 'NONE',  ( -8.355902744723985975, 8.642974711799791265, 1.040834085586084257E-14 ) ) ;
#87166 = CARTESIAN_POINT ( 'NONE',  ( -4.238895582566952314, 8.097128612970093897, 1.040834085586084257E-14 ) ) ;
#87167 = FACE_OUTER_BOUND ( 'NONE', #31605, .T. ) ;
#87170 = B_SPLINE_CURVE_WITH_KNOTS ( 'NONE', 3,
 ( #61844, #119173, #102867, #34658, #99668, #184101, #86611, #100728, #199277, #83405, #152678, #50919, #149487, #4261 ),
 .UNSPECIFIED., .F., .F.,
 ( 4, 2, 2, 2, 2, 2, 4 ),
 ( 6.159050845712786192E-06, 0.0002195312228448280628, 0.0004329033948439433470, 0.0008596477388421738071, 0.001073019910841287736, 0.001286392082840398954, 0.001713136426838625295 ),
 .UNSPECIFIED. ) ;
#87169 = CARTESIAN_POINT ( 'NONE',  ( 4.100303288188038131, -0.5556836211836749806, -1.680424235071773742 ) ) ;
#87168 = CARTESIAN_POINT ( 'NONE',  ( 6.580031098407260082, -2.049997751086956921, -0.4092652541880793526 ) ) ;
#87171 = CARTESIAN_POINT ( 'NONE',  ( -2.679285714285713826, 0.4970443252110354759, -0.09999999999999592548 ) ) ;
#87172 = CARTESIAN_POINT ( 'NONE',  ( 0.7971425760184660536, 1.793611693402120455, 1.258865353619270433 ) ) ;
#87173 = CARTESIAN_POINT ( 'NONE',  ( -0.006821830062568761018, -1.739981233400577088, -0.04623622425214619219 ) ) ;
#87175 = EDGE_CURVE ( 'NONE', #114100, #151754, #76229, .T. ) ;
#87174 = VECTOR ( 'NONE', #72395, 1000.000000000000000 ) ;
#87176 = CARTESIAN_POINT ( 'NONE',  ( 7.450369105909416589, 8.650851030771185890, -1.199719254218441611 ) ) ;
#87177 = CARTESIAN_POINT ( 'NONE',  ( 0.1331715793776418189, 1.377430125279802686, -2.211494238769554865 ) ) ;
#87178 = CARTESIAN_POINT ( 'NONE',  ( 0.8964060800229460835, 0.1715710081350088068, 2.292006659179766537 ) ) ;
#87179 = CARTESIAN_POINT ( 'NONE',  ( 0.4334776158547505864, -1.553986563932317377, -1.545601477622601472 ) ) ;
#87180 = CARTESIAN_POINT ( 'NONE',  ( 6.538463365017005202, 1.657764536579940495, -0.5080105315169358704 ) ) ;
#87181 = CARTESIAN_POINT ( 'NONE',  ( 3.141465813989018141, -1.946189201368169641, 1.040519825639886431 ) ) ;
#87182 =( BOUNDED_SURFACE ( )  B_SPLINE_SURFACE ( 3, 2, ( 
 ( #91876, #111364, #194667 ),
 ( #193605, #174192, #192525 ),
 ( #44179, #157932, #173114 ),
 ( #144902, #94007, #90798 ),
 ( #8448, #127640, #11650 ),
 ( #177369, #75597, #24695 ) ),
 .UNSPECIFIED., .F., .F., .F. ) 
 B_SPLINE_SURFACE_WITH_KNOTS ( ( 4, 2, 4 ),
 ( 3, 3 ),
 ( -4.336808689942017736E-19, 0.0003831416164015013842, 0.0007662832328030032020 ),
 ( 0.000000000000000000, 1.000000000000000000 ),
 .UNSPECIFIED. ) 
 GEOMETRIC_REPRESENTATION_ITEM ( )  RATIONAL_B_SPLINE_SURFACE ( (
 ( 1.000000000000000000, 0.7071067811865475727, 1.000000000000000000),
 ( 1.000000000000000000, 0.6829713513657061918, 1.000000000000000000),
 ( 1.000000000000000000, 0.6534833722367423547, 1.000000000000000000),
 ( 1.000000000000000000, 0.6054027484667425796, 1.000000000000000000),
 ( 1.000000000000000000, 0.5875453974411385394, 1.000000000000000000),
 ( 1.000000000000000000, 0.5879095031487528988, 1.000000000000000000) ) ) 
 REPRESENTATION_ITEM ( '' )  SURFACE ( )  );
#87183 = CARTESIAN_POINT ( 'NONE',  ( 0.4093307213487142326, -1.744552795675001100, 1.292164652415381365 ) ) ;
#87184 = DIRECTION ( 'NONE',  ( 0.000000000000000000, 0.000000000000000000, 1.000000000000000000 ) ) ;
#87185 = CARTESIAN_POINT ( 'NONE',  ( 1.640021805331920213, 2.111262888970814267, -0.1616085204505824935 ) ) ;
#87186 = CARTESIAN_POINT ( 'NONE',  ( 3.406250000000002220, 1.895863743164009740, -0.7852924748301655100 ) ) ;
#87187 = CARTESIAN_POINT ( 'NONE',  ( 6.727182134110203826, 2.399899341769623273, 2.668786705202597531 ) ) ;
#87188 = CARTESIAN_POINT ( 'NONE',  ( 5.526370178063710448, 1.147270165450631207, -1.547347761420419188 ) ) ;
#87189 = ORIENTED_EDGE ( 'NONE', *, *, #22632, .F. ) ;
#87191 = CARTESIAN_POINT ( 'NONE',  ( 1.499999999999989120, 5.254166666666684193, 0.8660254037844524744 ) ) ;
#87190 = CARTESIAN_POINT ( 'NONE',  ( 1.576131469712481303, -1.221787821332357860, 1.939473486982680628 ) ) ;
#87192 = CARTESIAN_POINT ( 'NONE',  ( 3.659811400685081040, 6.357198169852855685, -1.199719254218446718 ) ) ;
#87193 = CARTESIAN_POINT ( 'NONE',  ( 6.169123589417988995, 7.156064594864501416, -1.199719254218445830 ) ) ;
#87194 = EDGE_CURVE ( 'NONE', #40528, #171576, #116010, .T. ) ;
#87195 = CARTESIAN_POINT ( 'NONE',  ( 3.457896741714714395, -1.683011943829109791, -1.449823692882054482 ) ) ;
#87196 = CARTESIAN_POINT ( 'NONE',  ( -9.002250809794013264, 9.604973487622245898, -0.7216878364870267237 ) ) ;
#87197 = CARTESIAN_POINT ( 'NONE',  ( -3.946537740501743219, 2.817530495241825417, -0.7749999999999944711 ) ) ;
#87198 = CARTESIAN_POINT ( 'NONE',  ( 5.178851490740193242, 8.025448591630130579, 1.082531754730558626 ) ) ;
#87199 = CARTESIAN_POINT ( 'NONE',  ( -7.605760987142072160, 10.85684300409898384, 1.082531754730549967 ) ) ;
#87200 = CARTESIAN_POINT ( 'NONE',  ( 5.885648082108190238, 7.959951743916638733, 1.443375672974065660 ) ) ;
#87201 = CARTESIAN_POINT ( 'NONE',  ( 1.811172873341511336, 1.158687402475454098, -1.650082692374904125 ) ) ;
#87203 = CARTESIAN_POINT ( 'NONE',  ( 0.2392226684038156193, -0.1392734953599965297, -2.030321344557210139 ) ) ;
#87202 = CARTESIAN_POINT ( 'NONE',  ( 9.101601193475611140, 9.512956235343358102, -0.7998128361456221525 ) ) ;
#87204 = PLANE ( 'NONE',  #182270 ) ;
#87205 = CARTESIAN_POINT ( 'NONE',  ( 5.438229012412886476, 7.437962829272074750, -1.443375672974078761 ) ) ;
#87206 = CARTESIAN_POINT ( 'NONE',  ( 6.233937787808796038, 1.722893207988238862, 0.2456954999437432341 ) ) ;
#87207 =( NAMED_UNIT ( * ) PLANE_ANGLE_UNIT ( ) SI_UNIT ( $, .RADIAN. ) );
#87208 = CARTESIAN_POINT ( 'NONE',  ( 0.6823417656249882723, 2.176041667008084435, -1.181850606188749264 ) ) ;
#87209 = CARTESIAN_POINT ( 'NONE',  ( 0.8425835904034431056, -1.521979116790536768, 0.9028166612478020214 ) ) ;
#87210 = CARTESIAN_POINT ( 'NONE',  ( 1.283827520628720187, 1.646837967535810021, -1.163270716046126196 ) ) ;
#87211 = CARTESIAN_POINT ( 'NONE',  ( 0.06366010765614799061, -1.203631707120488947, 1.393476991864414760 ) ) ;
#87212 = CARTESIAN_POINT ( 'NONE',  ( 5.319995955860258974, 1.367515572929053791, -1.839686415443070100 ) ) ;
#87213 = CARTESIAN_POINT ( 'NONE',  ( 3.697050842446505392, -0.5329721798031424873, 1.762307204009383454 ) ) ;
#87214 = CARTESIAN_POINT ( 'NONE',  ( 8.959240580532112475, 9.346868853575953651, -0.7998128361456221525 ) ) ;
#87216 = EDGE_CURVE ( 'NONE', #42660, #168515, #209885, .T. ) ;
#87215 = CARTESIAN_POINT ( 'NONE',  ( 6.928203230275525648, 15.00000000000000000, -9.797958971132702644 ) ) ;
#87217 = CARTESIAN_POINT ( 'NONE',  ( 4.137589658204786858, -1.258905094989383189, -1.322318538811013688 ) ) ;
#87218 = CARTESIAN_POINT ( 'NONE',  ( 4.975232503164924935, -2.001511053420693020, -0.2440319332882301961 ) ) ;
#87219 = CARTESIAN_POINT ( 'NONE',  ( -7.004758919754800139, 11.32396917302262018, 0.000000000000000000 ) ) ;
#87221 = CARTESIAN_POINT ( 'NONE',  ( -6.851666526859749418, 9.086973262793417661, -1.599625672291271394 ) ) ;
#87220 = CARTESIAN_POINT ( 'NONE',  ( 4.012777769421401963, 1.602246665114055002, -1.597678914196493771 ) ) ;
#87222 = CARTESIAN_POINT ( 'NONE',  ( 6.176810970088661534, -1.998525488361714508, -0.6642400113570454678 ) ) ;
#87223 = CARTESIAN_POINT ( 'NONE',  ( -0.4465194593918104249, 3.080450244942127380, 0.4155024747329021939 ) ) ;
#87224 = CARTESIAN_POINT ( 'NONE',  ( 3.262232429473245432, -2.068111870375147987, 0.09887451149894616043 ) ) ;
#87225 = CARTESIAN_POINT ( 'NONE',  ( 3.216308754939877446, 4.775446185561722956, -1.599625672291262513 ) ) ;
#87226 = CARTESIAN_POINT ( 'NONE',  ( 1.360316468749964480, 2.046875000341397133, -4.857225732735059864E-14 ) ) ;
#87227 = CARTESIAN_POINT ( 'NONE',  ( 6.147156607449644206, 0.2074554230099104890, 2.110329589018632657 ) ) ;
#87228 = SHAPE_DEFINITION_REPRESENTATION ( #90285, #113740 ) ;
#87230 = CARTESIAN_POINT ( 'NONE',  ( 1.646969920108354524, -1.627708819445686572, 1.030247865989121880 ) ) ;
#87229 = CARTESIAN_POINT ( 'NONE',  ( -8.585337585951595685, 11.03931315507545108, -1.599625672291263179 ) ) ;
#87231 = CARTESIAN_POINT ( 'NONE',  ( -2.979759899953417612, 6.698413326579433225, 0.7998128361456352531 ) ) ;
#87232 = CARTESIAN_POINT ( 'NONE',  ( 6.526221542235329132, 1.009325857860805087, 1.690966299934024031 ) ) ;
#87233 = CARTESIAN_POINT ( 'NONE',  ( 4.136646265500957043, 5.919449624541475607, -1.443375672974068769 ) ) ;
#87234 = CARTESIAN_POINT ( 'NONE',  ( 5.580611138136594818, 6.171711880978127063, 0.8815597724760818599 ) ) ;
#87235 = DIRECTION ( 'NONE',  ( 0.3162277660168373861, -0.9486832980505139901, 0.000000000000000000 ) ) ;
#87236 = CARTESIAN_POINT ( 'NONE',  ( -3.581325132304157943, 7.329963087663487364, -0.7998128361456281477 ) ) ;
#87237 = CARTESIAN_POINT ( 'NONE',  ( 0.07096481000732741962, 0.8580841460674984988, 2.049194762706497031 ) ) ;
#87238 = CARTESIAN_POINT ( 'NONE',  ( 3.100711275163593239, -0.6099987009138232441, -2.015686496682663087 ) ) ;
#87239 = CARTESIAN_POINT ( 'NONE',  ( -5.354544322754380303, 5.211666229493680191, 0.7998128361456281477 ) ) ;
#87240 = CARTESIAN_POINT ( 'NONE',  ( 5.913327553854682783, 10.05063257947248800, -0.7998128361456291469 ) ) ;
#87241 = CARTESIAN_POINT ( 'NONE',  ( 0.8888279104573212352, 0.1313983060258062385, 1.856467483602406432 ) ) ;
#87242 = CARTESIAN_POINT ( 'NONE',  ( 6.100279051144945619, 9.204410428722734849, -1.199719254218440723 ) ) ;
#87243 = CARTESIAN_POINT ( 'NONE',  ( 3.635557746758808495, 7.393234471193928847, -0.7998128361456291469 ) ) ;
#87244 = CARTESIAN_POINT ( 'NONE',  ( -7.268579750702168774, 7.652633595340216921, -0.7216878364870338292 ) ) ;
#87245 = CARTESIAN_POINT ( 'NONE',  ( -7.782016984564068096, 10.10210578678999482, 1.443375672974090751 ) ) ;
#87246 = TOROIDAL_SURFACE ( 'NONE', #201466, 9.580000000000001847, 0.08000000000000000167 ) ;
#87247 = CARTESIAN_POINT ( 'NONE',  ( 0.7562902151678205787, 0.8540304730459827853, -1.941197329821432227 ) ) ;
#87248 = CARTESIAN_POINT ( 'NONE',  ( -7.598418745816086783, 7.829519723065708092, 0.000000000000000000 ) ) ;
#87250 = CARTESIAN_POINT ( 'NONE',  ( 5.002378505967388200, 1.956489882415031190, 0.1462272935644214900 ) ) ;
#87249 = CARTESIAN_POINT ( 'NONE',  ( 1.224999999999995204, 1.125000000000000888, -2.949029909160572061E-14 ) ) ;
#87251 = CARTESIAN_POINT ( 'NONE',  ( 2.430746436576446179, 2.096607243605509208, 0.5259719050795114148 ) ) ;
#87252 = CARTESIAN_POINT ( 'NONE',  ( 1.645803748337611783, 0.5784278848013635344, 1.748079663633335334 ) ) ;
#87253 = CIRCLE ( 'NONE', #149559, 2.725000000000000089 ) ;
#87255 = CARTESIAN_POINT ( 'NONE',  ( -4.485938484121875902, 7.064193607440066636, -1.134896524841392473 ) ) ;
#87254 = CARTESIAN_POINT ( 'NONE',  ( 0.01167607004786809163, -5.765528217051462789, -11.00020965659732930 ) ) ;
#87256 = CARTESIAN_POINT ( 'NONE',  ( 3.556370828957751140, -1.535720284108733624, -0.8187001993567950553 ) ) ;
#87257 = CARTESIAN_POINT ( 'NONE',  ( 4.004543651933685666, 7.806729363262467913, 0.1824581366321497422 ) ) ;
#87258 = CARTESIAN_POINT ( 'NONE',  ( 6.317736394288147039, 6.473040002865377396, 0.7216878364870317197 ) ) ;
#87259 = CARTESIAN_POINT ( 'NONE',  ( -10.37105062950515943, 6.927298630606520291, 5.133691221222295376 ) ) ;
#87260 = CARTESIAN_POINT ( 'NONE',  ( 0.2159880523044250267, -2.119658899406823505, 0.4233941889316418239 ) ) ;
#87261 = CARTESIAN_POINT ( 'NONE',  ( 3.936874915731437774, 1.117662071392529377, 1.677747830363854664 ) ) ;
#87262 = CARTESIAN_POINT ( 'NONE',  ( 0.000000000000000000, -0.02379966007286238305, -6.277139874739035896 ) ) ;
#87263 = CARTESIAN_POINT ( 'NONE',  ( 0.4972265960483426284, 1.796464302094663346, -1.202062886709959422 ) ) ;
#87264 = CARTESIAN_POINT ( 'NONE',  ( 3.450034532000289200, 1.971640592831106709, 0.001386944525654659321 ) ) ;
#87265 = CARTESIAN_POINT ( 'NONE',  ( 6.609000000000005315, 2.959011640422835487, 2.552823073452652913 ) ) ;
#87266 = CARTESIAN_POINT ( 'NONE',  ( 2.085399755688497336, -0.8285669363069894100, 1.756555673176816157 ) ) ;
#87269 = ORIENTED_EDGE ( 'NONE', *, *, #35714, .F. ) ;
#87268 = CARTESIAN_POINT ( 'NONE',  ( -5.980555157403903976, 6.149938236492225485, 0.000000000000000000 ) ) ;
#87267 = FACE_OUTER_BOUND ( 'NONE', #136710, .T. ) ;
#87270 = CARTESIAN_POINT ( 'NONE',  ( -4.570507181138272479, 7.385989907086349504, 1.082531754730549967 ) ) ;
#87271 = CARTESIAN_POINT ( 'NONE',  ( 3.901714345682657292, 7.774026846596938434, 0.7998128361456271485 ) ) ;
#87272 = CARTESIAN_POINT ( 'NONE',  ( -5.764151584465413869, 6.753873599078290546, -1.199719254218453823 ) ) ;
#87273 = CARTESIAN_POINT ( 'NONE',  ( -5.607179047703544583, 8.699403434699558346, 1.199719254218454489 ) ) ;
#87274 = CARTESIAN_POINT ( 'NONE',  ( -10.58855478214856660, 11.45566145536924552, -0.7216878364870217277 ) ) ;
#87275 = CARTESIAN_POINT ( 'NONE',  ( 6.528381088282158906, 1.336169653064466889, -1.881230508112927025 ) ) ;
#87277 = EDGE_CURVE ( 'NONE', #35460, #23166, #93520, .T. ) ;
#87276 = CARTESIAN_POINT ( 'NONE',  ( 6.742638286788313451, -1.923764577213080029, -0.3838556375530403630 ) ) ;
#87278 = CARTESIAN_POINT ( 'NONE',  ( 3.907043859180459933, -1.606318986283063799, 1.125903821926607318 ) ) ;
#87279 = CARTESIAN_POINT ( 'NONE',  ( 6.936968151686458306, 11.24487994360957188, 0.7998128361456462443 ) ) ;
#87280 = CARTESIAN_POINT ( 'NONE',  ( 1.652970434142877920, 1.038994816082598804, 1.728001345923817267 ) ) ;
#87281 = ORIENTED_EDGE ( 'NONE', *, *, #100563, .T. ) ;
#87282 = CARTESIAN_POINT ( 'NONE',  ( 2.782529222840863348, -0.6191273052778034636, -2.024769726974411377 ) ) ;
#87283 = CARTESIAN_POINT ( 'NONE',  ( -1.402160292154681736E-14, 1.868750000682816381, -1.732050807568863648 ) ) ;
#87285 = CARTESIAN_POINT ( 'NONE',  ( -4.557512192488103686, 8.468847991211438497, -0.7998128361456281477 ) ) ;
#87284 = CARTESIAN_POINT ( 'NONE',  ( -2.676845263694313637, 5.210404343363602919, -1.199719254218446718 ) ) ;
#87286 = CARTESIAN_POINT ( 'NONE',  ( 3.292734131499192252, 1.452021927685825275, 1.131891246899892289 ) ) ;
#87287 = ORIENTED_EDGE ( 'NONE', *, *, #86771, .F. ) ;
#87288 = CARTESIAN_POINT ( 'NONE',  ( -9.969323024750229578, 10.52529837183042716, -0.7998128361456291469 ) ) ;
#87289 = CARTESIAN_POINT ( 'NONE',  ( 0.3728825314828132509, 3.227879828479781388, 0.5317689764002214714 ) ) ;
#87290 = CARTESIAN_POINT ( 'NONE',  ( 4.236665939827915395, 1.302216991916404387, -1.673619383358643908 ) ) ;
#87291 = CARTESIAN_POINT ( 'NONE',  ( -9.994890815243229198, 3.870538056096196833, -5.945519334325427785 ) ) ;
#87292 = CARTESIAN_POINT ( 'NONE',  ( 6.938021921891177612, 9.117444880338284818, -1.599625672291262513 ) ) ;
#87293 = CARTESIAN_POINT ( 'NONE',  ( 5.272755944101470860, -1.938957023840400362, -0.6983732565980956819 ) ) ;
#87295 = CARTESIAN_POINT ( 'NONE',  ( 2.999365392321148516, -1.839032331094083927, 0.09308366406014097205 ) ) ;
#87294 = CARTESIAN_POINT ( 'NONE',  ( -6.418895661066105873, 9.576129806964074120, -1.199719254218440723 ) ) ;
#87296 = CARTESIAN_POINT ( 'NONE',  ( 9.206149998879153529, 10.69926207256923689, 1.199719254218453823 ) ) ;
#87297 = CARTESIAN_POINT ( 'NONE',  ( -1.201851678989727383E-14, 5.446875000341422357, -1.575800808251660134 ) ) ;
#87298 = CARTESIAN_POINT ( 'NONE',  ( 0.000000000000000000, 5.999999999999998224, 0.000000000000000000 ) ) ;
#87299 = CARTESIAN_POINT ( 'NONE',  ( -0.4652293495373896470, 7.465077128757534375, 4.424517295598821676 ) ) ;
#87300 = CARTESIAN_POINT ( 'NONE',  ( 0.09999999999999592548, -9.900000000000005684, 6.938893903907228378E-15 ) ) ;
#87301 = CARTESIAN_POINT ( 'NONE',  ( 2.245003380770736801, 0.4850519687749441644, 2.152760086278446394 ) ) ;
#87302 = CARTESIAN_POINT ( 'NONE',  ( 3.778848203065594102, -2.179170165155080774, -0.6077416658978853636 ) ) ;
#87303 = CARTESIAN_POINT ( 'NONE',  ( -5.910991785878158211, 9.839981483592442402, -0.7216878364870278340 ) ) ;
#87304 = CARTESIAN_POINT ( 'NONE',  ( 3.832113882524991411, -0.9361971883012323303, -1.550792431135393334 ) ) ;
#87305 = CARTESIAN_POINT ( 'NONE',  ( 4.188635153834672664, 1.476993813991718918, -1.219978962091677221 ) ) ;
#87306 = CARTESIAN_POINT ( 'NONE',  ( 1.364683531249988535, 4.176041667008081326, 0.7879004041258500513 ) ) ;
#87307 = CARTESIAN_POINT ( 'NONE',  ( 3.977382581243666504, 1.856787152588537548, -0.6629638669850937971 ) ) ;
#87308 = CARTESIAN_POINT ( 'NONE',  ( 0.9735099972556484627, 1.857407184102148001, -0.5107058244425541904 ) ) ;
#87309 = CARTESIAN_POINT ( 'NONE',  ( 4.522238337509359773, 1.150754656758418593, -1.474723989322044959 ) ) ;
#87310 = CARTESIAN_POINT ( 'NONE',  ( 3.176728247877279365, -1.374524503021319344, 1.853549100471873823 ) ) ;
#87311 = CARTESIAN_POINT ( 'NONE',  ( 4.369486748645814878, -0.3193033414996570007, 1.833288415851072273 ) ) ;
#87312 = CARTESIAN_POINT ( 'NONE',  ( -1.364683531250010295, 5.738541667008088432, -0.7879004041258300672 ) ) ;
#87313 = AXIS2_PLACEMENT_3D ( 'NONE', #99549, #128934, #181840 ) ;
#87314 = CIRCLE ( 'NONE', #208358, 11.54340198673881979 ) ;
#87315 = CARTESIAN_POINT ( 'NONE',  ( 0.3918150239524306189, -2.006371095615328226, 0.2024682584410575914 ) ) ;
#87317 = CARTESIAN_POINT ( 'NONE',  ( 1.541775746491366395, -1.526411702840410722, -1.451317155924846336 ) ) ;
#87316 = CARTESIAN_POINT ( 'NONE',  ( -3.999292125906916073, 5.688926785023260102, 1.443375672974064550 ) ) ;
#87318 = CARTESIAN_POINT ( 'NONE',  ( 2.535011535630975477, 5.901337858304024131, 0.7216878364870438212 ) ) ;
#87319 = CARTESIAN_POINT ( 'NONE',  ( -8.292783513053063160, 12.82666453187061073, 0.7998128361456481317 ) ) ;
#87320 = CARTESIAN_POINT ( 'NONE',  ( 6.591117433763723277, 1.884315261875910474, -1.059023293578951863 ) ) ;
#87321 = CARTESIAN_POINT ( 'NONE',  ( 3.515986968957810266, -0.6120941298391362473, 2.030368431519948391 ) ) ;
#87322 = CARTESIAN_POINT ( 'NONE',  ( -9.620326184871647257, -9.190313392136378212, 0.3418113563954127132 ) ) ;
#87324 = EDGE_CURVE ( 'NONE', #16328, #131029, #174472, .T. ) ;
#87323 = CARTESIAN_POINT ( 'NONE',  ( 1.283469775389501910, 0.1441914389909859651, -2.014673257830889685 ) ) ;
#87325 = CARTESIAN_POINT ( 'NONE',  ( -1.364683531250014514, 0.7385416670080887647, -0.7879004041258289570 ) ) ;
#87326 = CARTESIAN_POINT ( 'NONE',  ( -2.168941388506379742, 5.474256019991960542, -0.7216878364870267237 ) ) ;
#87327 = CARTESIAN_POINT ( 'NONE',  ( 3.798255590122797898, 7.583048621785260401, -0.7998128361456221525 ) ) ;
#87328 = EDGE_LOOP ( 'NONE', ( #198472, #130908, #145681, #196524 ) ) ;
#87329 = CARTESIAN_POINT ( 'NONE',  ( 1.651884467337715989, 0.6291892518628816600, -2.067965918892029631 ) ) ;
#87330 = CARTESIAN_POINT ( 'NONE',  ( 6.609999999999971010, 7.629137130509032971, 2.319999999999996287 ) ) ;
#87333 = CARTESIAN_POINT ( 'NONE',  ( 3.768803514918948938, 4.459654191235965293, -1.082531754730543083 ) ) ;
#87332 = CARTESIAN_POINT ( 'NONE',  ( 5.939880696562888751, 7.062853913145737295, -1.082531754730548412 ) ) ;
#87331 = CARTESIAN_POINT ( 'NONE',  ( 5.387385936583818591, 7.378645907471495846, -1.599625672291283607 ) ) ;
#87334 = CARTESIAN_POINT ( 'NONE',  ( 0.09999999999999592548, -9.919999999999998153, 9.579478065113978147 ) ) ;
#87335 = CARTESIAN_POINT ( 'NONE',  ( 5.507046092540283766, -0.04465857163906890998, 2.016188657829049991 ) ) ;
#87336 = CARTESIAN_POINT ( 'NONE',  ( -8.853111120043687166, 9.430977182913531820, 1.040834085586084257E-14 ) ) ;
#87337 = EDGE_CURVE ( 'NONE', #4447, #167565, #8504, .T. ) ;
#87338 = CARTESIAN_POINT ( 'NONE',  ( 0.3280006606478855224, 1.121390616443746602, -1.882787531365101685 ) ) ;
#87339 = CARTESIAN_POINT ( 'NONE',  ( 1.286813488861813459, 4.086408449757453099, -0.5514626414212294714 ) ) ;
#87341 = CARTESIAN_POINT ( 'NONE',  ( -1.402160292154681736E-14, 12.67187500034139802, 1.575800808251682339 ) ) ;
#87340 = CARTESIAN_POINT ( 'NONE',  ( 6.807524309086420367, -0.4794501827766698421, 2.115671360755105646 ) ) ;
#87342 = CARTESIAN_POINT ( 'NONE',  ( -8.809047120577080392, 11.30030761213851953, 1.599625672291269396 ) ) ;
#87343 = CARTESIAN_POINT ( 'NONE',  ( 4.346888830327386266, -1.803415170841724979, -0.9023466997552240798 ) ) ;
#87344 = CARTESIAN_POINT ( 'NONE',  ( -5.707619481228822345, 7.681975366232176583, -1.443375672974051449 ) ) ;
#87345 = CARTESIAN_POINT ( 'NONE',  ( -1.201851678989727383E-14, 1.634375000341421025, 1.575800808251672791 ) ) ;
#87346 = CARTESIAN_POINT ( 'NONE',  ( 0.6124999999999741762, 2.729166667349444797, -1.060881119635955327 ) ) ;
#87347 = MECHANICAL_DESIGN_GEOMETRIC_PRESENTATION_REPRESENTATION (  '', ( #104674 ), #142739 ) ;
#87348 = CARTESIAN_POINT ( 'NONE',  ( -1.500000000000008216, 9.750000000000001776, 3.469446951953614189E-15 ) ) ;
#87349 = CARTESIAN_POINT ( 'NONE',  ( 3.650762458506318087, -1.408968171862119423, 0.9946885059901353632 ) ) ;
#87350 = CARTESIAN_POINT ( 'NONE',  ( 4.692003678781083487, 7.631698837623355658, -1.199719254218450271 ) ) ;
#87351 = CARTESIAN_POINT ( 'NONE',  ( 1.897346677678591442, -0.6019946308016431713, 1.664328231202655273 ) ) ;
#87352 = CARTESIAN_POINT ( 'NONE',  ( 9.561524646135536543, 12.17819805862340310, -1.599625672291262513 ) ) ;
#87353 = CARTESIAN_POINT ( 'NONE',  ( 5.456176519787153012, 2.204477245749701719, -0.1032804940204190558 ) ) ;
#87354 = ORIENTED_EDGE ( 'NONE', *, *, #1511, .F. ) ;
#87355 = CARTESIAN_POINT ( 'NONE',  ( 4.535418805095452477, -0.09482428102505417733, 2.017666594091566346 ) ) ;
#87356 = CARTESIAN_POINT ( 'NONE',  ( -7.286581212701773502, 7.465709267765667789, 0.7998128361456341429 ) ) ;
#87358 = CARTESIAN_POINT ( 'NONE',  ( 3.937125189161301719, -1.678018027730580286, -1.117815418662113203 ) ) ;
#87357 = CARTESIAN_POINT ( 'NONE',  ( 3.949941927655271190, -1.463281269271698770, -1.534908012577620440 ) ) ;
#87359 = ORIENTED_EDGE ( 'NONE', *, *, #120662, .T. ) ;
#87360 = CARTESIAN_POINT ( 'NONE',  ( 4.037295881819344956, 7.932205305423046582, -0.7998128361456362523 ) ) ;
#87361 = ORIENTED_EDGE ( 'NONE', *, *, #181468, .T. ) ;
#87362 = CARTESIAN_POINT ( 'NONE',  ( 0.9713206009373563932, 1.803875226702996049, -0.4951341686536685494 ) ) ;
#87363 = EDGE_CURVE ( 'NONE', #7066, #17518, #129635, .T. ) ;
#87364 = CARTESIAN_POINT ( 'NONE',  ( -10.91838098853858519, -9.962496060591744751, 0.1694417511252961916 ) ) ;
#87365 = CARTESIAN_POINT ( 'NONE',  ( 5.707607943424125807, 1.375951858612366019, 1.178334608346263579 ) ) ;
#87366 = CARTESIAN_POINT ( 'NONE',  ( -6.305925513666572613, 6.529536985466737775, -1.006778644550405474E-06 ) ) ;
#87367 = CARTESIAN_POINT ( 'NONE',  ( -10.44369633504468631, 5.112959841837462882, -5.232137017608346596 ) ) ;
#87368 = CARTESIAN_POINT ( 'NONE',  ( -7.465774003072956688, -6.268611901546733201, 7.465774003072982445 ) ) ;
#87369 = CARTESIAN_POINT ( 'NONE',  ( 1.364683531249990311, 3.196875000341416140, 1.214306433183764966E-14 ) ) ;
#87370 = CARTESIAN_POINT ( 'NONE',  ( -5.606595252507366567, 5.572856915785063592, -0.3451608010808376870 ) ) ;
#87371 = CARTESIAN_POINT ( 'NONE',  ( 5.966997003790217136, 8.054858819212300958, -1.443375672974078761 ) ) ;
#87372 = CARTESIAN_POINT ( 'NONE',  ( 1.908577322519442454, 0.6123880975643315461, 1.863924812142327525 ) ) ;
#87373 = CARTESIAN_POINT ( 'NONE',  ( -5.045042558060949034, 6.018876084893449274, 1.082531754730549078 ) ) ;
#87374 = CARTESIAN_POINT ( 'NONE',  ( -4.613517410400161722, 8.604463755433990002, -0.7998128361456362523 ) ) ;
#87375 = CARTESIAN_POINT ( 'NONE',  ( 3.849942018323779358, -1.464806807754112539, -1.533599281611098597 ) ) ;
#87377 = FACE_OUTER_BOUND ( 'NONE', #163109, .T. ) ;
#87376 = CARTESIAN_POINT ( 'NONE',  ( -0.02948999725180690215, 0.001137248348246927814, -1.926291057026579656 ) ) ;
#87378 =( BOUNDED_SURFACE ( )  B_SPLINE_SURFACE ( 3, 2, ( 
 ( #112159, #160838, #43905 ),
 ( #95861, #96930, #210641 ),
 ( #46038, #11365, #143561 ),
 ( #177087, #209555, #176033 ),
 ( #178162, #145698, #62268 ),
 ( #93726, #61199, #27626 ),
 ( #48179, #159765, #126285 ),
 ( #211697, #44974, #158703 ),
 ( #29777, #28704, #161917 ),
 ( #60127, #12429, #127358 ),
 ( #13507, #79580, #129493 ),
 ( #94790, #10302, #78509 ),
 ( #144627, #128428, #113222 ),
 ( #179227, #76376, #30852 ),
 ( #142483, #162981, #80657 ),
 ( #146748, #64402, #212766 ),
 ( #130545, #114292, #180290 ),
 ( #208491, #34022, #35075 ) ),
 .UNSPECIFIED., .F., .F., .T. ) 
 B_SPLINE_SURFACE_WITH_KNOTS ( ( 4, 2, 2, 2, 2, 2, 2, 2, 4 ),
 ( 3, 3 ),
 ( 0.001893572594152294905, 0.002130269168421384217, 0.002366965742690473745, 0.002603662316959563273, 0.002840358891228652802, 0.003077055465497742330, 0.003313752039766831858, 0.003550448614035921387, 0.003787145188305010481 ),
 ( 0.000000000000000000, 1.000000000000000000 ),
 .UNSPECIFIED. ) 
 GEOMETRIC_REPRESENTATION_ITEM ( )  RATIONAL_B_SPLINE_SURFACE ( (
 ( 1.000000000000000000, 0.5649783097559792910, 1.000000000000000000),
 ( 1.000000000000000000, 0.5467450299869786035, 1.000000000000000000),
 ( 1.000000000000000000, 0.5350701846666650052, 1.000000000000000000),
 ( 1.000000000000000000, 0.5340147030925761484, 1.000000000000000000),
 ( 1.000000000000000000, 0.5447811154896929908, 1.000000000000000000),
 ( 1.000000000000000000, 0.5795975317819822559, 1.000000000000000000),
 ( 1.000000000000000000, 0.6028840214605843961, 1.000000000000000000),
 ( 1.000000000000000000, 0.6474634991924845817, 1.000000000000000000),
 ( 1.000000000000000000, 0.6683065367293009595, 1.000000000000000000),
 ( 1.000000000000000000, 0.6980320384850667859, 1.000000000000000000),
 ( 1.000000000000000000, 0.7066998895408396208, 1.000000000000000000),
 ( 1.000000000000000000, 0.7074845257686435129, 1.000000000000000000),
 ( 1.000000000000000000, 0.6995439292593913505, 1.000000000000000000),
 ( 1.000000000000000000, 0.6710262760327935228, 1.000000000000000000),
 ( 1.000000000000000000, 0.6504357685074171336, 1.000000000000000000),
 ( 1.000000000000000000, 0.6062099919889232247, 1.000000000000000000),
 ( 1.000000000000000000, 0.5828135443829657314, 1.000000000000000000),
 ( 1.000000000000000000, 0.5647844906712728985, 1.000000000000000000) ) ) 
 REPRESENTATION_ITEM ( '' )  SURFACE ( )  );
#87379 = CARTESIAN_POINT ( 'NONE',  ( 6.046159394557358624, 1.968988722785993462, 0.09938198387684710200 ) ) ;
#87380 = CARTESIAN_POINT ( 'NONE',  ( -0.6823417656250003738, 1.217708333674752286, -1.181850606188749264 ) ) ;
#87381 = CARTESIAN_POINT ( 'NONE',  ( 1.177990849177086075, 1.982702329297232113, -0.3483419944294365300 ) ) ;
#87382 = ORIENTED_EDGE ( 'NONE', *, *, #78658, .F. ) ;
#87383 = CARTESIAN_POINT ( 'NONE',  ( 0.7907972306774737614, 1.600388572762038830, -1.386229290198564001 ) ) ;
#87384 = CARTESIAN_POINT ( 'NONE',  ( 11.70591049654802696, 7.005752292624462640, -2.417405326248005082 ) ) ;
#87385 = CARTESIAN_POINT ( 'NONE',  ( 2.717306809760032138, -1.800131872397674471, -1.022606600864908399 ) ) ;
#87386 = ORIENTED_EDGE ( 'NONE', *, *, #20109, .F. ) ;
#87387 = CARTESIAN_POINT ( 'NONE',  ( 3.718679271898170491, 7.560485927181699317, 0.7998128361456271485 ) ) ;
#87388 = CARTESIAN_POINT ( 'NONE',  ( 6.387826650694035990, 7.481494509678370264, -1.199719254218452047 ) ) ;
#87389 = ORIENTED_EDGE ( 'NONE', *, *, #87162, .T. ) ;
#87391 = CARTESIAN_POINT ( 'NONE',  ( 5.412729640353754590, 7.337937218544611895, 1.599625672291267398 ) ) ;
#87390 = CARTESIAN_POINT ( 'NONE',  ( 5.033190428309433528, -1.478027449723118725, -1.478843810762977995 ) ) ;
#87394 = ORIENTED_EDGE ( 'NONE', *, *, #191290, .F. ) ;
#87393 = CARTESIAN_POINT ( 'NONE',  ( 1.998415993447474559, -1.776625121221590220, -0.3526093829155519388 ) ) ;
#87392 = CARTESIAN_POINT ( 'NONE',  ( 2.748829393344632166, -1.518919317350690967, 1.012417160375630898 ) ) ;
#87395 = CARTESIAN_POINT ( 'NONE',  ( 6.568967528192747984, -2.015767819289843388, -0.8987472251835016968 ) ) ;
#87396 = CARTESIAN_POINT ( 'NONE',  ( 4.104141037658032509, 5.763691012587534246, 1.360812383240009860 ) ) ;
#87397 = CARTESIAN_POINT ( 'NONE',  ( 4.506973327934083784, 1.708129512224244806, -1.397202154207459524 ) ) ;
#87398 = CARTESIAN_POINT ( 'NONE',  ( 8.471147050440139381, 8.777426401801974976, -0.7998128361456281477 ) ) ;
#87399 = CARTESIAN_POINT ( 'NONE',  ( 1.364683531249996529, 9.526041667008062319, 0.7879004041258403923 ) ) ;
#87400 = ORIENTED_EDGE ( 'NONE', *, *, #88823, .T. ) ;
#87401 = CARTESIAN_POINT ( 'NONE',  ( 3.334525359879161766, 1.211162569113528598, -1.479845612687477496 ) ) ;
#87402 = CARTESIAN_POINT ( 'NONE',  ( -3.867100128395853709, 5.534702787927018974, -1.599625672291256295 ) ) ;
#87403 = VECTOR ( 'NONE', #184214, 1000.000000000000000 ) ;
#87404 = CARTESIAN_POINT ( 'NONE',  ( 7.151035956204054855, 10.43029348462504124, 1.199719254218460707 ) ) ;
#87405 = CARTESIAN_POINT ( 'NONE',  ( 6.877413708759195998, -0.1538780216673047430, 2.036608477593480959 ) ) ;
#87406 = STYLED_ITEM ( 'NONE', ( #137967 ), #52970 ) ;
#87407 = CARTESIAN_POINT ( 'NONE',  ( -0.6801582343750316451, 0.8802083336747270614, -1.178068619123876282 ) ) ;
#87408 = CARTESIAN_POINT ( 'NONE',  ( 6.040607902356621928, -1.852314659301615096, 1.170993205287726990 ) ) ;
#87409 = CARTESIAN_POINT ( 'NONE',  ( 5.586791213849657822, 7.504901977030062454, -1.335864709735144817 ) ) ;
#87410 = CARTESIAN_POINT ( 'NONE',  ( -8.171050030069373804, 15.51987628351127313, -8.834037170385874660 ) ) ;
#87411 = ORIENTED_EDGE ( 'NONE', *, *, #57852, .F. ) ;
#87412 = ORIENTED_EDGE ( 'NONE', *, *, #208952, .T. ) ;
#87413 = CARTESIAN_POINT ( 'NONE',  ( 1.484314741415208694, 7.334687650741242848, -4.257443109328156616 ) ) ;
#87414 = CARTESIAN_POINT ( 'NONE',  ( 3.145614842782416432, 0.6765965015090926737, -1.744060075730607950 ) ) ;
#87415 = CARTESIAN_POINT ( 'NONE',  ( -3.285556943750000514, -1.276041666188709511, -1.896917185911906722 ) ) ;
#87416 = CARTESIAN_POINT ( 'NONE',  ( 4.000000000000012434, 5.999999999999998224, -0.7500000000000006661 ) ) ;
#87417 = CARTESIAN_POINT ( 'NONE',  ( -7.863365906246068349, 9.236643647784308797, -1.082531754730543971 ) ) ;
#87418 = CARTESIAN_POINT ( 'NONE',  ( 4.706615602599436343, 5.520081620234675412, 1.199719254218452935 ) ) ;
#87419 = CARTESIAN_POINT ( 'NONE',  ( 0.5144232481557647896, 0.7485027850700550767, 1.821871385004094845 ) ) ;
#87420 = CARTESIAN_POINT ( 'NONE',  ( 1.616814774554303780, 0.2004563524992293566, 2.006445175307514095 ) ) ;
#87421 = CARTESIAN_POINT ( 'NONE',  ( -10.47097470845587175, 11.11055866948701443, 1.040834085586084257E-14 ) ) ;
#87422 = CARTESIAN_POINT ( 'NONE',  ( 8.005163354226054295, 8.304055099544019214, 0.000000000000000000 ) ) ;
#87423 = CARTESIAN_POINT ( 'NONE',  ( -0.07900062026858570285, 7.629137130509076492, -2.773896239169175271 ) ) ;
#87424 = CARTESIAN_POINT ( 'NONE',  ( 1.904481915951491189, 1.622449043516610123, -1.473309109067892697 ) ) ;
#87425 = CARTESIAN_POINT ( 'NONE',  ( 6.498675964634617941, -0.4922777150685350156, -1.758009983081544991 ) ) ;
#87426 = CARTESIAN_POINT ( 'NONE',  ( -3.918470089549458635, 4.530302178351167441, -1.199719254218452047 ) ) ;
#87427 = CARTESIAN_POINT ( 'NONE',  ( 6.536439455564164724, 7.758839131980592718, 1.082531754730549967 ) ) ;
#87428 = CARTESIAN_POINT ( 'NONE',  ( 8.615316546479974136, 12.13862083994696839, 1.199719254218450271 ) ) ;
#87429 = CARTESIAN_POINT ( 'NONE',  ( 4.891794496432329886, 4.601515088792824670, -0.7998128361456211532 ) ) ;
#87430 = CARTESIAN_POINT ( 'NONE',  ( 6.699137298928145690, 8.909022496873262753, 1.443375672974065660 ) ) ;
#87431 = VERTEX_POINT ( 'NONE', #41035 ) ;
#87433 = CARTESIAN_POINT ( 'NONE',  ( 0.3111896917125516748, 1.672494819392616128, -1.120119447130196288 ) ) ;
#87432 = CARTESIAN_POINT ( 'NONE',  ( 3.737712173649463399, 1.832726675769575486, 0.1767833568970395008 ) ) ;
#87434 = CARTESIAN_POINT ( 'NONE',  ( 2.249760294480507294, -2.253934603285558502, -0.4491563171437322199 ) ) ;
#87436 = CARTESIAN_POINT ( 'NONE',  ( 6.526224699197019419, 1.005635830909179074, 1.684226478273798788 ) ) ;
#87435 = CARTESIAN_POINT ( 'NONE',  ( 2.873965376416980355, 6.296784005887697155, -0.7216878364870267237 ) ) ;
#87437 = CARTESIAN_POINT ( 'NONE',  ( -5.928993247877788697, 5.811580298812519807, 0.7998128361456341429 ) ) ;
#87438 = DIRECTION ( 'NONE',  ( -0.000000000000000000, 0.000000000000000000, -1.000000000000000000 ) ) ;
#87439 = CARTESIAN_POINT ( 'NONE',  ( 4.746305163667582150, 0.9781546018433548983, -1.643150005489722787 ) ) ;
#87440 = CARTESIAN_POINT ( 'NONE',  ( -9.001723924469462901, 12.58942944760136484, -1.199719254218446718 ) ) ;
#87441 = CARTESIAN_POINT ( 'NONE',  ( 6.469672735924913987, 6.762149564967588233, 0.2594904213018677797 ) ) ;
#87442 = CARTESIAN_POINT ( 'NONE',  ( -3.284818356260900796, 7.054314858938165678, 0.7998128361456352531 ) ) ;
#87444 = CARTESIAN_POINT ( 'NONE',  ( 1.182252951876180180, -1.824241171369020531, -0.4133900166373091767 ) ) ;
#87443 = CARTESIAN_POINT ( 'NONE',  ( 2.560199545759346496, -1.439800679921798165, 1.516228354532923372 ) ) ;
#87445 = CARTESIAN_POINT ( 'NONE',  ( 2.196638537759632470, -1.314794530490107638, -1.528507974810841219 ) ) ;
#87446 = CARTESIAN_POINT ( 'NONE',  ( 7.131225611108079399, 11.26358761302737754, 0.7216878364870438212 ) ) ;
#87447 = B_SPLINE_CURVE_WITH_KNOTS ( 'NONE', 3,
 ( #126016, #75051, #6819, #24144, #190915, #90246, #72898, #174712, #22849, #103067, #119376, #118309, #3400, #4456, #90031, #53246, #70526, #170185, #136643, #202668 ),
 .UNSPECIFIED., .F., .F.,
 ( 4, 2, 1, 1, 1, 1, 2, 2, 2, 2, 2, 4 ),
 ( 0.9387693520046538342, 0.9388889431140197139, 0.9390085342233857046, 0.9392477164421174640, 0.9397260808795810938, 0.9406828097545083534, 0.9425962675043629835, 0.9464231830040721327, 0.9540770140034904312, 0.9693846760023269171, 0.9846923380011635141, 1.000000000000000000 ),
 .UNSPECIFIED. ) ;
#87448 = CARTESIAN_POINT ( 'NONE',  ( -1.364683531250012516, 3.592708333674750065, 0.7879004041258379498 ) ) ;
#87449 = CARTESIAN_POINT ( 'NONE',  ( 2.858654643706417975, 0.2527927160936989659, -1.721832920378673748 ) ) ;
#87450 = VECTOR ( 'NONE', #70067, 1000.000000000000000 ) ;
#87451 = CARTESIAN_POINT ( 'NONE',  ( 5.009901455449552010, 5.803638771901306725, -1.199719254218452047 ) ) ;
#87453 = CARTESIAN_POINT ( 'NONE',  ( 0.3581693041846744086, 3.206512658508270164, -2.035393093115380747 ) ) ;
#87452 = CARTESIAN_POINT ( 'NONE',  ( 11.86145016429272836, 10.90000000000000036, 1.179999999999997051 ) ) ;
#87454 = CARTESIAN_POINT ( 'NONE',  ( 4.459404883141235842, 0.3742951803532655330, -1.683599696842478677 ) ) ;
#87455 = CARTESIAN_POINT ( 'NONE',  ( 3.685266855566126321, 1.588411730319793769, 1.510178839762461811 ) ) ;
#87456 = CARTESIAN_POINT ( 'NONE',  ( -1.436715752608711538, 7.421775496532096561, 4.237684949271969259 ) ) ;
#87457 = CARTESIAN_POINT ( 'NONE',  ( 3.959984535978885667, -0.6353779353734061441, 2.075986281735443750 ) ) ;
#87458 = CARTESIAN_POINT ( 'NONE',  ( 1.646812808029130215, -1.543121136568927243, 0.9753659028155501343 ) ) ;
#87459 = CARTESIAN_POINT ( 'NONE',  ( 0.3034670832338138835, -1.512625156342655819, -1.248876549296701333 ) ) ;
#87460 = CARTESIAN_POINT ( 'NONE',  ( 3.995394017595743641, -0.3581701549109669869, 2.086669383214428297 ) ) ;
#87461 = VERTEX_POINT ( 'NONE', #126610 ) ;
#87463 = CARTESIAN_POINT ( 'NONE',  ( -0.6823417656250003738, 2.780208333674753618, -1.181850606188749264 ) ) ;
#87462 = CARTESIAN_POINT ( 'NONE',  ( 5.126663105998436443, 0.1666055143465100530, 2.286395203598155845 ) ) ;
#87464 = CARTESIAN_POINT ( 'NONE',  ( 6.620655732516649294, 0.5971256128398574337, 1.879834161342401666 ) ) ;
#87465 = CARTESIAN_POINT ( 'NONE',  ( 10.55232363013785246, 11.20546574478267132, 0.000000000000000000 ) ) ;
#87466 = ADVANCED_FACE ( 'NONE', ( #124487 ), #43307, .F. ) ;
#87467 = CARTESIAN_POINT ( 'NONE',  ( 0.3289748556246673838, 1.459166701075472750, -1.538843095060193233 ) ) ;
#87468 = CARTESIAN_POINT ( 'NONE',  ( -5.639828713604883248, 6.642516923036197340, 1.082531754730548412 ) ) ;
#87469 = CARTESIAN_POINT ( 'NONE',  ( 0.000000000000000000, 13.49999999999999822, 0.000000000000000000 ) ) ;
#87470 = AXIS2_PLACEMENT_3D ( 'NONE', #106068, #73506, #123431 ) ;
#87471 = CARTESIAN_POINT ( 'NONE',  ( -6.033015167956818026, 6.140865238812146742, -0.7216878364870267237 ) ) ;
#87472 = AXIS2_PLACEMENT_3D ( 'NONE', #169091, #32698, #4427 ) ;
#87473 = DIRECTION ( 'NONE',  ( 0.000000000000000000, 1.000000000000000000, 0.000000000000000000 ) ) ;
#87474 = VERTEX_POINT ( 'NONE', #17011 ) ;
#87475 = CARTESIAN_POINT ( 'NONE',  ( 5.397111353752316987, -0.9091427841607623295, -1.799923777076550824 ) ) ;
#87477 = CARTESIAN_POINT ( 'NONE',  ( 4.241124981676721362, -0.1973008666005781619, -2.053083420615212429 ) ) ;
#87476 = CARTESIAN_POINT ( 'NONE',  ( 3.960953433486789521, 7.772862772376584850, -0.7998128361456221525 ) ) ;
#87479 = CARTESIAN_POINT ( 'NONE',  ( -0.1408020194049964258, 1.331054986036240173, -2.350941690117592575 ) ) ;
#87478 = CARTESIAN_POINT ( 'NONE',  ( 6.852720297064418986, 6.959538199522133262, 0.7998128361456331437 ) ) ;
#87480 = CARTESIAN_POINT ( 'NONE',  ( 5.013482942003290255, 9.071090208970993274, -0.7998128361456481317 ) ) ;
#87481 = CARTESIAN_POINT ( 'NONE',  ( 1.642778471875000035, -0.5760416661887077794, -2.845375778867859751 ) ) ;
#87482 = DIRECTION ( 'NONE',  ( -1.000000000000000000, 0.000000000000000000, 0.000000000000000000 ) ) ;
#87483 = CARTESIAN_POINT ( 'NONE',  ( 0.1114262914704557683, -2.049844763593706265, 0.4100319678014376912 ) ) ;
#87484 = CARTESIAN_POINT ( 'NONE',  ( 4.764296165657141202, 1.880435471729305030, -0.7283773170061805802 ) ) ;
#87485 = CARTESIAN_POINT ( 'NONE',  ( 3.386116603743833497, -0.3623624896987759914, -1.805063595765175499 ) ) ;
#87486 = CARTESIAN_POINT ( 'NONE',  ( 5.412729640353754590, 7.337937218544611895, 1.599625672291267398 ) ) ;
#87487 = EDGE_CURVE ( 'NONE', #25476, #180844, #113545, .T. ) ;
#87488 = CARTESIAN_POINT ( 'NONE',  ( 0.2172357734837098431, -1.693002290532450882, 0.3285655886510214230 ) ) ;
#87489 = AXIS2_PLACEMENT_3D ( 'NONE', #213813, #36144, #118540 ) ;
#87490 = DIRECTION ( 'NONE',  ( 1.214306433183764966E-17, 1.000000000000000000, 5.200009205990155575E-32 ) ) ;
#87491 = CARTESIAN_POINT ( 'NONE',  ( 0.5987520574620349700, -0.3298207119002970478, 2.274815185769126114 ) ) ;
#87492 = CARTESIAN_POINT ( 'NONE',  ( -7.237355071596549116, 7.338002426484427687, 1.040834085586084257E-14 ) ) ;
#87493 = CARTESIAN_POINT ( 'NONE',  ( 0.2458944382301266607, -1.750094391731635168, -1.433289930825008218 ) ) ;
#87494 = CARTESIAN_POINT ( 'NONE',  ( 3.422586708326117666, 1.336063110485498973, -1.628023012543792447 ) ) ;
#87495 = CARTESIAN_POINT ( 'NONE',  ( -5.472651281771599763, 6.413789912602166687, 1.199719254218452935 ) ) ;
#87496 = CARTESIAN_POINT ( 'NONE',  ( 6.588372581236919601, 9.773852880496709972, -1.199719254218440723 ) ) ;
#87497 = CARTESIAN_POINT ( 'NONE',  ( 6.712695452097489301, 7.964471127936110229, -1.082531754730548412 ) ) ;
#87498 = CARTESIAN_POINT ( 'NONE',  ( 6.500000003069670740, 7.552736074387352678E-08, -2.052068128417939175 ) ) ;
#87499 = CARTESIAN_POINT ( 'NONE',  ( -7.739006755302186846, 7.923262724141010516, 0.7998128361456462443 ) ) ;
#87500 = B_SPLINE_CURVE_WITH_KNOTS ( 'NONE', 3,
 ( #141933, #46540, #207946, #92104, #96369, #75826 ),
 .UNSPECIFIED., .F., .F.,
 ( 4, 2, 4 ),
 ( 0.000000000000000000, 0.0003844267940947825469, 0.0007688535881895650938 ),
 .UNSPECIFIED. ) ;
#87501 = CARTESIAN_POINT ( 'NONE',  ( 7.144783764277405247, 8.398297815487545392, -1.082531754730543971 ) ) ;
#87502 = CARTESIAN_POINT ( 'NONE',  ( 5.221388208558932931, 6.626734370510860117, 1.385765457383714816 ) ) ;
#87503 = AXIS2_PLACEMENT_3D ( 'NONE', #143172, #58674, #124823 ) ;
#87504 = CARTESIAN_POINT ( 'NONE',  ( -3.490334480514268645, 6.159475096320226939, -1.199719254218452935 ) ) ;
#87505 = CARTESIAN_POINT ( 'NONE',  ( 3.463320643641348173, -1.814240386431978713, 1.281607931980492054 ) ) ;
#87506 = CARTESIAN_POINT ( 'NONE',  ( 2.888834398507355239, 1.879202789969806497, -1.127179367409691935 ) ) ;
#87507 = CARTESIAN_POINT ( 'NONE',  ( -7.250913225210214641, 7.353820272367037170, 0.7998128361456341429 ) ) ;
#87508 = CARTESIAN_POINT ( 'NONE',  ( -4.339491684825780737, 7.220434844675483355, -1.199719254218455378 ) ) ;
#87509 = CARTESIAN_POINT ( 'NONE',  ( 5.582460749670235423, 1.169929261559121247, -1.574690175210855747 ) ) ;
#87510 = CARTESIAN_POINT ( 'NONE',  ( -1.364683531250000748, 1.759375000341421913, 0.000000000000000000 ) ) ;
#87511 = CARTESIAN_POINT ( 'NONE',  ( 6.610000000000003872, 7.053606217926155608, 2.318153411789238838 ) ) ;
#87512 = CARTESIAN_POINT ( 'NONE',  ( -5.097502569058215194, 6.970172302033127210, -1.443375672974053447 ) ) ;
#87513 = CARTESIAN_POINT ( 'NONE',  ( 4.939744792934912532, -2.012803497507458683, 0.6676120485993168874 ) ) ;
#87514 = CARTESIAN_POINT ( 'NONE',  ( -3.634467696915153034, 6.397906858779740524, 1.199719254218452935 ) ) ;
#87515 = ORIENTED_EDGE ( 'NONE', *, *, #16285, .T. ) ;
#87517 = CARTESIAN_POINT ( 'NONE',  ( 5.629794960336353071, -1.368038101806166029, -1.673757646710342550 ) ) ;
#87516 = CARTESIAN_POINT ( 'NONE',  ( -5.316205630334263965, 7.295602216847000498, -1.443375672974066548 ) ) ;
#87518 = CARTESIAN_POINT ( 'NONE',  ( 5.469824908109481854, 8.468880595181346393, -1.199719254218446718 ) ) ;
#87519 = CARTESIAN_POINT ( 'NONE',  ( 5.460457653299121361, -1.667157065227730106, -0.7818181906407914994 ) ) ;
#87520 = CARTESIAN_POINT ( 'NONE',  ( -5.867692518273577740, 6.026634161543212187, 0.3546184694816056360 ) ) ;
#87521 = CARTESIAN_POINT ( 'NONE',  ( -1.364683531250014514, 1.801041667008085767, -0.7879004041258289570 ) ) ;
#87522 = CARTESIAN_POINT ( 'NONE',  ( 0.09860955243249854008, -0.4675299588126168859, 1.676413046982327515 ) ) ;
#87523 = DIRECTION ( 'NONE',  ( 1.000000000000000000, 0.000000000000000000, 0.000000000000000000 ) ) ;
#87524 = CARTESIAN_POINT ( 'NONE',  ( -0.2939347205469681756, 8.204283511488997149, 1.979604457746021895 ) ) ;
#87525 = DIRECTION ( 'NONE',  ( -5.578564026256490882E-16, -1.000000000000000000, -9.066213480720158442E-32 ) ) ;
#87526 = CARTESIAN_POINT ( 'NONE',  ( 4.293933718354110418, -0.8299404887524584051, 1.996233173270183681 ) ) ;
#87527 = CARTESIAN_POINT ( 'NONE',  ( -3.411848212133334446, 7.132240014130862171, 0.7998128361456341429 ) ) ;
#87528 = CARTESIAN_POINT ( 'NONE',  ( -6.629573926958124197, 9.717958100551031819, 1.082531754730548412 ) ) ;
#87529 = CARTESIAN_POINT ( 'NONE',  ( 3.766626874709140704, -1.453462046928340579, 1.600284095077113333 ) ) ;
#87530 = CARTESIAN_POINT ( 'NONE',  ( 4.622318808457460015, 1.215050846432633946, -1.552280729921464708 ) ) ;
#87531 = CARTESIAN_POINT ( 'NONE',  ( 4.200348813226637112, -1.195399808894830773, -1.256130793262473455 ) ) ;
#87532 = CARTESIAN_POINT ( 'NONE',  ( 0.5038066827526345159, -2.180447833630628107, 0.2205874978757973448 ) ) ;
#87533 = CARTESIAN_POINT ( 'NONE',  ( 1.905729856612170758, 1.919199136376721793, 1.280985070478329435 ) ) ;
#87534 = CARTESIAN_POINT ( 'NONE',  ( 4.130192093715317370, 1.105610312200686174, -1.738907380658259560 ) ) ;
#87535 = CARTESIAN_POINT ( 'NONE',  ( 5.407742453289367646, -0.8769457196468108950, -1.732881886176732777 ) ) ;
#87536 = CARTESIAN_POINT ( 'NONE',  ( -6.507550544435101614, 10.53596670190887963, 0.000000000000000000 ) ) ;
#87537 = CARTESIAN_POINT ( 'NONE',  ( -5.712781623311813384, 7.758274208654143855, -1.599625672291271394 ) ) ;
#87538 = CARTESIAN_POINT ( 'NONE',  ( -5.029148636026397945, 4.832037928311032182, 0.7998128361456281477 ) ) ;
#87539 = CARTESIAN_POINT ( 'NONE',  ( -5.816084710138169633, 8.768887347594400694, 1.082531754730548412 ) ) ;
#87540 = CARTESIAN_POINT ( 'NONE',  ( 3.680891063843365174, -2.126115503207156809, -0.5908918699835326027 ) ) ;
#87541 = CARTESIAN_POINT ( 'NONE',  ( 0.000000000000000000, -2.734374999522040550, -3.793834371823813001 ) ) ;
#87542 = EDGE_LOOP ( 'NONE', ( #154519, #101122, #17827, #43081 ) ) ;
#87543 = CARTESIAN_POINT ( 'NONE',  ( 0.2388273096324589895, -0.1346187373043924163, -1.830540737478093982 ) ) ;
#87544 = CARTESIAN_POINT ( 'NONE',  ( -0.02900071798685523866, 4.082342745036794618, -2.728474045032194262 ) ) ;
#87545 = CARTESIAN_POINT ( 'NONE',  ( 1.499999999999989120, 5.577083334016153415, -0.8660254037844323793 ) ) ;
#87546 = CARTESIAN_POINT ( 'NONE',  ( 1.823500102806385970, 2.449814546280965732, -2.460149141570041831 ) ) ;
#87548 = CARTESIAN_POINT ( 'NONE',  ( 6.925078400183519278, 1.259550266093687920, 2.159391284976417857 ) ) ;
#87547 = CARTESIAN_POINT ( 'NONE',  ( -6.453559683527718249, 6.864596255245277057, -0.6992757447422948136 ) ) ;
#87549 = DIRECTION ( 'NONE',  ( 0.000000000000000000, 0.000000000000000000, 1.000000000000000000 ) ) ;
#87550 = EDGE_LOOP ( 'NONE', ( #172575, #73519, #46027, #80223 ) ) ;
#87551 = CARTESIAN_POINT ( 'NONE',  ( 3.309499033229778231, -0.4035708669713148899, 2.020805850887919863 ) ) ;
#87552 = CARTESIAN_POINT ( 'NONE',  ( -1.752700365193352367E-14, 0.07812500034142640104, -1.570758158831804474 ) ) ;
#87553 = CARTESIAN_POINT ( 'NONE',  ( -6.728924311084075960, 6.744833205886536120, 1.040834085586084257E-14 ) ) ;
#87554 = CARTESIAN_POINT ( 'NONE',  ( 0.07680821025393690105, 0.005952109439256307241, -1.810863387344714193 ) ) ;
#87555 = CYLINDRICAL_SURFACE ( 'NONE', #147805, 0.3999999999999997446 ) ;
#87556 = CARTESIAN_POINT ( 'NONE',  ( 4.630273154266905777, 5.360739087188218122, 1.199719254218464037 ) ) ;
#87557 = CARTESIAN_POINT ( 'NONE',  ( 1.534131747024346737, 1.016495879925772616, -1.792692027746685346 ) ) ;
#87559 = CARTESIAN_POINT ( 'NONE',  ( -0.6823417656250003738, 12.90104166700806232, 1.181850606188754593 ) ) ;
#87558 = PLANE ( 'NONE',  #107733 ) ;
#87560 = CARTESIAN_POINT ( 'NONE',  ( 5.982172092127724383, 8.002286745614243912, -1.599625672291262513 ) ) ;
#87561 = CIRCLE ( 'NONE', #104729, 6.200000000000000178 ) ;
#87562 = CARTESIAN_POINT ( 'NONE',  ( -0.2409995289980003397, 2.873648158547074338, -2.488896373646624749 ) ) ;
#87563 = CARTESIAN_POINT ( 'NONE',  ( 5.602238545945851023, -2.207063162045197924, -0.003355105161521875021 ) ) ;
#87564 = CARTESIAN_POINT ( 'NONE',  ( 6.626273523942327159, 1.310778252226969975, -1.843845376178480322 ) ) ;
#87565 = CARTESIAN_POINT ( 'NONE',  ( -5.450014563013544588, 5.460697866378308341, 0.7216878364870317197 ) ) ;
#87566 = CARTESIAN_POINT ( 'NONE',  ( 0.2863426850727782136, -0.6839425765656822476, -1.897108587135355684 ) ) ;
#87567 = CARTESIAN_POINT ( 'NONE',  ( 1.511505665106587459, 2.295766583369537095, 0.1122837871174054425 ) ) ;
#87568 =( LENGTH_UNIT ( ) NAMED_UNIT ( * ) SI_UNIT ( .MILLI., .METRE. ) );
#87569 = CARTESIAN_POINT ( 'NONE',  ( -0.4370932794886463468, -5.427673425445475708, -10.76345817711984054 ) ) ;
#87570 = DIRECTION ( 'NONE',  ( 0.000000000000000000, 0.000000000000000000, -1.000000000000000000 ) ) ;
#87571 = CARTESIAN_POINT ( 'NONE',  ( 2.307302758404996545, -0.4121581357655336175, 1.824517092411604979 ) ) ;
#87572 = CARTESIAN_POINT ( 'NONE',  ( 3.221888912838869690, 0.9023448338944944913, -1.803416113280359445 ) ) ;
#87574 = CARTESIAN_POINT ( 'NONE',  ( 6.639320575229281651, -0.0007625845807879281287, 2.103388539994067497 ) ) ;
#87573 = CARTESIAN_POINT ( 'NONE',  ( 0.6823417656249882723, 0.9260416670080831025, -1.181850606188749264 ) ) ;
#87576 = CARTESIAN_POINT ( 'NONE',  ( 5.426436078920066741, 1.255580583125959437, -1.690716914145540040 ) ) ;
#87575 = CARTESIAN_POINT ( 'NONE',  ( -8.045874094706015001, 11.47427131287732927, -1.199719254218446718 ) ) ;
#87577 = CARTESIAN_POINT ( 'NONE',  ( 6.120616281565444794, 9.228137197546649517, -1.199719254218440723 ) ) ;
#87579 = CARTESIAN_POINT ( 'NONE',  ( -7.823218330285243383, 9.085841792542966644, -1.199719254218446718 ) ) ;
#87578 = CARTESIAN_POINT ( 'NONE',  ( 3.413620815590684199, 7.204584394822967752, 0.7998128361456281477 ) ) ;
#87580 = CARTESIAN_POINT ( 'NONE',  ( 1.350829346764933936, 3.446353025980462892, -0.3155766437963711257 ) ) ;
#87581 = CARTESIAN_POINT ( 'NONE',  ( 4.394789018838915595, -1.960137222954833502, -0.4867870608649630393 ) ) ;
#87582 = CARTESIAN_POINT ( 'NONE',  ( 0.6823417656249917140, 4.842708333674755394, 1.181850606188765695 ) ) ;
#87583 = CARTESIAN_POINT ( 'NONE',  ( 0.9364711893796459075, -1.149011738537804250, 1.712694122252313100 ) ) ;
#87584 = CARTESIAN_POINT ( 'NONE',  ( 8.378575743565351175, 11.75846021992619406, -1.082531754730543083 ) ) ;
#87585 = CARTESIAN_POINT ( 'NONE',  ( 5.448557382023540896, 0.6217387762853660016, 2.070273951448368788 ) ) ;
#87586 = CARTESIAN_POINT ( 'NONE',  ( 7.523848900940885542, 7.742521570711348389, 0.7998128361456291469 ) ) ;
#87587 = CARTESIAN_POINT ( 'NONE',  ( -1.402160292154681736E-14, -0.1156249996585793222, 1.575800808251672791 ) ) ;
#87589 = CARTESIAN_POINT ( 'NONE',  ( -0.1108833634136767443, 0.0002062650063822807356, -1.896853557917008271 ) ) ;
#87588 = CARTESIAN_POINT ( 'NONE',  ( 5.071631979963703962, 8.074598522336444262, 1.199719254218451159 ) ) ;
#87590 = CARTESIAN_POINT ( 'NONE',  ( 7.415946836550714849, 9.675023947441092176, 1.443375672974076540 ) ) ;
#87592 = CARTESIAN_POINT ( 'NONE',  ( -6.735605996566196296E-15, -8.407420853759283830, 11.00029519899101338 ) ) ;
#87591 = CARTESIAN_POINT ( 'NONE',  ( 3.121698260611803999, 0.3212384671735257213, -2.147181447086630612 ) ) ;
#87594 = CARTESIAN_POINT ( 'NONE',  ( 2.102840161960460197, -0.4018910908503615653, 1.796694178532439956 ) ) ;
#87593 = CARTESIAN_POINT ( 'NONE',  ( -4.934804725694220906, 7.740727365743146571, -1.082531754730549967 ) ) ;
#87595 = EDGE_CURVE ( 'NONE', #90065, #53890, #58213, .T. ) ;
#87596 = CARTESIAN_POINT ( 'NONE',  ( 0.6823417656249917140, 3.842708333674754506, 1.181850606188765695 ) ) ;
#87597 = CARTESIAN_POINT ( 'NONE',  ( 3.456733517523991051, -1.933646301634945885, -1.031433503814835007 ) ) ;
#87598 = CARTESIAN_POINT ( 'NONE',  ( 6.983263157960368339, 1.232032666090671302, 2.265420076015733031 ) ) ;
#87599 = CARTESIAN_POINT ( 'NONE',  ( 4.329186484417943959, 0.1072846252610352574, 2.260086081085868948 ) ) ;
#87600 = CARTESIAN_POINT ( 'NONE',  ( -6.392833124043511894, 7.417059051927569868, 1.199719254218450271 ) ) ;
#87601 = DIRECTION ( 'NONE',  ( 0.000000000000000000, -1.000000000000000000, 0.000000000000000000 ) ) ;
#87602 = CARTESIAN_POINT ( 'NONE',  ( 6.492506472431533560, 6.747478052702773788, -0.04572756507489894595 ) ) ;
#87603 = CIRCLE ( 'NONE', #205086, 0.08000000000000020983 ) ;
#87604 = CARTESIAN_POINT ( 'NONE',  ( -6.009258394948636914E-15, 13.93750000000000178, -1.732050807568875195 ) ) ;
#87605 = CARTESIAN_POINT ( 'NONE',  ( 4.746763178560250651, 7.591621904078704297, 1.082531754730549078 ) ) ;
#87606 = CARTESIAN_POINT ( 'NONE',  ( 5.694547528447587048, -0.4312477495709844399, -1.716266690248748672 ) ) ;
#87607 = CARTESIAN_POINT ( 'NONE',  ( 6.747154001095143627, 11.02343010125301959, -0.7998128361456291469 ) ) ;
#87608 = CARTESIAN_POINT ( 'NONE',  ( 1.606614413041591360, -0.7575671727712609549, -1.965171518483445068 ) ) ;
#87609 = CARTESIAN_POINT ( 'NONE',  ( 1.364683531250000303, 12.00520833367473195, -0.7879004041258355073 ) ) ;
#87610 = CARTESIAN_POINT ( 'NONE',  ( 1.908593538011025492, 0.6150006609981206740, 1.871157805954210440 ) ) ;
#87611 = CARTESIAN_POINT ( 'NONE',  ( -4.981695098378565945, 4.776675467721892332, -0.7998128361456362523 ) ) ;
#87612 = CARTESIAN_POINT ( 'NONE',  ( 0.3265133270617843197, -1.284392789319420913, 1.483054880892266114 ) ) ;
#87614 = ORIENTED_EDGE ( 'NONE', *, *, #40364, .F. ) ;
#87613 = CARTESIAN_POINT ( 'NONE',  ( 5.748286673958676651, 0.8850744635948673000, -1.580567631948928797 ) ) ;
#87615 = CARTESIAN_POINT ( 'NONE',  ( 5.327991180490514012, 9.159814110640187579, 1.040834085586084257E-14 ) ) ;
#87616 = CARTESIAN_POINT ( 'NONE',  ( 1.364683531249986537, -0.5322916663252452718, -0.7879004041258309554 ) ) ;
#87617 = CARTESIAN_POINT ( 'NONE',  ( 4.768341783539651324, -1.221614081569386112, 1.416756073533788518 ) ) ;
#87618 = CARTESIAN_POINT ( 'NONE',  ( 5.207906454484914072, 0.6546344234062730916, -1.964071172066352400 ) ) ;
#87619 = AXIS2_PLACEMENT_3D ( 'NONE', #120914, #205259, #41744 ) ;
#87620 = CARTESIAN_POINT ( 'NONE',  ( -1.225000000000012301, 2.770833333333349469, 0.7072540797572637317 ) ) ;
#87621 = EDGE_CURVE ( 'NONE', #59844, #134155, #74368, .T. ) ;
#87622 = CARTESIAN_POINT ( 'NONE',  ( -6.427974226210522168, 6.671927150099951298, 0.000000000000000000 ) ) ;
#87623 = CARTESIAN_POINT ( 'NONE',  ( -0.7500000000000215383, 0.6916666666666876351, 1.299038105676659116 ) ) ;
#87624 = CARTESIAN_POINT ( 'NONE',  ( 8.586391356156291010, 8.911878091804165791, 0.7998128361456481317 ) ) ;
#87625 = CARTESIAN_POINT ( 'NONE',  ( -8.992082194361570302, 11.51384853155376220, 1.599625672291269396 ) ) ;
#87626 = CARTESIAN_POINT ( 'NONE',  ( 4.505052181490820651, 8.477920988373101707, -0.7998128361456381397 ) ) ;
#87627 = CARTESIAN_POINT ( 'NONE',  ( -1.364683531250014514, -0.7197916663252461600, 0.7879004041258379498 ) ) ;
#87628 = CARTESIAN_POINT ( 'NONE',  ( -1.201851678989727383E-14, 1.712500000000019229, 1.732050807568877637 ) ) ;
#87630 = CARTESIAN_POINT ( 'NONE',  ( 5.820528018968444961, 5.685037531751635953, 0.7998128361456341429 ) ) ;
#87629 = CARTESIAN_POINT ( 'NONE',  ( 4.826587731031282580, -1.282962940432516907, 1.484285152025546672 ) ) ;
#87631 = CARTESIAN_POINT ( 'NONE',  ( 2.917342117414220670, 0.6766092434087739305, 1.899328150365031664 ) ) ;
#87632 = CARTESIAN_POINT ( 'NONE',  ( 2.641684811942858424, 1.906066497734011378, -0.1923337340370822046 ) ) ;
#87633 = DIRECTION ( 'NONE',  ( 0.000000000000000000, 1.000000000000000000, 0.000000000000000000 ) ) ;
#87634 = AXIS2_PLACEMENT_3D ( 'NONE', #56315, #158097, #173281 ) ;
#87635 = CARTESIAN_POINT ( 'NONE',  ( 0.5740950506661415265, -1.212703583203307511, 1.825263377225619266 ) ) ;
#87636 = FILL_AREA_STYLE_COLOUR ( '', #111661 ) ;
#87637 = CARTESIAN_POINT ( 'NONE',  ( 2.618241971997347317, 1.224968108320439342, -1.413705424714882586 ) ) ;
#87638 = CARTESIAN_POINT ( 'NONE',  ( -1.201851678989727383E-14, 5.446875000341422357, -1.575800808251660134 ) ) ;
#87639 = CARTESIAN_POINT ( 'NONE',  ( 4.060795210881157580, 0.5408870827437872730, 1.939095388008914345 ) ) ;
#87640 = CARTESIAN_POINT ( 'NONE',  ( -9.494787648271923786, 9.971673765939062406, 1.040834085586084257E-14 ) ) ;
#87642 = CARTESIAN_POINT ( 'NONE',  ( 4.991875679739185223, -2.106924267290931851, 0.2088435281543659927 ) ) ;
#87641 = CARTESIAN_POINT ( 'NONE',  ( -4.433153041988574294, 8.115836282387899558, 1.040834085586084257E-14 ) ) ;
#87643 = MANIFOLD_SOLID_BREP ( 'Fillet1', #56949 ) ;
#87644 = CARTESIAN_POINT ( 'NONE',  ( -5.361566827843197380, 4.701484413405883522, -2.440314516401218992 ) ) ;
#87645 = CARTESIAN_POINT ( 'NONE',  ( 6.215297738502283842, -1.773692237561547147, -1.067698627785176768 ) ) ;
#87647 = CARTESIAN_POINT ( 'NONE',  ( 11.80235830595197655, 13.79999999999998295, 1.696088231482818065 ) ) ;
#87646 = CARTESIAN_POINT ( 'NONE',  ( 1.347338520094189862, 0.6037249722931283813, -2.001697839036377324 ) ) ;
#87649 = EDGE_LOOP ( 'NONE', ( #82610, #98648, #177860, #165242, #195985, #129179 ) ) ;
#87648 = CARTESIAN_POINT ( 'NONE',  ( 6.704125975539116489, -1.825092170400946845, 0.04854515157103055090 ) ) ;
#87650 = CARTESIAN_POINT ( 'NONE',  ( 7.344766530301147789, 9.591980256816594164, 1.599625672291281386 ) ) ;
#87651 = AXIS2_PLACEMENT_3D ( 'NONE', #159662, #178055, #110977 ) ;
#87652 = CARTESIAN_POINT ( 'NONE',  ( -0.5368768833858145184, 13.37576698399828246, -1.254641125003840507 ) ) ;
#87653 = PLANE ( 'NONE',  #58462 ) ;
#87654 = DIRECTION ( 'NONE',  ( 1.000000000000000000, -5.391474854832587087E-16, 0.000000000000000000 ) ) ;
#87655 = CARTESIAN_POINT ( 'NONE',  ( 5.463572716182812705, 9.317992568947877530, 0.7216878364870438212 ) ) ;
#87656 = CARTESIAN_POINT ( 'NONE',  ( 0.08225775502835978858, -1.185065876811146834, 1.370160863432666076 ) ) ;
#87657 = CARTESIAN_POINT ( 'NONE',  ( -8.830438121202295321, 9.196599317691152464, -0.7998128361456291469 ) ) ;
#87658 = CARTESIAN_POINT ( 'NONE',  ( 4.873266149108180123, 7.772895376346490970, 1.199719254218462483 ) ) ;
#87659 = CARTESIAN_POINT ( 'NONE',  ( -7.002681350352347067, -8.176227052203543622, 6.455298931196943535 ) ) ;
#87660 = DIRECTION ( 'NONE',  ( 3.209122457311483071E-14, 0.6299249119529743979, 0.7766560405359875796 ) ) ;
#87661 = CARTESIAN_POINT ( 'NONE',  ( 3.708318708537623021, 4.285125567170706695, -1.199719254218446718 ) ) ;
#87662 = ORIENTED_EDGE ( 'NONE', *, *, #146265, .F. ) ;
#87663 = CARTESIAN_POINT ( 'NONE',  ( 6.345327396762703742, 0.3419173589993273477, -1.987050850726256979 ) ) ;
#87664 = CARTESIAN_POINT ( 'NONE',  ( 0.1707708301344288415, 0.8156354886642532831, 1.957547177562010354 ) ) ;
#87665 = CARTESIAN_POINT ( 'NONE',  ( 0.4205179064188996341, -7.601391327209604134E-15, -1.181179690068133503 ) ) ;
#87666 = CARTESIAN_POINT ( 'NONE',  ( -5.016153647376219382, 6.875265226737464985, 1.443375672974064550 ) ) ;
#87667 = CARTESIAN_POINT ( 'NONE',  ( 3.816783937446950770, 4.411668334231586996, 1.199719254218464037 ) ) ;
#87668 = CARTESIAN_POINT ( 'NONE',  ( 3.485164662121999601, 0.04367138265829079852, 1.969119211374547707 ) ) ;
#87669 = CARTESIAN_POINT ( 'NONE',  ( 4.482046101484723266, -2.016035353076811809, -0.04666016718203602753 ) ) ;
#87670 = CARTESIAN_POINT ( 'NONE',  ( -5.357443255694392725, 9.402100898285455699, 0.000000000000000000 ) ) ;
#87671 = CARTESIAN_POINT ( 'NONE',  ( -10.95632728729436600, -7.911711732698783806, 0.3221646467111946022 ) ) ;
#87672 = CARTESIAN_POINT ( 'NONE',  ( 5.332042502257137606, 2.158596015244533373, 0.3771327725019049670 ) ) ;
#87673 = DIRECTION ( 'NONE',  ( -3.347138415753903010E-16, -0.6000000000000019762, 0.7999999999999986011 ) ) ;
#87674 = CARTESIAN_POINT ( 'NONE',  ( 2.661056112795460837, -1.675086148048400503, -0.9512456543366625272 ) ) ;
#87675 = CARTESIAN_POINT ( 'NONE',  ( -8.345207244411405156, 9.694828859023472134, 1.199719254218462483 ) ) ;
#87676 = CARTESIAN_POINT ( 'NONE',  ( -0.1298852118744100725, 0.003815113116375101580, -1.726395881205537330 ) ) ;
#87677 = CARTESIAN_POINT ( 'NONE',  ( 0.3466626200071438735, 2.201290530325435757, 0.1579762268871589825 ) ) ;
#87678 = ORIENTED_EDGE ( 'NONE', *, *, #188204, .T. ) ;
#87679 = CARTESIAN_POINT ( 'NONE',  ( 5.072158865288243668, 6.050511776658669127, 1.082531754730549078 ) ) ;
#87680 = CARTESIAN_POINT ( 'NONE',  ( 4.750814831274846384, -0.4274863908861815665, -1.922328355476431216 ) ) ;
#87682 = CARTESIAN_POINT ( 'NONE',  ( 3.844392992367959838, 1.075074360472785928, -1.701806764060603161 ) ) ;
#87681 = CARTESIAN_POINT ( 'NONE',  ( 0.06387186515662347797, -1.267698835582967476, 1.471343342715900615 ) ) ;
#87683 = CARTESIAN_POINT ( 'NONE',  ( 5.167441833834662823, -0.7673274391166631236, -2.166651051963175423 ) ) ;
#87684 = CARTESIAN_POINT ( 'NONE',  ( 3.203785720953303606, 0.6742969627455961401, -1.734658892920079243 ) ) ;
#87685 = CARTESIAN_POINT ( 'NONE',  ( 6.200875153403774043, 8.327716660428123419, -1.599625672291283607 ) ) ;
#87686 = CARTESIAN_POINT ( 'NONE',  ( 2.310781476690497271, 5.467761476598782977, -0.5169845646830224517 ) ) ;
#87687 =( LENGTH_UNIT ( ) NAMED_UNIT ( * ) SI_UNIT ( .MILLI., .METRE. ) );
#87688 = CARTESIAN_POINT ( 'NONE',  ( -6.205881626753225966, 8.263281202677319470, 1.599625672291283607 ) ) ;
#87689 = CARTESIAN_POINT ( 'NONE',  ( -3.824808732831001201, 7.476377598362539345, 0.7216878364870338292 ) ) ;
#87690 = CARTESIAN_POINT ( 'NONE',  ( 6.163634092203726489, 1.075319730316869560, 1.792882302630414593 ) ) ;
#87691 = CARTESIAN_POINT ( 'NONE',  ( 4.961921032921539521, 7.772363057508363759, -1.082531754730549078 ) ) ;
#87692 = ORIENTED_EDGE ( 'NONE', *, *, #122759, .F. ) ;
#87693 = CARTESIAN_POINT ( 'NONE',  ( -0.09185872022810087634, 6.492156809554922248, 3.106929658804562067 ) ) ;
#87694 = CARTESIAN_POINT ( 'NONE',  ( -1.138412281109779656E-15, -7.256398209935981392, -9.569423160902221781 ) ) ;
#87695 = CARTESIAN_POINT ( 'NONE',  ( 0.7854531640391904102, 1.224056292049885419, 1.354719642434290439 ) ) ;
#87696 = CARTESIAN_POINT ( 'NONE',  ( -6.112028321662274166, 6.025121218227761588, 0.7998128361456341429 ) ) ;
#87697 = STYLED_ITEM ( 'NONE', ( #24308 ), #66162 ) ;
#87698 = CARTESIAN_POINT ( 'NONE',  ( 2.302961303058923992, 1.131868135402936737, -1.313931383173136513 ) ) ;
#87699 = FILL_AREA_STYLE ('',( #170006 ) ) ;
#87700 = CARTESIAN_POINT ( 'NONE',  ( -11.89942855770814134, 11.29999999999999893, 0.6999999999999992895 ) ) ;
#87701 = CARTESIAN_POINT ( 'NONE',  ( -4.394814349124112951, 8.279033840620114049, -0.7998128361456281477 ) ) ;
#87702 = CARTESIAN_POINT ( 'NONE',  ( 0.000000000000000000, -8.407420853759283830, 10.91970695577495931 ) ) ;
#87704 = AXIS2_PLACEMENT_3D ( 'NONE', #139016, #203962, #39360 ) ;
#87703 = CARTESIAN_POINT ( 'NONE',  ( 6.977413708759169886, -0.1587332643391472231, 2.136494379638858909 ) ) ;
#87705 = CARTESIAN_POINT ( 'NONE',  ( 5.865807274569020180, 1.797851641234180509, -0.3166982042408575948 ) ) ;
#87706 = CARTESIAN_POINT ( 'NONE',  ( 3.520314338623427020, 0.8779579967637550775, 1.754372790864023646 ) ) ;
#87707 = CARTESIAN_POINT ( 'NONE',  ( 1.224999999999963896, -0.5624999993172064006, -2.428612866367529932E-14 ) ) ;
#87708 = CARTESIAN_POINT ( 'NONE',  ( -10.01677656239806247, 10.58066083241955901, 0.7998128361456462443 ) ) ;
#87709 = CARTESIAN_POINT ( 'NONE',  ( 5.991813822235618758, 9.077867661661846554, 1.199719254218462483 ) ) ;
#87710 = EDGE_CURVE ( 'NONE', #177025, #73290, #197845, .T. ) ;
#87711 = CARTESIAN_POINT ( 'NONE',  ( 4.055424778641623540, -1.844328037693225397, 1.046277804987456372 ) ) ;
#87712 = CARTESIAN_POINT ( 'NONE',  ( 6.827182134110222123, 4.687887262399931920, 2.751577338787388083 ) ) ;
#87713 = CARTESIAN_POINT ( 'NONE',  ( -9.484092147959342967, 11.02352791316275216, 1.199719254218462483 ) ) ;
#87714 = AXIS2_PLACEMENT_3D ( 'NONE', #159997, #110249, #111315 ) ;
#87715 = CARTESIAN_POINT ( 'NONE',  ( 2.272408084759574454, -0.9721198248324285363, -1.827787434591138238 ) ) ;
#87716 = CARTESIAN_POINT ( 'NONE',  ( 1.499999999999993117, 14.88541666734946567, 0.8660254037844409281 ) ) ;
#87718 = ORIENTED_EDGE ( 'NONE', *, *, #167500, .T. ) ;
#87717 = CARTESIAN_POINT ( 'NONE',  ( 5.057398377711723292, -1.905748072847958108, 1.140992067822230505 ) ) ;
#87719 = CARTESIAN_POINT ( 'NONE',  ( 1.934640009471942035, -1.849324232932574530, -1.365145410983016117 ) ) ;
#87720 = CARTESIAN_POINT ( 'NONE',  ( 8.703971430293332645, 12.13808852110884118, -1.082531754730543083 ) ) ;
#87722 = CARTESIAN_POINT ( 'NONE',  ( 1.642778471875000035, -4.076041666188710444, -2.845375778867859751 ) ) ;
#87721 = CARTESIAN_POINT ( 'NONE',  ( 7.512626515748113576, 7.937354821227203594, 0.7216878364870267237 ) ) ;
#87723 = DIRECTION ( 'NONE',  ( 0.000000000000000000, 0.000000000000000000, -1.000000000000000000 ) ) ;
#87724 = DIRECTION ( 'NONE',  ( 0.000000000000000000, 0.000000000000000000, -1.000000000000000000 ) ) ;
#87725 = ORIENTED_EDGE ( 'NONE', *, *, #95039, .F. ) ;
#87726 = CARTESIAN_POINT ( 'NONE',  ( -0.3641668253325896498, -9.063144096568910513, 9.630238394150005377 ) ) ;
#87727 = CARTESIAN_POINT ( 'NONE',  ( 2.636851627972558454, 1.802111047976437508, 0.6404684511054498097 ) ) ;
#87728 = CARTESIAN_POINT ( 'NONE',  ( -0.09252986280859777646, 7.021014873011406365, -3.994686497348480803 ) ) ;
#87729 = CARTESIAN_POINT ( 'NONE',  ( 4.471539400256457242, 1.672567520934200136, -0.4206060815013599741 ) ) ;
#87730 = CARTESIAN_POINT ( 'NONE',  ( 2.342982756445275427, -1.756855002775299379, -0.9896843009072552322 ) ) ;
#87731 = CARTESIAN_POINT ( 'NONE',  ( 4.166792231569245608, 1.501215554499458982, 1.740835934941728169 ) ) ;
#87732 = CARTESIAN_POINT ( 'NONE',  ( 3.356942810317259163, -1.715728140842260441, 1.474839417774987060 ) ) ;
#87733 = CARTESIAN_POINT ( 'NONE',  ( 5.848290838822029158, 2.103586024953810085, 0.1047431163101186502 ) ) ;
#87734 = CARTESIAN_POINT ( 'NONE',  ( -5.641601317062247212, 7.675230518029648508, -1.443375672974066548 ) ) ;
#87735 = CARTESIAN_POINT ( 'NONE',  ( 4.411239408862893008, -0.3036837672792407905, 1.743313046103856179 ) ) ;
#87737 = CARTESIAN_POINT ( 'NONE',  ( 0.9906304909971673789, -0.5616109214932778482, -2.222291424677411698 ) ) ;
#87736 = CARTESIAN_POINT ( 'NONE',  ( 6.363572996767764778, 8.517530811019446091, -1.599625672291283607 ) ) ;
#87738 = CARTESIAN_POINT ( 'NONE',  ( 6.193280126971262511, -0.6156851667328180344, 1.735278506779000640 ) ) ;
#87739 = CARTESIAN_POINT ( 'NONE',  ( -5.271422797614987665, 5.044414773505913274, -0.7998128361456221525 ) ) ;
#87740 = CARTESIAN_POINT ( 'NONE',  ( 5.666036703420031628, -1.392593631063457682, 1.692088878451535106 ) ) ;
#87741 = CARTESIAN_POINT ( 'NONE',  ( -6.317173229324657413, 6.334733287159020954, 0.000000000000000000 ) ) ;
#87742 = CARTESIAN_POINT ( 'NONE',  ( 1.360316468749955821, -0.9531249996585916540, -5.204170427930421283E-14 ) ) ;
#87743 = CARTESIAN_POINT ( 'NONE',  ( 3.947215336577725164, 7.320702380770685025, -0.8969922371624715618 ) ) ;
#87744 = CARTESIAN_POINT ( 'NONE',  ( 5.547352688424546763, 1.827615396715172258, -0.9727077141251788683 ) ) ;
#87745 = CARTESIAN_POINT ( 'NONE',  ( 1.622280145275534435, 1.995268681201247452, 0.2910785328335343536 ) ) ;
#87746 = CARTESIAN_POINT ( 'NONE',  ( 1.499999999999985123, -1.172916665983846363, -0.8660254037844323793 ) ) ;
#87747 = CARTESIAN_POINT ( 'NONE',  ( 4.037660154168158932, -1.329308714249255452, -1.394617731102282709 ) ) ;
#87748 = CARTESIAN_POINT ( 'NONE',  ( 1.364683531249997417, 10.73437500034139802, 2.602085213965210642E-15 ) ) ;
#87749 = CARTESIAN_POINT ( 'NONE',  ( 1.547463978342083157, 0.2240547868478468541, 2.210115929984892258 ) ) ;
#87751 = ORIENTED_EDGE ( 'NONE', *, *, #6325, .T. ) ;
#87750 = LINE ( 'NONE', #74706, #105964 ) ;
#87753 = CARTESIAN_POINT ( 'NONE',  ( -1.150196859685111317, 3.270291321728038714, 0.7750000000000083489 ) ) ;
#87752 = CARTESIAN_POINT ( 'NONE',  ( 1.490514837427000527, 7.209629588552902035, -4.246172784737240136 ) ) ;
#87754 = DIRECTION ( 'NONE',  ( -0.000000000000000000, 1.000000000000000000, -0.000000000000000000 ) ) ;
#87756 = EDGE_CURVE ( 'NONE', #23490, #163746, #150598, .T. ) ;
#87755 = CARTESIAN_POINT ( 'NONE',  ( 2.706824224222692088, 6.309712028235118453, 0.7998128361456362523 ) ) ;
#87757 = DIRECTION ( 'NONE',  ( 0.000000000000000000, -0.000000000000000000, 1.000000000000000000 ) ) ;
#87758 = DIRECTION ( 'NONE',  ( 2.949029909160572061E-17, 1.000000000000000000, -8.673600428462541149E-15 ) ) ;
#87759 = CARTESIAN_POINT ( 'NONE',  ( 4.581465296696157097, -0.8148697087324536792, 1.537882137665383064 ) ) ;
#87760 = CARTESIAN_POINT ( 'NONE',  ( 2.066782613880484565, 1.455849762852476248, -1.315278764014264912 ) ) ;
#87762 = CARTESIAN_POINT ( 'NONE',  ( 1.364683531249990311, 2.946875000341416140, 1.214306433183764966E-14 ) ) ;
#87761 = CARTESIAN_POINT ( 'NONE',  ( 6.010342169559767633, 5.906487374108181143, -0.7998128361456281477 ) ) ;
#87763 = CARTESIAN_POINT ( 'NONE',  ( -4.397013243575890407, 7.155424720373004810, 1.066431095959238462 ) ) ;
#87764 = CARTESIAN_POINT ( 'NONE',  ( -1.737499999999997824, -1.997916665710752770, 3.009438278150925683 ) ) ;
#87765 = CARTESIAN_POINT ( 'NONE',  ( 6.707479306934847507, -1.574971382793718178, -1.169550641929931079 ) ) ;
#87766 = CARTESIAN_POINT ( 'NONE',  ( -9.643927338022246332, 10.14567007064778004, -0.7998128361456291469 ) ) ;
#87767 = CARTESIAN_POINT ( 'NONE',  ( -5.273758565591545988, 6.215435083687305351, 1.082531754730546636 ) ) ;
#87768 = CARTESIAN_POINT ( 'NONE',  ( 5.243375144629232487, 0.3886363430659239837, -1.978554426619572926 ) ) ;
#87769 = CARTESIAN_POINT ( 'NONE',  ( 1.657462679512666348, -1.941143012291703940, -1.162103002166763988 ) ) ;
#87771 = ORIENTED_EDGE ( 'NONE', *, *, #172633, .T. ) ;
#87770 = CARTESIAN_POINT ( 'NONE',  ( -6.579784621333750749, 6.570836901177822931, 0.7998128361456341429 ) ) ;
#87773 = EDGE_CURVE ( 'NONE', #120419, #183827, #159103, .T. ) ;
#87772 = CARTESIAN_POINT ( 'NONE',  ( -1.364683531250010295, 5.738541667008088432, -0.7879004041258300672 ) ) ;
#87774 = CARTESIAN_POINT ( 'NONE',  ( 1.422894040683621464, -0.05142188859055819850, 1.870020055627517497 ) ) ;
#87775 = CARTESIAN_POINT ( 'NONE',  ( 0.4922575064417636925, -1.726078246012904938, 0.1672019070194027679 ) ) ;
#87776 = AXIS2_PLACEMENT_3D ( 'NONE', #108622, #56611, #122775 ) ;
#87778 = CARTESIAN_POINT ( 'NONE',  ( 4.476244563333130699, -2.125884358948509689, -0.5320566845071761364 ) ) ;
#87777 = CARTESIAN_POINT ( 'NONE',  ( -0.6801582343750368631, 1.682291667008048552, 1.178068619123803451 ) ) ;
#87779 = CARTESIAN_POINT ( 'NONE',  ( 6.036188935239226616, 1.144513723677667461, -2.003705632283636184 ) ) ;
#87780 = CARTESIAN_POINT ( 'NONE',  ( 0.07516593201271813685, 0.0004601587237540622779, -2.044269526395313452 ) ) ;
#87781 = CARTESIAN_POINT ( 'NONE',  ( 2.941277052067638120, 0.6983745205926906729, -1.812199837690719129 ) ) ;
#87782 = CARTESIAN_POINT ( 'NONE',  ( -4.406036734316882253, 8.084200590104265061, -0.7216878364870257245 ) ) ;
#87783 = EDGE_CURVE ( 'NONE', #79633, #120384, #65828, .T. ) ;
#87784 = CARTESIAN_POINT ( 'NONE',  ( 10.48884024596648601, 1.000000000000000888, -5.608780650328974104 ) ) ;
#87785 = CARTESIAN_POINT ( 'NONE',  ( 3.431622278034673901, 7.017660067766835930, -1.734723475976807094E-15 ) ) ;
#87786 =( NAMED_UNIT ( * ) PLANE_ANGLE_UNIT ( ) SI_UNIT ( $, .RADIAN. ) );
#87787 = CARTESIAN_POINT ( 'NONE',  ( 3.059220373557011818, -1.198860207862334049, 1.621182619130703051 ) ) ;
#87788 = CARTESIAN_POINT ( 'NONE',  ( -3.402733366905605905, 6.913679994791092298, 0.7216878364870317197 ) ) ;
#87789 = CARTESIAN_POINT ( 'NONE',  ( -4.606738333593328072, 8.596554832492683929, 0.7998128361456281477 ) ) ;
#87790 = CARTESIAN_POINT ( 'NONE',  ( 9.097684769969825780, 10.57271930550834860, -1.199719254218446718 ) ) ;
#87792 = CARTESIAN_POINT ( 'NONE',  ( -10.43059486372414568, 5.377696206510353072, -5.769669902936525929 ) ) ;
#87791 = CARTESIAN_POINT ( 'NONE',  ( 1.154616158753757338, -1.440623569337009968, 1.121372061650728558 ) ) ;
#87793 = CARTESIAN_POINT ( 'NONE',  ( -5.743814354044916470, 6.730146830254374990, -1.199719254218453823 ) ) ;
#87794 = CARTESIAN_POINT ( 'NONE',  ( -4.522526758610270647, 7.433975764090723359, -1.199719254218453823 ) ) ;
#87795 = CARTESIAN_POINT ( 'NONE',  ( -9.510677803526956353, 3.006766436585398772, 6.782528980676592489 ) ) ;
#87796 = ORIENTED_EDGE ( 'NONE', *, *, #98243, .T. ) ;
#87797 = CARTESIAN_POINT ( 'NONE',  ( 0.2511322555047851290, -1.735185354305257110, 1.289038484408123963 ) ) ;
#87798 = CARTESIAN_POINT ( 'NONE',  ( -5.438229012412888252, 9.358701257874761481, -0.7216878364870338292 ) ) ;
#87799 = UNCERTAINTY_MEASURE_WITH_UNIT (LENGTH_MEASURE( 1.000000000000000082E-05 ), #61778, 'distance_accuracy_value', 'NONE');
#87800 = CARTESIAN_POINT ( 'NONE',  ( 4.582292731738905722, 5.408724944192588424, -1.082531754730548412 ) ) ;
#87801 = CARTESIAN_POINT ( 'NONE',  ( -4.274898507010545856, 3.881803101134051470, -0.7998128361456221525 ) ) ;
#87802 = CARTESIAN_POINT ( 'NONE',  ( -10.47097470845587175, 11.11055866948701443, 1.040834085586084257E-14 ) ) ;
#87803 = CARTESIAN_POINT ( 'NONE',  ( 5.391273274344085209, -0.05166147132495273880, -2.019192591660509351 ) ) ;
#87805 = ORIENTED_EDGE ( 'NONE', *, *, #18607, .F. ) ;
#87804 = CARTESIAN_POINT ( 'NONE',  ( 5.883471028171038952, 0.1659795297097066691, -2.215133764073994982 ) ) ;
#87806 = CARTESIAN_POINT ( 'NONE',  ( -5.887983850084758330, 10.09134126839936840, 0.7998128361456291469 ) ) ;
#87807 = CARTESIAN_POINT ( 'NONE',  ( 5.296431564432884542, 9.330920591813708143, 1.040834085586084257E-14 ) ) ;
#87808 = CARTESIAN_POINT ( 'NONE',  ( 5.612203307022772591, -0.9243832361092527705, -1.842014774801424615 ) ) ;
#87809 = CARTESIAN_POINT ( 'NONE',  ( 3.639296212489909532, 0.7283784247123015199, 1.880435045658496618 ) ) ;
#87810 = EDGE_LOOP ( 'NONE', ( #210453, #94622, #4493, #87805 ) ) ;
#87811 =( BOUNDED_SURFACE ( )  B_SPLINE_SURFACE ( 1, 2, ( 
 ( #84595, #166923, #149599, #170103, #118230, #87801, #153874, #203651, #186349, #55302, #150683, #1185, #135493, #37984, #5443, #36901, #53164, #67249, #69385, #101915, #2244, #35837, #104057, #133384, #71522, #199389, #167981, #117158, #19586, #119292, #102983, #86727, #136563, #202584, #126785, #60623, #156004, #208987, #175462, #142987, #92091, #7591, #125713, #206867, #27047, #76867, #24915, #174406, #25983, #93155, #122530, #91019, #6522, #9737, #140854, #207932, #188491, #158145, #73675, #139774, #40123, #205801, #154938, #23846, #89953, #106233, #157081, #172258, #57432, #123593, #192741, #189558, #44396, #41204, #171177, #59554, #22768, #88884, #107311, #72599, #173335, #138699, #204717, #56366, #58498, #8669, #43336, #74752, #124654, #75812, #190610, #141921, #191674, #42269, #108381, #109456, #159193, #10793, #127866, #179725, #61697, #213260, #114776, #111581, #79003, #177590, #112650, #194891, #193816, #47607, #97419, #30270, #176517, #62750, #28129, #15055, #82200, #198083, #65925, #132072, #29203, #164530, #64887, #178659, #131033, #46529, #16117, #81147, #94225, #110517, #95293, #147232, #31344, #160263, #148293, #80072, #161342, #197023, #214291, #12924, #163473, #45464, #48660, #180774, #212190, #162411, #96356, #11865, #32400, #145120, #98466, #211126, #77942, #144063, #128910, #13988, #146175, #63828, #129986, #195974, #113721, #210058, #183970, #115839, #1994, #181825, #168791, #21445, #137382, #5193, #71268, #182903, #103808, #4130, #51857, #152544, #134195, #169857, #20397, #33458, #49710, #50776, #86480, #119041, #202333, #186099, #87553, #70199, #153622, #66994, #99534, #167729, #136312, #53983, #3062, #19330, #165595, #117979, #200204, #116904, #199131, #120121, #17186, #37729, #83261, #34520, #149347, #927, #101661, #133132, #100592, #69132, #166667, #18258, #84341, #150429, #68059, #35582, #85408, #185025, #151493, #135254, #201268, #52908, #36650, #102736, #206620, #58249, #207689, #154686, #57184, #38799, #42025, #173082, #25733, #6270, #190363, #39874, #105984, #72341, #172006, #187171, #56119, #122276, #138447, #123346, #204465, #188234, #23596, #158952, #89705, #26804, #155755, #10547, #91844, #92906, #109207, #7340, #76621, #73417, #203398, #124405, #59308, #139520, #189312, #104880, #108134, #24663, #157901, #205546, #174162, #40950, #107057, #90770, #156831, #170923, #8418, #74504, #140608, #9495, #75567, #141677, #125465, #55051, #191427, #121201, #43094, #22520, #175219, #88630, #48417, #193575, #32145, #28950, #180523, #208743, #114529, #112397, #143811, #14806, #98225, #45218, #195718, #77690, #47353, #97169, #30019, #194638, #210880, #126533, #63578, #160016, #211943, #93975, #31097, #146987, #209808, #111333, #61443, #144873, #12674, #11616, #79819, #129735, #62505, #60370, #95034, #192494, #113468, #164277, #15867, #142734, #44146, #127610, #196774, #163224, #128670, #80897, #78750, #110267, #179473, #176276, #27878, #177337, #213005, #64641, #130781, #161084, #46281, #178408, #96104, #162159, #13746, #145931, #36392, #86220, #35322, #199954, #81952, #150172, #166402, #83009, #16929, #118780, #197828, #3865, #37464, #149084, #49460, #136050, #133946, #33204, #148037, #101400, #102470, #103542, #185833, #66729, #119855, #152291, #53722, #2804, #132873, #168536, #117725, #69939, #202062, #1739, #85150, #214045, #50523, #663, #115580, #19070, #198876, #20134, #65672, #181574, #116646, #182642, #99287, #131819, #169603, #34263, #165335, #67797, #68876, #184766, #100336, #17994, #84083, #51600, #183714, #134996, #201006, #167475, #151235, #52651, #23330, #74246, #204196, #8162, #55851, #205283, #194114, #87288, #187974, #54789, #153357, #75306, #41763, #24391, #107876, #4928, #120935, #89438, #157636, #137117, #90503, #21186, #128154, #71004, #203146, #61998, #172819, #156567, #186908, #106791, #140340, #38540, #111882, #104617, #155490, #56921, #170665, #22252, #141422, #88362, #123094, #154428, #6006, #173902, #206358, #72076, #124148, #45764, #73145, #207428, #138187, #57985, #9234, #40688, #122008, #190110, #105704, #7073, #39601, #25477, #91584, #171732, #139251 ),
 ( #189051, #30573, #129222, #148, #145424, #79308, #29499, #83558, #98765, #31636, #51072, #146469, #96654, #14279, #212488, #80374, #161640, #130273, #195196, #131319, #149640, #163771, #65164, #46833, #67284, #162707, #181067, #112946, #64130, #116128, #197312, #66214, #99823, #13235, #15349, #132362, #196262, #47909, #178958, #198364, #211425, #63055, #95591, #1222, #164821, #97713, #177886, #114019, #180015, #81442, #147520, #213541, #48953, #115071, #32685, #16412, #133423, #82492, #148579, #50004, #182115, #33745, #165889, #17474, #199429, #117197, #18553, #85693, #184249, #68357, #183195, #55335, #151781, #34801, #185318, #104093, #153909, #138734, #3354, #52137, #171210, #86766, #170142, #21728, #69424, #100876, #101951, #119331, #87838, #135530, #5479, #201554, #152837, #72637, #166963, #53200, #150721, #84630, #22804, #137667, #120410, #203689, #2281, #134490, #36940, #39087, #200493, #186385, #118265, #6557, #35876, #168018, #154972, #54273, #38022, #19621, #202623, #71559, #103022, #204752, #169077, #20676, #4412, #70483, #136599, #88918, #121487, #187459, #105173, #89986, #143023, #175497, #156037, #159224, #11899, #108419, #110549, #107346, #93193, #44432, #75846, #77973, #141953, #140888, #124686, #28161, #207965, #27085, #157115, #7626, #173368, #40157, #8704, #73711, #9773, #94257, #42304, #56403, #24952, #205837, #172292, #59591, #91054, #10825, #122564, #23880, #74788, #123629, #139809, #188526, #209018, #206900, #106270, #190644, #43368, #76899, #144096, #58531, #57470, #176551, #26017, #109490, #60654, #174441, #189593, #41239, #92128, #126817, #158180, #192773, #125748, #191710, #160296, #61730, #162440, #29235, #127898, #49739, #16144, #213288, #82229, #193849, #95327, #63857, #132100, #111615, #64914, #210091, #99560, #45499, #177627, #33488, #147256, #131063, #161376, #81177, #197051, #12959, #83289, #79037, #212222, #31371, #145152, #211158, #115866, #62782, #97447, #128945, #194923, #148320, #114804, #46560, #98495, #165625, #47638, #181851, #112680, #32429, #198109, #15087, #17213, #48689, #80102, #130013, #178690, #180803, #164559, #96389, #30303, #163503, #14016, #146206, #196004, #214319, #113750, #179754, #65951, #102764, #186125, #71294, #199160, #135279, #103832, #51883, #2020, #100619, #37759, #116933, #50805, #957, #55080, #70228, #3088, #22551, #118006, #68089, #200233, #183995, #149374, #69159, #136339, #169880, #170952, #35609, #84371, #203425, #119070, #202359, #54009, #101687, #67023, #134223, #151520, #120148, #167756, #21470, #19355, #185051, #104911, #133159, #85435, #182932, #34548, #121229, #87579, #152570, #153650, #166694, #18285, #201293, #137406, #150459, #4157, #52934, #38827, #36676, #168819, #187199, #86505, #5219, #20423, #174191, #91875, #138473, #176306, #204495, #90797, #124436, #56145, #188264, #208772, #89736, #190394, #39904, #122306, #175248, #207719, #106013, #191459, #44178, #140634, #142767, #139550, #125496, #76652, #108164, #110298, #25763, #173113, #156861, #60402, #157931, #59342, #189341, #172035, #42052, #23628, #192524, #155785, #9524, #7369, #73446, #26834, #75596, #43124, #10578, #205577, #74534, #109238, #57214, #123374, #40980, #92937, #107091, #24694, #154717, #126564, #141708, #8447, #88657, #206647, #58280, #158981, #6298, #72373, #11649, #194666, #193604, #195748, #214075, #13776, #27909, #210909, #177368, #143843, #179505, #78780, #196804, #94006, #209837, #62536, #95068, #45246, #160045, #180554, #128698, #64668, #49489, #46311, #28982, #81981, #211970, #80925, #14835, #112427, #77721, #12703, #30047, #147016, #178441, #213039, #96137, #63609, #197857, #61474, #162189, #127639, #111363, #148069, #48447, #31126, #114561, #161116, #144901, #79851, #164309, #145960, #97200, #129765, #131849, #47385, #113498, #65701, #163253, #130814, #32175, #98252, #15897, #115610, #54822, #83040, #183745, #2835, #149114, #66760, #87319, #182671, #68904, #132901, #695, #53754, #86250, #198906, #69969, #137150, #19101, #21216, #18026, #3897, #169633, #201037, #203177, #52680, #51630, #35355, #153387, #118811, #152320, #67828, #50551, #135023 ) ),
 .UNSPECIFIED., .F., .F., .T. ) 
 B_SPLINE_SURFACE_WITH_KNOTS ( ( 2, 2 ),
 ( 3, 2, 2, 2, 2, 2, 2, 2, 2, 2, 2, 2, 2, 2, 2, 2, 2, 2, 2, 2, 2, 2, 2, 2, 2, 2, 2, 2, 2, 2, 2, 2, 2, 2, 2, 2, 2, 2, 2, 2, 2, 2, 2, 2, 2, 2, 2, 2, 2, 2, 2, 2, 2, 2, 2, 2, 2, 2, 2, 2, 2, 2, 2, 2, 2, 2, 2, 2, 2, 2, 2, 2, 2, 2, 2, 2, 2, 2, 2, 2, 2, 2, 2, 2, 2, 2, 2, 2, 2, 2, 2, 2, 2, 2, 2, 2, 2, 2, 2, 2, 2, 2, 2, 2, 2, 2, 2, 2, 2, 2, 2, 2, 2, 2, 2, 2, 2, 2, 2, 2, 2, 2, 2, 2, 2, 2, 2, 2, 2, 2, 2, 2, 2, 2, 2, 2, 2, 2, 2, 2, 2, 2, 2, 2, 2, 2, 2, 2, 2, 2, 2, 2, 2, 2, 2, 2, 2, 2, 2, 2, 2, 2, 2, 2, 2, 2, 2, 2, 2, 2, 2, 2, 2, 2, 2, 2, 2, 2, 2, 2, 2, 2, 2, 2, 2, 2, 2, 2, 2, 2, 2, 2, 2, 2, 2, 2, 2, 2, 2, 2, 2, 2, 2, 2, 2, 2, 2, 2, 2, 2, 2, 2, 2, 2, 2, 2, 2, 2, 2, 2, 2, 2, 2, 2, 2, 2, 2, 2, 2, 2, 2, 2, 2, 2, 2, 2, 2, 2, 2, 2, 3 ),
 ( 0.000000000000000000, 1.000000000000000000 ),
 ( 0.000000000000000000, 0.004166666666666666609, 0.008333333333333333218, 0.01250000000000000069, 0.01666666666666666644, 0.02083333333333333218, 0.02500000000000000139, 0.02916666666666666713, 0.03333333333333333287, 0.03749999999999999861, 0.04166666666666666435, 0.04583333333333333010, 0.05000000000000000278, 0.05416666666666666852, 0.05833333333333333426, 0.06250000000000000000, 0.06666666666666666574, 0.07083333333333333148, 0.07499999999999999722, 0.07916666666666666297, 0.08333333333333332871, 0.08749999999999999445, 0.09166666666666666019, 0.09583333333333333981, 0.1000000000000000056, 0.1041666666666666713, 0.1083333333333333370, 0.1125000000000000028, 0.1166666666666666685, 0.1208333333333333343, 0.1250000000000000000, 0.1291666666666666796, 0.1333333333333333315, 0.1375000000000000111, 0.1416666666666666630, 0.1458333333333333426, 0.1499999999999999944, 0.1541666666666666741, 0.1583333333333333259, 0.1625000000000000056, 0.1666666666666666574, 0.1708333333333333370, 0.1749999999999999889, 0.1791666666666666685, 0.1833333333333333204, 0.1875000000000000000, 0.1916666666666666796, 0.1958333333333333315, 0.2000000000000000111, 0.2041666666666666630, 0.2083333333333333426, 0.2124999999999999944, 0.2166666666666666741, 0.2208333333333333259, 0.2250000000000000056, 0.2291666666666666574, 0.2333333333333333370, 0.2374999999999999889, 0.2416666666666666685, 0.2458333333333333204, 0.2500000000000000000, 0.2541666666666666519, 0.2583333333333333592, 0.2625000000000000111, 0.2666666666666666630, 0.2708333333333333148, 0.2750000000000000222, 0.2791666666666666741, 0.2833333333333333259, 0.2874999999999999778, 0.2916666666666666852, 0.2958333333333333370, 0.2999999999999999889, 0.3041666666666666408, 0.3083333333333333481, 0.3125000000000000000, 0.3166666666666666519, 0.3208333333333333592, 0.3250000000000000111, 0.3291666666666666630, 0.3333333333333333148, 0.3375000000000000222, 0.3416666666666666741, 0.3458333333333333259, 0.3499999999999999778, 0.3541666666666666852, 0.3583333333333333370, 0.3624999999999999889, 0.3666666666666666408, 0.3708333333333333481, 0.3750000000000000000, 0.3791666666666666519, 0.3833333333333333592, 0.3875000000000000111, 0.3916666666666666630, 0.3958333333333333148, 0.4000000000000000222, 0.4041666666666666741, 0.4083333333333333259, 0.4124999999999999778, 0.4166666666666666852, 0.4208333333333333370, 0.4249999999999999889, 0.4291666666666666408, 0.4333333333333333481, 0.4375000000000000000, 0.4416666666666666519, 0.4458333333333333592, 0.4500000000000000111, 0.4541666666666666630, 0.4583333333333333148, 0.4625000000000000222, 0.4666666666666666741, 0.4708333333333333259, 0.4749999999999999778, 0.4791666666666666852, 0.4833333333333333370, 0.4874999999999999889, 0.4916666666666666408, 0.4958333333333333481, 0.5000000000000000000, 0.5041666666666666519, 0.5083333333333333037, 0.5124999999999999556, 0.5166666666666667185, 0.5208333333333333703, 0.5250000000000000222, 0.5291666666666666741, 0.5333333333333333259, 0.5374999999999999778, 0.5416666666666666297, 0.5458333333333332815, 0.5500000000000000444, 0.5541666666666666963, 0.5583333333333333481, 0.5625000000000000000, 0.5666666666666666519, 0.5708333333333333037, 0.5749999999999999556, 0.5791666666666667185, 0.5833333333333333703, 0.5875000000000000222, 0.5916666666666666741, 0.5958333333333333259, 0.5999999999999999778, 0.6041666666666666297, 0.6083333333333332815, 0.6125000000000000444, 0.6166666666666666963, 0.6208333333333333481, 0.6250000000000000000, 0.6291666666666666519, 0.6333333333333333037, 0.6374999999999999556, 0.6416666666666667185, 0.6458333333333333703, 0.6500000000000000222, 0.6541666666666666741, 0.6583333333333333259, 0.6624999999999999778, 0.6666666666666666297, 0.6708333333333332815, 0.6750000000000000444, 0.6791666666666666963, 0.6833333333333333481, 0.6875000000000000000, 0.6916666666666666519, 0.6958333333333333037, 0.6999999999999999556, 0.7041666666666667185, 0.7083333333333333703, 0.7125000000000000222, 0.7166666666666666741, 0.7208333333333333259, 0.7249999999999999778, 0.7291666666666666297, 0.7333333333333332815, 0.7375000000000000444, 0.7416666666666666963, 0.7458333333333333481, 0.7500000000000000000, 0.7541666666666666519, 0.7583333333333333037, 0.7624999999999999556, 0.7666666666666667185, 0.7708333333333333703, 0.7750000000000000222, 0.7791666666666666741, 0.7833333333333333259, 0.7874999999999999778, 0.7916666666666666297, 0.7958333333333332815, 0.8000000000000000444, 0.8041666666666666963, 0.8083333333333333481, 0.8125000000000000000, 0.8166666666666666519, 0.8208333333333333037, 0.8249999999999999556, 0.8291666666666667185, 0.8333333333333333703, 0.8375000000000000222, 0.8416666666666666741, 0.8458333333333333259, 0.8499999999999999778, 0.8541666666666666297, 0.8583333333333332815, 0.8625000000000000444, 0.8666666666666666963, 0.8708333333333333481, 0.8750000000000000000, 0.8791666666666666519, 0.8833333333333333037, 0.8874999999999999556, 0.8916666666666667185, 0.8958333333333333703, 0.9000000000000000222, 0.9041666666666666741, 0.9083333333333333259, 0.9124999999999999778, 0.9166666666666666297, 0.9208333333333332815, 0.9250000000000000444, 0.9291666666666666963, 0.9333333333333333481, 0.9375000000000000000, 0.9416666666666666519, 0.9458333333333333037, 0.9499999999999999556, 0.9541666666666667185, 0.9583333333333333703, 0.9625000000000000222, 0.9666666666666666741, 0.9708333333333333259, 0.9749999999999999778, 0.9791666666666666297, 0.9833333333333332815, 0.9875000000000000444, 0.9916666666666666963, 0.9958333333333333481, 1.000000000000000000 ),
 .UNSPECIFIED. ) 
 GEOMETRIC_REPRESENTATION_ITEM ( )  RATIONAL_B_SPLINE_SURFACE ( (
 ( 1.000000000000000000, 0.8660254037844387076, 1.000000000000000000, 0.8660254037844387076, 1.000000000000000000, 0.8660254037844387076, 1.000000000000000000, 0.8660254037844387076, 1.000000000000000000, 0.8660254037844387076, 1.000000000000000000, 0.8660254037844387076, 1.000000000000000000, 0.8660254037844387076, 1.000000000000000000, 0.8660254037844387076, 1.000000000000000000, 0.8660254037844387076, 1.000000000000000000, 0.8660254037844387076, 1.000000000000000000, 0.8660254037844387076, 1.000000000000000000, 0.8660254037844387076, 1.000000000000000000, 0.8660254037844387076, 1.000000000000000000, 0.8660254037844387076, 1.000000000000000000, 0.8660254037844387076, 1.000000000000000000, 0.8660254037844387076, 1.000000000000000000, 0.8660254037844387076, 1.000000000000000000, 0.8660254037844387076, 1.000000000000000000, 0.8660254037844387076, 1.000000000000000000, 0.8660254037844387076, 1.000000000000000000, 0.8660254037844387076, 1.000000000000000000, 0.8660254037844387076, 1.000000000000000000, 0.8660254037844387076, 1.000000000000000000, 0.8660254037844387076, 1.000000000000000000, 0.8660254037844387076, 1.000000000000000000, 0.8660254037844387076, 1.000000000000000000, 0.8660254037844387076, 1.000000000000000000, 0.8660254037844387076, 1.000000000000000000, 0.8660254037844387076, 1.000000000000000000, 0.8660254037844387076, 1.000000000000000000, 0.8660254037844387076, 1.000000000000000000, 0.8660254037844387076, 1.000000000000000000, 0.8660254037844387076, 1.000000000000000000, 0.8660254037844387076, 1.000000000000000000, 0.8660254037844387076, 1.000000000000000000, 0.8660254037844387076, 1.000000000000000000, 0.8660254037844387076, 1.000000000000000000, 0.8660254037844387076, 1.000000000000000000, 0.8660254037844387076, 1.000000000000000000, 0.8660254037844387076, 1.000000000000000000, 0.8660254037844387076, 1.000000000000000000, 0.8660254037844387076, 1.000000000000000000, 0.8660254037844387076, 1.000000000000000000, 0.8660254037844387076, 1.000000000000000000, 0.8660254037844387076, 1.000000000000000000, 0.8660254037844387076, 1.000000000000000000, 0.8660254037844387076, 1.000000000000000000, 0.8660254037844387076, 1.000000000000000000, 0.8660254037844387076, 1.000000000000000000, 0.8660254037844387076, 1.000000000000000000, 0.8660254037844387076, 1.000000000000000000, 0.8660254037844387076, 1.000000000000000000, 0.8660254037844387076, 1.000000000000000000, 0.8660254037844387076, 1.000000000000000000, 0.8660254037844387076, 1.000000000000000000, 0.8660254037844387076, 1.000000000000000000, 0.8660254037844387076, 1.000000000000000000, 0.8660254037844387076, 1.000000000000000000, 0.8660254037844387076, 1.000000000000000000, 0.8660254037844387076, 1.000000000000000000, 0.8660254037844387076, 1.000000000000000000, 0.8660254037844387076, 1.000000000000000000, 0.8660254037844387076, 1.000000000000000000, 0.8660254037844387076, 1.000000000000000000, 0.8660254037844387076, 1.000000000000000000, 0.8660254037844387076, 1.000000000000000000, 0.8660254037844387076, 1.000000000000000000, 0.8660254037844387076, 1.000000000000000000, 0.8660254037844387076, 1.000000000000000000, 0.8660254037844387076, 1.000000000000000000, 0.8660254037844387076, 1.000000000000000000, 0.8660254037844387076, 1.000000000000000000, 0.8660254037844387076, 1.000000000000000000, 0.8660254037844387076, 1.000000000000000000, 0.8660254037844387076, 1.000000000000000000, 0.8660254037844387076, 1.000000000000000000, 0.8660254037844387076, 1.000000000000000000, 0.8660254037844387076, 1.000000000000000000, 0.8660254037844387076, 1.000000000000000000, 0.8660254037844387076, 1.000000000000000000, 0.8660254037844387076, 1.000000000000000000, 0.8660254037844387076, 1.000000000000000000, 0.8660254037844387076, 1.000000000000000000, 0.8660254037844387076, 1.000000000000000000, 0.8660254037844387076, 1.000000000000000000, 0.8660254037844387076, 1.000000000000000000, 0.8660254037844387076, 1.000000000000000000, 0.8660254037844387076, 1.000000000000000000, 0.8660254037844387076, 1.000000000000000000, 0.8660254037844387076, 1.000000000000000000, 0.8660254037844387076, 1.000000000000000000, 0.8660254037844387076, 1.000000000000000000, 0.8660254037844387076, 1.000000000000000000, 0.8660254037844387076, 1.000000000000000000, 0.8660254037844387076, 1.000000000000000000, 0.8660254037844387076, 1.000000000000000000, 0.8660254037844387076, 1.000000000000000000, 0.8660254037844387076, 1.000000000000000000, 0.8660254037844387076, 1.000000000000000000, 0.8660254037844387076, 1.000000000000000000, 0.8660254037844387076, 1.000000000000000000, 0.8660254037844387076, 1.000000000000000000, 0.8660254037844387076, 1.000000000000000000, 0.8660254037844387076, 1.000000000000000000, 0.8660254037844387076, 1.000000000000000000, 0.8660254037844387076, 1.000000000000000000, 0.8660254037844387076, 1.000000000000000000, 0.8660254037844387076, 1.000000000000000000, 0.8660254037844387076, 1.000000000000000000, 0.8660254037844387076, 1.000000000000000000, 0.8660254037844387076, 1.000000000000000000, 0.8660254037844387076, 1.000000000000000000, 0.8660254037844387076, 1.000000000000000000, 0.8660254037844387076, 1.000000000000000000, 0.8660254037844387076, 1.000000000000000000, 0.8660254037844387076, 1.000000000000000000, 0.8660254037844387076, 1.000000000000000000, 0.8660254037844387076, 1.000000000000000000, 0.8660254037844387076, 1.000000000000000000, 0.8660254037844387076, 1.000000000000000000, 0.8660254037844387076, 1.000000000000000000, 0.8660254037844387076, 1.000000000000000000, 0.8660254037844387076, 1.000000000000000000, 0.8660254037844387076, 1.000000000000000000, 0.8660254037844387076, 1.000000000000000000, 0.8660254037844387076, 1.000000000000000000, 0.8660254037844387076, 1.000000000000000000, 0.8660254037844387076, 1.000000000000000000, 0.8660254037844387076, 1.000000000000000000, 0.8660254037844387076, 1.000000000000000000, 0.8660254037844387076, 1.000000000000000000, 0.8660254037844387076, 1.000000000000000000, 0.8660254037844387076, 1.000000000000000000, 0.8660254037844387076, 1.000000000000000000, 0.8660254037844387076, 1.000000000000000000, 0.8660254037844387076, 1.000000000000000000, 0.8660254037844387076, 1.000000000000000000, 0.8660254037844387076, 1.000000000000000000, 0.8660254037844387076, 1.000000000000000000, 0.8660254037844387076, 1.000000000000000000, 0.8660254037844387076, 1.000000000000000000, 0.8660254037844387076, 1.000000000000000000, 0.8660254037844387076, 1.000000000000000000, 0.8660254037844387076, 1.000000000000000000, 0.8660254037844387076, 1.000000000000000000, 0.8660254037844387076, 1.000000000000000000, 0.8660254037844387076, 1.000000000000000000, 0.8660254037844387076, 1.000000000000000000, 0.8660254037844387076, 1.000000000000000000, 0.8660254037844387076, 1.000000000000000000, 0.8660254037844387076, 1.000000000000000000, 0.8660254037844387076, 1.000000000000000000, 0.8660254037844387076, 1.000000000000000000, 0.8660254037844387076, 1.000000000000000000, 0.8660254037844387076, 1.000000000000000000, 0.8660254037844387076, 1.000000000000000000, 0.8660254037844387076, 1.000000000000000000, 0.8660254037844387076, 1.000000000000000000, 0.8660254037844387076, 1.000000000000000000, 0.8660254037844387076, 1.000000000000000000, 0.8660254037844387076, 1.000000000000000000, 0.8660254037844387076, 1.000000000000000000, 0.8660254037844387076, 1.000000000000000000, 0.8660254037844387076, 1.000000000000000000, 0.8660254037844387076, 1.000000000000000000, 0.8660254037844387076, 1.000000000000000000, 0.8660254037844387076, 1.000000000000000000, 0.8660254037844387076, 1.000000000000000000, 0.8660254037844387076, 1.000000000000000000, 0.8660254037844387076, 1.000000000000000000, 0.8660254037844387076, 1.000000000000000000, 0.8660254037844387076, 1.000000000000000000, 0.8660254037844387076, 1.000000000000000000, 0.8660254037844387076, 1.000000000000000000, 0.8660254037844387076, 1.000000000000000000, 0.8660254037844387076, 1.000000000000000000, 0.8660254037844387076, 1.000000000000000000, 0.8660254037844387076, 1.000000000000000000, 0.8660254037844387076, 1.000000000000000000, 0.8660254037844387076, 1.000000000000000000, 0.8660254037844387076, 1.000000000000000000, 0.8660254037844387076, 1.000000000000000000, 0.8660254037844387076, 1.000000000000000000, 0.8660254037844387076, 1.000000000000000000, 0.8660254037844387076, 1.000000000000000000, 0.8660254037844387076, 1.000000000000000000, 0.8660254037844387076, 1.000000000000000000, 0.8660254037844387076, 1.000000000000000000, 0.8660254037844387076, 1.000000000000000000, 0.8660254037844387076, 1.000000000000000000, 0.8660254037844387076, 1.000000000000000000, 0.8660254037844387076, 1.000000000000000000, 0.8660254037844387076, 1.000000000000000000, 0.8660254037844387076, 1.000000000000000000, 0.8660254037844387076, 1.000000000000000000, 0.8660254037844387076, 1.000000000000000000, 0.8660254037844387076, 1.000000000000000000, 0.8660254037844387076, 1.000000000000000000, 0.8660254037844387076, 1.000000000000000000, 0.8660254037844387076, 1.000000000000000000, 0.8660254037844387076, 1.000000000000000000, 0.8660254037844387076, 1.000000000000000000, 0.8660254037844387076, 1.000000000000000000, 0.8660254037844387076, 1.000000000000000000, 0.8660254037844387076, 1.000000000000000000, 0.8660254037844387076, 1.000000000000000000, 0.8660254037844387076, 1.000000000000000000, 0.8660254037844387076, 1.000000000000000000, 0.8660254037844387076, 1.000000000000000000, 0.8660254037844387076, 1.000000000000000000, 0.8660254037844387076, 1.000000000000000000, 0.8660254037844387076, 1.000000000000000000, 0.8660254037844387076, 1.000000000000000000, 0.8660254037844387076, 1.000000000000000000, 0.8660254037844387076, 1.000000000000000000, 0.8660254037844387076, 1.000000000000000000, 0.8660254037844387076, 1.000000000000000000, 0.8660254037844387076, 1.000000000000000000, 0.8660254037844387076, 1.000000000000000000, 0.8660254037844387076, 1.000000000000000000, 0.8660254037844387076, 1.000000000000000000, 0.8660254037844387076, 1.000000000000000000, 0.8660254037844387076, 1.000000000000000000, 0.8660254037844387076, 1.000000000000000000, 0.8660254037844387076, 1.000000000000000000, 0.8660254037844387076, 1.000000000000000000, 0.8660254037844387076, 1.000000000000000000, 0.8660254037844387076, 1.000000000000000000, 0.8660254037844387076, 1.000000000000000000, 0.8660254037844387076, 1.000000000000000000, 0.8660254037844387076, 1.000000000000000000, 0.8660254037844387076, 1.000000000000000000, 0.8660254037844387076, 1.000000000000000000, 0.8660254037844387076, 1.000000000000000000, 0.8660254037844387076, 1.000000000000000000, 0.8660254037844387076, 1.000000000000000000, 0.8660254037844387076, 1.000000000000000000, 0.8660254037844387076, 1.000000000000000000, 0.8660254037844387076, 1.000000000000000000, 0.8660254037844387076, 1.000000000000000000),
 ( 1.000000000000000000, 0.8660254037844387076, 1.000000000000000000, 0.8660254037844387076, 1.000000000000000000, 0.8660254037844387076, 1.000000000000000000, 0.8660254037844387076, 1.000000000000000000, 0.8660254037844387076, 1.000000000000000000, 0.8660254037844387076, 1.000000000000000000, 0.8660254037844387076, 1.000000000000000000, 0.8660254037844387076, 1.000000000000000000, 0.8660254037844387076, 1.000000000000000000, 0.8660254037844387076, 1.000000000000000000, 0.8660254037844387076, 1.000000000000000000, 0.8660254037844387076, 1.000000000000000000, 0.8660254037844387076, 1.000000000000000000, 0.8660254037844387076, 1.000000000000000000, 0.8660254037844387076, 1.000000000000000000, 0.8660254037844387076, 1.000000000000000000, 0.8660254037844387076, 1.000000000000000000, 0.8660254037844387076, 1.000000000000000000, 0.8660254037844387076, 1.000000000000000000, 0.8660254037844387076, 1.000000000000000000, 0.8660254037844387076, 1.000000000000000000, 0.8660254037844387076, 1.000000000000000000, 0.8660254037844387076, 1.000000000000000000, 0.8660254037844387076, 1.000000000000000000, 0.8660254037844387076, 1.000000000000000000, 0.8660254037844387076, 1.000000000000000000, 0.8660254037844387076, 1.000000000000000000, 0.8660254037844387076, 1.000000000000000000, 0.8660254037844387076, 1.000000000000000000, 0.8660254037844387076, 1.000000000000000000, 0.8660254037844387076, 1.000000000000000000, 0.8660254037844387076, 1.000000000000000000, 0.8660254037844387076, 1.000000000000000000, 0.8660254037844387076, 1.000000000000000000, 0.8660254037844387076, 1.000000000000000000, 0.8660254037844387076, 1.000000000000000000, 0.8660254037844387076, 1.000000000000000000, 0.8660254037844387076, 1.000000000000000000, 0.8660254037844387076, 1.000000000000000000, 0.8660254037844387076, 1.000000000000000000, 0.8660254037844387076, 1.000000000000000000, 0.8660254037844387076, 1.000000000000000000, 0.8660254037844387076, 1.000000000000000000, 0.8660254037844387076, 1.000000000000000000, 0.8660254037844387076, 1.000000000000000000, 0.8660254037844387076, 1.000000000000000000, 0.8660254037844387076, 1.000000000000000000, 0.8660254037844387076, 1.000000000000000000, 0.8660254037844387076, 1.000000000000000000, 0.8660254037844387076, 1.000000000000000000, 0.8660254037844387076, 1.000000000000000000, 0.8660254037844387076, 1.000000000000000000, 0.8660254037844387076, 1.000000000000000000, 0.8660254037844387076, 1.000000000000000000, 0.8660254037844387076, 1.000000000000000000, 0.8660254037844387076, 1.000000000000000000, 0.8660254037844387076, 1.000000000000000000, 0.8660254037844387076, 1.000000000000000000, 0.8660254037844387076, 1.000000000000000000, 0.8660254037844387076, 1.000000000000000000, 0.8660254037844387076, 1.000000000000000000, 0.8660254037844387076, 1.000000000000000000, 0.8660254037844387076, 1.000000000000000000, 0.8660254037844387076, 1.000000000000000000, 0.8660254037844387076, 1.000000000000000000, 0.8660254037844387076, 1.000000000000000000, 0.8660254037844387076, 1.000000000000000000, 0.8660254037844387076, 1.000000000000000000, 0.8660254037844387076, 1.000000000000000000, 0.8660254037844387076, 1.000000000000000000, 0.8660254037844387076, 1.000000000000000000, 0.8660254037844387076, 1.000000000000000000, 0.8660254037844387076, 1.000000000000000000, 0.8660254037844387076, 1.000000000000000000, 0.8660254037844387076, 1.000000000000000000, 0.8660254037844387076, 1.000000000000000000, 0.8660254037844387076, 1.000000000000000000, 0.8660254037844387076, 1.000000000000000000, 0.8660254037844387076, 1.000000000000000000, 0.8660254037844387076, 1.000000000000000000, 0.8660254037844387076, 1.000000000000000000, 0.8660254037844387076, 1.000000000000000000, 0.8660254037844387076, 1.000000000000000000, 0.8660254037844387076, 1.000000000000000000, 0.8660254037844387076, 1.000000000000000000, 0.8660254037844387076, 1.000000000000000000, 0.8660254037844387076, 1.000000000000000000, 0.8660254037844387076, 1.000000000000000000, 0.8660254037844387076, 1.000000000000000000, 0.8660254037844387076, 1.000000000000000000, 0.8660254037844387076, 1.000000000000000000, 0.8660254037844387076, 1.000000000000000000, 0.8660254037844387076, 1.000000000000000000, 0.8660254037844387076, 1.000000000000000000, 0.8660254037844387076, 1.000000000000000000, 0.8660254037844387076, 1.000000000000000000, 0.8660254037844387076, 1.000000000000000000, 0.8660254037844387076, 1.000000000000000000, 0.8660254037844387076, 1.000000000000000000, 0.8660254037844387076, 1.000000000000000000, 0.8660254037844387076, 1.000000000000000000, 0.8660254037844387076, 1.000000000000000000, 0.8660254037844387076, 1.000000000000000000, 0.8660254037844387076, 1.000000000000000000, 0.8660254037844387076, 1.000000000000000000, 0.8660254037844387076, 1.000000000000000000, 0.8660254037844387076, 1.000000000000000000, 0.8660254037844387076, 1.000000000000000000, 0.8660254037844387076, 1.000000000000000000, 0.8660254037844387076, 1.000000000000000000, 0.8660254037844387076, 1.000000000000000000, 0.8660254037844387076, 1.000000000000000000, 0.8660254037844387076, 1.000000000000000000, 0.8660254037844387076, 1.000000000000000000, 0.8660254037844387076, 1.000000000000000000, 0.8660254037844387076, 1.000000000000000000, 0.8660254037844387076, 1.000000000000000000, 0.8660254037844387076, 1.000000000000000000, 0.8660254037844387076, 1.000000000000000000, 0.8660254037844387076, 1.000000000000000000, 0.8660254037844387076, 1.000000000000000000, 0.8660254037844387076, 1.000000000000000000, 0.8660254037844387076, 1.000000000000000000, 0.8660254037844387076, 1.000000000000000000, 0.8660254037844387076, 1.000000000000000000, 0.8660254037844387076, 1.000000000000000000, 0.8660254037844387076, 1.000000000000000000, 0.8660254037844387076, 1.000000000000000000, 0.8660254037844387076, 1.000000000000000000, 0.8660254037844387076, 1.000000000000000000, 0.8660254037844387076, 1.000000000000000000, 0.8660254037844387076, 1.000000000000000000, 0.8660254037844387076, 1.000000000000000000, 0.8660254037844387076, 1.000000000000000000, 0.8660254037844387076, 1.000000000000000000, 0.8660254037844387076, 1.000000000000000000, 0.8660254037844387076, 1.000000000000000000, 0.8660254037844387076, 1.000000000000000000, 0.8660254037844387076, 1.000000000000000000, 0.8660254037844387076, 1.000000000000000000, 0.8660254037844387076, 1.000000000000000000, 0.8660254037844387076, 1.000000000000000000, 0.8660254037844387076, 1.000000000000000000, 0.8660254037844387076, 1.000000000000000000, 0.8660254037844387076, 1.000000000000000000, 0.8660254037844387076, 1.000000000000000000, 0.8660254037844387076, 1.000000000000000000, 0.8660254037844387076, 1.000000000000000000, 0.8660254037844387076, 1.000000000000000000, 0.8660254037844387076, 1.000000000000000000, 0.8660254037844387076, 1.000000000000000000, 0.8660254037844387076, 1.000000000000000000, 0.8660254037844387076, 1.000000000000000000, 0.8660254037844387076, 1.000000000000000000, 0.8660254037844387076, 1.000000000000000000, 0.8660254037844387076, 1.000000000000000000, 0.8660254037844387076, 1.000000000000000000, 0.8660254037844387076, 1.000000000000000000, 0.8660254037844387076, 1.000000000000000000, 0.8660254037844387076, 1.000000000000000000, 0.8660254037844387076, 1.000000000000000000, 0.8660254037844387076, 1.000000000000000000, 0.8660254037844387076, 1.000000000000000000, 0.8660254037844387076, 1.000000000000000000, 0.8660254037844387076, 1.000000000000000000, 0.8660254037844387076, 1.000000000000000000, 0.8660254037844387076, 1.000000000000000000, 0.8660254037844387076, 1.000000000000000000, 0.8660254037844387076, 1.000000000000000000, 0.8660254037844387076, 1.000000000000000000, 0.8660254037844387076, 1.000000000000000000, 0.8660254037844387076, 1.000000000000000000, 0.8660254037844387076, 1.000000000000000000, 0.8660254037844387076, 1.000000000000000000, 0.8660254037844387076, 1.000000000000000000, 0.8660254037844387076, 1.000000000000000000, 0.8660254037844387076, 1.000000000000000000, 0.8660254037844387076, 1.000000000000000000, 0.8660254037844387076, 1.000000000000000000, 0.8660254037844387076, 1.000000000000000000, 0.8660254037844387076, 1.000000000000000000, 0.8660254037844387076, 1.000000000000000000, 0.8660254037844387076, 1.000000000000000000, 0.8660254037844387076, 1.000000000000000000, 0.8660254037844387076, 1.000000000000000000, 0.8660254037844387076, 1.000000000000000000, 0.8660254037844387076, 1.000000000000000000, 0.8660254037844387076, 1.000000000000000000, 0.8660254037844387076, 1.000000000000000000, 0.8660254037844387076, 1.000000000000000000, 0.8660254037844387076, 1.000000000000000000, 0.8660254037844387076, 1.000000000000000000, 0.8660254037844387076, 1.000000000000000000, 0.8660254037844387076, 1.000000000000000000, 0.8660254037844387076, 1.000000000000000000, 0.8660254037844387076, 1.000000000000000000, 0.8660254037844387076, 1.000000000000000000, 0.8660254037844387076, 1.000000000000000000, 0.8660254037844387076, 1.000000000000000000, 0.8660254037844387076, 1.000000000000000000, 0.8660254037844387076, 1.000000000000000000, 0.8660254037844387076, 1.000000000000000000, 0.8660254037844387076, 1.000000000000000000, 0.8660254037844387076, 1.000000000000000000, 0.8660254037844387076, 1.000000000000000000, 0.8660254037844387076, 1.000000000000000000, 0.8660254037844387076, 1.000000000000000000, 0.8660254037844387076, 1.000000000000000000, 0.8660254037844387076, 1.000000000000000000, 0.8660254037844387076, 1.000000000000000000, 0.8660254037844387076, 1.000000000000000000, 0.8660254037844387076, 1.000000000000000000, 0.8660254037844387076, 1.000000000000000000, 0.8660254037844387076, 1.000000000000000000, 0.8660254037844387076, 1.000000000000000000, 0.8660254037844387076, 1.000000000000000000, 0.8660254037844387076, 1.000000000000000000, 0.8660254037844387076, 1.000000000000000000, 0.8660254037844387076, 1.000000000000000000, 0.8660254037844387076, 1.000000000000000000, 0.8660254037844387076, 1.000000000000000000, 0.8660254037844387076, 1.000000000000000000, 0.8660254037844387076, 1.000000000000000000, 0.8660254037844387076, 1.000000000000000000, 0.8660254037844387076, 1.000000000000000000, 0.8660254037844387076, 1.000000000000000000, 0.8660254037844387076, 1.000000000000000000, 0.8660254037844387076, 1.000000000000000000, 0.8660254037844387076, 1.000000000000000000, 0.8660254037844387076, 1.000000000000000000, 0.8660254037844387076, 1.000000000000000000, 0.8660254037844387076, 1.000000000000000000, 0.8660254037844387076, 1.000000000000000000, 0.8660254037844387076, 1.000000000000000000, 0.8660254037844387076, 1.000000000000000000, 0.8660254037844387076, 1.000000000000000000, 0.8660254037844387076, 1.000000000000000000, 0.8660254037844387076, 1.000000000000000000, 0.8660254037844387076, 1.000000000000000000, 0.8660254037844387076, 1.000000000000000000) ) ) 
 REPRESENTATION_ITEM ( '' )  SURFACE ( )  );
#87812 = DIRECTION ( 'NONE',  ( -0.7592566023652995710, 0.6507913734559652719, 0.000000000000000000 ) ) ;
#87813 = CARTESIAN_POINT ( 'NONE',  ( 4.864678189204997949, 4.569879397027603929, 0.7998128361456341429 ) ) ;
#87815 = ORIENTED_EDGE ( 'NONE', *, *, #40298, .T. ) ;
#87814 = CARTESIAN_POINT ( 'NONE',  ( -7.095713291905736853, 9.371694488680407886, 1.599625672291269396 ) ) ;
#87816 = CARTESIAN_POINT ( 'NONE',  ( 4.596911992430688265, 8.487755744900498556, -0.08351877912710949092 ) ) ;
#87817 = CARTESIAN_POINT ( 'NONE',  ( 3.655624903986275154, -0.3905385215352343287, -1.977747697055858955 ) ) ;
#87818 = CARTESIAN_POINT ( 'NONE',  ( 3.187279605439637287, -0.7454021820463945236, 1.683677988101241141 ) ) ;
#87819 = CARTESIAN_POINT ( 'NONE',  ( -0.008622056139523381901, 15.44694768828586540, 11.95585894197802013 ) ) ;
#87820 = CARTESIAN_POINT ( 'NONE',  ( 2.227567673948157800, 0.002208658356158287820, 2.307868969919598889 ) ) ;
#87821 = CARTESIAN_POINT ( 'NONE',  ( 4.706615602599436343, 5.520081620234675412, 1.199719254218452935 ) ) ;
#87822 = CARTESIAN_POINT ( 'NONE',  ( 3.374459016379764087, -1.290570702369205014, 1.733878788530068160 ) ) ;
#87823 = CARTESIAN_POINT ( 'NONE',  ( 8.772289083241844310, 10.19309100432570148, -1.199719254218446718 ) ) ;
#87825 = CARTESIAN_POINT ( 'NONE',  ( 2.712125330650519750, 1.116209241849321465, -1.679223868463100011 ) ) ;
#87824 = CARTESIAN_POINT ( 'NONE',  ( 6.620655732516645742, 0.007553340620044741646, 1.826407896915737794 ) ) ;
#87826 = CARTESIAN_POINT ( 'NONE',  ( -6.247609857798938293, 6.183299677053865295, -0.7998128361456291469 ) ) ;
#87827 = CARTESIAN_POINT ( 'NONE',  ( 3.005512134316370432, 2.280722703800378337, 0.2841129622813722277 ) ) ;
#87828 = CARTESIAN_POINT ( 'NONE',  ( -9.608184375698545665, 14.88196915126796327, -7.189074558220958089 ) ) ;
#87829 = CARTESIAN_POINT ( 'NONE',  ( 1.123270288250308280, 2.860197346350005887, 0.7749999999993786304 ) ) ;
#87830 = CARTESIAN_POINT ( 'NONE',  ( 2.360033908006432757, 0.7977434165707707470, 1.692156362554583460 ) ) ;
#87831 = CARTESIAN_POINT ( 'NONE',  ( 0.5617156953909893113, 1.950523934018918659, -0.2849811346736507156 ) ) ;
#87833 = CARTESIAN_POINT ( 'NONE',  ( -8.086512275908061653, 8.398962174839683215, 0.000000000000000000 ) ) ;
#87832 = CARTESIAN_POINT ( 'NONE',  ( 0.6823417656249917140, 4.842708333674755394, 1.181850606188765695 ) ) ;
#87834 = CARTESIAN_POINT ( 'NONE',  ( 2.157103830005083100, -1.704838622333640030, 1.401371054633032909 ) ) ;
#87835 = EDGE_LOOP ( 'NONE', ( #104802, #104689, #131660, #111604 ) ) ;
#87836 = CARTESIAN_POINT ( 'NONE',  ( -11.94105721237523099, 10.19999999999999929, 1.187919463087248273 ) ) ;
#87837 = CARTESIAN_POINT ( 'NONE',  ( 5.379888026524302980, 5.170957540566797128, -0.7998128361456211532 ) ) ;
#87838 = CARTESIAN_POINT ( 'NONE',  ( -4.894657149733403045, 5.669187081899118574, -1.199719254218446718 ) ) ;
#87839 = CARTESIAN_POINT ( 'NONE',  ( -7.720982897393580124, -5.907420853759296264, 7.834948825496934610 ) ) ;
#87840 = CARTESIAN_POINT ( 'NONE',  ( 6.420779677996255153, 1.839401344301737184, 0.7098503129845078474 ) ) ;
#87841 = CARTESIAN_POINT ( 'NONE',  ( 6.164718480307596060, -1.636601974411681981, 1.627217620858178337 ) ) ;
#87842 = CARTESIAN_POINT ( 'NONE',  ( 6.877413160773132361, -0.1400689347856296230, 1.829862831089356545 ) ) ;
#87843 = CARTESIAN_POINT ( 'NONE',  ( 3.661030488878083577, 1.629037084659604728, -1.265030972029494993 ) ) ;
#87844 = CARTESIAN_POINT ( 'NONE',  ( 5.341549334104184865, 8.215262742221458581, 1.082531754730558626 ) ) ;
#87845 = CARTESIAN_POINT ( 'NONE',  ( 6.373214726875630731, 9.593111727067046957, 1.199719254218452047 ) ) ;
#87846 = CARTESIAN_POINT ( 'NONE',  ( 6.873620692004076105, 10.00267932643801672, -1.082531754730537976 ) ) ;
#87847 = CARTESIAN_POINT ( 'NONE',  ( 0.6823417656249917140, 3.905208333674754950, 1.181850606188765695 ) ) ;
#87848 = CARTESIAN_POINT ( 'NONE',  ( -10.30143037061213285, 3.720351604917702115, -6.155881949090546534 ) ) ;
#87849 = CARTESIAN_POINT ( 'NONE',  ( 4.107757354816228279, 6.775838766385488654, -1.082531754730548412 ) ) ;
#87850 = CARTESIAN_POINT ( 'NONE',  ( 6.180164126497881938, -1.200935631872475540, -1.808625420649534021 ) ) ;
#87852 = CARTESIAN_POINT ( 'NONE',  ( 5.214338956685347526, 1.703448749313410282, 0.6994016148276983591 ) ) ;
#87851 = CARTESIAN_POINT ( 'NONE',  ( 6.639320575229252341, 0.005161017367553630275, 1.896863882003448021 ) ) ;
#87853 = EDGE_CURVE ( 'NONE', #50012, #89957, #192461, .T. ) ;
#87854 = CARTESIAN_POINT ( 'NONE',  ( 0.3769810270647707684, 3.049942316455285685, -0.4288785890453113980 ) ) ;
#87855 = CARTESIAN_POINT ( 'NONE',  ( 6.532779862045914321, -1.958661757936002612, 0.9833580883553474372 ) ) ;
#87856 = CARTESIAN_POINT ( 'NONE',  ( 0.7197278698120104234, -0.9953326032119573785, -1.583558375183778288 ) ) ;
#87857 = CARTESIAN_POINT ( 'NONE',  ( -4.956836104118029773, 6.830226236571708576, 1.450618959550575182 ) ) ;
#87858 = CARTESIAN_POINT ( 'NONE',  ( -0.4000000000000114575, 2.999999999999999112, 2.023857702507764422 ) ) ;
#87859 = CARTESIAN_POINT ( 'NONE',  ( 6.378761646814803399, 6.917158162233129737, 0.8102004381213165907 ) ) ;
#87860 = CARTESIAN_POINT ( 'NONE',  ( 11.35605497252127272, 13.61418145951645542, -3.553547709190210124 ) ) ;
#87861 = CARTESIAN_POINT ( 'NONE',  ( 1.990718100289643244, 1.541686266772484437, -0.8690610084590517648 ) ) ;
#87862 = CARTESIAN_POINT ( 'NONE',  ( 0.1527893875182678718, 0.3269112364552365091, 1.883972597190447518 ) ) ;
#87864 = CARTESIAN_POINT ( 'NONE',  ( 4.042530882030176187, -1.416877165883747125, 1.289359272694647451 ) ) ;
#87863 = CARTESIAN_POINT ( 'NONE',  ( -9.236128959407555072, 11.79856975744075598, -1.599625672291263179 ) ) ;
#87865 = CARTESIAN_POINT ( 'NONE',  ( 9.367496997597598352, 4.518459255872631530, 7.500000000000000000 ) ) ;
#87866 = CARTESIAN_POINT ( 'NONE',  ( 5.828554260932977904, -1.250890888562717684, 1.521285551415082482 ) ) ;
#87867 = CARTESIAN_POINT ( 'NONE',  ( 0.01804983835817890528, -0.5593552815991027494, 2.045460531183339814 ) ) ;
#87868 = CARTESIAN_POINT ( 'NONE',  ( -2.300079615812729905, 5.835176651756807331, -0.7998128361456281477 ) ) ;
#87869 = CARTESIAN_POINT ( 'NONE',  ( 2.307302758404996545, -0.4121581357655336175, 1.824517092411604979 ) ) ;
#87871 = VERTEX_POINT ( 'NONE', #117805 ) ;
#87870 = CARTESIAN_POINT ( 'NONE',  ( 6.287718881003963034, 1.195215413365672275, 1.243919913892058693 ) ) ;
#87873 = CARTESIAN_POINT ( 'NONE',  ( 4.094199201646931741, 4.839282492418613302, -1.082531754730543083 ) ) ;
#87872 = CARTESIAN_POINT ( 'NONE',  ( 3.176612885197922953, -1.314426786483071208, 1.772596291930063739 ) ) ;
#87874 = CARTESIAN_POINT ( 'NONE',  ( 1.364683531249988535, 3.676041667008087099, 0.7879004041258500513 ) ) ;
#87875 = CARTESIAN_POINT ( 'NONE',  ( 1.205618545266523567, -1.624909386276121692, -1.270427818644123796 ) ) ;
#87876 = CARTESIAN_POINT ( 'NONE',  ( 6.962275575817444384, 8.081408578997208991, -1.199719254218446718 ) ) ;
#87877 = CARTESIAN_POINT ( 'NONE',  ( -9.642873567817536795, 12.27310513391906532, 1.599625672291281386 ) ) ;
#87878 = CARTESIAN_POINT ( 'NONE',  ( -8.669853050657241766, 2.974000657017267901, -7.806370750283158522 ) ) ;
#87879 = CARTESIAN_POINT ( 'NONE',  ( -5.427341564172148303, 5.226320001155936090, 0.000000000000000000 ) ) ;
#87880 = CARTESIAN_POINT ( 'NONE',  ( -7.470306724222256278, -6.701288531902446444, -8.074422843256989779 ) ) ;
#87881 = ORIENTED_EDGE ( 'NONE', *, *, #115314, .T. ) ;
#87882 = CARTESIAN_POINT ( 'NONE',  ( 2.998552181135270001, 2.054425100943928051, 0.2560010573490826835 ) ) ;
#87883 = CARTESIAN_POINT ( 'NONE',  ( -1.500000000000013101, 3.879166666666685970, -0.8660254037844313801 ) ) ;
#87884 = CARTESIAN_POINT ( 'NONE',  ( 3.649115900372475796, 7.409052317076538330, 1.040834085586084257E-14 ) ) ;
#87885 = CARTESIAN_POINT ( 'NONE',  ( -5.987767821832088444, 7.191367801968548079, 1.216456708157914512 ) ) ;
#87886 = CARTESIAN_POINT ( 'NONE',  ( 0.9264325174072656210, -0.9100096784926974269, -1.803132658094412477 ) ) ;
#87887 = CARTESIAN_POINT ( 'NONE',  ( 1.123270288250308280, 2.922697346350005887, 0.7749999999993786304 ) ) ;
#87888 = CARTESIAN_POINT ( 'NONE',  ( -0.6823417656250212460, 3.551041667008085323, 1.181850606188767472 ) ) ;
#87889 = ADVANCED_FACE ( 'NONE', ( #85228 ), #168615, .F. ) ;
#87891 = CARTESIAN_POINT ( 'NONE',  ( 9.083599731475983319, 11.62061899152058686, 1.443375672974076540 ) ) ;
#87890 = CARTESIAN_POINT ( 'NONE',  ( 0.1749903794560644099, 4.092791488633133135, -2.510332109122221045 ) ) ;
#87892 = CARTESIAN_POINT ( 'NONE',  ( 6.151720201709268920, -0.2930281871833945173, -1.994563951915592881 ) ) ;
#87893 = CARTESIAN_POINT ( 'NONE',  ( 5.542171544414384421, 0.7827158775690710169, 1.748735243013665785 ) ) ;
#87894 = CARTESIAN_POINT ( 'NONE',  ( 6.539320575229276677, 2.966918982532817051, 2.456386401752636672 ) ) ;
#87895 = CARTESIAN_POINT ( 'NONE',  ( 3.843468145482429321, 0.7371271433744167600, -2.064019554291535830 ) ) ;
#87896 = CARTESIAN_POINT ( 'NONE',  ( -1.500000000000013101, 2.410416667349482456, -0.8660254037844313801 ) ) ;
#87897 = CARTESIAN_POINT ( 'NONE',  ( 2.724755696555291262, 1.382288352666941389, -1.321784923088549446 ) ) ;
#87898 = CARTESIAN_POINT ( 'NONE',  ( -5.229694566569281555, 7.124396299129368337, 1.599625672291267398 ) ) ;
#87899 = CARTESIAN_POINT ( 'NONE',  ( 5.355107487273504496, 6.310342158982962246, -1.082531754730543083 ) ) ;
#87901 = CARTESIAN_POINT ( 'NONE',  ( 1.142204091441896718, 0.8197918422115093584, 1.842440257734210274 ) ) ;
#87900 = CARTESIAN_POINT ( 'NONE',  ( 10.38614328979755719, 3.507114751586604129, -5.996442624206805405 ) ) ;
#87902 = CARTESIAN_POINT ( 'NONE',  ( 0.6823417656249969321, 11.08854166700806765, -1.181850606188757036 ) ) ;
#87904 = CARTESIAN_POINT ( 'NONE',  ( -5.550083779947821760, 7.568460058062819407, -1.599625672291271394 ) ) ;
#87903 = CARTESIAN_POINT ( 'NONE',  ( 6.040607902356621928, -1.852314659301615096, 1.170993205287726990 ) ) ;
#87906 = ORIENTED_EDGE ( 'NONE', *, *, #62295, .T. ) ;
#87905 = CARTESIAN_POINT ( 'NONE',  ( 2.520142033498268486, 1.128878695625197492, -1.304093658461308980 ) ) ;
#87907 = CARTESIAN_POINT ( 'NONE',  ( -0.1405533004718312329, 2.055874972810427526, -2.136773944524199109 ) ) ;
#87908 = CARTESIAN_POINT ( 'NONE',  ( 6.123478934866503742, 10.29580919065294431, 0.7998128361456462443 ) ) ;
#87909 = CARTESIAN_POINT ( 'NONE',  ( 3.876741858503734761, 6.610283703974623393, 1.199719254218462483 ) ) ;
#87910 = CARTESIAN_POINT ( 'NONE',  ( 0.8362905744919849615, -1.092891352686057527, 1.629061181365853539 ) ) ;
#87911 = CARTESIAN_POINT ( 'NONE',  ( 3.832150974156964818, 7.622593236491780999, 1.040834085586084257E-14 ) ) ;
#87912 = CARTESIAN_POINT ( 'NONE',  ( -1.499999999999946709, 7.750000000000000000, 15.75000000000000711 ) ) ;
#87913 = ORIENTED_EDGE ( 'NONE', *, *, #114510, .F. ) ;
#87914 = CARTESIAN_POINT ( 'NONE',  ( -0.4000000000000361045, 3.964661556059730696, -0.9099571394229808430 ) ) ;
#87915 = ORIENTED_EDGE ( 'NONE', *, *, #108416, .T. ) ;
#87916 = CARTESIAN_POINT ( 'NONE',  ( 4.424329001689049079, -0.7786147893445326540, -1.635752125832173220 ) ) ;
#87917 = ORIENTED_EDGE ( 'NONE', *, *, #135584, .F. ) ;
#87918 = CARTESIAN_POINT ( 'NONE',  ( 9.215791728987056786, 11.77484298861683598, -1.599625672291262513 ) ) ;
#87919 = CARTESIAN_POINT ( 'NONE',  ( 3.923105346307896202, 5.670318552149568703, -1.599625672291269396 ) ) ;
#87920 = CARTESIAN_POINT ( 'NONE',  ( 5.162699569786796339, 0.5314807639728249544, 1.731738579618222973 ) ) ;
#87921 = CARTESIAN_POINT ( 'NONE',  ( 5.844973620822823790, 9.833236634353070826, 0.7216878364870317197 ) ) ;
#87922 = CARTESIAN_POINT ( 'NONE',  ( 1.355808955840426748E-16, 3.500000000000003109, 2.025000000000006573 ) ) ;
#87923 = CARTESIAN_POINT ( 'NONE',  ( 5.712091369430416066, 6.087825614771766425, 0.6924918054137980672 ) ) ;
#87925 = CARTESIAN_POINT ( 'NONE',  ( -1.364683531250010295, 14.88020833367472839, 0.7879004041258445001 ) ) ;
#87924 = CARTESIAN_POINT ( 'NONE',  ( 5.072628826387419743, 1.283713728693743894, -1.347665127999774448 ) ) ;
#87926 = B_SPLINE_CURVE_WITH_KNOTS ( 'NONE', 3,
 ( #8409, #173073, #187161, #24654, #206610, #42016, #108125, #174152, #91835, #9485, #75558 ),
 .UNSPECIFIED., .F., .F.,
 ( 4, 1, 1, 1, 1, 1, 1, 1, 4 ),
 ( 0.000000000000000000, 0.2256777920876190668, 0.3978457394851813711, 0.5256768607792676740, 0.6183602023682204241, 0.6850295134299612121, 0.7345374503969632762, 0.7752450576501028756, 1.000000000000000000 ),
 .UNSPECIFIED. ) ;
#87927 = CARTESIAN_POINT ( 'NONE',  ( 3.075699878008768096, -0.7735687425090407299, 1.752645402151173926 ) ) ;
#87928 = CIRCLE ( 'NONE', #108714, 0.2999999999999999334 ) ;
#87929 = CYLINDRICAL_SURFACE ( 'NONE', #24772, 0.3999999999999997446 ) ;
#87930 = CARTESIAN_POINT ( 'NONE',  ( -10.52284959769361805, 5.420271152154175986, 5.071911021504272199 ) ) ;
#87931 = CARTESIAN_POINT ( 'NONE',  ( -10.99956415888072492, -9.918872522958837479, 0.09791994008663019999 ) ) ;
#87932 = CARTESIAN_POINT ( 'NONE',  ( 6.925078400183575233, 4.688909937558557672, 2.706876980850602354 ) ) ;
#87933 = AXIS2_PLACEMENT_3D ( 'NONE', #97215, #211986, #98266 ) ;
#87934 = CARTESIAN_POINT ( 'NONE',  ( 8.283668668269706714, 8.766627655843892697, 1.040834085586084257E-14 ) ) ;
#87935 = CARTESIAN_POINT ( 'NONE',  ( -2.442440228756222353, 6.001264033524212671, -0.7998128361456281477 ) ) ;
#87936 = SURFACE_STYLE_USAGE ( .BOTH. , #137770 ) ;
#87937 = CARTESIAN_POINT ( 'NONE',  ( 1.043050037176814326, -1.649054093272810606, -1.284947313888247900 ) ) ;
#87938 = CARTESIAN_POINT ( 'NONE',  ( 4.854701522145073334, 7.821512988214679218, -1.199719254218450271 ) ) ;
#87939 = CARTESIAN_POINT ( 'NONE',  ( 6.528350403681292491, 1.108413491673976736, -1.575378176345716419 ) ) ;
#87940 = CARTESIAN_POINT ( 'NONE',  ( -6.091691091241777656, 6.001394449403842479, 0.7998128361456341429 ) ) ;
#87941 = CARTESIAN_POINT ( 'NONE',  ( 2.028078973712159172, 1.053637016394028292, -1.490636434207486483 ) ) ;
#87942 = CARTESIAN_POINT ( 'NONE',  ( -3.039951802757244526, 2.724153688964686904, 2.451370731312843443 ) ) ;
#87943 = CARTESIAN_POINT ( 'NONE',  ( 1.845825534506392085, -1.251752223804462272, -1.445855903880132631 ) ) ;
#87944 = CARTESIAN_POINT ( 'NONE',  ( 1.873436276770530595, -0.2440693053713405281, 1.954313301998261920 ) ) ;
#87945 = CARTESIAN_POINT ( 'NONE',  ( 4.001460698126992455, -1.936627024540507946, 0.1462448094460607750 ) ) ;
#87946 = VERTEX_POINT ( 'NONE', #103632 ) ;
#87947 = CARTESIAN_POINT ( 'NONE',  ( -6.434831245971854408, -8.233137084989849086, -7.097136523687855636 ) ) ;
#87948 = CARTESIAN_POINT ( 'NONE',  ( -3.793249116773374396, 7.647484079536056356, 0.7998128361456352531 ) ) ;
#87950 = CARTESIAN_POINT ( 'NONE',  ( 3.885109016898561585, -1.979880364965879380, -0.7601140796509860964 ) ) ;
#87949 = CARTESIAN_POINT ( 'NONE',  ( 5.643937085038755797, 9.806620042512378177, -0.7998128361456481317 ) ) ;
#87951 = CARTESIAN_POINT ( 'NONE',  ( -10.62873463776380056, 13.79999999999998295, 3.199999999999997957 ) ) ;
#87952 = CARTESIAN_POINT ( 'NONE',  ( 8.452618703115982512, 11.94880668935564216, 1.199719254218450271 ) ) ;
#87953 = CARTESIAN_POINT ( 'NONE',  ( -5.478376588373717659, 8.549133898814758936, -1.199719254218452047 ) ) ;
#87954 = CARTESIAN_POINT ( 'NONE',  ( 4.067082894419602468, 3.847277586352047862, -0.7216878364870188411 ) ) ;
#87955 = VERTEX_POINT ( 'NONE', #101484 ) ;
#87956 = CARTESIAN_POINT ( 'NONE',  ( 5.875479466675786355, 7.948088359245467416, -1.599625672291283607 ) ) ;
#87957 = CARTESIAN_POINT ( 'NONE',  ( 8.283668668269706714, 8.766627655843896250, 1.040834085586084257E-14 ) ) ;
#87958 = CARTESIAN_POINT ( 'NONE',  ( 3.562960707638890501, -1.610701098693729350, -0.8595150645765645692 ) ) ;
#87959 = CARTESIAN_POINT ( 'NONE',  ( 10.99962150373185210, -9.919999999999998153, -0.09125116240077391083 ) ) ;
#87960 = CARTESIAN_POINT ( 'NONE',  ( -9.490344339885977476, 11.13478515369756217, -1.082531754730539753 ) ) ;
#87961 = CARTESIAN_POINT ( 'NONE',  ( -4.584844773125573703, 8.498748274393685520, 0.004977730536110530624 ) ) ;
#87962 = CARTESIAN_POINT ( 'NONE',  ( 6.589320575229281829, 7.629137130509070275, 2.703262396134015866 ) ) ;
#87963 = CARTESIAN_POINT ( 'NONE',  ( 4.750782166719051069, -1.502237938222051650, 1.114538048626475986 ) ) ;
#87964 = CARTESIAN_POINT ( 'NONE',  ( 7.618792255875527886, 10.97600916757510170, 1.199719254218460707 ) ) ;
#87965 = CARTESIAN_POINT ( 'NONE',  ( 1.664548039484465614, -1.362698257634049614, 1.362033803609383531 ) ) ;
#87966 = CARTESIAN_POINT ( 'NONE',  ( 6.719590461409528537, 0.3385411321301828869, -1.932175811092277096 ) ) ;
#87967 = EDGE_CURVE ( 'NONE', #15788, #84713, #140256, .T. ) ;
#87968 = CARTESIAN_POINT ( 'NONE',  ( 1.364683531249996529, 9.026041667008060543, 0.7879004041258405033 ) ) ;
#87969 = CARTESIAN_POINT ( 'NONE',  ( -7.063961727919978451, 8.200042423116789436, 1.199719254218450271 ) ) ;
#87970 = CARTESIAN_POINT ( 'NONE',  ( 3.161022370280501814, 6.839609865302569425, 0.000000000000000000 ) ) ;
#87971 = EDGE_CURVE ( 'NONE', #119323, #1199, #102552, .T. ) ;
#87972 = CARTESIAN_POINT ( 'NONE',  ( -5.763624699140883934, 6.857221916153382502, -1.082531754730549967 ) ) ;
#87973 = CARTESIAN_POINT ( 'NONE',  ( 0.7907972306774737614, 1.600388572762038830, -1.386229290198564001 ) ) ;
#87974 = STYLED_ITEM ( 'NONE', ( #138455 ), #108668 ) ;
#87975 = CARTESIAN_POINT ( 'NONE',  ( 3.475000000000000533, -2.245833333333331350, -2.006292185433951047 ) ) ;
#87976 = CARTESIAN_POINT ( 'NONE',  ( 5.190316231837919680, 1.068962568377257671, -1.772817291931286787 ) ) ;
#87978 = CARTESIAN_POINT ( 'NONE',  ( -1.364683531250014514, 2.051041667008086655, -0.7879004041258289570 ) ) ;
#87977 = CARTESIAN_POINT ( 'NONE',  ( 0.6261898170028465938, 0.1349980957352381883, 1.836376839866371569 ) ) ;
#87979 = EDGE_LOOP ( 'NONE', ( #208335, #53174 ) ) ;
#87980 = CARTESIAN_POINT ( 'NONE',  ( 5.713622356042774797, 2.214598200325838206, 0.6159738146167788031 ) ) ;
#87981 = CARTESIAN_POINT ( 'NONE',  ( 5.178851490740187913, 8.985817805931475277, 0.7216878364870438212 ) ) ;
#87982 = CARTESIAN_POINT ( 'NONE',  ( 5.411112705629925301, 5.485588709422586362, 0.000000000000000000 ) ) ;
#87983 = CARTESIAN_POINT ( 'NONE',  ( 1.324644486801781040, 2.210297274253099520, 0.6072788910070088253 ) ) ;
#87984 = FACE_OUTER_BOUND ( 'NONE', #164895, .T. ) ;
#87985 = CARTESIAN_POINT ( 'NONE',  ( -5.424143973919053785, 8.485862515284315677, 1.199719254218454489 ) ) ;
#87986 = CARTESIAN_POINT ( 'NONE',  ( 5.630791504788829727, -1.754662785997921359, 0.8323459256341717571 ) ) ;
#87987 = ORIENTED_EDGE ( 'NONE', *, *, #76253, .F. ) ;
#87990 = ADVANCED_FACE ( 'NONE', ( #87377 ), #79579, .T. ) ;
#87989 = CARTESIAN_POINT ( 'NONE',  ( 7.904040366642689719, 10.24446639921506552, 1.443375672974076540 ) ) ;
#87988 = AXIS2_PLACEMENT_3D ( 'NONE', #80726, #64473, #111158 ) ;
#87992 = ORIENTED_EDGE ( 'NONE', *, *, #170841, .F. ) ;
#87991 =( BOUNDED_SURFACE ( )  B_SPLINE_SURFACE ( 1, 2, ( 
 ( #73181, #155527, #3896, #54821, #88393, #105740, #172855, #68903, #4958, #104648, #102499, #7107, #135022, #205317, #55883, #6038, #118810, #137149, #72109, #186940, #38573, #168563, #138218, #139287, #204231, #69968, #122041, #202095, #188005, #39631, #56955, #171767, #23363, #184795, #89473, #24426, #37498, #21215, #123127, #185863, #189086, #201036, #40719, #106825, #151262, #36423, #20162, #86249, #152319, #136078, #53753, #119886, #103574, #62289, #43927, #142506, #75337, #127378, #61222, #208514, #141454, #193350, #207461, #25510, #59080, #44994, #144648, #93747, #12455, #42866, #9266, #74279, #111103, #112180, #178184, #143584, #191200, #125240, #108974, #174993, #206390, #91618, #92681, #90538, #26578, #156603, #110042, #158726, #192266, #177109, #78530, #8194, #126306, #10323, #210663, #140373, #28725, #160861, #76397, #128449, #60149, #176054, #27648, #159785, #94811, #46058, #11387, #77465, #209577, #194416, #58017, #157669, #41798, #124181, #190144, #107911, #173937, #130566, #149947, #114311, #113245, #132653, #117500, #163000, #34045, #198657, #29799, #49249, #145720, #15647, #179250, #131604, #115370, #80677, #196556, #1516, #180310, #30873, #50306, #95884, #14581, #100118, #116424, #161938, #181362, #211719, #81736, #96952, #197605, #32986, #146768, #51377, #13531, #31930, #99063, #195494, #166180, #79601, #83857, #148868, #165117, #63355, #98012, #16709, #164068, #147817, #47130, #82794, #17768, #443, #212785, #213836, #64422, #65454, #66511, #67580, #182415, #133725, #129514, #199731, #48199, #69725, #53498, #155275, #3646, #103321, #18845, #137964, #169383, #54569, #35100, #201854, #88138, #171513, #104394, #119635, #86002, #105480, #6855, #136898, #20968, #168322, #5778, #154208, #87065, #19917, #71857, #152076, #118565, #135829, #203985, #23107, #186690, #89222, #185619, #102248, #167260, #55632, #205063, #56705, #22029, #37251, #153137, #4711, #70785, #84930, #184550, #202927, #183491, #120717, #101171, #38318, #170441, #121788, #187755, #72934, #151019, #39384, #139038, #2586, #68656, #134779, #200788, #52439, #36171, #190949, #42613, #108723, #207211, #60970, #78279, #76151, #174749, #142255, #26322, #110851, #57770, #74023, #175804, #92436, #158475, #172599, #44745, #127126, #189899, #10075, #208267, #77211, #160606, #12208, #141200, #176858, #27396, #28471, #109797, #94563, #144407, #59900, #206139, #91361, #58835, #173684, #210407, #124990, #123931, #25260, #126053, #143330, #192015, #43678, #24178, #122872, #41541, #11134, #90281, #93496, #188833, #40469, #157421, #159536, #106572, #209323, #193096, #156350, #7934, #140113, #107655, #9012, #75088, #99872, #180062, #29547, #161690, #63104, #149689, #115119, #95639, #212540, #194165, #32734, #65212, #165935, #129272, #111932, #17520, #195245, #46881, #132411, #45812, #112993, #128204, #13284, #83608, #194, #62049, #31685, #213587 ),
 ( #182163, #177934, #66263, #198413, #179006, #33794, #130321, #196311, #47955, #146521, #50057, #79357, #15398, #114070, #81489, #97761, #116178, #211470, #145475, #181115, #163819, #147566, #30620, #162758, #96709, #64180, #14332, #164866, #80422, #131363, #197358, #16460, #49001, #98814, #82540, #148628, #150769, #103072, #20721, #52186, #22852, #133474, #3403, #5523, #71604, #151830, #185366, #152881, #70529, #203735, #69472, #135579, #34847, #4459, #2331, #137715, #68407, #55381, #121536, #134534, #119380, #86815, #170188, #39135, #105218, #19669, #187506, #54320, #171258, #202672, #88966, #1272, #201601, #84682, #184298, #85748, #118312, #67330, #53249, #200540, #35923, #169127, #21774, #36989, #136647, #51120, #199476, #102000, #104141, #117243, #120461, #183243, #100922, #168069, #38071, #167010, #186433, #87883, #153957, #18602, #43418, #56452, #155021, #107399, #192826, #58582, #122612, #40207, #156092, #28214, #208016, #188575, #91105, #72686, #125800, #158230, #44484, #7677, #204801, #110601, #73761, #139856, #10874, #138781, #205887, #6605, #106317, #176602, #93241, #172341, #124737, #92180, #9821, #108469, #57520, #23929, #90033, #123678, #189640, #190696, #41291, #126868, #173421, #26068, #25003, #59642, #209067, #157166, #42357, #76949, #8758, #74839, #142001, #140939, #191762, #206953, #174491, #109542, #75897, #175546, #27135, #143074, #159275, #60704, #95377, #45550, #14065, #114849, #164607, #193902, #113798, #147305, #63905, #197095, #210139, #94307, #46610, #132147, #212270, #61783, #111666, #161426, #181898, #213331, #127949, #30355, #11950, #64956, #97495, #198153, #13009, #144147, #49786, #79086, #145204, #16192, #78023, #211210, #160348, #177673, #115912, #32471, #29283, #130061, #31419, #163552, #47686, #62835, #128997, #194974, #112732, #178742, #196054, #96442, #65997, #162493, #179800, #80152, #131108, #148368, #146257, #15135, #82273, #81223, #48736, #180849, #98543, #214367, #182980, #199208, #4204, #36722, #116980, #34597, #169927, #71340, #119116, #100665, #50855, #167805, #54059, #103879, #133204, #52980, #37804, #21511, #184040, #3136, #185095, #102808, #87623, #35657, #101736, #67068, #168864, #166743, #153694, #18337, #5263, #137456, #84418, #151569, #20467, #202404, #203471, #55125, #51931, #121270, #86553, #33533, #152617, #99605, #165671, #19404, #150507, #2068, #118055, #68139, #17260, #85483, #134272, #200280, #135326, #120194, #69206, #201340, #83336, #149421, #70272, #136388, #1004, #186170, #145752, #187245, #158760, #12490, #79634, #208546, #126339, #60181, #128482, #211753, #143617, #43958, #209611, #176086, #178219, #125273, #141488, #28759, #27684, #93782, #22596, #76431, #95918, #192299, #59115, #78563, #63391, #109007, #194450, #144683, #38872, #61254, #88703, #159819, #191235, #77498, #127412, #26613, #104957, #170998, #110074, #193384, #207494, #46094, #154761 ) ),
 .UNSPECIFIED., .F., .F., .T. ) 
 B_SPLINE_SURFACE_WITH_KNOTS ( ( 2, 2 ),
 ( 3, 2, 2, 2, 2, 2, 2, 2, 2, 2, 2, 2, 2, 2, 2, 2, 2, 2, 2, 2, 2, 2, 2, 2, 2, 2, 2, 2, 2, 2, 2, 2, 2, 2, 2, 2, 2, 2, 2, 2, 2, 2, 2, 2, 2, 2, 2, 2, 2, 2, 2, 2, 2, 2, 2, 2, 2, 2, 2, 2, 2, 2, 2, 2, 2, 2, 2, 2, 2, 2, 2, 2, 2, 2, 2, 2, 2, 2, 2, 2, 2, 2, 2, 2, 2, 2, 2, 2, 2, 2, 2, 2, 2, 2, 2, 2, 2, 2, 2, 2, 2, 2, 2, 2, 2, 2, 2, 2, 2, 2, 2, 2, 2, 2, 2, 2, 2, 2, 2, 2, 2, 2, 2, 2, 2, 2, 2, 2, 2, 2, 2, 2, 2, 2, 2, 2, 2, 2, 2, 2, 2, 2, 2, 2, 2, 2, 2, 2, 2, 2, 2, 2, 2, 2, 2, 2, 2, 2, 2, 2, 2, 2, 2, 2, 2, 2, 2, 2, 3 ),
 ( 0.000000000000000000, 1.000000000000000000 ),
 ( 0.000000000000000000, 0.005952380952380952051, 0.01190476190476190410, 0.01785714285714285615, 0.02380952380952380820, 0.02976190476190476025, 0.03571428571428571230, 0.04166666666666666435, 0.04761904761904761640, 0.05357142857142856845, 0.05952380952380952051, 0.06547619047619047949, 0.07142857142857142461, 0.07738095238095238360, 0.08333333333333332871, 0.08928571428571428770, 0.09523809523809523281, 0.1011904761904761918, 0.1071428571428571369, 0.1130952380952380959, 0.1190476190476190410, 0.1250000000000000000, 0.1309523809523809590, 0.1369047619047619180, 0.1428571428571428492, 0.1488095238095238082, 0.1547619047619047672, 0.1607142857142857262, 0.1666666666666666574, 0.1726190476190476164, 0.1785714285714285754, 0.1845238095238095344, 0.1904761904761904656, 0.1964285714285714246, 0.2023809523809523836, 0.2083333333333333426, 0.2142857142857142738, 0.2202380952380952328, 0.2261904761904761918, 0.2321428571428571508, 0.2380952380952380820, 0.2440476190476190410, 0.2500000000000000000, 0.2559523809523809312, 0.2619047619047619180, 0.2678571428571428492, 0.2738095238095238360, 0.2797619047619047672, 0.2857142857142856984, 0.2916666666666666852, 0.2976190476190476164, 0.3035714285714285476, 0.3095238095238095344, 0.3154761904761904656, 0.3214285714285714524, 0.3273809523809523836, 0.3333333333333333148, 0.3392857142857143016, 0.3452380952380952328, 0.3511904761904761640, 0.3571428571428571508, 0.3630952380952380820, 0.3690476190476190688, 0.3750000000000000000, 0.3809523809523809312, 0.3869047619047619180, 0.3928571428571428492, 0.3988095238095238360, 0.4047619047619047672, 0.4107142857142856984, 0.4166666666666666852, 0.4226190476190476164, 0.4285714285714285476, 0.4345238095238095344, 0.4404761904761904656, 0.4464285714285714524, 0.4523809523809523836, 0.4583333333333333148, 0.4642857142857143016, 0.4702380952380952328, 0.4761904761904761640, 0.4821428571428571508, 0.4880952380952380820, 0.4940476190476190688, 0.5000000000000000000, 0.5059523809523809312, 0.5119047619047618625, 0.5178571428571429047, 0.5238095238095238360, 0.5297619047619047672, 0.5357142857142856984, 0.5416666666666666297, 0.5476190476190476719, 0.5535714285714286031, 0.5595238095238095344, 0.5654761904761904656, 0.5714285714285713969, 0.5773809523809523281, 0.5833333333333333703, 0.5892857142857143016, 0.5952380952380952328, 0.6011904761904761640, 0.6071428571428570953, 0.6130952380952381375, 0.6190476190476190688, 0.6250000000000000000, 0.6309523809523809312, 0.6369047619047618625, 0.6428571428571429047, 0.6488095238095238360, 0.6547619047619047672, 0.6607142857142856984, 0.6666666666666666297, 0.6726190476190476719, 0.6785714285714286031, 0.6845238095238095344, 0.6904761904761904656, 0.6964285714285713969, 0.7023809523809523281, 0.7083333333333333703, 0.7142857142857143016, 0.7202380952380952328, 0.7261904761904761640, 0.7321428571428570953, 0.7380952380952381375, 0.7440476190476190688, 0.7500000000000000000, 0.7559523809523809312, 0.7619047619047618625, 0.7678571428571429047, 0.7738095238095238360, 0.7797619047619047672, 0.7857142857142856984, 0.7916666666666666297, 0.7976190476190476719, 0.8035714285714286031, 0.8095238095238095344, 0.8154761904761904656, 0.8214285714285713969, 0.8273809523809523281, 0.8333333333333333703, 0.8392857142857143016, 0.8452380952380952328, 0.8511904761904761640, 0.8571428571428570953, 0.8630952380952381375, 0.8690476190476190688, 0.8750000000000000000, 0.8809523809523809312, 0.8869047619047618625, 0.8928571428571429047, 0.8988095238095238360, 0.9047619047619047672, 0.9107142857142856984, 0.9166666666666666297, 0.9226190476190476719, 0.9285714285714286031, 0.9345238095238095344, 0.9404761904761904656, 0.9464285714285713969, 0.9523809523809523281, 0.9583333333333333703, 0.9642857142857143016, 0.9702380952380952328, 0.9761904761904761640, 0.9821428571428570953, 0.9880952380952381375, 0.9940476190476190688, 1.000000000000000000 ),
 .UNSPECIFIED. ) 
 GEOMETRIC_REPRESENTATION_ITEM ( )  RATIONAL_B_SPLINE_SURFACE ( (
 ( 1.000000000000000000, 0.8660254037844387076, 1.000000000000000000, 0.8660254037844387076, 1.000000000000000000, 0.8660254037844387076, 1.000000000000000000, 0.8660254037844387076, 1.000000000000000000, 0.8660254037844387076, 1.000000000000000000, 0.8660254037844387076, 1.000000000000000000, 0.8660254037844387076, 1.000000000000000000, 0.8660254037844387076, 1.000000000000000000, 0.8660254037844387076, 1.000000000000000000, 0.8660254037844387076, 1.000000000000000000, 0.8660254037844387076, 1.000000000000000000, 0.8660254037844387076, 1.000000000000000000, 0.8660254037844387076, 1.000000000000000000, 0.8660254037844387076, 1.000000000000000000, 0.8660254037844387076, 1.000000000000000000, 0.8660254037844387076, 1.000000000000000000, 0.8660254037844387076, 1.000000000000000000, 0.8660254037844387076, 1.000000000000000000, 0.8660254037844387076, 1.000000000000000000, 0.8660254037844387076, 1.000000000000000000, 0.8660254037844387076, 1.000000000000000000, 0.8660254037844387076, 1.000000000000000000, 0.8660254037844387076, 1.000000000000000000, 0.8660254037844387076, 1.000000000000000000, 0.8660254037844387076, 1.000000000000000000, 0.8660254037844387076, 1.000000000000000000, 0.8660254037844387076, 1.000000000000000000, 0.8660254037844387076, 1.000000000000000000, 0.8660254037844387076, 1.000000000000000000, 0.8660254037844387076, 1.000000000000000000, 0.8660254037844387076, 1.000000000000000000, 0.8660254037844387076, 1.000000000000000000, 0.8660254037844387076, 1.000000000000000000, 0.8660254037844387076, 1.000000000000000000, 0.8660254037844387076, 1.000000000000000000, 0.8660254037844387076, 1.000000000000000000, 0.8660254037844387076, 1.000000000000000000, 0.8660254037844387076, 1.000000000000000000, 0.8660254037844387076, 1.000000000000000000, 0.8660254037844387076, 1.000000000000000000, 0.8660254037844387076, 1.000000000000000000, 0.8660254037844387076, 1.000000000000000000, 0.8660254037844387076, 1.000000000000000000, 0.8660254037844387076, 1.000000000000000000, 0.8660254037844387076, 1.000000000000000000, 0.8660254037844387076, 1.000000000000000000, 0.8660254037844387076, 1.000000000000000000, 0.8660254037844387076, 1.000000000000000000, 0.8660254037844387076, 1.000000000000000000, 0.8660254037844387076, 1.000000000000000000, 0.8660254037844387076, 1.000000000000000000, 0.8660254037844387076, 1.000000000000000000, 0.8660254037844387076, 1.000000000000000000, 0.8660254037844387076, 1.000000000000000000, 0.8660254037844387076, 1.000000000000000000, 0.8660254037844387076, 1.000000000000000000, 0.8660254037844387076, 1.000000000000000000, 0.8660254037844387076, 1.000000000000000000, 0.8660254037844387076, 1.000000000000000000, 0.8660254037844387076, 1.000000000000000000, 0.8660254037844387076, 1.000000000000000000, 0.8660254037844387076, 1.000000000000000000, 0.8660254037844387076, 1.000000000000000000, 0.8660254037844387076, 1.000000000000000000, 0.8660254037844387076, 1.000000000000000000, 0.8660254037844387076, 1.000000000000000000, 0.8660254037844387076, 1.000000000000000000, 0.8660254037844387076, 1.000000000000000000, 0.8660254037844387076, 1.000000000000000000, 0.8660254037844387076, 1.000000000000000000, 0.8660254037844387076, 1.000000000000000000, 0.8660254037844387076, 1.000000000000000000, 0.8660254037844387076, 1.000000000000000000, 0.8660254037844387076, 1.000000000000000000, 0.8660254037844387076, 1.000000000000000000, 0.8660254037844387076, 1.000000000000000000, 0.8660254037844387076, 1.000000000000000000, 0.8660254037844387076, 1.000000000000000000, 0.8660254037844387076, 1.000000000000000000, 0.8660254037844387076, 1.000000000000000000, 0.8660254037844387076, 1.000000000000000000, 0.8660254037844387076, 1.000000000000000000, 0.8660254037844387076, 1.000000000000000000, 0.8660254037844387076, 1.000000000000000000, 0.8660254037844387076, 1.000000000000000000, 0.8660254037844387076, 1.000000000000000000, 0.8660254037844387076, 1.000000000000000000, 0.8660254037844387076, 1.000000000000000000, 0.8660254037844387076, 1.000000000000000000, 0.8660254037844387076, 1.000000000000000000, 0.8660254037844387076, 1.000000000000000000, 0.8660254037844387076, 1.000000000000000000, 0.8660254037844387076, 1.000000000000000000, 0.8660254037844387076, 1.000000000000000000, 0.8660254037844387076, 1.000000000000000000, 0.8660254037844387076, 1.000000000000000000, 0.8660254037844387076, 1.000000000000000000, 0.8660254037844387076, 1.000000000000000000, 0.8660254037844387076, 1.000000000000000000, 0.8660254037844387076, 1.000000000000000000, 0.8660254037844387076, 1.000000000000000000, 0.8660254037844387076, 1.000000000000000000, 0.8660254037844387076, 1.000000000000000000, 0.8660254037844387076, 1.000000000000000000, 0.8660254037844387076, 1.000000000000000000, 0.8660254037844387076, 1.000000000000000000, 0.8660254037844387076, 1.000000000000000000, 0.8660254037844387076, 1.000000000000000000, 0.8660254037844387076, 1.000000000000000000, 0.8660254037844387076, 1.000000000000000000, 0.8660254037844387076, 1.000000000000000000, 0.8660254037844387076, 1.000000000000000000, 0.8660254037844387076, 1.000000000000000000, 0.8660254037844387076, 1.000000000000000000, 0.8660254037844387076, 1.000000000000000000, 0.8660254037844387076, 1.000000000000000000, 0.8660254037844387076, 1.000000000000000000, 0.8660254037844387076, 1.000000000000000000, 0.8660254037844387076, 1.000000000000000000, 0.8660254037844387076, 1.000000000000000000, 0.8660254037844387076, 1.000000000000000000, 0.8660254037844387076, 1.000000000000000000, 0.8660254037844387076, 1.000000000000000000, 0.8660254037844387076, 1.000000000000000000, 0.8660254037844387076, 1.000000000000000000, 0.8660254037844387076, 1.000000000000000000, 0.8660254037844387076, 1.000000000000000000, 0.8660254037844387076, 1.000000000000000000, 0.8660254037844387076, 1.000000000000000000, 0.8660254037844387076, 1.000000000000000000, 0.8660254037844387076, 1.000000000000000000, 0.8660254037844387076, 1.000000000000000000, 0.8660254037844387076, 1.000000000000000000, 0.8660254037844387076, 1.000000000000000000, 0.8660254037844387076, 1.000000000000000000, 0.8660254037844387076, 1.000000000000000000, 0.8660254037844387076, 1.000000000000000000, 0.8660254037844387076, 1.000000000000000000, 0.8660254037844387076, 1.000000000000000000, 0.8660254037844387076, 1.000000000000000000, 0.8660254037844387076, 1.000000000000000000, 0.8660254037844387076, 1.000000000000000000, 0.8660254037844387076, 1.000000000000000000, 0.8660254037844387076, 1.000000000000000000, 0.8660254037844387076, 1.000000000000000000, 0.8660254037844387076, 1.000000000000000000, 0.8660254037844387076, 1.000000000000000000, 0.8660254037844387076, 1.000000000000000000, 0.8660254037844387076, 1.000000000000000000, 0.8660254037844387076, 1.000000000000000000, 0.8660254037844387076, 1.000000000000000000, 0.8660254037844387076, 1.000000000000000000, 0.8660254037844387076, 1.000000000000000000, 0.8660254037844387076, 1.000000000000000000, 0.8660254037844387076, 1.000000000000000000, 0.8660254037844387076, 1.000000000000000000, 0.8660254037844387076, 1.000000000000000000, 0.8660254037844387076, 1.000000000000000000, 0.8660254037844387076, 1.000000000000000000, 0.8660254037844387076, 1.000000000000000000, 0.8660254037844387076, 1.000000000000000000, 0.8660254037844387076, 1.000000000000000000, 0.8660254037844387076, 1.000000000000000000, 0.8660254037844387076, 1.000000000000000000, 0.8660254037844387076, 1.000000000000000000, 0.8660254037844387076, 1.000000000000000000, 0.8660254037844387076, 1.000000000000000000, 0.8660254037844387076, 1.000000000000000000),
 ( 1.000000000000000000, 0.8660254037844387076, 1.000000000000000000, 0.8660254037844387076, 1.000000000000000000, 0.8660254037844387076, 1.000000000000000000, 0.8660254037844387076, 1.000000000000000000, 0.8660254037844387076, 1.000000000000000000, 0.8660254037844387076, 1.000000000000000000, 0.8660254037844387076, 1.000000000000000000, 0.8660254037844387076, 1.000000000000000000, 0.8660254037844387076, 1.000000000000000000, 0.8660254037844387076, 1.000000000000000000, 0.8660254037844387076, 1.000000000000000000, 0.8660254037844387076, 1.000000000000000000, 0.8660254037844387076, 1.000000000000000000, 0.8660254037844387076, 1.000000000000000000, 0.8660254037844387076, 1.000000000000000000, 0.8660254037844387076, 1.000000000000000000, 0.8660254037844387076, 1.000000000000000000, 0.8660254037844387076, 1.000000000000000000, 0.8660254037844387076, 1.000000000000000000, 0.8660254037844387076, 1.000000000000000000, 0.8660254037844387076, 1.000000000000000000, 0.8660254037844387076, 1.000000000000000000, 0.8660254037844387076, 1.000000000000000000, 0.8660254037844387076, 1.000000000000000000, 0.8660254037844387076, 1.000000000000000000, 0.8660254037844387076, 1.000000000000000000, 0.8660254037844387076, 1.000000000000000000, 0.8660254037844387076, 1.000000000000000000, 0.8660254037844387076, 1.000000000000000000, 0.8660254037844387076, 1.000000000000000000, 0.8660254037844387076, 1.000000000000000000, 0.8660254037844387076, 1.000000000000000000, 0.8660254037844387076, 1.000000000000000000, 0.8660254037844387076, 1.000000000000000000, 0.8660254037844387076, 1.000000000000000000, 0.8660254037844387076, 1.000000000000000000, 0.8660254037844387076, 1.000000000000000000, 0.8660254037844387076, 1.000000000000000000, 0.8660254037844387076, 1.000000000000000000, 0.8660254037844387076, 1.000000000000000000, 0.8660254037844387076, 1.000000000000000000, 0.8660254037844387076, 1.000000000000000000, 0.8660254037844387076, 1.000000000000000000, 0.8660254037844387076, 1.000000000000000000, 0.8660254037844387076, 1.000000000000000000, 0.8660254037844387076, 1.000000000000000000, 0.8660254037844387076, 1.000000000000000000, 0.8660254037844387076, 1.000000000000000000, 0.8660254037844387076, 1.000000000000000000, 0.8660254037844387076, 1.000000000000000000, 0.8660254037844387076, 1.000000000000000000, 0.8660254037844387076, 1.000000000000000000, 0.8660254037844387076, 1.000000000000000000, 0.8660254037844387076, 1.000000000000000000, 0.8660254037844387076, 1.000000000000000000, 0.8660254037844387076, 1.000000000000000000, 0.8660254037844387076, 1.000000000000000000, 0.8660254037844387076, 1.000000000000000000, 0.8660254037844387076, 1.000000000000000000, 0.8660254037844387076, 1.000000000000000000, 0.8660254037844387076, 1.000000000000000000, 0.8660254037844387076, 1.000000000000000000, 0.8660254037844387076, 1.000000000000000000, 0.8660254037844387076, 1.000000000000000000, 0.8660254037844387076, 1.000000000000000000, 0.8660254037844387076, 1.000000000000000000, 0.8660254037844387076, 1.000000000000000000, 0.8660254037844387076, 1.000000000000000000, 0.8660254037844387076, 1.000000000000000000, 0.8660254037844387076, 1.000000000000000000, 0.8660254037844387076, 1.000000000000000000, 0.8660254037844387076, 1.000000000000000000, 0.8660254037844387076, 1.000000000000000000, 0.8660254037844387076, 1.000000000000000000, 0.8660254037844387076, 1.000000000000000000, 0.8660254037844387076, 1.000000000000000000, 0.8660254037844387076, 1.000000000000000000, 0.8660254037844387076, 1.000000000000000000, 0.8660254037844387076, 1.000000000000000000, 0.8660254037844387076, 1.000000000000000000, 0.8660254037844387076, 1.000000000000000000, 0.8660254037844387076, 1.000000000000000000, 0.8660254037844387076, 1.000000000000000000, 0.8660254037844387076, 1.000000000000000000, 0.8660254037844387076, 1.000000000000000000, 0.8660254037844387076, 1.000000000000000000, 0.8660254037844387076, 1.000000000000000000, 0.8660254037844387076, 1.000000000000000000, 0.8660254037844387076, 1.000000000000000000, 0.8660254037844387076, 1.000000000000000000, 0.8660254037844387076, 1.000000000000000000, 0.8660254037844387076, 1.000000000000000000, 0.8660254037844387076, 1.000000000000000000, 0.8660254037844387076, 1.000000000000000000, 0.8660254037844387076, 1.000000000000000000, 0.8660254037844387076, 1.000000000000000000, 0.8660254037844387076, 1.000000000000000000, 0.8660254037844387076, 1.000000000000000000, 0.8660254037844387076, 1.000000000000000000, 0.8660254037844387076, 1.000000000000000000, 0.8660254037844387076, 1.000000000000000000, 0.8660254037844387076, 1.000000000000000000, 0.8660254037844387076, 1.000000000000000000, 0.8660254037844387076, 1.000000000000000000, 0.8660254037844387076, 1.000000000000000000, 0.8660254037844387076, 1.000000000000000000, 0.8660254037844387076, 1.000000000000000000, 0.8660254037844387076, 1.000000000000000000, 0.8660254037844387076, 1.000000000000000000, 0.8660254037844387076, 1.000000000000000000, 0.8660254037844387076, 1.000000000000000000, 0.8660254037844387076, 1.000000000000000000, 0.8660254037844387076, 1.000000000000000000, 0.8660254037844387076, 1.000000000000000000, 0.8660254037844387076, 1.000000000000000000, 0.8660254037844387076, 1.000000000000000000, 0.8660254037844387076, 1.000000000000000000, 0.8660254037844387076, 1.000000000000000000, 0.8660254037844387076, 1.000000000000000000, 0.8660254037844387076, 1.000000000000000000, 0.8660254037844387076, 1.000000000000000000, 0.8660254037844387076, 1.000000000000000000, 0.8660254037844387076, 1.000000000000000000, 0.8660254037844387076, 1.000000000000000000, 0.8660254037844387076, 1.000000000000000000, 0.8660254037844387076, 1.000000000000000000, 0.8660254037844387076, 1.000000000000000000, 0.8660254037844387076, 1.000000000000000000, 0.8660254037844387076, 1.000000000000000000, 0.8660254037844387076, 1.000000000000000000, 0.8660254037844387076, 1.000000000000000000, 0.8660254037844387076, 1.000000000000000000, 0.8660254037844387076, 1.000000000000000000, 0.8660254037844387076, 1.000000000000000000, 0.8660254037844387076, 1.000000000000000000, 0.8660254037844387076, 1.000000000000000000, 0.8660254037844387076, 1.000000000000000000, 0.8660254037844387076, 1.000000000000000000, 0.8660254037844387076, 1.000000000000000000, 0.8660254037844387076, 1.000000000000000000, 0.8660254037844387076, 1.000000000000000000, 0.8660254037844387076, 1.000000000000000000, 0.8660254037844387076, 1.000000000000000000, 0.8660254037844387076, 1.000000000000000000, 0.8660254037844387076, 1.000000000000000000, 0.8660254037844387076, 1.000000000000000000, 0.8660254037844387076, 1.000000000000000000, 0.8660254037844387076, 1.000000000000000000, 0.8660254037844387076, 1.000000000000000000, 0.8660254037844387076, 1.000000000000000000, 0.8660254037844387076, 1.000000000000000000, 0.8660254037844387076, 1.000000000000000000, 0.8660254037844387076, 1.000000000000000000, 0.8660254037844387076, 1.000000000000000000, 0.8660254037844387076, 1.000000000000000000, 0.8660254037844387076, 1.000000000000000000, 0.8660254037844387076, 1.000000000000000000, 0.8660254037844387076, 1.000000000000000000, 0.8660254037844387076, 1.000000000000000000, 0.8660254037844387076, 1.000000000000000000, 0.8660254037844387076, 1.000000000000000000, 0.8660254037844387076, 1.000000000000000000, 0.8660254037844387076, 1.000000000000000000, 0.8660254037844387076, 1.000000000000000000, 0.8660254037844387076, 1.000000000000000000, 0.8660254037844387076, 1.000000000000000000, 0.8660254037844387076, 1.000000000000000000, 0.8660254037844387076, 1.000000000000000000) ) ) 
 REPRESENTATION_ITEM ( '' )  SURFACE ( )  );
#87993 = CARTESIAN_POINT ( 'NONE',  ( 5.924064563541377559, -1.897137492723115049, 0.2407653536913647030 ) ) ;
#87994 = CARTESIAN_POINT ( 'NONE',  ( 5.559779856078610472, 1.205038519190555268, 1.616695979245158066 ) ) ;
#87995 =( REPRESENTATION_RELATIONSHIP ('NONE','NONE', #84563, #99753 ) REPRESENTATION_RELATIONSHIP_WITH_TRANSFORMATION ( #172763 )SHAPE_REPRESENTATION_RELATIONSHIP( ) );
#87997 = SURFACE_SIDE_STYLE ('',( #184410 ) ) ;
#87996 = CARTESIAN_POINT ( 'NONE',  ( -8.636707547105197946, 10.03491254549959777, -1.199719254218446718 ) ) ;
#87998 = CARTESIAN_POINT ( 'NONE',  ( -1.642778471874998480, -2.238541666188708312, 2.845375778867863303 ) ) ;
#88000 = CARTESIAN_POINT ( 'NONE',  ( 1.727073733189425031, -1.667858853059518420, 0.5925122568580538651 ) ) ;
#87999 = CARTESIAN_POINT ( 'NONE',  ( 2.255913092623571092, 0.8947350874906587759, 1.889642235345281307 ) ) ;
#88001 = CARTESIAN_POINT ( 'NONE',  ( -0.3553982319964891778, -6.532648833121158738, -9.473247973006305500 ) ) ;
#88003 = CARTESIAN_POINT ( 'NONE',  ( 3.802894434091105946, 1.965436290923015639, 1.179407150283459105 ) ) ;
#88002 = CARTESIAN_POINT ( 'NONE',  ( 5.273195401072370281, 5.116759154198018855, -0.7998128361456481317 ) ) ;
#88004 = CARTESIAN_POINT ( 'NONE',  ( 2.905909708737213659, 1.260233761464889302, -1.200475698291984861 ) ) ;
#88005 = CARTESIAN_POINT ( 'NONE',  ( 9.999301985278609806, 11.62460605670194447, 1.199719254218452047 ) ) ;
#88006 = CARTESIAN_POINT ( 'NONE',  ( -2.679885790744698681, -0.4618020869171932108, -0.1056289066552756756 ) ) ;
#88007 = CARTESIAN_POINT ( 'NONE',  ( 2.582960874182936628, 1.135899660060729399, -1.309998962497432196 ) ) ;
#88008 = CARTESIAN_POINT ( 'NONE',  ( 3.631445352573436480, 0.05657863903951602241, -2.170607583040237820 ) ) ;
#88009 = CARTESIAN_POINT ( 'NONE',  ( 5.009901455449552010, 5.803638771901306725, -1.199719254218452047 ) ) ;
#88010 = CARTESIAN_POINT ( 'NONE',  ( 4.522672878804367969, 0.3494810548456111499, 1.985869246038343583 ) ) ;
#88011 = CARTESIAN_POINT ( 'NONE',  ( 2.437500000000002220, 1.451031289061020857, -1.451031289061217366 ) ) ;
#88012 = CARTESIAN_POINT ( 'NONE',  ( -1.499999999999997780, 3.181250000682818602, 1.214306433183764966E-14 ) ) ;
#88013 = CARTESIAN_POINT ( 'NONE',  ( 1.254767684091241620, -1.520462189517374219, 1.182783339890740359 ) ) ;
#88014 = CARTESIAN_POINT ( 'NONE',  ( -0.7500000000000006661, 8.739583334016129967, -1.299038105676657340 ) ) ;
#88015 = CARTESIAN_POINT ( 'NONE',  ( 4.430067838210618447, -2.178247905445731103, 0.4349904863075284567 ) ) ;
#88016 = ORIENTED_EDGE ( 'NONE', *, *, #164742, .F. ) ;
#88017 = CARTESIAN_POINT ( 'NONE',  ( -0.1108833634137010304, 7.629137130509073828, -2.496956624467902675 ) ) ;
#88018 = CARTESIAN_POINT ( 'NONE',  ( -1.500000000000013101, -0.07916666666664513852, 0.8660254037844403729 ) ) ;
#88019 = CARTESIAN_POINT ( 'NONE',  ( 7.076466111328892694, 10.34329533227067799, -1.199719254218441611 ) ) ;
#88020 = CARTESIAN_POINT ( 'NONE',  ( -1.642778471875000035, -1.917708332855375897, -2.845375778867859751 ) ) ;
#88021 = CARTESIAN_POINT ( 'NONE',  ( 0.8916360836422586589, -0.05999620363036740206, -2.220659203727569420 ) ) ;
#88022 = CARTESIAN_POINT ( 'NONE',  ( 5.810985101215744741, -1.547553103248515027, 1.205733875218002238 ) ) ;
#88023 = CARTESIAN_POINT ( 'NONE',  ( 7.917598520700710019, 12.18102267421877727, -0.7216878364870328300 ) ) ;
#88024 = DIRECTION ( 'NONE',  ( -0.9982742078614211811, 0.000000000000000000, -0.05872483221476467591 ) ) ;
#88025 = CARTESIAN_POINT ( 'NONE',  ( 6.555986116969920730, 2.257040928323080564, -0.1566935481548906162 ) ) ;
#88026 = CARTESIAN_POINT ( 'NONE',  ( -5.695833931516914639, 6.778132687258748845, 1.082531754730549078 ) ) ;
#88027 = CARTESIAN_POINT ( 'NONE',  ( 3.543474241949475356, 1.865888119384132127, -0.8795106731672995837 ) ) ;
#88028 = CARTESIAN_POINT ( 'NONE',  ( -5.362413449404877852, 6.214902764849178141, -1.199719254218446718 ) ) ;
#88030 = EDGE_CURVE ( 'NONE', #93560, #155662, #115675, .T. ) ;
#88029 = CARTESIAN_POINT ( 'NONE',  ( -1.499999999999997780, 3.431250000682818602, 1.214306433183764966E-14 ) ) ;
#88031 = CARTESIAN_POINT ( 'NONE',  ( 1.364683531249986981, -1.115624999658580752, 0.000000000000000000 ) ) ;
#88032 = CARTESIAN_POINT ( 'NONE',  ( 5.307814152003552444, -1.861618091082300808, 0.1822119596564600597 ) ) ;
#88033 = CARTESIAN_POINT ( 'NONE',  ( 3.937908632975633871, -1.444535402496229137, -0.9590898762639500363 ) ) ;
#88034 = CARTESIAN_POINT ( 'NONE',  ( 3.403587037673636129, -0.7086591031593177936, -1.589830453666951415 ) ) ;
#88035 = CARTESIAN_POINT ( 'NONE',  ( 0.5215107003284430442, -2.174349661526672417, 0.7262685697029276355 ) ) ;
#88036 = CARTESIAN_POINT ( 'NONE',  ( -1.201851678989727383E-14, 4.134375000341417028, 1.575800808251672791 ) ) ;
#88037 = CARTESIAN_POINT ( 'NONE',  ( 5.126549769544753055, 0.1549841644245806838, 2.085076985156742779 ) ) ;
#88038 = CARTESIAN_POINT ( 'NONE',  ( 6.714805131850001274, -0.1305238817815305985, 1.911932681171425896 ) ) ;
#88039 = EDGE_CURVE ( 'NONE', #196836, #88097, #125428, .T. ) ;
#88041 = ORIENTED_EDGE ( 'NONE', *, *, #113537, .T. ) ;
#88040 = CARTESIAN_POINT ( 'NONE',  ( 0.4499999999999834133, 3.949999999999988187, -0.5000000000000299760 ) ) ;
#88042 = CARTESIAN_POINT ( 'NONE',  ( 0.6334356698059575574, 0.5880228326464317368, 1.928751028484784413 ) ) ;
#88043 = CARTESIAN_POINT ( 'NONE',  ( 0.9672155168029163974, -1.668165459610539081, 1.309123814877902969 ) ) ;
#88044 = CARTESIAN_POINT ( 'NONE',  ( 6.925078400183534377, -0.01048729610059368801, 2.244148362790527873 ) ) ;
#88045 = PLANE ( 'NONE',  #96791 ) ;
#88046 = CARTESIAN_POINT ( 'NONE',  ( -9.013473194986783454, 9.410140237106395134, -0.7998128361456291469 ) ) ;
#88047 = CARTESIAN_POINT ( 'NONE',  ( 5.361359679200154105, 8.342337828120466980, 1.199719254218462483 ) ) ;
#88048 = CARTESIAN_POINT ( 'NONE',  ( 2.174623584685225541, 0.9092215167782154994, 1.915816808323366871 ) ) ;
#88049 = CARTESIAN_POINT ( 'NONE',  ( 0.000000000000000000, -4.500000000000003553, 0.000000000000000000 ) ) ;
#88050 = CARTESIAN_POINT ( 'NONE',  ( 4.494645072041675071, -0.4025399330690944133, -1.780595394402582077 ) ) ;
#88051 = ORIENTED_EDGE ( 'NONE', *, *, #87175, .T. ) ;
#88052 = CARTESIAN_POINT ( 'NONE',  ( -7.119966945832006289, 8.335658187339330283, 1.199719254218452047 ) ) ;
#88053 = CARTESIAN_POINT ( 'NONE',  ( -0.4644097342743094270, -8.233137084989863297, -9.488641820551086070 ) ) ;
#88054 = CARTESIAN_POINT ( 'NONE',  ( 1.737499999999999378, -4.272916665710751793, -3.009438278150925683 ) ) ;
#88055 = CARTESIAN_POINT ( 'NONE',  ( -6.693975156845199059, 8.832723654451292816, 1.599625672291283607 ) ) ;
#88056 = CARTESIAN_POINT ( 'NONE',  ( 2.513930914015961804, -0.6297079463782135900, 1.919214091249999088 ) ) ;
#88057 = CARTESIAN_POINT ( 'NONE',  ( 5.192482782645277517, -2.189556457885518892, -0.2746672974567528347 ) ) ;
#88058 = CARTESIAN_POINT ( 'NONE',  ( -3.772911886352873445, 7.623757310712140800, 0.7998128361456352531 ) ) ;
#88059 = CARTESIAN_POINT ( 'NONE',  ( 3.731172809088632025, 0.04972793443442201367, -1.860468898575567520 ) ) ;
#88060 = CARTESIAN_POINT ( 'NONE',  ( 9.836604141914616406, 11.43479190611061647, 1.199719254218452047 ) ) ;
#88061 = CARTESIAN_POINT ( 'NONE',  ( 10.50000000000000178, 12.59159113040219857, -3.600000000000000977 ) ) ;
#88062 = VERTEX_POINT ( 'NONE', #145254 ) ;
#88063 = ORIENTED_EDGE ( 'NONE', *, *, #1238, .F. ) ;
#88064 = CARTESIAN_POINT ( 'NONE',  ( -5.251085567194491155, 5.020688004682002159, -0.7998128361456221525 ) ) ;
#88065 = CARTESIAN_POINT ( 'NONE',  ( -9.806625181386236179, 10.33548422123910449, -0.7998128361456291469 ) ) ;
#88066 = CARTESIAN_POINT ( 'NONE',  ( 4.635264976507449397, -1.668059998867366778, 0.7425182445051290436 ) ) ;
#88068 = CARTESIAN_POINT ( 'NONE',  ( -4.646091124696241081, 7.101299429195864654, -1.386232413501260474 ) ) ;
#88067 = CARTESIAN_POINT ( 'NONE',  ( -4.950662367645459305, 5.804802846121667415, -1.199719254218453823 ) ) ;
#88069 = CARTESIAN_POINT ( 'NONE',  ( 4.936581118797800372, 8.100871430792054184, -1.059671831818540966 ) ) ;
#88070 = CARTESIAN_POINT ( 'NONE',  ( 0.4909827745146425060, 1.656533638411663345, 0.5119339833263967243 ) ) ;
#88071 = CARTESIAN_POINT ( 'NONE',  ( 6.650350966976619205, -1.419654684173769166, 1.172063944840713523 ) ) ;
#88072 = CARTESIAN_POINT ( 'NONE',  ( 5.672612835131308984, -1.468196381517340665, 1.780430754307258390 ) ) ;
#88073 = CARTESIAN_POINT ( 'NONE',  ( 4.044074958626150185, 7.940114228364351767, 0.7998128361456271485 ) ) ;
#88074 = CARTESIAN_POINT ( 'NONE',  ( 1.124374118904346798, 1.229854006068244132, -1.653384075620732307 ) ) ;
#88075 = CARTESIAN_POINT ( 'NONE',  ( 4.808338034340912337, 8.761478140039733020, 1.040834085586084257E-14 ) ) ;
#88076 = CARTESIAN_POINT ( 'NONE',  ( 0.5794536021234627521, 1.392335491182377316, -1.458330535474762213 ) ) ;
#88077 = FACE_OUTER_BOUND ( 'NONE', #62429, .T. ) ;
#88079 = AXIS2_PLACEMENT_3D ( 'NONE', #135401, #22672, #18425 ) ;
#88078 = CARTESIAN_POINT ( 'NONE',  ( -6.774234028683526532, 7.932303117332766718, 1.199719254218452047 ) ) ;
#88080 = CARTESIAN_POINT ( 'NONE',  ( 5.823093596695693819, -0.04436734784114480107, 1.870300906237104988 ) ) ;
#88081 = VECTOR ( 'NONE', #123728, 1000.000000000000000 ) ;
#88083 = CARTESIAN_POINT ( 'NONE',  ( -3.122120512896910505, 6.864500708346841229, 0.7998128361456352531 ) ) ;
#88082 = CARTESIAN_POINT ( 'NONE',  ( 3.375170810042011915, -1.688748480992762868, -0.8973671847329609541 ) ) ;
#88084 = B_SPLINE_CURVE_WITH_KNOTS ( 'NONE', 3,
 ( #197868, #98262, #184810, #182685, #81992, #130824 ),
 .UNSPECIFIED., .F., .F.,
 ( 4, 2, 4 ),
 ( 0.000000000000000000, 0.0003155923098472861849, 0.0006311846196945723698 ),
 .UNSPECIFIED. ) ;
#88085 = CARTESIAN_POINT ( 'NONE',  ( 5.162800556355915838, -1.600310254184673431, 1.519886962452212664 ) ) ;
#88086 = CARTESIAN_POINT ( 'NONE',  ( 1.224999999999969225, 1.937500000682795820, -2.081668171172168513E-14 ) ) ;
#88087 = CARTESIAN_POINT ( 'NONE',  ( -7.065207446052809814, 9.336104335185325453, -1.443375672974066548 ) ) ;
#88088 = CARTESIAN_POINT ( 'NONE',  ( 5.356880090730874677, 5.422317325373725794, 0.7216878364870328300 ) ) ;
#88089 = CARTESIAN_POINT ( 'NONE',  ( -4.123088111887291518, 7.824370207261548416, 0.000000000000000000 ) ) ;
#88090 = CARTESIAN_POINT ( 'NONE',  ( 5.848313825214911610, 1.045240856298999432, -1.844880668361434939 ) ) ;
#88091 = CARTESIAN_POINT ( 'NONE',  ( 3.083396755883772933, -0.1683641986609325514, -2.301487591144059763 ) ) ;
#88092 = CARTESIAN_POINT ( 'NONE',  ( 4.035565188342554954, 1.848088059160474694, -0.6588067414724924076 ) ) ;
#88093 = CARTESIAN_POINT ( 'NONE',  ( -5.418418667316934112, 6.350518529071726981, -1.199719254218453823 ) ) ;
#88094 = CARTESIAN_POINT ( 'NONE',  ( 1.041763817972749750, 1.313373124611896703, 1.457441342770829262 ) ) ;
#88095 = CARTESIAN_POINT ( 'NONE',  ( 9.276214967470513884, 13.85813420416141639, 7.540790294154477991 ) ) ;
#88096 = CARTESIAN_POINT ( 'NONE',  ( 3.555981428534177091, 7.370671776590375757, 0.7998128361456271485 ) ) ;
#88097 = VERTEX_POINT ( 'NONE', #13057 ) ;
#88098 = CARTESIAN_POINT ( 'NONE',  ( 6.051970301643104122, 1.040788372175960541, 1.727066800951609249 ) ) ;
#88099 = CARTESIAN_POINT ( 'NONE',  ( -8.025536864285518490, 11.45054454405341282, -1.199719254218446718 ) ) ;
#88101 = CARTESIAN_POINT ( 'NONE',  ( 0.3218710511002781383, 1.760991339961643920, 0.5373333866721883290 ) ) ;
#88100 = CIRCLE ( 'NONE', #160768, 0.08000000000000025147 ) ;
#88102 = LINE ( 'NONE', #133952, #87006 ) ;
#88103 = CARTESIAN_POINT ( 'NONE',  ( 2.588947950494639993, 2.104950400290429791, 0.5311738530254602741 ) ) ;
#88104 = DIRECTION ( 'NONE',  ( -0.000000000000000000, -1.000000000000000000, -0.000000000000000000 ) ) ;
#88105 = CARTESIAN_POINT ( 'NONE',  ( 0.3344391967911933272, -1.139684030083350841, -1.788147294700337397 ) ) ;
#88106 = CARTESIAN_POINT ( 'NONE',  ( -1.500000000000015099, 1.160416667349484898, -0.8660254037844313801 ) ) ;
#88107 = CARTESIAN_POINT ( 'NONE',  ( 10.37606763316019531, 10.99983374830873650, 0.7998128361456462443 ) ) ;
#88108 = CARTESIAN_POINT ( 'NONE',  ( 1.854512760316388897, 2.488359591189891251, 2.484105960264901825 ) ) ;
#88109 = CARTESIAN_POINT ( 'NONE',  ( 5.820234798683411981, 7.319712794923219690, 1.284739950006764220 ) ) ;
#88110 = ORIENTED_EDGE ( 'NONE', *, *, #199274, .F. ) ;
#88111 = CARTESIAN_POINT ( 'NONE',  ( 0.4212572661226633985, -0.1035701926632242170, 2.058322702938982562 ) ) ;
#88113 = DIRECTION ( 'NONE',  ( 0.000000000000000000, 0.000000000000000000, 1.000000000000000000 ) ) ;
#88112 = CARTESIAN_POINT ( 'NONE',  ( -9.667127221743832877, 11.23706883257798772, 1.199719254218462483 ) ) ;
#88114 = CARTESIAN_POINT ( 'NONE',  ( 1.364683531249988757, 1.634375000341421691, 0.000000000000000000 ) ) ;
#88115 = CARTESIAN_POINT ( 'NONE',  ( 6.076298462418691315, 7.128931413452940014, -1.143247356662546732 ) ) ;
#88116 = ORIENTED_EDGE ( 'NONE', *, *, #13918, .T. ) ;
#88117 = CARTESIAN_POINT ( 'NONE',  ( 3.053266463924544372, -1.685387242695039811, 0.9035085923766730254 ) ) ;
#88118 = CARTESIAN_POINT ( 'NONE',  ( 5.506658716161647149, 1.338116961444441921, -1.158480101542769036 ) ) ;
#88119 = CARTESIAN_POINT ( 'NONE',  ( 6.900173834712277632, 7.014900660111269559, -0.7998128361456341429 ) ) ;
#88120 = CARTESIAN_POINT ( 'NONE',  ( -4.440459003675619520, 5.139289244831666714, 1.199719254218462483 ) ) ;
#88121 = CARTESIAN_POINT ( 'NONE',  ( 0.4042039562905282435, -1.797914468929398879, -0.2212116797051487393 ) ) ;
#88123 = CARTESIAN_POINT ( 'NONE',  ( 0.7432033230480495911, 0.3705163548812146490, -1.879356322977752347 ) ) ;
#88122 = CARTESIAN_POINT ( 'NONE',  ( 4.044555541517573793, 7.746237447724527492, 0.4662041258270445132 ) ) ;
#88124 = CARTESIAN_POINT ( 'NONE',  ( 2.400909748719297188, 0.4512941399696759337, 2.020426262116347349 ) ) ;
#88125 = CARTESIAN_POINT ( 'NONE',  ( 1.364683531249986537, -0.07395833299191513499, 0.7879004041258500513 ) ) ;
#88126 = CARTESIAN_POINT ( 'NONE',  ( 6.702024585102262400, -1.870183347854617040, 0.04844413084104796929 ) ) ;
#88127 = CARTESIAN_POINT ( 'NONE',  ( 2.877373901574116211, 1.733520850877915187, -0.5729475677913041798 ) ) ;
#88129 = CARTESIAN_POINT ( 'NONE',  ( 6.385878362533466301, 6.816559200039058020, 0.5486352003098924346 ) ) ;
#88128 = CARTESIAN_POINT ( 'NONE',  ( 6.727182134110200273, -0.004969159814478123736, 2.189081792362323586 ) ) ;
#88130 = CARTESIAN_POINT ( 'NONE',  ( -1.402160292154681736E-14, 0.3218750003414227456, 1.575800808251672791 ) ) ;
#88131 = CARTESIAN_POINT ( 'NONE',  ( 3.859879052112312969, -0.6014189565349871147, 1.973034901002912678 ) ) ;
#88132 = CARTESIAN_POINT ( 'NONE',  ( -5.228640796364566690, 9.251831362400652736, -0.7998128361456231517 ) ) ;
#88133 = CARTESIAN_POINT ( 'NONE',  ( 6.591235234537977661, 10.84152487360300299, 0.7998128361456462443 ) ) ;
#88134 = CARTESIAN_POINT ( 'NONE',  ( 4.680589345215795838, 6.483773540883647435, -1.599625672291256517 ) ) ;
#88136 = CARTESIAN_POINT ( 'NONE',  ( 0.7202740732663616141, -1.155732025818452913, -1.826486478054230256 ) ) ;
#88135 = CIRCLE ( 'NONE', #136536, 0.07999999999999993228 ) ;
#88137 = CARTESIAN_POINT ( 'NONE',  ( 6.725056259267968350, -1.891221747171191403, -0.8428681758992571105 ) ) ;
#88138 = CARTESIAN_POINT ( 'NONE',  ( -1.364683531250000748, 1.821875000341421913, 0.000000000000000000 ) ) ;
#88139 = CARTESIAN_POINT ( 'NONE',  ( 3.936934155531632396, 0.3128429973590241553, 2.138701728237289768 ) ) ;
#88140 = CARTESIAN_POINT ( 'NONE',  ( 4.442060220718175856, -1.244341337028841421, -1.590709041654225553 ) ) ;
#88141 = CARTESIAN_POINT ( 'NONE',  ( 4.879147978569815969, 4.879180288469956217, -0.1512534140984626019 ) ) ;
#88142 = VECTOR ( 'NONE', #35468, 1000.000000000000000 ) ;
#88143 = EDGE_CURVE ( 'NONE', #19657, #125687, #208203, .T. ) ;
#88146 = CARTESIAN_POINT ( 'NONE',  ( 7.483737605063422116, 7.833374748769873719, -0.7216878364870257245 ) ) ;
#88145 = CARTESIAN_POINT ( 'NONE',  ( -3.285556943750000514, -3.638541666188706891, -1.896917185911906500 ) ) ;
#88144 = LINE ( 'NONE', #55636, #28262 ) ;
#88147 = CARTESIAN_POINT ( 'NONE',  ( -6.414942957921379474, 7.513130201443591005, -1.199719254218452047 ) ) ;
#88148 = CARTESIAN_POINT ( 'NONE',  ( 2.483611571103708116, -0.6279893487078171965, 1.916353726171161620 ) ) ;
#88149 = CARTESIAN_POINT ( 'NONE',  ( -7.714753101375940503, 8.959299025482085455, 1.199719254218462483 ) ) ;
#88150 = CARTESIAN_POINT ( 'NONE',  ( -4.952806187693842510, 4.672695395264567786, 0.7998128361456341429 ) ) ;
#88151 = CARTESIAN_POINT ( 'NONE',  ( 6.670655732516623360, 7.629137130509072051, 2.773739711112707784 ) ) ;
#88152 = CARTESIAN_POINT ( 'NONE',  ( 5.414289803398987466, -1.912571729023364364, 0.006307610287324683096 ) ) ;
#88153 = DIRECTION ( 'NONE',  ( 0.000000000000000000, 0.000000000000000000, 1.000000000000000000 ) ) ;
#88154 = CARTESIAN_POINT ( 'NONE',  ( 4.324687812634874895, 7.989293514808604613, 0.7216878364870317197 ) ) ;
#88156 = CARTESIAN_POINT ( 'NONE',  ( 4.833611329963474645, 0.6298591494234163646, -1.915606498650752831 ) ) ;
#88155 = CARTESIAN_POINT ( 'NONE',  ( -7.117667457050096402, 10.28740055232499984, 1.082531754730549967 ) ) ;
#88157 = CARTESIAN_POINT ( 'NONE',  ( -1.500000000000011324, 5.170833333333356485, 0.8660254037844403729 ) ) ;
#88158 = CARTESIAN_POINT ( 'NONE',  ( -8.012344526598182026E-15, 14.85937500034139980, -1.575800808251669460 ) ) ;
#88159 = CARTESIAN_POINT ( 'NONE',  ( 6.229511965242640059, -1.622199917339474329, 0.5863599495292673991 ) ) ;
#88160 = CARTESIAN_POINT ( 'NONE',  ( 4.213551878797002992, 8.137837301896977849, 0.000000000000000000 ) ) ;
#88162 = DIRECTION ( 'NONE',  ( 7.993605777301127091E-15, 0.000000000000000000, -1.000000000000000000 ) ) ;
#88161 = CARTESIAN_POINT ( 'NONE',  ( 8.093854517678360949, 12.38665467069271386, 1.040834085586084257E-14 ) ) ;
#88163 = CARTESIAN_POINT ( 'NONE',  ( 5.008994926481016741, 1.626754543590884561, 0.9232732976792232815 ) ) ;
#88164 = CARTESIAN_POINT ( 'NONE',  ( 6.047140908842845164, 0.2017661761196144488, 2.003097277516131758 ) ) ;
#88165 =( NAMED_UNIT ( * ) PLANE_ANGLE_UNIT ( ) SI_UNIT ( $, .RADIAN. ) );
#88166 = CARTESIAN_POINT ( 'NONE',  ( 2.606376076552410659, 2.069701014239883730, 0.05521581806712527740 ) ) ;
#88167 = CARTESIAN_POINT ( 'NONE',  ( -1.419999999067534713, 7.203691543881443948, -4.238255391841854625 ) ) ;
#88168 = ORIENTED_EDGE ( 'NONE', *, *, #30238, .T. ) ;
#88169 = B_SPLINE_CURVE_WITH_KNOTS ( 'NONE', 3,
 ( #177308, #146960, #212975, #195689, #97142, #28923 ),
 .UNSPECIFIED., .F., .F.,
 ( 4, 2, 4 ),
 ( 0.001259240562161249421, 0.001573673787268791650, 0.001888107012376333878 ),
 .UNSPECIFIED. ) ;
#88170 = CARTESIAN_POINT ( 'NONE',  ( 0.4566579290818244541, -1.899626807963299635, -0.6766942018802262204 ) ) ;
#88171 = CARTESIAN_POINT ( 'NONE',  ( 4.299344108864946890, 6.109263775132799168, -1.443375672974068769 ) ) ;
#88172 = DIRECTION ( 'NONE',  ( 0.000000000000000000, 0.000000000000000000, 1.000000000000000000 ) ) ;
#88173 = CARTESIAN_POINT ( 'NONE',  ( 6.575341312503417690, 10.61505593132193326, -0.7216878364870267237 ) ) ;
#88174 = ADVANCED_FACE ( 'NONE', ( #8804 ), #92227, .T. ) ;
#88175 = CARTESIAN_POINT ( 'NONE',  ( 6.751070424600909448, 9.963667031088037973, -1.199719254218441611 ) ) ;
#88176 = AXIS2_PLACEMENT_3D ( 'NONE', #21465, #139545, #52930 ) ;
#88178 = CARTESIAN_POINT ( 'NONE',  ( 6.345329912860430355, 0.3219833572893218698, -1.888178885089139669 ) ) ;
#88177 = CARTESIAN_POINT ( 'NONE',  ( -5.032047568966410367, 9.022472597102808578, 1.214306433183764966E-14 ) ) ;
#88179 = CARTESIAN_POINT ( 'NONE',  ( -9.579665964948885559, -7.246166700194470067, -0.07999999999998980149 ) ) ;
#88180 = CARTESIAN_POINT ( 'NONE',  ( -1.456858692995781412, -3.148926244281702314, 3.052706761563094950 ) ) ;
#88181 = CARTESIAN_POINT ( 'NONE',  ( -0.6823417656250003738, -0.9697916663252494907, -1.181850606188749264 ) ) ;
#88183 = ORIENTED_EDGE ( 'NONE', *, *, #212623, .T. ) ;
#88182 = CARTESIAN_POINT ( 'NONE',  ( 4.446711195602238931, 6.210915699667823198, -1.443375672974051449 ) ) ;
#88184 = CARTESIAN_POINT ( 'NONE',  ( -4.810445574750349174, 4.506608013497163334, 0.7998128361456341429 ) ) ;
#88185 = CARTESIAN_POINT ( 'NONE',  ( -6.887178846062105286, 10.97886638714038554, -0.7216878364870267237 ) ) ;
#88186 = CARTESIAN_POINT ( 'NONE',  ( 2.588937169860201504, -0.3686131662095324391, -2.129881858774537395 ) ) ;
#88187 = CARTESIAN_POINT ( 'NONE',  ( -7.770231434407805615, 8.237893892996801526, 0.000000000000000000 ) ) ;
#88188 = CARTESIAN_POINT ( 'NONE',  ( 4.909461021924231616, 8.741805268971372556, 0.7216878364870317197 ) ) ;
#88189 = CARTESIAN_POINT ( 'NONE',  ( 0.7387272492362946252, 1.258454933865692293, -1.706699550108881080 ) ) ;
#88190 = CARTESIAN_POINT ( 'NONE',  ( 5.948246703923279810, 1.823645139926059144, 0.08696428134234018836 ) ) ;
#88191 = CARTESIAN_POINT ( 'NONE',  ( 2.706272882855005335, -0.7510657119417161187, -1.822867458954416708 ) ) ;
#88192 = CARTESIAN_POINT ( 'NONE',  ( 4.236511230858605259, 1.172298487584079396, -1.510895503047122945 ) ) ;
#88193 = VERTEX_POINT ( 'NONE', #127996 ) ;
#88194 = CARTESIAN_POINT ( 'NONE',  ( 4.510180775305682843, 1.969176117969779982, -0.04608634298608124680 ) ) ;
#88195 = CARTESIAN_POINT ( 'NONE',  ( 0.9021669503554888836, 1.471007182523446311, -1.267884427665219471 ) ) ;
#88196 = ORIENTED_EDGE ( 'NONE', *, *, #141409, .F. ) ;
#88197 = CARTESIAN_POINT ( 'NONE',  ( -6.296835998904160014, 6.311006518335105397, 0.000000000000000000 ) ) ;
#88199 = CARTESIAN_POINT ( 'NONE',  ( -0.4041367621137837984, 3.038026290190025236, 0.4210133165200240501 ) ) ;
#88198 = CARTESIAN_POINT ( 'NONE',  ( -4.984557751679625781, 5.844347460828191565, 1.199719254218452935 ) ) ;
#88201 = CARTESIAN_POINT ( 'NONE',  ( 6.522881301506172846, 6.782652071278222117, -0.7216878364870458196 ) ) ;
#88200 = CARTESIAN_POINT ( 'NONE',  ( 6.825640269476072497, 10.05066518344239412, 1.199719254218460707 ) ) ;
#88203 = EDGE_LOOP ( 'NONE', ( #96806, #141257 ) ) ;
#88202 = CARTESIAN_POINT ( 'NONE',  ( 5.567032834676129305, -1.504811603839781631, 1.179860560037985895 ) ) ;
#88204 = ADVANCED_FACE ( 'NONE', ( #62883 ), #157208, .T. ) ;
#88205 = CARTESIAN_POINT ( 'NONE',  ( 1.079469989902905214, -0.05558308599296066244, -2.206230565744627281 ) ) ;
#88206 = EDGE_CURVE ( 'NONE', #96770, #184855, #212880, .T. ) ;
#88207 = DIRECTION ( 'NONE',  ( 1.000000000000000000, -0.000000000000000000, -0.000000000000000000 ) ) ;
#88208 = CARTESIAN_POINT ( 'NONE',  ( 6.305343602688459725, 1.750316497599126331, -0.9943532346578187742 ) ) ;
#88209 = CARTESIAN_POINT ( 'NONE',  ( -0.02338929933905566777, 0.2563879980532010605, -1.746150209723141167 ) ) ;
#88210 = CARTESIAN_POINT ( 'NONE',  ( -6.177748251148500458, 7.053635085330046905, 1.079103885897433779 ) ) ;
#88211 = CARTESIAN_POINT ( 'NONE',  ( 6.953912913643685911, -8.144978210217292514, -6.511381374296902003 ) ) ;
#88212 = CARTESIAN_POINT ( 'NONE',  ( 2.664580169416390643, -0.7900844611210651180, -1.913877855911281012 ) ) ;
#88213 = CARTESIAN_POINT ( 'NONE',  ( -7.400052914960538963, 7.527816577075747695, 1.040834085586084257E-14 ) ) ;
#88214 = CARTESIAN_POINT ( 'NONE',  ( -4.612386318492403880, 8.373339136000554461, 0.1892495524792922046 ) ) ;
#88216 = CARTESIAN_POINT ( 'NONE',  ( 0.9015118058452382677, 1.767791302423503685, 1.243857928393626633 ) ) ;
#88215 = CARTESIAN_POINT ( 'NONE',  ( -2.740719608256871442, 6.349256642941639051, 0.7998128361456341429 ) ) ;
#88217 = CARTESIAN_POINT ( 'NONE',  ( -11.75716154505269984, 8.610272713044158976, -2.418301517245814658 ) ) ;
#88218 = CARTESIAN_POINT ( 'NONE',  ( 4.421367491832268293, 7.211993602896056288, 1.082531754730549078 ) ) ;
#88219 = CARTESIAN_POINT ( 'NONE',  ( 0.000000000000000000, 0.000000000000000000, 0.000000000000000000 ) ) ;
#88220 = CARTESIAN_POINT ( 'NONE',  ( 1.364683531249996529, 13.02604166700806410, 0.7879004041258405033 ) ) ;
#88222 = CARTESIAN_POINT ( 'NONE',  ( -4.522526758610270647, 7.433975764090723359, -1.199719254218453823 ) ) ;
#88221 = CARTESIAN_POINT ( 'NONE',  ( 6.825078400183593352, 2.989295776279639938, 2.209688085509611710 ) ) ;
#88224 = CARTESIAN_POINT ( 'NONE',  ( 4.289544331642456854, 1.336530783054422189, -1.104934575851760137 ) ) ;
#88223 = AXIS2_PLACEMENT_3D ( 'NONE', #74655, #90922, #43242 ) ;
#88225 = CARTESIAN_POINT ( 'NONE',  ( -4.115063316947640715, 4.759660943649018705, 1.199719254218462483 ) ) ;
#88226 = CARTESIAN_POINT ( 'NONE',  ( 2.448173108494243078, -0.8891298726186761536, 1.869765896676472083 ) ) ;
#88227 = CARTESIAN_POINT ( 'NONE',  ( 4.446934944069580453, -1.891868754433777555, -0.9506184929228760350 ) ) ;
#88228 = CIRCLE ( 'NONE', #171257, 2.500000000000000888 ) ;
#88229 = CARTESIAN_POINT ( 'NONE',  ( 8.098297826064319693, 8.342435640030188893, 0.7998128361456481317 ) ) ;
#88230 = CARTESIAN_POINT ( 'NONE',  ( -0.6823417656250212460, 4.051041667008085767, 1.181850606188767472 ) ) ;
#88231 = CARTESIAN_POINT ( 'NONE',  ( 1.604289258337993296, 1.966964933800469106, 0.1018061066037061896 ) ) ;
#88232 = CARTESIAN_POINT ( 'NONE',  ( 1.353610510645312237, -1.387278792934818705, -1.316581319992945920 ) ) ;
#88233 = CARTESIAN_POINT ( 'NONE',  ( 5.138769532551322072, -1.968056315684912683, 1.175056510511104158 ) ) ;
#88234 = CARTESIAN_POINT ( 'NONE',  ( 1.787459277025660542, 1.258035843444211155, 1.323286951131589895 ) ) ;
#88235 = CARTESIAN_POINT ( 'NONE',  ( 4.193214648376505593, 8.114110533073061404, 0.000000000000000000 ) ) ;
#88237 = EDGE_CURVE ( 'NONE', #183165, #123242, #3622, .T. ) ;
#88236 = CARTESIAN_POINT ( 'NONE',  ( 6.141480396866128899, 6.267408005873028820, -0.7216878364870257245 ) ) ;
#88238 = CARTESIAN_POINT ( 'NONE',  ( -7.694415870955439551, 8.935572256658169010, 1.199719254218462483 ) ) ;
#88239 = CARTESIAN_POINT ( 'NONE',  ( 3.006110871101048687, -0.8120814715368419590, 1.842311383860009588 ) ) ;
#88240 = CARTESIAN_POINT ( 'NONE',  ( 3.116010788575247936, 1.952738871351952232, -0.1875660449981580158 ) ) ;
#88241 = CARTESIAN_POINT ( 'NONE',  ( -8.193204901359996128, 8.453160561208463264, 1.040834085586084257E-14 ) ) ;
#88242 = CARTESIAN_POINT ( 'NONE',  ( -5.063080299699540987, 7.994345218703034384, 1.199719254218464037 ) ) ;
#88243 = CARTESIAN_POINT ( 'NONE',  ( 0.07516593201269992919, 2.015085533825950126, -2.458757630349134082 ) ) ;
#88245 = CARTESIAN_POINT ( 'NONE',  ( 4.346413238989558003, 0.4729554063761501892, 1.705410949051559877 ) ) ;
#88244 = CARTESIAN_POINT ( 'NONE',  ( 5.753879374300719718, 0.8463200818398952663, 1.911864941374420201 ) ) ;
#88246 = CARTESIAN_POINT ( 'NONE',  ( -0.3282377607281458110, 2.198664549684619551, -1.225000000000048717 ) ) ;
#88247 = CARTESIAN_POINT ( 'NONE',  ( 0.3049557181189038180, 1.908793570626087455, 1.076422248949958638 ) ) ;
#88248 = CARTESIAN_POINT ( 'NONE',  ( 6.439394946090388316, 0.6587646163928980725, -1.611052209844960670 ) ) ;
#88249 = CARTESIAN_POINT ( 'NONE',  ( 7.962716289927667113, 8.184257181204083409, -0.7998128361456291469 ) ) ;
#88250 = CARTESIAN_POINT ( 'NONE',  ( 0.1333692844072559003, 5.722267537706915874, -2.647605121726896105 ) ) ;
#88251 = CARTESIAN_POINT ( 'NONE',  ( 6.592461167385279097, -0.5184713896582182624, 2.248443398875634269 ) ) ;
#88253 = ADVANCED_FACE ( 'NONE', ( #191805 ), #124783, .T. ) ;
#88252 = DIRECTION ( 'NONE',  ( -0.7592566023653003482, 0.6507913734559641616, 0.000000000000000000 ) ) ;
#88254 = CARTESIAN_POINT ( 'NONE',  ( 6.450542193449531503, 1.198949306261879455, 1.252755643323471668 ) ) ;
#88255 = CARTESIAN_POINT ( 'NONE',  ( 1.506762622594171930, -0.7967928049063888185, -2.058199171410409978 ) ) ;
#88256 = CARTESIAN_POINT ( 'NONE',  ( 0.7081837076810155729, 0.6824709381345904768, -2.061040276042750641 ) ) ;
#88257 = CARTESIAN_POINT ( 'NONE',  ( -0.7500000000000215383, 3.941666666666690411, 1.299038105676671107 ) ) ;
#88258 = CARTESIAN_POINT ( 'NONE',  ( 0.8665975061730617490, -2.067159395656243515, -0.4576585243742418152 ) ) ;
#88260 = VECTOR ( 'NONE', #189130, 1000.000000000000000 ) ;
#88259 = CARTESIAN_POINT ( 'NONE',  ( 2.562500000000001332, -1.451031289061222251, -1.451031289061014196 ) ) ;
#88261 = CARTESIAN_POINT ( 'NONE',  ( -0.5475226324602718853, 7.495867147881379644, -1.923617955668145862 ) ) ;
#88262 = CARTESIAN_POINT ( 'NONE',  ( 4.770489386553291133, -1.258480429039417592, 1.458564191902473661 ) ) ;
#88263 = VERTEX_POINT ( 'NONE', #190742 ) ;
#88265 = CARTESIAN_POINT ( 'NONE',  ( 0.6823417656249882723, -0.8447916663252494907, 1.181850606188755259 ) ) ;
#88264 = CARTESIAN_POINT ( 'NONE',  ( 1.751946580633024331, 2.285858364093972028, -0.1737669427509143383 ) ) ;
#88266 = CARTESIAN_POINT ( 'NONE',  ( 5.281064527722868718, 6.119995689553514140, 1.199719254218462483 ) ) ;
#88267 = CARTESIAN_POINT ( 'NONE',  ( 5.789495288235341874, 6.713164910151406595, 1.199719254218462483 ) ) ;
#88268 = CARTESIAN_POINT ( 'NONE',  ( 4.125785508553894587, -0.3794599818576475658, 2.188496638732019495 ) ) ;
#88269 = CARTESIAN_POINT ( 'NONE',  ( -7.944714827928056167, 10.29191993738131927, 1.443375672974090751 ) ) ;
#88270 = CARTESIAN_POINT ( 'NONE',  ( -6.385527162356468445, 10.39360608948380538, 1.040834085586084257E-14 ) ) ;
#88271 = CARTESIAN_POINT ( 'NONE',  ( 5.612712406377503349, 8.531619659873665995, -1.082531754730543083 ) ) ;
#88272 = CARTESIAN_POINT ( 'NONE',  ( -8.961576348508655698, 9.557519949455999253, -0.7216878364870267237 ) ) ;
#88273 = CARTESIAN_POINT ( 'NONE',  ( 6.224601922449876312, 6.434659462379210382, 0.000000000000000000 ) ) ;
#88274 =( GEOMETRIC_REPRESENTATION_CONTEXT ( 3 ) GLOBAL_UNCERTAINTY_ASSIGNED_CONTEXT ( ( #205743 ) ) GLOBAL_UNIT_ASSIGNED_CONTEXT ( ( #183504, #146783, #82806 ) ) REPRESENTATION_CONTEXT ( 'NONE', 'WORKASPACE' ) );
#88275 = ORIENTED_EDGE ( 'NONE', *, *, #178413, .F. ) ;
#88276 = CARTESIAN_POINT ( 'NONE',  ( 1.318982659667154334, 0.9913977828604101372, -1.755770081111128977 ) ) ;
#88278 = CARTESIAN_POINT ( 'NONE',  ( 6.584441931359013900, 1.190761153509769521, -1.684076666428784064 ) ) ;
#88277 = CARTESIAN_POINT ( 'NONE',  ( 8.437251666405968464, 8.737881787095446384, 1.040834085586084257E-14 ) ) ;
#88279 =( NAMED_UNIT ( * ) PLANE_ANGLE_UNIT ( ) SI_UNIT ( $, .RADIAN. ) );
#88280 = CARTESIAN_POINT ( 'NONE',  ( 6.224601922005513543, 7.395028676162137771, -1.082531754730548412 ) ) ;
#88281 = CARTESIAN_POINT ( 'NONE',  ( 6.444851825500396814, -1.403812859381381895, -1.028626497576446086 ) ) ;
#88283 = ADVANCED_FACE ( 'NONE', ( #143124 ), #19301, .T. ) ;
#88282 = CARTESIAN_POINT ( 'NONE',  ( -11.01135777277261951, 13.50500854530268668, -1.400000000000001465 ) ) ;
#88284 = CARTESIAN_POINT ( 'NONE',  ( -0.6823417656250003738, 2.467708333674753618, -1.181850606188749264 ) ) ;
#88285 = CARTESIAN_POINT ( 'NONE',  ( 1.440303513825416992, 0.3384911870211620988, 1.736878781881325384 ) ) ;
#88286 = CARTESIAN_POINT ( 'NONE',  ( 6.609999999999995879, 0.01081285896096205283, 1.720159828161060833 ) ) ;
#88287 = CARTESIAN_POINT ( 'NONE',  ( 6.286628787680052177, 1.509496725765889114, -0.8662470760552234417 ) ) ;
#88288 = CARTESIAN_POINT ( 'NONE',  ( 4.195090427499806651, 1.841111018879896477, 1.365591311898015192 ) ) ;
#88289 = CARTESIAN_POINT ( 'NONE',  ( 3.345483972246702020, 1.841320589717788447, -0.001054884335952021917 ) ) ;
#88290 =( GEOMETRIC_REPRESENTATION_CONTEXT ( 3 ) GLOBAL_UNCERTAINTY_ASSIGNED_CONTEXT ( ( #187420 ) ) GLOBAL_UNIT_ASSIGNED_CONTEXT ( ( #37613, #200092, #169743 ) ) REPRESENTATION_CONTEXT ( 'NONE', 'WORKASPACE' ) );
#88291 = ADVANCED_FACE ( 'NONE', ( #209117 ), #60754, .T. ) ;
#88292 = CARTESIAN_POINT ( 'NONE',  ( 8.666686507633574621, 11.13422023037111330, 1.599625672291281386 ) ) ;
#88293 =( LENGTH_UNIT ( ) NAMED_UNIT ( * ) SI_UNIT ( .MILLI., .METRE. ) );
#88294 = CARTESIAN_POINT ( 'NONE',  ( 4.366094929315432083, 0.8608494910617261464, 1.609850404305966265 ) ) ;
#88295 = CARTESIAN_POINT ( 'NONE',  ( 5.027970288326706338, -1.728003250605243180, 1.038991650911202713 ) ) ;
#88296 = CARTESIAN_POINT ( 'NONE',  ( -8.533967624797991647, 12.04371376465130439, -1.199719254218446718 ) ) ;
#88298 = CARTESIAN_POINT ( 'NONE',  ( -8.106849506328558164, 8.422688943663599659, 0.000000000000000000 ) ) ;
#88297 = CARTESIAN_POINT ( 'NONE',  ( 3.186655532321683637, -2.228779239134215384, -0.3884498486929898742 ) ) ;
#88299 = CARTESIAN_POINT ( 'NONE',  ( 6.792010069470917344, -0.9048057162561828903, 1.900113248071538585 ) ) ;
#88300 = CARTESIAN_POINT ( 'NONE',  ( 9.598595877357185557, 13.73909624707286703, 8.266025096903813818 ) ) ;
#88301 = CARTESIAN_POINT ( 'NONE',  ( 3.807136610393092813, -1.694265131726957252, 1.189645435975445809 ) ) ;
#88302 = CARTESIAN_POINT ( 'NONE',  ( 3.728655938958122196, 4.308852335994623139, -1.199719254218446718 ) ) ;
#88303 = CARTESIAN_POINT ( 'NONE',  ( -1.360316468750028651, 1.692708333674761922, 0.7853790794158620470 ) ) ;
#88304 = CARTESIAN_POINT ( 'NONE',  ( 6.235037545507011281, 1.978399733989940401, 0.7636319146847592165 ) ) ;
#88306 = CARTESIAN_POINT ( 'NONE',  ( 2.033698780422585006, -1.258094322230184581, -1.459052628860134648 ) ) ;
#88305 = CARTESIAN_POINT ( 'NONE',  ( -9.938290294017125603, 11.55342575023019691, -1.199719254218441611 ) ) ;
#88307 = CARTESIAN_POINT ( 'NONE',  ( 9.584291988782252858, -7.189630408304556575, -0.001123102408822191766 ) ) ;
#88308 = CARTESIAN_POINT ( 'NONE',  ( 0.3089591345776849241, -1.584006439100977603, 1.170298647042963935 ) ) ;
#88309 = CARTESIAN_POINT ( 'NONE',  ( 3.716343503477301802, 7.349834830783237294, -1.734723475976807094E-15 ) ) ;
#88310 = CARTESIAN_POINT ( 'NONE',  ( 5.861148881710747993, 5.995921596292371092, 0.2991943293650864422 ) ) ;
#88311 = CARTESIAN_POINT ( 'NONE',  ( 0.000000000000000000, -8.233137084989849086, 0.000000000000000000 ) ) ;
#88312 = CARTESIAN_POINT ( 'NONE',  ( -4.711622075948912247, 5.455646162483875017, -1.199719254218446718 ) ) ;
#88313 = CARTESIAN_POINT ( 'NONE',  ( 0.03578803411239706023, -0.1004787818888741302, 2.219253419324648036 ) ) ;
#88314 = CARTESIAN_POINT ( 'NONE',  ( 1.852698501422584298, 0.6601115537133980249, 1.999908888789264649 ) ) ;
#88315 = CARTESIAN_POINT ( 'NONE',  ( -4.492547798081878874, 6.334668079219206049, 1.599625672291263179 ) ) ;
#88316 = CARTESIAN_POINT ( 'NONE',  ( 8.111855979677986994, 8.358253485912799263, 1.040834085586084257E-14 ) ) ;
#88317 = CARTESIAN_POINT ( 'NONE',  ( 0.3966288646398182238, 0.3121968076400126746, 1.834509442227350462 ) ) ;
#88318 = CARTESIAN_POINT ( 'NONE',  ( 6.693975156845185737, 8.832723654451292816, 1.599625672291281386 ) ) ;
#88319 = CARTESIAN_POINT ( 'NONE',  ( 0.07700591528353981086, 0.003617085621422309362, -1.910863332519038726 ) ) ;
#88320 = CARTESIAN_POINT ( 'NONE',  ( -6.455090533882193782, 9.584670485287619002, -1.082531754730549967 ) ) ;
#88321 = CARTESIAN_POINT ( 'NONE',  ( -8.134528978519403708, 11.47373899403920205, 1.082531754730549967 ) ) ;
#88322 = CARTESIAN_POINT ( 'NONE',  ( 0.7035762090183244055, 1.867434778015097940, -1.004864118554361863 ) ) ;
#88323 = CARTESIAN_POINT ( 'NONE',  ( -5.738844160334429567, 9.917344963690652548, 0.000000000000000000 ) ) ;
#88325 = CARTESIAN_POINT ( 'NONE',  ( 2.875390130891414042, -0.1950805366632331617, 1.952157403750237163 ) ) ;
#88324 = CARTESIAN_POINT ( 'NONE',  ( -2.353626204688216217E-14, 0.9375000000000365263, -1.414508159514579644 ) ) ;
#88326 = CARTESIAN_POINT ( 'NONE',  ( 2.114359756454447847, -1.018641858927371135, -1.906637348776268004 ) ) ;
#88327 = CARTESIAN_POINT ( 'NONE',  ( 2.102840161960460197, -0.4018910908503615653, 1.796694178532439956 ) ) ;
#88329 = CARTESIAN_POINT ( 'NONE',  ( -5.430810130430261395, 6.303639405459422917, -1.045180951442852946 ) ) ;
#88328 = CARTESIAN_POINT ( 'NONE',  ( -3.962726036944197894, 7.845207153068690431, -0.7998128361456481317 ) ) ;
#88330 = CARTESIAN_POINT ( 'NONE',  ( 3.239928156850964580, 0.4239778953066320466, 1.687749859276384878 ) ) ;
#88331 = CARTESIAN_POINT ( 'NONE',  ( 5.856759171423504107, 5.935233242856626568, -0.7216878364870257245 ) ) ;
#88332 = CARTESIAN_POINT ( 'NONE',  ( -10.78552488895401318, 8.017604977416297629, -4.042330561003328881 ) ) ;
#88333 = CARTESIAN_POINT ( 'NONE',  ( 1.042116488573753497, 0.8753402851892390091, -1.976733581976031218 ) ) ;
#88334 = CARTESIAN_POINT ( 'NONE',  ( 2.917342117414220670, 0.6766092434087739305, 1.899328150365031664 ) ) ;
#88335 = CARTESIAN_POINT ( 'NONE',  ( -0.1007326007326104361, -9.919999999999998153, -10.99953876047306167 ) ) ;
#88336 = B_SPLINE_CURVE_WITH_KNOTS ( 'NONE', 3,
 ( #197092, #80148, #146251, #212267 ),
 .UNSPECIFIED., .F., .F.,
 ( 4, 4 ),
 ( 1.951563910473910678E-18, 0.0006335992342243210260 ),
 .UNSPECIFIED. ) ;
#88337 = CARTESIAN_POINT ( 'NONE',  ( 0.07536363704235826688, -0.001874865094115066300, -2.144269471569634877 ) ) ;
#88338 = CARTESIAN_POINT ( 'NONE',  ( 1.762511527598693784, -1.395553132451602174, 1.392767733363926119 ) ) ;
#88339 = B_SPLINE_CURVE_WITH_KNOTS ( 'NONE', 3,
 ( #168807, #71282, #137395, #152558, #4145, #199148, #70216, #203414, #187187, #175239 ),
 .UNSPECIFIED., .F., .F.,
 ( 4, 3, 3, 4 ),
 ( 2.070599078951341269E-17, 6.251588761609448285E-05, 0.0001877407159084782664, 0.0003399624922859439112 ),
 .UNSPECIFIED. ) ;
#88340 = CARTESIAN_POINT ( 'NONE',  ( 0.5445930744353514319, 3.250057683544645304, -0.4000000000000409339 ) ) ;
#88341 = CARTESIAN_POINT ( 'NONE',  ( 2.190873381757904692, 1.502741926987064325, 1.230217333823523163 ) ) ;
#88343 = EDGE_LOOP ( 'NONE', ( #96611, #212600, #106632, #111696, #202836, #72194, #132243, #174640 ) ) ;
#88342 = CARTESIAN_POINT ( 'NONE',  ( -3.838366886444665393, 7.492195444245147939, 0.000000000000000000 ) ) ;
#88344 = CARTESIAN_POINT ( 'NONE',  ( -4.136646265500964148, 6.879818838842817641, -1.082531754730551743 ) ) ;
#88345 = CARTESIAN_POINT ( 'NONE',  ( -0.2106854629474881058, 5.722459385925042774, -2.591190942950042597 ) ) ;
#88346 = CARTESIAN_POINT ( 'NONE',  ( 4.376249722160992839, 8.327651452488305850, 0.000000000000000000 ) ) ;
#88347 = CARTESIAN_POINT ( 'NONE',  ( -5.631432701629818460, 7.663367133358481631, 1.599625672291263179 ) ) ;
#88348 = CARTESIAN_POINT ( 'NONE',  ( -5.610041701004606196, 9.767075427805856691, -0.7998128361456362523 ) ) ;
#88349 = CARTESIAN_POINT ( 'NONE',  ( 1.854049621773927514, 5.499999999999998224, 0.7500000000000006661 ) ) ;
#88350 = CARTESIAN_POINT ( 'NONE',  ( 6.440458288041322810, 2.281167638128688946, 0.3475669597150666257 ) ) ;
#88351 = FACE_BOUND ( 'NONE', #195313, .T. ) ;
#88352 = CARTESIAN_POINT ( 'NONE',  ( 4.662917994108885189, 1.519075486231920458, -1.241376779329693258 ) ) ;
#88353 = CARTESIAN_POINT ( 'NONE',  ( 7.096803341749390981, 10.36702210109460154, -1.199719254218441611 ) ) ;
#88354 = CARTESIAN_POINT ( 'NONE',  ( 1.459611520199757706, -1.915600648959712382, -0.6298732728240025169 ) ) ;
#88355 = ORIENTED_EDGE ( 'NONE', *, *, #63060, .T. ) ;
#88356 = CARTESIAN_POINT ( 'NONE',  ( 2.589187231636483233, 1.791351791295469731, 1.128514814827277002 ) ) ;
#88357 = CARTESIAN_POINT ( 'NONE',  ( -1.201851678989727383E-14, 1.243750000682821044, 1.732050807568877637 ) ) ;
#88359 = CARTESIAN_POINT ( 'NONE',  ( -6.368579470117215813, 8.453095353268645695, 1.599625672291283607 ) ) ;
#88358 = DIRECTION ( 'NONE',  ( 0.000000000000000000, -1.000000000000000000, 0.000000000000000000 ) ) ;
#88360 = CARTESIAN_POINT ( 'NONE',  ( 2.765369989423609454, 0.9851603262180377296, 1.555203531693909680 ) ) ;
#88361 = ORIENTED_EDGE ( 'NONE', *, *, #141283, .T. ) ;
#88362 = CARTESIAN_POINT ( 'NONE',  ( -8.299562589859897699, 12.83457345481192036, -0.7998128361456281477 ) ) ;
#88363 = CARTESIAN_POINT ( 'NONE',  ( -1.408440994509118749, 7.230285460703087530, 4.273713947604063534 ) ) ;
#88364 = CARTESIAN_POINT ( 'NONE',  ( 4.306960158517386894, -0.4675538901007176285, -2.068242682749166672 ) ) ;
#88365 = CARTESIAN_POINT ( 'NONE',  ( 0.1109373197970727615, -1.806229982939497658, 0.3559056038356380736 ) ) ;
#88366 = CARTESIAN_POINT ( 'NONE',  ( 1.499999999999990896, 5.556250000682820378, 1.214306433183764966E-14 ) ) ;
#88367 = CARTESIAN_POINT ( 'NONE',  ( 5.940443861082012944, 10.08226827123770697, 0.7998128361456462443 ) ) ;
#88368 = CARTESIAN_POINT ( 'NONE',  ( 4.411438286107774331, -0.3560947707623678959, 2.029623144953551339 ) ) ;
#88370 = CARTESIAN_POINT ( 'NONE',  ( 1.223879446662301307, 1.774596971308094018, 0.4907264878865265634 ) ) ;
#88369 = CARTESIAN_POINT ( 'NONE',  ( -5.703176172842872482, 9.805455968292021041, 0.000000000000000000 ) ) ;
#88371 = CARTESIAN_POINT ( 'NONE',  ( -1.364683531249997417, 5.509375000341417916, 1.214306433183764966E-14 ) ) ;
#88372 =( NAMED_UNIT ( * ) PLANE_ANGLE_UNIT ( ) SI_UNIT ( $, .RADIAN. ) );
#88373 = CARTESIAN_POINT ( 'NONE',  ( 10.95700306400770785, -7.901429653175738643, -0.3289054322349463377 ) ) ;
#88374 = CARTESIAN_POINT ( 'NONE',  ( 0.9970219447392356660, -0.5395372827587068265, -2.139793933917451874 ) ) ;
#88375 = CARTESIAN_POINT ( 'NONE',  ( 3.444836229973327946, 0.5457880569446837971, 2.195490905318697283 ) ) ;
#88376 = CARTESIAN_POINT ( 'NONE',  ( -7.212574532790092974, 10.39812547402169862, -1.082531754730543971 ) ) ;
#88377 = CARTESIAN_POINT ( 'NONE',  ( 3.181707836761258790, 1.766318828868058910, -0.4016052188219875752 ) ) ;
#88378 = CARTESIAN_POINT ( 'NONE',  ( 4.381993024020896854, -1.915445973796879864, -0.04088167158281148100 ) ) ;
#88379 = CARTESIAN_POINT ( 'NONE',  ( 5.547352688424546763, 1.827615396715172258, -0.9727077141251788683 ) ) ;
#88380 = CARTESIAN_POINT ( 'NONE',  ( -1.201851678989727383E-14, 4.009375000341416140, -1.575800808251660134 ) ) ;
#88381 = CARTESIAN_POINT ( 'NONE',  ( 3.643400374902918681, -1.492087795311855425, -1.288628176122036839 ) ) ;
#88382 = CARTESIAN_POINT ( 'NONE',  ( 1.342661396784496697, 0.3730742192328758144, 1.889760217127177455 ) ) ;
#88383 = CARTESIAN_POINT ( 'NONE',  ( 3.414787578387419309, 1.690673485743508619, 0.8009127983473337542 ) ) ;
#88384 = CARTESIAN_POINT ( 'NONE',  ( 3.756711156304150201, 0.8293906405268698379, 2.153668854807685662 ) ) ;
#88385 = CARTESIAN_POINT ( 'NONE',  ( 4.053051418270800177, 1.573051355563404252, -0.9941624863331417483 ) ) ;
#88386 = CARTESIAN_POINT ( 'NONE',  ( -0.6823417656250212460, 4.801041667008086655, 1.181850606188767472 ) ) ;
#88387 = AXIS2_PLACEMENT_3D ( 'NONE', #131157, #61831, #197148 ) ;
#88388 = CARTESIAN_POINT ( 'NONE',  ( 11.89942855770813956, 9.719999999999998863, 0.6999999999999992895 ) ) ;
#88389 =( BOUNDED_SURFACE ( )  B_SPLINE_SURFACE ( 1, 2, ( 
 ( #169680, #55940, #206443, #205370, #190192, #122093, #121026, #23414, #38624, #171821, #170751, #41851, #22337, #203228, #57005, #9320, #156652, #123177, #155579, #71088, #189136, #107961, #173989, #89526, #40775, #54873, #185914, #141506, #137206, #154510, #186993, #37548, #106880, #21268, #188057, #58070, #172907, #25561, #39686, #104700, #7163, #88451, #73233, #6092, #91672, #72160, #138269, #204283, #157725, #103628, #139340, #24481, #90593, #74329, #8245, #124233, #87373, #75394, #207515, #59133, #153443, #5015, #77518, #110095, #93801, #211772, #193405, #142557, #208564, #60198, #78581, #63410, #159841, #95935, #29855, #12510, #210714, #178238, #176106, #45049, #62342, #61273, #129561, #161991, #13581, #209633, #194470, #47185, #145771, #127435, #79654, #11442, #195548, #113299, #179306, #192318, #175045, #80730, #43976, #126359, #30927, #111161, #10373, #97003, #128502, #163056, #94861, #46112, #27706, #14636, #146820, #143639, #177161, #212840, #125293, #191251, #112230, #42916, #109026, #28779, #160916, #158777, #144703, #26630, #92732, #76450, #35146, #196610, #64477, #98062, #83904, #101223, #132703, #65508, #50354, #147870, #131654, #198709, #167306, #184598, #166230, #493, #19963, #52481, #15701, #130617, #165165, #116476, #182466, #118609, #18893, #66561, #82843, #48249, #16760, #114364, #149994, #148920, #133772, #81787, #84977, #213885, #151069, #180358, #34095, #2631, #68704, #134826, #100166, #99116, #197657, #49303, #200830, #181411, #17821, #183540, #199780, #1565, #36215, #102294, #67627, #168368, #86047, #152123, #31984, #164118, #51426, #115419, #117546, #33038, #72981, #6904, #204029, #5834, #22075, #41594, #135876, #187804, #169430, #140164, #103368, #69770, #185666, #171559, #172650, #170491, #136949, #201895, #188877, #139084, #107705, #206187, #7982, #21014, #23156, #56754, #53548, #39432, #120763, #205111, #119679, #87112, #88187, #57815, #71905, #123977, #153182, #4756, #90327, #25308, #189944, #173731, #70831, #105525, #202974, #156396, #154259, #91410, #54615, #74071, #3693 ),
 ( #106620, #37295, #89271, #138014, #155320, #186741, #40518, #122919, #24225, #38363, #104442, #55677, #121833, #77264, #160657, #174797, #157470, #113045, #42663, #126103, #26373, #59947, #12254, #143377, #45861, #210456, #142306, #141249, #192063, #158525, #78331, #145520, #159586, #109841, #208317, #43726, #29598, #11184, #92486, #10122, #76197, #110902, #95684, #175855, #128253, #62094, #44797, #28523, #194216, #27444, #209376, #94613, #93542, #161738, #111982, #177983, #61020, #144453, #79403, #13329, #127179, #211519, #193147, #63155, #129320, #195296, #176908, #207258, #179051, #46927, #30670, #9065, #75140, #108772, #58886, #125042, #190997, #66319, #33844, #213636, #51174, #117297, #65263, #147618, #183294, #52238, #34899, #165986, #100972, #2384, #114119, #49050, #130370, #81536, #181165, #212589, #184354, #67384, #14380, #96753, #196361, #116230, #133524, #164917, #97808, #82592, #180111, #163871, #16510, #199531, #68462, #198465, #32789, #182221, #134590, #167061, #99925, #132463, #48001, #17572, #18653, #84732, #148679, #83656, #31735, #162803, #118365, #15447, #131409, #197409, #80472, #149746, #146571, #98865, #150821, #1323, #200590, #247, #115170, #50109, #64228, #24778, #20773, #43200, #86869, #53302, #103123, #175325, #168122, #35976, #208847, #135632, #4512, #119434, #102056, #190473, #19723, #123460, #207791, #58361, #109314, #189423, #185421, #90879, #169181, #156941, #152935, #26908, #70584, #37039, #139636, #93014, #85802, #205659, #42133, #173198, #141785, #91950, #57295, #151882, #41064, #107171, #174268, #159057, #8532, #74611, #140717, #206731, #125575, #124514, #108245, #25843, #158012, #9599, #191536, #75676, #59419, #10653, #76726, #142842, #60478, #126636, #3456, #69525, #201652, #130885, #97272, #31196, #62605, #47459, #114637, #213111, #128767, #81000, #12779, #64743, #147088, #196879, #45320, #27987, #148149, #111439, #61551, #48516, #194743, #77798, #180629, #195819, #163326, #162260, #129838, #95141, #32252, #98322, #161191, #29058, #164387, #214150, #15971, #113574, #82057 ) ),
 .UNSPECIFIED., .F., .F., .T. ) 
 B_SPLINE_SURFACE_WITH_KNOTS ( ( 2, 2 ),
 ( 3, 2, 2, 2, 2, 2, 2, 2, 2, 2, 2, 2, 2, 2, 2, 2, 2, 2, 2, 2, 2, 2, 2, 2, 2, 2, 2, 2, 2, 2, 2, 2, 2, 2, 2, 2, 2, 2, 2, 2, 2, 2, 2, 2, 2, 2, 2, 2, 2, 2, 2, 2, 2, 2, 2, 2, 2, 2, 2, 2, 2, 2, 2, 2, 2, 2, 2, 2, 2, 2, 2, 2, 2, 2, 2, 2, 2, 2, 2, 2, 2, 2, 2, 2, 2, 2, 2, 2, 2, 2, 2, 2, 2, 2, 2, 2, 2, 2, 2, 2, 2, 2, 2, 2, 2, 2, 2, 2, 2, 2, 2, 2, 2, 2, 2, 2, 2, 2, 2, 2, 3 ),
 ( 0.000000000000000000, 1.000000000000000000 ),
 ( 0.000000000000000000, 0.008333333333333333218, 0.01666666666666666644, 0.02500000000000000139, 0.03333333333333333287, 0.04166666666666666435, 0.05000000000000000278, 0.05833333333333333426, 0.06666666666666666574, 0.07499999999999999722, 0.08333333333333332871, 0.09166666666666666019, 0.1000000000000000056, 0.1083333333333333370, 0.1166666666666666685, 0.1250000000000000000, 0.1333333333333333315, 0.1416666666666666630, 0.1499999999999999944, 0.1583333333333333259, 0.1666666666666666574, 0.1749999999999999889, 0.1833333333333333204, 0.1916666666666666796, 0.2000000000000000111, 0.2083333333333333426, 0.2166666666666666741, 0.2250000000000000056, 0.2333333333333333370, 0.2416666666666666685, 0.2500000000000000000, 0.2583333333333333592, 0.2666666666666666630, 0.2750000000000000222, 0.2833333333333333259, 0.2916666666666666852, 0.2999999999999999889, 0.3083333333333333481, 0.3166666666666666519, 0.3250000000000000111, 0.3333333333333333148, 0.3416666666666666741, 0.3499999999999999778, 0.3583333333333333370, 0.3666666666666666408, 0.3750000000000000000, 0.3833333333333333592, 0.3916666666666666630, 0.4000000000000000222, 0.4083333333333333259, 0.4166666666666666852, 0.4249999999999999889, 0.4333333333333333481, 0.4416666666666666519, 0.4500000000000000111, 0.4583333333333333148, 0.4666666666666666741, 0.4749999999999999778, 0.4833333333333333370, 0.4916666666666666408, 0.5000000000000000000, 0.5083333333333333037, 0.5166666666666667185, 0.5250000000000000222, 0.5333333333333333259, 0.5416666666666666297, 0.5500000000000000444, 0.5583333333333333481, 0.5666666666666666519, 0.5749999999999999556, 0.5833333333333333703, 0.5916666666666666741, 0.5999999999999999778, 0.6083333333333332815, 0.6166666666666666963, 0.6250000000000000000, 0.6333333333333333037, 0.6416666666666667185, 0.6500000000000000222, 0.6583333333333333259, 0.6666666666666666297, 0.6750000000000000444, 0.6833333333333333481, 0.6916666666666666519, 0.6999999999999999556, 0.7083333333333333703, 0.7166666666666666741, 0.7249999999999999778, 0.7333333333333332815, 0.7416666666666666963, 0.7500000000000000000, 0.7583333333333333037, 0.7666666666666667185, 0.7750000000000000222, 0.7833333333333333259, 0.7916666666666666297, 0.8000000000000000444, 0.8083333333333333481, 0.8166666666666666519, 0.8249999999999999556, 0.8333333333333333703, 0.8416666666666666741, 0.8499999999999999778, 0.8583333333333332815, 0.8666666666666666963, 0.8750000000000000000, 0.8833333333333333037, 0.8916666666666667185, 0.9000000000000000222, 0.9083333333333333259, 0.9166666666666666297, 0.9250000000000000444, 0.9333333333333333481, 0.9416666666666666519, 0.9499999999999999556, 0.9583333333333333703, 0.9666666666666666741, 0.9749999999999999778, 0.9833333333333332815, 0.9916666666666666963, 1.000000000000000000 ),
 .UNSPECIFIED. ) 
 GEOMETRIC_REPRESENTATION_ITEM ( )  RATIONAL_B_SPLINE_SURFACE ( (
 ( 1.000000000000000000, 0.8660254037844387076, 1.000000000000000000, 0.8660254037844387076, 1.000000000000000000, 0.8660254037844387076, 1.000000000000000000, 0.8660254037844387076, 1.000000000000000000, 0.8660254037844387076, 1.000000000000000000, 0.8660254037844387076, 1.000000000000000000, 0.8660254037844387076, 1.000000000000000000, 0.8660254037844387076, 1.000000000000000000, 0.8660254037844387076, 1.000000000000000000, 0.8660254037844387076, 1.000000000000000000, 0.8660254037844387076, 1.000000000000000000, 0.8660254037844387076, 1.000000000000000000, 0.8660254037844387076, 1.000000000000000000, 0.8660254037844387076, 1.000000000000000000, 0.8660254037844387076, 1.000000000000000000, 0.8660254037844387076, 1.000000000000000000, 0.8660254037844387076, 1.000000000000000000, 0.8660254037844387076, 1.000000000000000000, 0.8660254037844387076, 1.000000000000000000, 0.8660254037844387076, 1.000000000000000000, 0.8660254037844387076, 1.000000000000000000, 0.8660254037844387076, 1.000000000000000000, 0.8660254037844387076, 1.000000000000000000, 0.8660254037844387076, 1.000000000000000000, 0.8660254037844387076, 1.000000000000000000, 0.8660254037844387076, 1.000000000000000000, 0.8660254037844387076, 1.000000000000000000, 0.8660254037844387076, 1.000000000000000000, 0.8660254037844387076, 1.000000000000000000, 0.8660254037844387076, 1.000000000000000000, 0.8660254037844387076, 1.000000000000000000, 0.8660254037844387076, 1.000000000000000000, 0.8660254037844387076, 1.000000000000000000, 0.8660254037844387076, 1.000000000000000000, 0.8660254037844387076, 1.000000000000000000, 0.8660254037844387076, 1.000000000000000000, 0.8660254037844387076, 1.000000000000000000, 0.8660254037844387076, 1.000000000000000000, 0.8660254037844387076, 1.000000000000000000, 0.8660254037844387076, 1.000000000000000000, 0.8660254037844387076, 1.000000000000000000, 0.8660254037844387076, 1.000000000000000000, 0.8660254037844387076, 1.000000000000000000, 0.8660254037844387076, 1.000000000000000000, 0.8660254037844387076, 1.000000000000000000, 0.8660254037844387076, 1.000000000000000000, 0.8660254037844387076, 1.000000000000000000, 0.8660254037844387076, 1.000000000000000000, 0.8660254037844387076, 1.000000000000000000, 0.8660254037844387076, 1.000000000000000000, 0.8660254037844387076, 1.000000000000000000, 0.8660254037844387076, 1.000000000000000000, 0.8660254037844387076, 1.000000000000000000, 0.8660254037844387076, 1.000000000000000000, 0.8660254037844387076, 1.000000000000000000, 0.8660254037844387076, 1.000000000000000000, 0.8660254037844387076, 1.000000000000000000, 0.8660254037844387076, 1.000000000000000000, 0.8660254037844387076, 1.000000000000000000, 0.8660254037844387076, 1.000000000000000000, 0.8660254037844387076, 1.000000000000000000, 0.8660254037844387076, 1.000000000000000000, 0.8660254037844387076, 1.000000000000000000, 0.8660254037844387076, 1.000000000000000000, 0.8660254037844387076, 1.000000000000000000, 0.8660254037844387076, 1.000000000000000000, 0.8660254037844387076, 1.000000000000000000, 0.8660254037844387076, 1.000000000000000000, 0.8660254037844387076, 1.000000000000000000, 0.8660254037844387076, 1.000000000000000000, 0.8660254037844387076, 1.000000000000000000, 0.8660254037844387076, 1.000000000000000000, 0.8660254037844387076, 1.000000000000000000, 0.8660254037844387076, 1.000000000000000000, 0.8660254037844387076, 1.000000000000000000, 0.8660254037844387076, 1.000000000000000000, 0.8660254037844387076, 1.000000000000000000, 0.8660254037844387076, 1.000000000000000000, 0.8660254037844387076, 1.000000000000000000, 0.8660254037844387076, 1.000000000000000000, 0.8660254037844387076, 1.000000000000000000, 0.8660254037844387076, 1.000000000000000000, 0.8660254037844387076, 1.000000000000000000, 0.8660254037844387076, 1.000000000000000000, 0.8660254037844387076, 1.000000000000000000, 0.8660254037844387076, 1.000000000000000000, 0.8660254037844387076, 1.000000000000000000, 0.8660254037844387076, 1.000000000000000000, 0.8660254037844387076, 1.000000000000000000, 0.8660254037844387076, 1.000000000000000000, 0.8660254037844387076, 1.000000000000000000, 0.8660254037844387076, 1.000000000000000000, 0.8660254037844387076, 1.000000000000000000, 0.8660254037844387076, 1.000000000000000000, 0.8660254037844387076, 1.000000000000000000, 0.8660254037844387076, 1.000000000000000000, 0.8660254037844387076, 1.000000000000000000, 0.8660254037844387076, 1.000000000000000000, 0.8660254037844387076, 1.000000000000000000, 0.8660254037844387076, 1.000000000000000000, 0.8660254037844387076, 1.000000000000000000, 0.8660254037844387076, 1.000000000000000000, 0.8660254037844387076, 1.000000000000000000, 0.8660254037844387076, 1.000000000000000000, 0.8660254037844387076, 1.000000000000000000, 0.8660254037844387076, 1.000000000000000000, 0.8660254037844387076, 1.000000000000000000, 0.8660254037844387076, 1.000000000000000000, 0.8660254037844387076, 1.000000000000000000, 0.8660254037844387076, 1.000000000000000000, 0.8660254037844387076, 1.000000000000000000, 0.8660254037844387076, 1.000000000000000000, 0.8660254037844387076, 1.000000000000000000, 0.8660254037844387076, 1.000000000000000000, 0.8660254037844387076, 1.000000000000000000, 0.8660254037844387076, 1.000000000000000000, 0.8660254037844387076, 1.000000000000000000, 0.8660254037844387076, 1.000000000000000000, 0.8660254037844387076, 1.000000000000000000, 0.8660254037844387076, 1.000000000000000000),
 ( 1.000000000000000000, 0.8660254037844387076, 1.000000000000000000, 0.8660254037844387076, 1.000000000000000000, 0.8660254037844387076, 1.000000000000000000, 0.8660254037844387076, 1.000000000000000000, 0.8660254037844387076, 1.000000000000000000, 0.8660254037844387076, 1.000000000000000000, 0.8660254037844387076, 1.000000000000000000, 0.8660254037844387076, 1.000000000000000000, 0.8660254037844387076, 1.000000000000000000, 0.8660254037844387076, 1.000000000000000000, 0.8660254037844387076, 1.000000000000000000, 0.8660254037844387076, 1.000000000000000000, 0.8660254037844387076, 1.000000000000000000, 0.8660254037844387076, 1.000000000000000000, 0.8660254037844387076, 1.000000000000000000, 0.8660254037844387076, 1.000000000000000000, 0.8660254037844387076, 1.000000000000000000, 0.8660254037844387076, 1.000000000000000000, 0.8660254037844387076, 1.000000000000000000, 0.8660254037844387076, 1.000000000000000000, 0.8660254037844387076, 1.000000000000000000, 0.8660254037844387076, 1.000000000000000000, 0.8660254037844387076, 1.000000000000000000, 0.8660254037844387076, 1.000000000000000000, 0.8660254037844387076, 1.000000000000000000, 0.8660254037844387076, 1.000000000000000000, 0.8660254037844387076, 1.000000000000000000, 0.8660254037844387076, 1.000000000000000000, 0.8660254037844387076, 1.000000000000000000, 0.8660254037844387076, 1.000000000000000000, 0.8660254037844387076, 1.000000000000000000, 0.8660254037844387076, 1.000000000000000000, 0.8660254037844387076, 1.000000000000000000, 0.8660254037844387076, 1.000000000000000000, 0.8660254037844387076, 1.000000000000000000, 0.8660254037844387076, 1.000000000000000000, 0.8660254037844387076, 1.000000000000000000, 0.8660254037844387076, 1.000000000000000000, 0.8660254037844387076, 1.000000000000000000, 0.8660254037844387076, 1.000000000000000000, 0.8660254037844387076, 1.000000000000000000, 0.8660254037844387076, 1.000000000000000000, 0.8660254037844387076, 1.000000000000000000, 0.8660254037844387076, 1.000000000000000000, 0.8660254037844387076, 1.000000000000000000, 0.8660254037844387076, 1.000000000000000000, 0.8660254037844387076, 1.000000000000000000, 0.8660254037844387076, 1.000000000000000000, 0.8660254037844387076, 1.000000000000000000, 0.8660254037844387076, 1.000000000000000000, 0.8660254037844387076, 1.000000000000000000, 0.8660254037844387076, 1.000000000000000000, 0.8660254037844387076, 1.000000000000000000, 0.8660254037844387076, 1.000000000000000000, 0.8660254037844387076, 1.000000000000000000, 0.8660254037844387076, 1.000000000000000000, 0.8660254037844387076, 1.000000000000000000, 0.8660254037844387076, 1.000000000000000000, 0.8660254037844387076, 1.000000000000000000, 0.8660254037844387076, 1.000000000000000000, 0.8660254037844387076, 1.000000000000000000, 0.8660254037844387076, 1.000000000000000000, 0.8660254037844387076, 1.000000000000000000, 0.8660254037844387076, 1.000000000000000000, 0.8660254037844387076, 1.000000000000000000, 0.8660254037844387076, 1.000000000000000000, 0.8660254037844387076, 1.000000000000000000, 0.8660254037844387076, 1.000000000000000000, 0.8660254037844387076, 1.000000000000000000, 0.8660254037844387076, 1.000000000000000000, 0.8660254037844387076, 1.000000000000000000, 0.8660254037844387076, 1.000000000000000000, 0.8660254037844387076, 1.000000000000000000, 0.8660254037844387076, 1.000000000000000000, 0.8660254037844387076, 1.000000000000000000, 0.8660254037844387076, 1.000000000000000000, 0.8660254037844387076, 1.000000000000000000, 0.8660254037844387076, 1.000000000000000000, 0.8660254037844387076, 1.000000000000000000, 0.8660254037844387076, 1.000000000000000000, 0.8660254037844387076, 1.000000000000000000, 0.8660254037844387076, 1.000000000000000000, 0.8660254037844387076, 1.000000000000000000, 0.8660254037844387076, 1.000000000000000000, 0.8660254037844387076, 1.000000000000000000, 0.8660254037844387076, 1.000000000000000000, 0.8660254037844387076, 1.000000000000000000, 0.8660254037844387076, 1.000000000000000000, 0.8660254037844387076, 1.000000000000000000, 0.8660254037844387076, 1.000000000000000000, 0.8660254037844387076, 1.000000000000000000, 0.8660254037844387076, 1.000000000000000000, 0.8660254037844387076, 1.000000000000000000, 0.8660254037844387076, 1.000000000000000000, 0.8660254037844387076, 1.000000000000000000, 0.8660254037844387076, 1.000000000000000000, 0.8660254037844387076, 1.000000000000000000, 0.8660254037844387076, 1.000000000000000000, 0.8660254037844387076, 1.000000000000000000, 0.8660254037844387076, 1.000000000000000000, 0.8660254037844387076, 1.000000000000000000, 0.8660254037844387076, 1.000000000000000000, 0.8660254037844387076, 1.000000000000000000, 0.8660254037844387076, 1.000000000000000000, 0.8660254037844387076, 1.000000000000000000, 0.8660254037844387076, 1.000000000000000000, 0.8660254037844387076, 1.000000000000000000, 0.8660254037844387076, 1.000000000000000000, 0.8660254037844387076, 1.000000000000000000, 0.8660254037844387076, 1.000000000000000000, 0.8660254037844387076, 1.000000000000000000, 0.8660254037844387076, 1.000000000000000000, 0.8660254037844387076, 1.000000000000000000, 0.8660254037844387076, 1.000000000000000000, 0.8660254037844387076, 1.000000000000000000, 0.8660254037844387076, 1.000000000000000000, 0.8660254037844387076, 1.000000000000000000, 0.8660254037844387076, 1.000000000000000000, 0.8660254037844387076, 1.000000000000000000, 0.8660254037844387076, 1.000000000000000000) ) ) 
 REPRESENTATION_ITEM ( '' )  SURFACE ( )  );
#88390 = CARTESIAN_POINT ( 'NONE',  ( 1.436301726765435438, 1.036571610867568216, -1.833232669937171266 ) ) ;
#88391 = CIRCLE ( 'NONE', #209417, 2.000000000000000000 ) ;
#88392 = CARTESIAN_POINT ( 'NONE',  ( 2.684151225381301575, 6.075334163012737321, 0.000000000000000000 ) ) ;
#88394 = CARTESIAN_POINT ( 'NONE',  ( 5.052321652499934146, 4.905166280363509657, 0.2868986031296373862 ) ) ;
#88393 = CARTESIAN_POINT ( 'NONE',  ( 0.6823417656249899377, 5.738541667008087543, -1.181850606188754593 ) ) ;
#88395 = CARTESIAN_POINT ( 'NONE',  ( 1.350866880800080105, 4.253815248464132281, 0.3155278943301796923 ) ) ;
#88396 = CARTESIAN_POINT ( 'NONE',  ( 3.058948843759463188, 0.5191580478346514704, 2.055925682384197373 ) ) ;
#88397 = CARTESIAN_POINT ( 'NONE',  ( -4.981227357108504172, 4.889801201946265330, -0.2148083726750001365 ) ) ;
#88398 = CARTESIAN_POINT ( 'NONE',  ( 1.265885189609064376, 0.5823756177252036315, -1.934031124627869414 ) ) ;
#88399 = CARTESIAN_POINT ( 'NONE',  ( 1.364683531249988757, 0.6343750003414208027, 0.000000000000000000 ) ) ;
#88400 = CARTESIAN_POINT ( 'NONE',  ( -3.090895834235680262, 5.589500325708124606, 1.082531754730560403 ) ) ;
#88401 = CARTESIAN_POINT ( 'NONE',  ( 5.823390672269506574, 6.752709524857930745, -1.199719254218446718 ) ) ;
#88402 = ORIENTED_EDGE ( 'NONE', *, *, #47626, .T. ) ;
#88403 = CARTESIAN_POINT ( 'NONE',  ( 0.7554163591718568993, -1.825703804718967316, -1.157005318491082901 ) ) ;
#88404 = DIRECTION ( 'NONE',  ( 0.000000000000000000, -0.8000000000000623279, -0.5999999999999167111 ) ) ;
#88407 = CARTESIAN_POINT ( 'NONE',  ( 6.539320575229233157, 0.001224430076711413356, 2.103502572931112091 ) ) ;
#88406 = CARTESIAN_POINT ( 'NONE',  ( 3.826480369638860602E-16, 4.400000000000001243, -2.150000000000006573 ) ) ;
#88405 = CARTESIAN_POINT ( 'NONE',  ( 6.073126464278658432, 6.050012061272033392, 0.000000000000000000 ) ) ;
#88408 = CARTESIAN_POINT ( 'NONE',  ( 10.68346185744421462, 11.56638637654751989, 0.000000000000000000 ) ) ;
#88409 = CARTESIAN_POINT ( 'NONE',  ( 5.858611323429600226, -1.916351766245901977, -0.6279953093112633500 ) ) ;
#88410 = CARTESIAN_POINT ( 'NONE',  ( -8.188761592974051595, 9.616271948966963024, -1.082531754730543971 ) ) ;
#88411 = CARTESIAN_POINT ( 'NONE',  ( -0.1232117409455633916, -0.1621322592461546530, -2.156395338765437764 ) ) ;
#88412 = PLANE ( 'NONE',  #126052 ) ;
#88414 = CARTESIAN_POINT ( 'NONE',  ( -8.012344526598182026E-15, 12.04687500034140335, -1.575800808251669460 ) ) ;
#88413 = CARTESIAN_POINT ( 'NONE',  ( 0.5325469457231490900, 1.160272198634606955, -1.942242498246045113 ) ) ;
#88415 = CARTESIAN_POINT ( 'NONE',  ( -9.484092147959342967, 11.02352791316275216, 1.199719254218462483 ) ) ;
#88416 = CARTESIAN_POINT ( 'NONE',  ( 4.329314735043091389, -1.561880650076686861, -1.275557594027726394 ) ) ;
#88418 = CARTESIAN_POINT ( 'NONE',  ( 0.7553224350208649351, 1.845776580612036533, -0.5121453728616427448 ) ) ;
#88417 = CARTESIAN_POINT ( 'NONE',  ( -4.880572110795192486, 8.637825195995631589, 1.214306433183764966E-14 ) ) ;
#88419 = CARTESIAN_POINT ( 'NONE',  ( 1.364683531249988757, 1.446875000341421469, 0.000000000000000000 ) ) ;
#88420 = DIRECTION ( 'NONE',  ( 0.000000000000000000, 0.000000000000000000, -1.000000000000000000 ) ) ;
#88421 = EDGE_CURVE ( 'NONE', #158934, #26788, #29333, .T. ) ;
#88422 = CARTESIAN_POINT ( 'NONE',  ( -1.402160292154681736E-14, 9.812499999999998224, 1.732050807568881190 ) ) ;
#88423 = CARTESIAN_POINT ( 'NONE',  ( 3.088212622510533301, -1.699425283745788162, -0.2941843989033367524 ) ) ;
#88424 = CARTESIAN_POINT ( 'NONE',  ( 4.472210567661338843, 6.310941310395290493, 1.599625672291261402 ) ) ;
#88425 = CARTESIAN_POINT ( 'NONE',  ( 2.266550661271060640, -1.615954428537921483, -0.7220204016161780869 ) ) ;
#88426 = CARTESIAN_POINT ( 'NONE',  ( 10.55910270694468345, 11.21337466772398095, 0.7998128361456462443 ) ) ;
#88428 = PRESENTATION_LAYER_ASSIGNMENT (  '', '', ( #29523 ) ) ;
#88427 = CARTESIAN_POINT ( 'NONE',  ( 5.122202071631626552, -1.176711583861598243, -1.866687997650509079 ) ) ;
#88429 = VERTEX_POINT ( 'NONE', #61829 ) ;
#88430 = CARTESIAN_POINT ( 'NONE',  ( 4.131121313247118287, 1.848376352210901574, 0.8146727144991843250 ) ) ;
#88431 = CARTESIAN_POINT ( 'NONE',  ( -6.237633190739009237, 9.434933268240943249, 1.199719254218452047 ) ) ;
#88433 = CARTESIAN_POINT ( 'NONE',  ( 3.989861366179075830, -2.010826228832915508, 0.1511578083489423796 ) ) ;
#88432 = CARTESIAN_POINT ( 'NONE',  ( 4.723349490952149843, 1.845327050471495367, 1.044454997443218236 ) ) ;
#88435 = EDGE_LOOP ( 'NONE', ( #48802, #47276, #110361, #146559 ) ) ;
#88434 = CARTESIAN_POINT ( 'NONE',  ( 4.113381391103660967, 1.458659968308340993, 1.074121561303176264 ) ) ;
#88436 = CARTESIAN_POINT ( 'NONE',  ( 5.574337433874081427, 6.532423756721743580, -1.199719254218452047 ) ) ;
#88437 = EDGE_CURVE ( 'NONE', #6228, #74385, #137792, .T. ) ;
#88438 = ORIENTED_EDGE ( 'NONE', *, *, #15624, .T. ) ;
#88439 = CARTESIAN_POINT ( 'NONE',  ( 1.481098450213329754, 1.729700800547562478, -0.7128637423776187365 ) ) ;
#88440 = EDGE_CURVE ( 'NONE', #19519, #137701, #182027, .T. ) ;
#88441 = CARTESIAN_POINT ( 'NONE',  ( -10.91910517057295671, -9.994362614652946064, 0.1236848126708565976 ) ) ;
#88442 = CARTESIAN_POINT ( 'NONE',  ( 6.498695496729308907, -1.778006411731817060, -0.3456425897902185018 ) ) ;
#88444 = STYLED_ITEM ( 'NONE', ( #34642 ), #88722 ) ;
#88443 = CARTESIAN_POINT ( 'NONE',  ( 0.3999999999999576672, 0.6284510210557148202, -1.086836331270426781 ) ) ;
#88445 = CARTESIAN_POINT ( 'NONE',  ( -11.38600250725030172, 3.712543481068769857, -5.706073308245968256 ) ) ;
#88446 = CARTESIAN_POINT ( 'NONE',  ( -0.7500000000000006661, 8.489583334016129967, -1.299038105676657340 ) ) ;
#88447 = CARTESIAN_POINT ( 'NONE',  ( 1.364683531249988535, 3.426041667008085323, 0.7879004041258500513 ) ) ;
#88448 = CARTESIAN_POINT ( 'NONE',  ( -0.1581436608063293003, -1.178060542814472367, -1.506996232563104554 ) ) ;
#88449 = VECTOR ( 'NONE', #147679, 1000.000000000000000 ) ;
#88450 = CARTESIAN_POINT ( 'NONE',  ( 5.709392085130549077, 9.675058176045386205, 0.000000000000000000 ) ) ;
#88451 = CARTESIAN_POINT ( 'NONE',  ( -5.316205630334276400, 5.374863788244313767, -0.7216878364870338292 ) ) ;
#88452 = CARTESIAN_POINT ( 'NONE',  ( -4.437261413422502798, 8.398831758960053406, 0.000000000000000000 ) ) ;
#88453 = CARTESIAN_POINT ( 'NONE',  ( 4.254221937059123881, 0.9039275175388860051, -1.918405034562712608 ) ) ;
#88455 =( NAMED_UNIT ( * ) SI_UNIT ( $, .STERADIAN. ) SOLID_ANGLE_UNIT ( ) );
#88454 = CARTESIAN_POINT ( 'NONE',  ( -0.02968770228140015649, 0.7448490463385792903, -1.910291535987144629 ) ) ;
#88456 = CARTESIAN_POINT ( 'NONE',  ( 5.606699263565281477, 1.494642942781895023, -1.285547057225975509 ) ) ;
#88457 = CARTESIAN_POINT ( 'NONE',  ( -1.402160292154681736E-14, 0.9468750003414176941, -1.575800808251659024 ) ) ;
#88458 = CARTESIAN_POINT ( 'NONE',  ( 0.5627444733627232631, 0.5882401669465211480, 1.925320163072720359 ) ) ;
#88459 = VERTEX_POINT ( 'NONE', #183026 ) ;
#88460 = CARTESIAN_POINT ( 'NONE',  ( 6.298082486376491929, -1.000091913425070311, -1.866304853008766917 ) ) ;
#88461 = CARTESIAN_POINT ( 'NONE',  ( 11.84810327283921261, 6.845834857362776305, 1.964380509715618617 ) ) ;
#88462 = CARTESIAN_POINT ( 'NONE',  ( 1.943885480841448965, 1.426152643941134501, 1.501071833787496645 ) ) ;
#88463 = ORIENTED_EDGE ( 'NONE', *, *, #124624, .F. ) ;
#88464 = CARTESIAN_POINT ( 'NONE',  ( 5.041653019435334393, 6.975290837464928728, -1.599625672291269396 ) ) ;
#88465 = CARTESIAN_POINT ( 'NONE',  ( 6.249382461256315580, 6.255644057745969988, -0.7998128361456481317 ) ) ;
#88466 = EDGE_LOOP ( 'NONE', ( #67113, #185577, #60749, #138654 ) ) ;
#88468 = CARTESIAN_POINT ( 'NONE',  ( 4.656335691289526402, 7.519809842224722374, -1.199719254218452047 ) ) ;
#88467 = CARTESIAN_POINT ( 'NONE',  ( 4.541018360983569480, -1.615799657739678263, -1.326631217474142366 ) ) ;
#88471 = EDGE_LOOP ( 'NONE', ( #131813, #37446, #18724, #78876, #40193, #194449, #142303, #58502 ) ) ;
#88470 = CARTESIAN_POINT ( 'NONE',  ( 1.400706157114139261, -0.2655193030335687987, -1.791778796870816759 ) ) ;
#88469 = CARTESIAN_POINT ( 'NONE',  ( 3.434410497111122673, 1.780829521046650932, 0.4009754434649847044 ) ) ;
#88472 = CARTESIAN_POINT ( 'NONE',  ( 9.495541471879706208, -9.135662283479117463, -0.2985557471763389259 ) ) ;
#88473 = DIRECTION ( 'NONE',  ( 0.000000000000000000, 1.000000000000000000, 0.000000000000000000 ) ) ;
#88474 = CARTESIAN_POINT ( 'NONE',  ( 4.788207028248289809, -1.043783763870303360, 1.944324211313207318 ) ) ;
#88475 = CARTESIAN_POINT ( 'NONE',  ( 7.904567251967224095, 9.180748867838630645, 1.199719254218462483 ) ) ;
#88476 = CARTESIAN_POINT ( 'NONE',  ( -1.364683531250000748, 8.671875000341403350, 0.000000000000000000 ) ) ;
#88477 = CARTESIAN_POINT ( 'NONE',  ( 2.543496672408153358, -1.783599581865771500, 0.6900697577220117340 ) ) ;
#88478 =( BOUNDED_SURFACE ( )  B_SPLINE_SURFACE ( 3, 3, ( 
 ( #130328, #162763, #196317, #170197, #73767, #20727, #201606, #168076, #203742, #21781 ),
 ( #187513, #53255, #86822, #119385, #3411, #52192, #70536, #88972, #69477, #4464 ),
 ( #136655, #185373, #40214, #155027, #138787, #35928, #87890, #39144, #152886, #118318 ),
 ( #36993, #120468, #103077, #169132, #202680, #153963, #7683, #184304, #105225, #102006 ),
 ( #6612, #19674, #204807, #186440, #54329, #38077, #72692, #104149, #5530, #71610 ),
 ( #137723, #56458, #55387, #121542, #171265, #22859, #122620, #23936, #188581, #106323 ),
 ( #135585, #172346, #90040, #156098, #139863, #85754, #151835, #26076, #111673, #174498 ) ),
 .UNSPECIFIED., .T., .F., .T. ) 
 B_SPLINE_SURFACE_WITH_KNOTS ( ( 4, 3, 4 ),
 ( 4, 1, 1, 1, 1, 1, 1, 4 ),
 ( 0.000000000000000000, 0.5000000000000000000, 1.000000000000000000 ),
 ( 0.000000000000000000, 0.09790276019723312406, 0.1918320694002237370, 0.2608036337010187777, 0.3626611837559554630, 0.5214803378330250538, 0.7337833476510040587, 1.000000000000000000 ),
 .UNSPECIFIED. ) 
 GEOMETRIC_REPRESENTATION_ITEM ( )  RATIONAL_B_SPLINE_SURFACE ( (
 ( 1.000000000000000444, 1.000000000000000444, 1.000000000000000000, 1.000000000000000444, 1.000000000000000222, 1.000000000000000222, 1.000000000000000444, 1.000000000000000000, 1.000000000000000222, 1.000000000000000222),
 ( 0.3333333333333334814, 0.3333333333333334814, 0.3333333333333334814, 0.3333333333333334259, 0.3333333333333333703, 0.3333333333333334259, 0.3333333333333335369, 0.3333333333333333703, 0.3333333333333334259, 0.3333333333333334259),
 ( 0.3333333333333334814, 0.3333333333333334814, 0.3333333333333334814, 0.3333333333333334259, 0.3333333333333333703, 0.3333333333333334259, 0.3333333333333335369, 0.3333333333333333703, 0.3333333333333334259, 0.3333333333333334259),
 ( 1.000000000000000444, 1.000000000000000444, 1.000000000000000000, 1.000000000000000444, 1.000000000000000222, 1.000000000000000222, 1.000000000000000444, 1.000000000000000000, 1.000000000000000222, 1.000000000000000222),
 ( 0.3333333333333334814, 0.3333333333333334814, 0.3333333333333334814, 0.3333333333333334259, 0.3333333333333333703, 0.3333333333333334259, 0.3333333333333335369, 0.3333333333333333703, 0.3333333333333334259, 0.3333333333333334259),
 ( 0.3333333333333334814, 0.3333333333333334814, 0.3333333333333334814, 0.3333333333333334259, 0.3333333333333333703, 0.3333333333333334259, 0.3333333333333335369, 0.3333333333333333703, 0.3333333333333334259, 0.3333333333333334259),
 ( 1.000000000000000444, 1.000000000000000444, 1.000000000000000000, 1.000000000000000444, 1.000000000000000222, 1.000000000000000222, 1.000000000000000444, 1.000000000000000000, 1.000000000000000222, 1.000000000000000222) ) ) 
 REPRESENTATION_ITEM ( '' )  SURFACE ( )  );
#88479 = CARTESIAN_POINT ( 'NONE',  ( 7.801827329660018684, 11.18955008699033726, 1.199719254218460707 ) ) ;
#88480 = CARTESIAN_POINT ( 'NONE',  ( 0.000000000000000000, 0.08000000000000020983, 11.09999999999999964 ) ) ;
#88481 = CARTESIAN_POINT ( 'NONE',  ( -1.500000000000008216, 10.28125000068279249, 3.469446951953614189E-15 ) ) ;
#88482 = CARTESIAN_POINT ( 'NONE',  ( 6.198795224570643470, 1.821041368708445907, 1.219022265761634971 ) ) ;
#88483 = CARTESIAN_POINT ( 'NONE',  ( 5.646014316602349759, 7.456765758048159221, -1.329534273556526758 ) ) ;
#88484 = DIRECTION ( 'NONE',  ( -0.6095094443613831015, -1.732612801327082678E-12, 0.7927788072560203458 ) ) ;
#88485 = ORIENTED_EDGE ( 'NONE', *, *, #181214, .F. ) ;
#88486 = VERTEX_POINT ( 'NONE', #32520 ) ;
#88487 = CARTESIAN_POINT ( 'NONE',  ( 9.578206920975004479, -9.954640969533222972, -0.1671882237015355210 ) ) ;
#88488 = CARTESIAN_POINT ( 'NONE',  ( 3.321420150926617687, -1.803644938814071175, 0.4956094624995326381 ) ) ;
#88489 = CARTESIAN_POINT ( 'NONE',  ( -3.285556943750000070, -1.596874999522043037, 0.000000000000000000 ) ) ;
#88490 = CARTESIAN_POINT ( 'NONE',  ( -3.602337597214539753E-15, 12.59375000068279782, 1.500000000000001554 ) ) ;
#88491 = CARTESIAN_POINT ( 'NONE',  ( -7.700668062882078502, 9.046829497192987901, -1.082531754730543971 ) ) ;
#88492 = CARTESIAN_POINT ( 'NONE',  ( 3.562760505341037831, 7.378580699531681830, -1.734723475976807094E-15 ) ) ;
#88493 = CARTESIAN_POINT ( 'NONE',  ( 6.420769920452011448, -1.468259139554881409, 1.459777494992514857 ) ) ;
#88494 = CARTESIAN_POINT ( 'NONE',  ( 1.212517793387542842, 1.944078472882956987, 0.5350667013180390175 ) ) ;
#88495 = CARTESIAN_POINT ( 'NONE',  ( -8.513630394377489807, 12.01998699582738972, -1.199719254218446718 ) ) ;
#88496 = CARTESIAN_POINT ( 'NONE',  ( 5.806634928402749196, 9.996434193103704402, -0.7998128361456481317 ) ) ;
#88497 = CARTESIAN_POINT ( 'NONE',  ( 2.236732156574683827, 5.553345249405011508, 1.040834085586084257E-14 ) ) ;
#88498 = CARTESIAN_POINT ( 'NONE',  ( 1.166276502169643070, -1.387892208999995436, 1.695937554688830451 ) ) ;
#88499 = CARTESIAN_POINT ( 'NONE',  ( 5.514214477338499343, -0.8245889995748826307, -1.628937154514856767 ) ) ;
#88500 = CARTESIAN_POINT ( 'NONE',  ( -5.122283107864663343, 4.870418468797203637, 0.000000000000000000 ) ) ;
#88501 = CARTESIAN_POINT ( 'NONE',  ( 6.861835142292147083, 7.178098218861903135, 0.7216878364870328300 ) ) ;
#88503 = ADVANCED_FACE ( 'NONE', ( #146305 ), #47735, .F. ) ;
#88502 = CARTESIAN_POINT ( 'NONE',  ( 8.238550898598388628, 12.76339314834017102, 0.7998128361456462443 ) ) ;
#88504 = CARTESIAN_POINT ( 'NONE',  ( -6.330731382938325602, 6.350551133041632212, 0.7998128361456281477 ) ) ;
#88505 = CARTESIAN_POINT ( 'NONE',  ( 3.517450787741589036, 6.191110788085444128, -1.199719254218446718 ) ) ;
#88506 = CARTESIAN_POINT ( 'NONE',  ( 7.851580356089786328, 8.332800968292465527, 0.000000000000000000 ) ) ;
#88507 = ORIENTED_EDGE ( 'NONE', *, *, #71393, .T. ) ;
#88509 = CARTESIAN_POINT ( 'NONE',  ( 6.398696026112846269, -1.975200287401058130, -0.3884956089365321774 ) ) ;
#88508 = CARTESIAN_POINT ( 'NONE',  ( 4.089279031174639201, -0.7008038172400687937, 1.702867937621636463 ) ) ;
#88510 = CARTESIAN_POINT ( 'NONE',  ( 1.529136539685072238, 2.264261833246409505, -0.3938019620175516322 ) ) ;
#88512 = CARTESIAN_POINT ( 'NONE',  ( 6.977413161700751765, -0.1449424838519241254, 1.929857014940839832 ) ) ;
#88511 = CARTESIAN_POINT ( 'NONE',  ( 4.582292731738905722, 5.408724944192588424, -1.082531754730548412 ) ) ;
#88513 = CARTESIAN_POINT ( 'NONE',  ( -3.567766978690493307, 7.314145241780881435, 1.040834085586084257E-14 ) ) ;
#88514 = CARTESIAN_POINT ( 'NONE',  ( -5.055603177353559019, 6.862042912877393874, -1.261393572340614666 ) ) ;
#88515 = CARTESIAN_POINT ( 'NONE',  ( 3.884940529579200774, -1.786240503712609895, -0.6835825222790415934 ) ) ;
#88516 = CARTESIAN_POINT ( 'NONE',  ( -10.45741655484220267, 11.09474082360439873, -0.7998128361456221525 ) ) ;
#88517 = CARTESIAN_POINT ( 'NONE',  ( 6.229241538080760421, 6.920885192246182704, -0.8282608007674150397 ) ) ;
#88518 = CARTESIAN_POINT ( 'NONE',  ( -6.861835142292179057, 9.098836647464588978, 1.443375672974064550 ) ) ;
#88520 = CARTESIAN_POINT ( 'NONE',  ( 1.340467186903429253, 0.3614942610149494695, 1.835218787103513050 ) ) ;
#88519 = CARTESIAN_POINT ( 'NONE',  ( 2.946908815893133138, -1.710673590971498292, -1.201729372296795662 ) ) ;
#88521 = CARTESIAN_POINT ( 'NONE',  ( 1.950545848857932807, 1.388271641964162084, 1.462223312268404074 ) ) ;
#88522 = CARTESIAN_POINT ( 'NONE',  ( 8.432808358020016826, 10.86136238915529084, 1.443375672974076540 ) ) ;
#88523 = CARTESIAN_POINT ( 'NONE',  ( 1.364683531249988535, 3.926041667008087543, 0.7879004041258499402 ) ) ;
#88524 = CARTESIAN_POINT ( 'NONE',  ( 3.579424886596099586, -0.8542006638617373193, 1.516299650553302181 ) ) ;
#88525 = CARTESIAN_POINT ( 'NONE',  ( 5.345992642490140057, 5.131412925860272090, 1.040834085586084257E-14 ) ) ;
#88527 = CARTESIAN_POINT ( 'NONE',  ( 11.86145016429273014, 13.50587876334730453, -1.100000000000000089 ) ) ;
#88526 = CARTESIAN_POINT ( 'NONE',  ( -6.689586359223961054, -7.817744194000433744, 6.745922712994593340 ) ) ;
#88528 = CARTESIAN_POINT ( 'NONE',  ( 3.967213729759576868, 0.2084270747255561884, -1.712163910207653128 ) ) ;
#88529 = CARTESIAN_POINT ( 'NONE',  ( 4.265290774032561849, 2.125562838249666964, -0.5332280334861272397 ) ) ;
#88530 = CARTESIAN_POINT ( 'NONE',  ( 5.268293329372571776, 1.085216321637239023, 1.921556908365213312 ) ) ;
#88531 = CARTESIAN_POINT ( 'NONE',  ( -9.928285507789787800, 5.423409019249701757, -6.081825614513333811 ) ) ;
#88532 = CARTESIAN_POINT ( 'NONE',  ( 3.608415011292832819, 2.171239808225163159, 0.005094884836047069293 ) ) ;
#88533 = CARTESIAN_POINT ( 'NONE',  ( 2.596107596775329540, -1.820790993511243849, -0.1344670722737417168 ) ) ;
#88534 = CARTESIAN_POINT ( 'NONE',  ( 0.3999999999999758193, 2.999999999999999112, 7.500000000000000000 ) ) ;
#88535 = CARTESIAN_POINT ( 'NONE',  ( 4.206348283080693307, 1.299600563804912623, -1.671539989125019332 ) ) ;
#88536 = CARTESIAN_POINT ( 'NONE',  ( -0.4019237886466802689, 9.729914550367427140, -1.500000000000002887 ) ) ;
#88537 = ORIENTED_EDGE ( 'NONE', *, *, #162856, .T. ) ;
#88539 = CARTESIAN_POINT ( 'NONE',  ( 0.6823417656249899377, 2.155208333674753174, 1.181850606188767472 ) ) ;
#88538 = CARTESIAN_POINT ( 'NONE',  ( 4.968466765020612463, -2.157917790226408172, -0.7739415147586664601 ) ) ;
#88540 = CARTESIAN_POINT ( 'NONE',  ( 6.720655732516647163, 0.5950723047917580999, 1.879543361893110109 ) ) ;
#88541 = CARTESIAN_POINT ( 'NONE',  ( 8.191097360950562845, 12.70803068775103739, -0.7998128361456352531 ) ) ;
#88542 = CARTESIAN_POINT ( 'NONE',  ( 0.8035760164417544704, 1.868272328500224289, -1.003034915376184388 ) ) ;
#88543 = CARTESIAN_POINT ( 'NONE',  ( -6.900736999675794792, 7.153207375817628666, 1.040834085586084257E-14 ) ) ;
#88544 = DIRECTION ( 'NONE',  ( 0.000000000000000000, 0.000000000000000000, -1.000000000000000000 ) ) ;
#88545 = CARTESIAN_POINT ( 'NONE',  ( -4.080641047588902559, 7.704572288921609058, -0.7216878364870257245 ) ) ;
#88546 = CARTESIAN_POINT ( 'NONE',  ( 6.883263157960363365, 3.690127339433949327, 2.567897385111846731 ) ) ;
#88548 = ORIENTED_EDGE ( 'NONE', *, *, #196068, .T. ) ;
#88547 = STYLED_ITEM ( 'NONE', ( #63469 ), #194681 ) ;
#88549 = CARTESIAN_POINT ( 'NONE',  ( 5.537732479266092689, -1.587839044716709669, 1.242724925242834066 ) ) ;
#88551 = CARTESIAN_POINT ( 'NONE',  ( 3.045816552677531597, 1.455321998776702319, 1.461834479831431555 ) ) ;
#88550 = CARTESIAN_POINT ( 'NONE',  ( 4.449046963578762615, 8.342305224150557308, -0.7998128361456231517 ) ) ;
#88553 = CARTESIAN_POINT ( 'NONE',  ( -0.1408020194050146334, 2.009929383927198998, -2.515281701100045009 ) ) ;
#88552 = CARTESIAN_POINT ( 'NONE',  ( 5.820193082016415609, 10.01225203898631655, 0.000000000000000000 ) ) ;
#88554 = CARTESIAN_POINT ( 'NONE',  ( 5.580062740476173566, 8.667767742934335828, 1.199719254218451159 ) ) ;
#88556 = EDGE_CURVE ( 'NONE', #126234, #206477, #152649, .T. ) ;
#88555 = CARTESIAN_POINT ( 'NONE',  ( 3.285556943750000070, -0.9843749995220412163, 0.000000000000000000 ) ) ;
#88557 = LINE ( 'NONE', #154617, #119874 ) ;
#88558 = CARTESIAN_POINT ( 'NONE',  ( 6.210891007176935652, -0.2719346519345893776, 2.174439262769362280 ) ) ;
#88559 = CARTESIAN_POINT ( 'NONE',  ( 3.287732575140737801, 1.587837554856496691, -1.242726844152845178 ) ) ;
#88560 = CARTESIAN_POINT ( 'NONE',  ( 3.509164994824386596, -1.813400730843343966, 0.3181347684400454012 ) ) ;
#88561 = EDGE_CURVE ( 'NONE', #165933, #168625, #147200, .T. ) ;
#88562 = CARTESIAN_POINT ( 'NONE',  ( 6.518772930072240790, 6.499656594706071822, -0.7998128361456281477 ) ) ;
#88563 =( LENGTH_UNIT ( ) NAMED_UNIT ( * ) SI_UNIT ( .MILLI., .METRE. ) );
#88564 = CARTESIAN_POINT ( 'NONE',  ( 0.1820471141361617307, -1.670984272841398832, -0.4269972090983116253 ) ) ;
#88565 = CARTESIAN_POINT ( 'NONE',  ( -4.451154503988200339, 4.087435097607984957, 1.214306433183764966E-14 ) ) ;
#88566 = CARTESIAN_POINT ( 'NONE',  ( 0.5285108043569552994, -1.967359331218739626, 1.188758619093014168 ) ) ;
#88567 = CARTESIAN_POINT ( 'NONE',  ( -5.228640796364566690, 9.251831362400652736, -0.7998128361456231517 ) ) ;
#88568 = CARTESIAN_POINT ( 'NONE',  ( 6.420815857685610695, 2.108269355124866351, 0.8215519888849237562 ) ) ;
#88569 = CARTESIAN_POINT ( 'NONE',  ( 3.194068465612946994, -0.8531780664592978347, 1.925702383005133855 ) ) ;
#88570 = CARTESIAN_POINT ( 'NONE',  ( -3.610214042988883598, 7.433943160120816351, 0.7998128361456352531 ) ) ;
#88571 = CARTESIAN_POINT ( 'NONE',  ( 7.426115451983150706, 9.686887332112256388, -1.599625672291262513 ) ) ;
#88572 = CARTESIAN_POINT ( 'NONE',  ( 6.170369307550823912, 7.331757292631694511, 1.082531754730549967 ) ) ;
#88573 = DIRECTION ( 'NONE',  ( 1.000000000000000000, 0.000000000000000000, 0.000000000000000000 ) ) ;
#88574 = CARTESIAN_POINT ( 'NONE',  ( -7.088215381846223906, 7.164006121775713609, 0.7998128361456341429 ) ) ;
#88575 = CARTESIAN_POINT ( 'NONE',  ( 6.222829318548112276, 9.243422724072711816, -1.082531754730537976 ) ) ;
#88576 = CARTESIAN_POINT ( 'NONE',  ( 5.480859523967800406, 6.436073219340427976, 1.263442102793509880 ) ) ;
#88577 = CARTESIAN_POINT ( 'NONE',  ( -3.411848212133334446, 7.132240014130862171, 0.7998128361456341429 ) ) ;
#88578 = CARTESIAN_POINT ( 'NONE',  ( 3.955514033904330873, -1.931546270572735979, 1.097109147590840550 ) ) ;
#88579 = CARTESIAN_POINT ( 'NONE',  ( 2.361504994916805877, 2.148894721571582789, -0.4289216190115978100 ) ) ;
#88580 = CARTESIAN_POINT ( 'NONE',  ( -5.377780486114890124, 9.425827667109372143, 0.000000000000000000 ) ) ;
#88581 = CARTESIAN_POINT ( 'NONE',  ( -3.949167883330528372, 7.829389307186077396, 1.214306433183764966E-14 ) ) ;
#88582 = CARTESIAN_POINT ( 'NONE',  ( 5.090269282739749102, 1.010147525469132557, -1.681691772506640481 ) ) ;
#88583 = CARTESIAN_POINT ( 'NONE',  ( -1.364683531250012516, 1.530208333674756505, 0.7879004041258379498 ) ) ;
#88584 = CARTESIAN_POINT ( 'NONE',  ( -4.502716413514313842, 5.386162249589033557, -1.082531754730549967 ) ) ;
#88586 = CARTESIAN_POINT ( 'NONE',  ( -5.585596099150182958, 8.499983968108443477, -1.082531754730544860 ) ) ;
#88585 = VECTOR ( 'NONE', #24684, 1000.000000000000000 ) ;
#88587 = CARTESIAN_POINT ( 'NONE',  ( 5.097945154717048233, 1.425953928781589886, 1.569717048080176314 ) ) ;
#88588 = CARTESIAN_POINT ( 'NONE',  ( -4.995253251992230581, 4.792493313604505367, 0.000000000000000000 ) ) ;
#88589 = ORIENTED_EDGE ( 'NONE', *, *, #66088, .T. ) ;
#88590 = CARTESIAN_POINT ( 'NONE',  ( 5.840740251263128791, 0.4172088472891195554, 2.120894824392767664 ) ) ;
#88591 = CARTESIAN_POINT ( 'NONE',  ( 4.957477724091233995, 8.935474444748447098, -0.7998128361456281477 ) ) ;
#88592 = CARTESIAN_POINT ( 'NONE',  ( 4.739718475747470627, 1.836682745182907972, 0.1304020654292817605 ) ) ;
#88593 = CARTESIAN_POINT ( 'NONE',  ( -5.907986510169434879, 6.002582827494773454, 0.1128355114666315662 ) ) ;
#88594 = CARTESIAN_POINT ( 'NONE',  ( -1.364683531250000748, 1.321875000341421469, 0.000000000000000000 ) ) ;
#88595 = CARTESIAN_POINT ( 'NONE',  ( 0.06344835015564037617, -1.139564578658038618, 1.315610641012928239 ) ) ;
#88596 = FACE_OUTER_BOUND ( 'NONE', #193997, .T. ) ;
#88597 = FACE_OUTER_BOUND ( 'NONE', #173744, .T. ) ;
#88598 = CARTESIAN_POINT ( 'NONE',  ( -0.4465194593918104249, 3.080450244942127380, 0.4155024747329021939 ) ) ;
#88599 = CARTESIAN_POINT ( 'NONE',  ( 4.346650381253648554, 0.5737703434565506466, 2.084106190491950006 ) ) ;
#88600 = CARTESIAN_POINT ( 'NONE',  ( -3.113568832632681360, 6.784247404713427798, -0.7998128361456281477 ) ) ;
#88601 = EDGE_CURVE ( 'NONE', #137788, #45474, #96493, .T. ) ;
#88602 = CARTESIAN_POINT ( 'NONE',  ( -7.009202228140744673, 10.16085778526412042, -1.082531754730537088 ) ) ;
#88603 = CARTESIAN_POINT ( 'NONE',  ( 3.081113354808207916, -0.1575343947536785305, -2.156009052512488200 ) ) ;
#88604 = CARTESIAN_POINT ( 'NONE',  ( 4.675049781410951510, 0.003005680196035282782, -1.971530341645504780 ) ) ;
#88605 = CARTESIAN_POINT ( 'NONE',  ( 3.690549081386824248, -1.031632686913460883, -1.393354295182136715 ) ) ;
#88606 = B_SPLINE_CURVE_WITH_KNOTS ( 'NONE', 3,
 ( #185316, #36938, #116125, #103020 ),
 .UNSPECIFIED., .F., .F.,
 ( 4, 4 ),
 ( 0.000000000000000000, 3.568395612623403724E-05 ),
 .UNSPECIFIED. ) ;
#88607 = CARTESIAN_POINT ( 'NONE',  ( 0.5213437761196970666, -2.079166062760181788, 0.6930039600180630810 ) ) ;
#88608 = CARTESIAN_POINT ( 'NONE',  ( 1.448709080243043124, 2.305037702096077723, 0.1111474144101440020 ) ) ;
#88609 = CARTESIAN_POINT ( 'NONE',  ( 3.901680821178232339, -0.6019389665811913925, 1.970883251864594454 ) ) ;
#88610 = CARTESIAN_POINT ( 'NONE',  ( 5.847205921155025798, 0.5594960185140216424, -1.859740419532672773 ) ) ;
#88611 = CARTESIAN_POINT ( 'NONE',  ( -7.741342523278709642, 10.05465224862374285, 1.443375672974090751 ) ) ;
#88612 = VECTOR ( 'NONE', #152947, 1000.000000000000000 ) ;
#88613 = CARTESIAN_POINT ( 'NONE',  ( -4.630991987519598396, 7.560518531151607213, 1.199719254218452935 ) ) ;
#88614 = CARTESIAN_POINT ( 'NONE',  ( -11.89942855770814134, 13.79999999999999893, -0.7000000000000009548 ) ) ;
#88615 = VERTEX_POINT ( 'NONE', #179848 ) ;
#88616 = CARTESIAN_POINT ( 'NONE',  ( -7.714226216051410567, 9.062647342557177410, 1.082531754730558626 ) ) ;
#88617 = CARTESIAN_POINT ( 'NONE',  ( 3.329339556154627289, 0.05228039400686017302, 2.206313527657398854 ) ) ;
#88618 = CARTESIAN_POINT ( 'NONE',  ( 3.285556943750000070, -3.521874999522042859, 0.000000000000000000 ) ) ;
#88619 = ORIENTED_EDGE ( 'NONE', *, *, #6240, .T. ) ;
#88620 = CARTESIAN_POINT ( 'NONE',  ( 0.5493571781046421298, 1.373546829346812714, 1.255761559867879962 ) ) ;
#88621 = CARTESIAN_POINT ( 'NONE',  ( -0.02880301295724378360, 1.300294777490899056, -2.522425657339548266 ) ) ;
#88622 = FILL_AREA_STYLE ('',( #74496 ) ) ;
#88623 =( NAMED_UNIT ( * ) SI_UNIT ( $, .STERADIAN. ) SOLID_ANGLE_UNIT ( ) );
#88625 = CARTESIAN_POINT ( 'NONE',  ( 6.925078400183552141, 7.052169149086129352, 2.642497803771151954 ) ) ;
#88624 = CARTESIAN_POINT ( 'NONE',  ( -6.392190997713585787, 6.905894197498253284, -0.8087526810517248199 ) ) ;
#88626 = CARTESIAN_POINT ( 'NONE',  ( 6.685540632719009224, -0.7820230359689305244, 1.665195522482863399 ) ) ;
#88627 = ORIENTED_EDGE ( 'NONE', *, *, #92114, .F. ) ;
#88628 = CARTESIAN_POINT ( 'NONE',  ( 2.219669609025213930, -1.999274383190910775, 0.4996674803129513842 ) ) ;
#88629 = CARTESIAN_POINT ( 'NONE',  ( -0.6801582343750420812, -0.06770833299193229626, 1.178068619123801675 ) ) ;
#88630 = CARTESIAN_POINT ( 'NONE',  ( -6.021792782764022078, 10.17717534653336209, -0.7998128361456291469 ) ) ;
#88631 = CYLINDRICAL_SURFACE ( 'NONE', #71689, 0.07999999999999998779 ) ;
#88632 = CARTESIAN_POINT ( 'NONE',  ( 4.090809663021327758, 5.795697244990093644, 1.599625672291267398 ) ) ;
#88633 = CARTESIAN_POINT ( 'NONE',  ( 0.9364841293936125854, 2.030268333626069843, 0.3529954148920669277 ) ) ;
#88635 = CARTESIAN_POINT ( 'NONE',  ( 4.950658015114751009, -1.558304906039936988, -0.9804572199803849308 ) ) ;
#88634 = CARTESIAN_POINT ( 'NONE',  ( -1.854512760316423536, 9.001999999999998892, 2.484105960264900936 ) ) ;
#88636 = CARTESIAN_POINT ( 'NONE',  ( 6.331821432781979730, 7.345878745455822312, -1.199719254218445830 ) ) ;
#88637 = CARTESIAN_POINT ( 'NONE',  ( -6.414942957921379474, 7.513130201443591005, -1.199719254218452047 ) ) ;
#88638 = CARTESIAN_POINT ( 'NONE',  ( 5.293864907607461312, 4.747529046662108954, 2.500000000000000444 ) ) ;
#88639 = EDGE_CURVE ( 'NONE', #53408, #122076, #180898, .T. ) ;
#88640 = CARTESIAN_POINT ( 'NONE',  ( 5.742855475442601332, 0.4270144693867898300, 2.165010647329483895 ) ) ;
#88641 = CARTESIAN_POINT ( 'NONE',  ( 0.8608787451157871029, -1.566265403972837866, 1.489986575276234460 ) ) ;
#88642 = CARTESIAN_POINT ( 'NONE',  ( -4.284013352238262407, 6.021101549076499637, -1.443375672974053447 ) ) ;
#88643 = CARTESIAN_POINT ( 'NONE',  ( 0.3516297456669579269, -1.353986107606550471, -1.350798769753497552 ) ) ;
#88644 = CARTESIAN_POINT ( 'NONE',  ( 0.6027503803631119039, 1.865048444749048739, 0.7672877736318934883 ) ) ;
#88645 = CARTESIAN_POINT ( 'NONE',  ( 6.333067150914805765, 9.442309871825708356, 1.082531754730549967 ) ) ;
#88646 = CARTESIAN_POINT ( 'NONE',  ( 7.220996296834734096, 15.51845925587262798, -9.590923008284281792 ) ) ;
#88647 = CARTESIAN_POINT ( 'NONE',  ( 6.481121912432155519, -1.750430003815309998, -0.7703581994758443852 ) ) ;
#88648 = DIRECTION ( 'NONE',  ( 5.551115123125766062E-17, 0.000000000000000000, -1.000000000000000000 ) ) ;
#88649 = CARTESIAN_POINT ( 'NONE',  ( 1.428351348257720588, 1.801920623737063520, 0.5021531274154652502 ) ) ;
#88650 = CARTESIAN_POINT ( 'NONE',  ( 2.835173002801576914, -1.651343842416473917, -1.157098616274463865 ) ) ;
#88652 = CARTESIAN_POINT ( 'NONE',  ( 11.41108574530292863, 13.75836855377623635, 3.405883542057587476 ) ) ;
#88651 = CARTESIAN_POINT ( 'NONE',  ( -1.364683531250000748, 0.5093750003414208027, 0.000000000000000000 ) ) ;
#88654 = CARTESIAN_POINT ( 'NONE',  ( 4.846364118386396136, 2.100373345016784743, 0.1556085008114059531 ) ) ;
#88653 = CARTESIAN_POINT ( 'NONE',  ( -7.720478407978036195, 11.09464301169468037, -1.199719254218446718 ) ) ;
#88655 = CARTESIAN_POINT ( 'NONE',  ( 8.392660782059197189, 9.750191319612612872, 1.199719254218462483 ) ) ;
#88657 = CARTESIAN_POINT ( 'NONE',  ( -9.365985188942097750, 9.821404230054264772, 0.7998128361456462443 ) ) ;
#88656 = CARTESIAN_POINT ( 'NONE',  ( 3.725458348705031231, 7.568394850123006279, -1.734723475976807094E-15 ) ) ;
#88658 = CARTESIAN_POINT ( 'NONE',  ( 0.07538891330674687974, -7.154544010627095219, -9.499700864329895467 ) ) ;
#88659 = CARTESIAN_POINT ( 'NONE',  ( 4.219013726799848207, 1.558537513506755845, -1.284668789120123833 ) ) ;
#88660 = CARTESIAN_POINT ( 'NONE',  ( 0.6823417656249917140, 4.342708333674755394, 1.181850606188765695 ) ) ;
#88661 = CARTESIAN_POINT ( 'NONE',  ( 6.461391904901197414, 1.712781507706350848, 1.149079448644703350 ) ) ;
#88662 = CARTESIAN_POINT ( 'NONE',  ( 9.761507412159302177, 10.49077285704843199, -0.7216878364870257245 ) ) ;
#88663 = CARTESIAN_POINT ( 'NONE',  ( 5.009125465012424172, 1.878017946038791575, 1.070212309444783294 ) ) ;
#88664 = CARTESIAN_POINT ( 'NONE',  ( 6.282224075085741433, 8.422623735723785643, 1.599625672291268286 ) ) ;
#88665 = CARTESIAN_POINT ( 'NONE',  ( 1.364683531249986537, -1.073958332991911790, 0.7879004041258500513 ) ) ;
#88667 = CARTESIAN_POINT ( 'NONE',  ( -7.900729602272470231, -6.805008568744116637, 7.460470246983066822 ) ) ;
#88666 = CARTESIAN_POINT ( 'NONE',  ( 5.448397627845284141, 7.449826213943242514, 1.599625672291268286 ) ) ;
#88668 =( BOUNDED_SURFACE ( )  B_SPLINE_SURFACE ( 3, 2, ( 
 ( #3251, #117094, #164719 ),
 ( #118166, #183094, #184152 ),
 ( #49907, #150619, #182014 ),
 ( #19516, #85593, #35775 ),
 ( #33645, #152730, #70383 ),
 ( #69319, #16308, #165791 ) ),
 .UNSPECIFIED., .F., .F., .F. ) 
 B_SPLINE_SURFACE_WITH_KNOTS ( ( 4, 2, 4 ),
 ( 3, 3 ),
 ( -4.065758146820641628E-19, 0.0003831416164015016010, 0.0007662832328030036357 ),
 ( 0.000000000000000000, 1.000000000000000000 ),
 .UNSPECIFIED. ) 
 GEOMETRIC_REPRESENTATION_ITEM ( )  RATIONAL_B_SPLINE_SURFACE ( (
 ( 1.000000000000000000, 0.7071067811865475727, 1.000000000000000000),
 ( 1.000000000000000000, 0.6829713513656306967, 1.000000000000000000),
 ( 1.000000000000000000, 0.6534833722368420528, 1.000000000000000000),
 ( 1.000000000000000000, 0.6054027484666428816, 1.000000000000000000),
 ( 1.000000000000000000, 0.5875453974412017111, 1.000000000000000000),
 ( 1.000000000000000000, 0.5879095031487528988, 1.000000000000000000) ) ) 
 REPRESENTATION_ITEM ( '' )  SURFACE ( )  );
#88669 = CARTESIAN_POINT ( 'NONE',  ( 6.927853306458739979, 10.06595070996845642, 1.082531754730558626 ) ) ;
#88670 = CARTESIAN_POINT ( 'NONE',  ( 1.908858375081338377, 0.6798548000985217277, 2.062075944584631504 ) ) ;
#88672 = CARTESIAN_POINT ( 'NONE',  ( 1.927068723821170559, -1.203646435588998420, -1.393412863611859454 ) ) ;
#88671 = CARTESIAN_POINT ( 'NONE',  ( -5.368665641331555882, 8.246898433986675769, 1.082531754730548412 ) ) ;
#88673 = B_SPLINE_CURVE_WITH_KNOTS ( 'NONE', 3,
 ( #184346, #4505, #70576, #173471 ),
 .UNSPECIFIED., .F., .F.,
 ( 4, 4 ),
 ( 0.0006426233018256924130, 0.0009180112871920716004 ),
 .UNSPECIFIED. ) ;
#88674 = CARTESIAN_POINT ( 'NONE',  ( 0.6823417656249899377, 3.676041667008085767, -1.181850606188754593 ) ) ;
#88675 = CARTESIAN_POINT ( 'NONE',  ( 2.806388347806953121, 1.585463108415147149, -1.513251884624075672 ) ) ;
#88676 = CARTESIAN_POINT ( 'NONE',  ( 3.086313801757624820, 6.452272078211774620, 0.4027703449977940720 ) ) ;
#88677 = CARTESIAN_POINT ( 'NONE',  ( 3.397619368019880959, 1.782376118940771637, 1.393485768503288202 ) ) ;
#88678 = CARTESIAN_POINT ( 'NONE',  ( -5.032047568966410367, 9.022472597102808578, 1.214306433183764966E-14 ) ) ;
#88679 = CARTESIAN_POINT ( 'NONE',  ( 1.364683531249988535, 5.467708333674750953, -0.7879004041258300672 ) ) ;
#88680 = CARTESIAN_POINT ( 'NONE',  ( 6.385878362533466301, 6.816559200039058020, 0.5486352003098924346 ) ) ;
#88681 = CARTESIAN_POINT ( 'NONE',  ( -1.500000000000008216, 13.99999999999999822, 3.469446951953614189E-15 ) ) ;
#88682 = CARTESIAN_POINT ( 'NONE',  ( 4.245111494854632461, 7.966730820723463502, 0.000000000000000000 ) ) ;
#88683 = CARTESIAN_POINT ( 'NONE',  ( 5.290226454957744018, -1.756441682966399132, -0.2160651130965525468 ) ) ;
#88684 = CARTESIAN_POINT ( 'NONE',  ( 7.801827329660018684, 11.18955008699033726, 1.199719254218460707 ) ) ;
#88685 = CARTESIAN_POINT ( 'NONE',  ( 2.133940825901488481, -1.375048162780323935, -1.595187971101755364 ) ) ;
#88687 = CARTESIAN_POINT ( 'NONE',  ( -1.499999999999997780, 2.400000000000020339, 1.214306433183764966E-14 ) ) ;
#88686 = CARTESIAN_POINT ( 'NONE',  ( -8.012344526598182026E-15, 10.54687500034139624, -1.575800808251669460 ) ) ;
#88688 = CARTESIAN_POINT ( 'NONE',  ( 1.258185455790395979, -1.969739565659900160, -0.003359478883382254876 ) ) ;
#88689 = CARTESIAN_POINT ( 'NONE',  ( -2.810282979782591006, 6.500690253046801814, 0.000000000000000000 ) ) ;
#88690 = CYLINDRICAL_SURFACE ( 'NONE', #177635, 1.250000000000000000 ) ;
#88692 = ORIENTED_EDGE ( 'NONE', *, *, #40961, .F. ) ;
#88691 = CARTESIAN_POINT ( 'NONE',  ( 5.554893708145399067, 0.3617622393776204204, 1.774916939089685730 ) ) ;
#88693 = CARTESIAN_POINT ( 'NONE',  ( 5.504247177468168495, 9.365446107114122398, 0.7216878364870438212 ) ) ;
#88694 = EDGE_CURVE ( 'NONE', #131029, #48008, #115961, .T. ) ;
#88695 = CARTESIAN_POINT ( 'NONE',  ( 0.000000000000000000, 3.480000000000000426, -2.000000000000000000 ) ) ;
#88697 = CARTESIAN_POINT ( 'NONE',  ( 4.311305935566238645, -0.3199438451688824125, 1.842931056080451935 ) ) ;
#88696 = PRESENTATION_LAYER_ASSIGNMENT (  '', '', ( #168158 ) ) ;
#88698 = CARTESIAN_POINT ( 'NONE',  ( 5.172746982222708567, 1.431596967658786745, -1.495705434250683918 ) ) ;
#88699 = CARTESIAN_POINT ( 'NONE',  ( 1.224999999999979661, 1.624999999999987566, -3.989863994746656317E-14 ) ) ;
#88700 = CARTESIAN_POINT ( 'NONE',  ( -4.787437638956927977, 7.639075441208117212, -1.082531754730549967 ) ) ;
#88701 = CARTESIAN_POINT ( 'NONE',  ( 2.912612998216587368, -0.9539908294626121554, 1.749314886574315331 ) ) ;
#88703 = CARTESIAN_POINT ( 'NONE',  ( -1.500000000000001332, -0.8499999999999757749, 0.000000000000000000 ) ) ;
#88702 = CIRCLE ( 'NONE', #189028, 4.000000000000000000 ) ;
#88704 = CARTESIAN_POINT ( 'NONE',  ( 8.450809820019639318, 8.753699632978056755, -0.7998128361456291469 ) ) ;
#88705 = CARTESIAN_POINT ( 'NONE',  ( -9.664264568442742842, 10.16939683947169115, -0.7998128361456291469 ) ) ;
#88706 = CARTESIAN_POINT ( 'NONE',  ( 5.830888582329017744, 8.960397891762626799, -1.199719254218452047 ) ) ;
#88707 = CARTESIAN_POINT ( 'NONE',  ( -1.364683531250000748, 0.2593750003414205252, 0.000000000000000000 ) ) ;
#88708 = CARTESIAN_POINT ( 'NONE',  ( 0.7499999999999885647, 0.7333333333333567072, 1.299038105676657340 ) ) ;
#88710 = CARTESIAN_POINT ( 'NONE',  ( 4.798696304233017074, 7.685897223992134819, -1.199719254218452047 ) ) ;
#88709 = CARTESIAN_POINT ( 'NONE',  ( 4.580490334204036174, 1.208584658811951762, -1.545285769342201965 ) ) ;
#88711 = CARTESIAN_POINT ( 'NONE',  ( 2.038435264984053585, 1.930122609968443204, -0.5825652091262025767 ) ) ;
#88712 = EDGE_CURVE ( 'NONE', #61752, #44, #47888, .T. ) ;
#88713 = DIRECTION ( 'NONE',  ( -0.2460297208025352678, 6.661338147750954034E-16, 0.9692622846690294169 ) ) ;
#88714 = CARTESIAN_POINT ( 'NONE',  ( 0.3280006606478855224, 1.121390616443746602, -1.882787531365101685 ) ) ;
#88715 = CARTESIAN_POINT ( 'NONE',  ( -11.91826848676304884, 10.09166292761251071, 1.400000051402189971 ) ) ;
#88716 = CARTESIAN_POINT ( 'NONE',  ( 1.967826412060974084, 0.9573937279930484490, 1.606809688844474726 ) ) ;
#88717 = CARTESIAN_POINT ( 'NONE',  ( 0.6823417656249899377, 4.676041667008086655, -1.181850606188754593 ) ) ;
#88718 = CARTESIAN_POINT ( 'NONE',  ( 4.623295736497193609, 1.753618999902604614, 0.9886709913553303197 ) ) ;
#88719 = CARTESIAN_POINT ( 'NONE',  ( -6.835281999583978418, 11.12624609948998966, -0.7998128361456291469 ) ) ;
#88721 = CARTESIAN_POINT ( 'NONE',  ( 3.269268187362909028, 1.912946029434154038, -0.9076713616091285353 ) ) ;
#88720 = CARTESIAN_POINT ( 'NONE',  ( -4.284013352238250860, 7.941839977679187257, -0.7216878364870267237 ) ) ;
#88722 = MANIFOLD_SOLID_BREP ( 'Fillet1', #136432 ) ;
#88723 =( NAMED_UNIT ( * ) PLANE_ANGLE_UNIT ( ) SI_UNIT ( $, .RADIAN. ) );
#88724 = CARTESIAN_POINT ( 'NONE',  ( 5.160626937512653001, -0.6942339714755951796, -1.950645400549338104 ) ) ;
#88726 = CARTESIAN_POINT ( 'NONE',  ( 6.720655732516679137, 3.688991442244013097, 2.587785764416630219 ) ) ;
#88725 = CARTESIAN_POINT ( 'NONE',  ( 1.540690653510309538, -1.764467595836321401, 1.121255944808132288 ) ) ;
#88728 = ORIENTED_EDGE ( 'NONE', *, *, #192353, .T. ) ;
#88727 = CARTESIAN_POINT ( 'NONE',  ( 6.405291383686446238, 1.519602032305459538, 1.011395407323860907 ) ) ;
#88729 = CARTESIAN_POINT ( 'NONE',  ( 8.437251666405968464, 8.737881787095446384, 1.040834085586084257E-14 ) ) ;
#88730 = CARTESIAN_POINT ( 'NONE',  ( 0.005207752244010266374, 14.55743561439478739, 11.94812378735272240 ) ) ;
#88731 = FILL_AREA_STYLE_COLOUR ( '', #127669 ) ;
#88732 = CARTESIAN_POINT ( 'NONE',  ( -9.470186914265017464, 4.005096909781187264, 6.837150237413082365 ) ) ;
#88733 = CARTESIAN_POINT ( 'NONE',  ( 6.114364089638775646, 10.07724917131317355, 0.7216878364870438212 ) ) ;
#88734 = CARTESIAN_POINT ( 'NONE',  ( -1.364683531250000748, 12.67187500034139980, 0.000000000000000000 ) ) ;
#88735 = CARTESIAN_POINT ( 'NONE',  ( 5.936178161767468708, -1.066166440211462563, -1.587280745415058814 ) ) ;
#88736 = CARTESIAN_POINT ( 'NONE',  ( -7.049349804101573191, 10.31165964050546258, -1.199719254218440723 ) ) ;
#88737 = CARTESIAN_POINT ( 'NONE',  ( 5.789495288235341874, 6.713164910151406595, 1.199719254218462483 ) ) ;
#88738 = FACE_OUTER_BOUND ( 'NONE', #192755, .T. ) ;
#88739 = CARTESIAN_POINT ( 'NONE',  ( -0.7500000000000179856, 12.32291666734946389, 1.299038105676658228 ) ) ;
#88740 = CARTESIAN_POINT ( 'NONE',  ( 4.196412238629597447, 4.854568018944682706, -1.199719254218452047 ) ) ;
#88741 = ORIENTED_EDGE ( 'NONE', *, *, #4565, .F. ) ;
#88742 = AXIS2_PLACEMENT_3D ( 'NONE', #84324, #1978, #22503 ) ;
#88743 = CARTESIAN_POINT ( 'NONE',  ( 5.782827418265350516, 1.646828846085298448, -1.163285542026312847 ) ) ;
#88744 = CARTESIAN_POINT ( 'NONE',  ( -0.02259406399240069044, -1.896172633340575064, -0.9493637518730789759 ) ) ;
#88745 = LINE ( 'NONE', #72460, #33078 ) ;
#88746 = CARTESIAN_POINT ( 'NONE',  ( -1.499999999999961364, 8.500000000000000000, 10.64483442802188762 ) ) ;
#88747 = CARTESIAN_POINT ( 'NONE',  ( -4.853455804012230423, 6.685451076146141425, 1.443375672974064550 ) ) ;
#88748 = CARTESIAN_POINT ( 'NONE',  ( 2.198393463710220264, 5.716542807637226886, 0.7998128361456462443 ) ) ;
#88749 = CARTESIAN_POINT ( 'NONE',  ( 3.608217298448283206, 1.969629311412910866, 0.004557946788486669405 ) ) ;
#88750 = CARTESIAN_POINT ( 'NONE',  ( 4.077750037130567939, -0.7691059624741981571, 1.864175985064358665 ) ) ;
#88751 = CARTESIAN_POINT ( 'NONE',  ( -7.854251061018346469, 8.057714414143200443, -0.7998128361456291469 ) ) ;
#88752 = CARTESIAN_POINT ( 'NONE',  ( 6.727182134110178069, 2.947419669445831669, 2.641212418657997496 ) ) ;
#88753 = CIRCLE ( 'NONE', #102505, 11.00000000000000000 ) ;
#88754 = CARTESIAN_POINT ( 'NONE',  ( 4.681673494351117348, -1.034495392153191418, 1.931897795048514554 ) ) ;
#88755 = CARTESIAN_POINT ( 'NONE',  ( 5.398914348987510436, 6.259949555863199677, -2.500000000000000444 ) ) ;
#88756 = CARTESIAN_POINT ( 'NONE',  ( 2.784106279807782247, -0.9919383200396988398, 1.651252367177785230 ) ) ;
#88757 = CARTESIAN_POINT ( 'NONE',  ( -6.509886312855995172, 10.74661779830734254, -0.7998128361456291469 ) ) ;
#88758 = CARTESIAN_POINT ( 'NONE',  ( -0.02988540731099428513, 6.948706544289728448, -2.321349141872154132 ) ) ;
#88759 = CARTESIAN_POINT ( 'NONE',  ( 0.1005910224048736229, -2.206496634663042133, -0.04943112074598519229 ) ) ;
#88760 = DIRECTION ( 'NONE',  ( 0.000000000000000000, 8.546850786086437571E-32, 1.000000000000000000 ) ) ;
#88762 = EDGE_CURVE ( 'NONE', #7256, #135209, #40041, .T. ) ;
#88761 = CARTESIAN_POINT ( 'NONE',  ( -3.929058411375426108, 5.999999999999998224, 0.7499999999999988898 ) ) ;
#88763 = CARTESIAN_POINT ( 'NONE',  ( 4.202137545231717120, 6.989912005157271402, 1.199719254218462483 ) ) ;
#88764 = ORIENTED_EDGE ( 'NONE', *, *, #165266, .F. ) ;
#88765 = CARTESIAN_POINT ( 'NONE',  ( 3.770576118376296471, 7.413106214832098750, 0.7216878364870257245 ) ) ;
#88767 = CARTESIAN_POINT ( 'NONE',  ( 3.070950286465543577, -1.523008450377001832, 1.316504112208529920 ) ) ;
#88766 = CARTESIAN_POINT ( 'NONE',  ( -0.09434409087969403140, -0.8304652339055562660, -1.753633067539569490 ) ) ;
#88768 = CARTESIAN_POINT ( 'NONE',  ( 5.220190998831037987, -1.937735447606624639, -1.235822935930783517 ) ) ;
#88770 = CARTESIAN_POINT ( 'NONE',  ( 3.449909520549806707, -0.7582208578979282576, 1.699682486939468440 ) ) ;
#88769 = CARTESIAN_POINT ( 'NONE',  ( 10.50000000000000178, 10.19999999999999929, -3.600000000000000977 ) ) ;
#88771 = CARTESIAN_POINT ( 'NONE',  ( 3.285556943750000070, -0.2843749995220419269, 0.000000000000000000 ) ) ;
#88772 = CARTESIAN_POINT ( 'NONE',  ( -10.14529669463614070, -6.681160345275602985, 1.138412281109779656E-15 ) ) ;
#88773 = CARTESIAN_POINT ( 'NONE',  ( 6.258066496116281741, 0.7254575739856858885, -1.769658340881982816 ) ) ;
#88774 = CARTESIAN_POINT ( 'NONE',  ( -7.043624497499477499, 8.176315654292865887, 1.199719254218450271 ) ) ;
#88775 = CARTESIAN_POINT ( 'NONE',  ( -4.258669648468323743, 6.061810238003387141, 1.443375672974065660 ) ) ;
#88776 = CARTESIAN_POINT ( 'NONE',  ( 5.847236579984706140, 0.6061975457797988964, -2.000951093856804253 ) ) ;
#88777 = CARTESIAN_POINT ( 'NONE',  ( 4.338245966692901412, 8.005111361209628740, -0.7216878364870197293 ) ) ;
#88778 = ORIENTED_EDGE ( 'NONE', *, *, #64050, .F. ) ;
#88779 = CARTESIAN_POINT ( 'NONE',  ( 9.499606442108964544, 7.849261790823902629, -0.08647222121513191417 ) ) ;
#88780 = LINE ( 'NONE', #75713, #20147 ) ;
#88781 = CARTESIAN_POINT ( 'NONE',  ( 0.06470675514189982991, -1.629034059718449834, -0.8243793580787887043 ) ) ;
#88782 = CARTESIAN_POINT ( 'NONE',  ( -3.750802052474980108, 7.527686161196117887, 1.040834085586084257E-14 ) ) ;
#88783 = CARTESIAN_POINT ( 'NONE',  ( 2.988574679986736093, -1.732066829584472556, 0.08781845822969887305 ) ) ;
#88784 = CARTESIAN_POINT ( 'NONE',  ( 0.3282377607281127818, 1.886164550367421588, 1.224999999999948352 ) ) ;
#88785 = CARTESIAN_POINT ( 'NONE',  ( 6.183927461164522299, 6.387205924212962849, 0.000000000000000000 ) ) ;
#88786 = CARTESIAN_POINT ( 'NONE',  ( -7.054319997812058318, 7.124461507069184130, 1.040834085586084257E-14 ) ) ;
#88787 = CARTESIAN_POINT ( 'NONE',  ( -11.86145016429273014, 10.90000000000000036, 1.179999999999997051 ) ) ;
#88788 = CARTESIAN_POINT ( 'NONE',  ( 0.5146170122050791607, 0.7890519337857507809, 1.914186188738425942 ) ) ;
#88789 = CARTESIAN_POINT ( 'NONE',  ( 5.426323838365306074, 1.084245000580752238, -1.468710674947353967 ) ) ;
#88790 = CARTESIAN_POINT ( 'NONE',  ( 3.168751141962049989, 1.424179589570490512, -1.349414796185027576 ) ) ;
#88791 = CARTESIAN_POINT ( 'NONE',  ( -1.225000000000028066, -0.9583333326505286687, -0.7072540797572817173 ) ) ;
#88792 = CARTESIAN_POINT ( 'NONE',  ( -8.371269781434001800, 11.85389961405997816, -1.199719254218446718 ) ) ;
#88793 = CARTESIAN_POINT ( 'NONE',  ( 5.777746017718023097, 9.892454120646377191, 0.7998128361456462443 ) ) ;
#88794 = CARTESIAN_POINT ( 'NONE',  ( 4.002672028760116518, -2.097606743168555443, -0.3097674545872729501 ) ) ;
#88795 = CARTESIAN_POINT ( 'NONE',  ( -4.297571505851936813, 4.116180966356429494, 1.214306433183764966E-14 ) ) ;
#88796 = CARTESIAN_POINT ( 'NONE',  ( -9.297140650669053485, 11.86975006391249643, 1.599625672291281386 ) ) ;
#88797 = CARTESIAN_POINT ( 'NONE',  ( 2.008725816923035978, 0.6454906730102347723, 1.967154155859623055 ) ) ;
#88799 = CARTESIAN_POINT ( 'NONE',  ( -1.500000000000008216, 15.28125000068279782, 3.469446951953614189E-15 ) ) ;
#88798 = CARTESIAN_POINT ( 'NONE',  ( 6.827182134110199030, 7.629137130509070275, 2.410944104600701188 ) ) ;
#88801 = ORIENTED_EDGE ( 'NONE', *, *, #11908, .T. ) ;
#88800 = CARTESIAN_POINT ( 'NONE',  ( 4.213700991847090016, 1.784230803775087137, 1.322971166850190450 ) ) ;
#88802 = CARTESIAN_POINT ( 'NONE',  ( 2.127932615311285414, 0.5078372532463393263, 2.241765503411979221 ) ) ;
#88804 = CARTESIAN_POINT ( 'NONE',  ( 6.578975509608026684, 1.922407110116808981, 0.7477742492353837145 ) ) ;
#88803 = CARTESIAN_POINT ( 'NONE',  ( 10.08690309888728187, 10.87040115823107911, -0.7216878364870257245 ) ) ;
#88806 = CARTESIAN_POINT ( 'NONE',  ( -3.474999999999998312, -1.020833333333332815, 2.006292185433951047 ) ) ;
#88805 = CARTESIAN_POINT ( 'NONE',  ( 7.024532985656128936, 9.288650798055913427, 1.443375672974065660 ) ) ;
#88807 = EDGE_CURVE ( 'NONE', #206426, #113379, #178435, .T. ) ;
#88808 = DIRECTION ( 'NONE',  ( 1.276756478318932585E-15, -1.000000000000000000, 1.665334536937738262E-16 ) ) ;
#88809 = CARTESIAN_POINT ( 'NONE',  ( 6.304252605626877504, 1.359535501544101077, -1.241908024382516240 ) ) ;
#88810 = DIRECTION ( 'NONE',  ( 0.000000000000000000, -1.000000000000000000, 0.000000000000000000 ) ) ;
#88811 = CARTESIAN_POINT ( 'NONE',  ( 3.252119977711815491, 0.8557668478980616777, -1.710280963351323846 ) ) ;
#88812 = CARTESIAN_POINT ( 'NONE',  ( -0.1106727585416019261, 7.629137130509112907, -2.603481208547548054 ) ) ;
#88813 = CARTESIAN_POINT ( 'NONE',  ( 4.330854930063167352, 0.08572247821646634958, 1.722753318990229099 ) ) ;
#88814 = CARTESIAN_POINT ( 'NONE',  ( 2.870327622459168726, -1.987497926849005836, -0.3399570244180456502 ) ) ;
#88815 = ADVANCED_FACE ( 'NONE', ( #119156 ), #102852, .T. ) ;
#88816 = CARTESIAN_POINT ( 'NONE',  ( 3.604340556743702795, -0.1682163741436558391, 2.292568252494499692 ) ) ;
#88817 = CARTESIAN_POINT ( 'NONE',  ( 3.901889172025752472, -0.6612649319669267056, 2.163591406342895596 ) ) ;
#88818 = CARTESIAN_POINT ( 'NONE',  ( 6.727182134110234024, -0.002100931800118072384, 2.089081857379895268 ) ) ;
#88819 = CARTESIAN_POINT ( 'NONE',  ( -6.455090533882213322, 6.703562842383589349, -0.7216878364870338292 ) ) ;
#88820 = VERTEX_POINT ( 'NONE', #37846 ) ;
#88821 = CARTESIAN_POINT ( 'NONE',  ( 4.868267778354250730, -1.156333057219432581, 1.339767963349105528 ) ) ;
#88822 = AXIS2_PLACEMENT_3D ( 'NONE', #14359, #63133, #175831 ) ;
#88823 = EDGE_CURVE ( 'NONE', #96482, #71979, #104998, .T. ) ;
#88825 = CARTESIAN_POINT ( 'NONE',  ( 0.7270408775228944798, 0.1741418271693234987, 2.285704298519490862 ) ) ;
#88824 = CARTESIAN_POINT ( 'NONE',  ( 8.039058738260216330, 8.343599714250547805, -0.7998128361456341429 ) ) ;
#88826 = CARTESIAN_POINT ( 'NONE',  ( 5.841722611436679813, 1.839261846420519930, 0.08593139445873398952 ) ) ;
#88827 = CARTESIAN_POINT ( 'NONE',  ( -2.598358995313378550, 6.183169261174235487, 0.7998128361456341429 ) ) ;
#88828 = CARTESIAN_POINT ( 'NONE',  ( 6.035146784841348477, -1.584849238314169240, -1.513754250258770639 ) ) ;
#88829 = CARTESIAN_POINT ( 'NONE',  ( -3.820365424000704557, 7.679119771301277098, -0.7998128361456481317 ) ) ;
#88830 = CARTESIAN_POINT ( 'NONE',  ( -3.623053363349869382, 5.249981562040033189, 1.599625672291267398 ) ) ;
#88831 = CARTESIAN_POINT ( 'NONE',  ( -0.8448260811288544891, 15.46906395968185244, 12.00404981830694240 ) ) ;
#88832 = CARTESIAN_POINT ( 'NONE',  ( 6.303194806757332458, -1.751150776259063457, 1.104182018118210262 ) ) ;
#88833 = CARTESIAN_POINT ( 'NONE',  ( 0.07540816263147330500, 1.497505997221737273, 1.350731191893522976 ) ) ;
#88834 = CARTESIAN_POINT ( 'NONE',  ( -0.6823417656249969321, 5.467708333674756283, -1.181850606188749264 ) ) ;
#88835 = CARTESIAN_POINT ( 'NONE',  ( 3.773980605468800320, 1.071039916736727937, 1.601146377209327731 ) ) ;
#88836 = CARTESIAN_POINT ( 'NONE',  ( -1.364683531250010295, 10.13020833367472839, 0.7879004041258445001 ) ) ;
#88837 = CARTESIAN_POINT ( 'NONE',  ( 1.336510806674645391, -1.239524924825789132, -1.843257696707498061 ) ) ;
#88839 = ORIENTED_EDGE ( 'NONE', *, *, #45284, .F. ) ;
#88838 = CARTESIAN_POINT ( 'NONE',  ( -0.7500000000000006661, 13.23958333401613352, -1.299038105676657340 ) ) ;
#88841 = DIRECTION ( 'NONE',  ( 0.000000000000000000, 0.000000000000000000, -1.000000000000000000 ) ) ;
#88840 = FACE_BOUND ( 'NONE', #76603, .T. ) ;
#88842 = CARTESIAN_POINT ( 'NONE',  ( 2.381428537494710618, 5.930083727052461562, 0.7998128361456462443 ) ) ;
#88843 = CARTESIAN_POINT ( 'NONE',  ( -2.788906526875773208E-15, 8.968750000682797818, -1.499999999999998446 ) ) ;
#88844 = CARTESIAN_POINT ( 'NONE',  ( 11.92619526913699879, 10.90000000000000036, -1.328859060402686199 ) ) ;
#88845 = CARTESIAN_POINT ( 'NONE',  ( 9.905435134813219022, 11.51422724318055835, -6.695335200864244385 ) ) ;
#88846 = CARTESIAN_POINT ( 'NONE',  ( 8.215877899756996783, 12.52901528311778989, 1.040834085586084257E-14 ) ) ;
#88847 = CARTESIAN_POINT ( 'NONE',  ( 2.418345249890076154, 0.8361516037145629854, 1.774881043358336630 ) ) ;
#88849 = CARTESIAN_POINT ( 'NONE',  ( -1.364683531249997417, 2.571875000341422357, 1.214306433183764966E-14 ) ) ;
#88848 = CARTESIAN_POINT ( 'NONE',  ( 6.634017235788401301, 6.634108284708264414, 0.7998128361456341429 ) ) ;
#88850 = CARTESIAN_POINT ( 'NONE',  ( 11.92619526913699879, 12.69999999999998153, 1.328859060402684644 ) ) ;
#88851 = CIRCLE ( 'NONE', #92276, 0.07999999999999943268 ) ;
#88852 = CARTESIAN_POINT ( 'NONE',  ( 6.443807124430430910, 1.351966286592180211, 1.421895456074427688 ) ) ;
#88853 = CARTESIAN_POINT ( 'NONE',  ( -9.318531651294266638, 9.766041769465124034, -0.7998128361456291469 ) ) ;
#88854 = EDGE_CURVE ( 'NONE', #81797, #68330, #107380, .T. ) ;
#88855 = CARTESIAN_POINT ( 'NONE',  ( -3.917943204224913156, 7.514758138330285497, -0.7216878364870257245 ) ) ;
#88856 = CARTESIAN_POINT ( 'NONE',  ( 0.4271420986578051138, 2.166143833277152542, 0.6532491227348672380 ) ) ;
#88858 = ORIENTED_EDGE ( 'NONE', *, *, #141701, .T. ) ;
#88857 = CARTESIAN_POINT ( 'NONE',  ( -5.961834861707238531, 7.978559976790334574, -1.599625672291263179 ) ) ;
#88859 = CARTESIAN_POINT ( 'NONE',  ( 1.364683531249990311, 5.363541667008086655, 0.7879004041258500513 ) ) ;
#88860 = CARTESIAN_POINT ( 'NONE',  ( 1.440467042440606749, 0.3595057747620767907, 1.835501880432292010 ) ) ;
#88861 = CARTESIAN_POINT ( 'NONE',  ( 0.2109833617158912156, 1.658496975328831891, 0.5066527762955413960 ) ) ;
#88863 = CARTESIAN_POINT ( 'NONE',  ( 4.318054327947466575, 1.347776305887092185, -1.728067674571641898 ) ) ;
#88862 = CARTESIAN_POINT ( 'NONE',  ( -1.360316468750062846, 1.619791667008073643, -0.7853790794159301036 ) ) ;
#88864 = CARTESIAN_POINT ( 'NONE',  ( 5.245303717312764569, -1.982421492789496753, 1.180877550764187545 ) ) ;
#88865 = CARTESIAN_POINT ( 'NONE',  ( 0.3388364525104338165, 0.3516977924403408284, 2.030485180972623205 ) ) ;
#88866 = CARTESIAN_POINT ( 'NONE',  ( 2.607286591753724014, -1.920749920159558810, 0.2854125566163211447 ) ) ;
#88867 = CARTESIAN_POINT ( 'NONE',  ( -5.883875478206491927, 5.966868934103426447, 0.000000000000000000 ) ) ;
#88868 = FILL_AREA_STYLE ('',( #22750 ) ) ;
#88869 = CARTESIAN_POINT ( 'NONE',  ( 4.800995793014950941, 5.734154859006458160, -1.082531754730548412 ) ) ;
#88870 = CARTESIAN_POINT ( 'NONE',  ( 1.224999999999995204, 2.875000000000002665, 0.000000000000000000 ) ) ;
#88871 = CARTESIAN_POINT ( 'NONE',  ( 3.551407868487792552, -1.352154898762620849, 1.496051317864899088 ) ) ;
#88872 = CARTESIAN_POINT ( 'NONE',  ( -3.565431210269599749, 7.103494145382415859, 0.7216878364870317197 ) ) ;
#88873 = CARTESIAN_POINT ( 'NONE',  ( -5.986807348886189040, 9.142303119412650503, -1.199719254218452047 ) ) ;
#88874 = CARTESIAN_POINT ( 'NONE',  ( 0.4170821662628897974, 3.033599471985628959, -0.4170821662629418114 ) ) ;
#88876 = CARTESIAN_POINT ( 'NONE',  ( 7.784592198500480897, -5.601927612791806510, -7.772296586883602920 ) ) ;
#88875 = CARTESIAN_POINT ( 'NONE',  ( 0.6096330727367264002, -1.817201089070449971, 0.1759225495863714350 ) ) ;
#88877 = CARTESIAN_POINT ( 'NONE',  ( -6.947627372360122955, 7.070263120700404968, 0.000000000000000000 ) ) ;
#88878 = CARTESIAN_POINT ( 'NONE',  ( 11.41010744128096555, 2.630042260599927850, -3.716153451272507180 ) ) ;
#88879 = CARTESIAN_POINT ( 'NONE',  ( -10.71692179555930302, 5.308633586712264041, 6.728550107195007790 ) ) ;
#88880 = ORIENTED_EDGE ( 'NONE', *, *, #167387, .F. ) ;
#88881 = CARTESIAN_POINT ( 'NONE',  ( 5.647358743468454456, -1.623080139260910437, -1.269863021155111849 ) ) ;
#88882 = CARTESIAN_POINT ( 'NONE',  ( -6.360183458142173230, 9.473945563590925545, 1.082531754730549967 ) ) ;
#88883 = CARTESIAN_POINT ( 'NONE',  ( 7.960045584554727327, 8.459343734834927631, 0.7216878364870267237 ) ) ;
#88884 = CARTESIAN_POINT ( 'NONE',  ( -5.251085567194491155, 5.020688004682002159, -0.7998128361456221525 ) ) ;
#88885 = CARTESIAN_POINT ( 'NONE',  ( -9.297140650669053485, 11.86975006391249643, 1.599625672291281386 ) ) ;
#88886 = CARTESIAN_POINT ( 'NONE',  ( 5.918619479961092722, -0.7289874232782632690, -1.883701229315833059 ) ) ;
#88888 = ORIENTED_EDGE ( 'NONE', *, *, #71139, .F. ) ;
#88887 = CARTESIAN_POINT ( 'NONE',  ( 5.707756388377941192, 1.680692789272177468, 1.452518960167401341 ) ) ;
#88889 = CARTESIAN_POINT ( 'NONE',  ( -5.340986169140711226, 5.195848383611072485, 0.000000000000000000 ) ) ;
#88890 = CARTESIAN_POINT ( 'NONE',  ( 4.659198344590585350, 8.587481835331020719, 0.7998128361456462443 ) ) ;
#88891 = CARTESIAN_POINT ( 'NONE',  ( 5.840714686760185792, 0.3996242267790580116, 2.021590886677153254 ) ) ;
#88892 = CARTESIAN_POINT ( 'NONE',  ( 4.307267641921147749, 1.238321930042911578, -1.591317616567271775 ) ) ;
#88893 = VERTEX_POINT ( 'NONE', #137497 ) ;
#88894 = CARTESIAN_POINT ( 'NONE',  ( -1.877679919396925134, 2.480539018720154143, 2.466641060286964837 ) ) ;
#88895 = VECTOR ( 'NONE', #148134, 1000.000000000000000 ) ;
#88897 = ORIENTED_EDGE ( 'NONE', *, *, #4984, .F. ) ;
#88896 = CARTESIAN_POINT ( 'NONE',  ( -6.526270840131767059, 8.707344961610770540, -1.599625672291271394 ) ) ;
#88898 = CARTESIAN_POINT ( 'NONE',  ( 4.669458948634179762, 8.398658883068243597, -0.5498995856093937817 ) ) ;
#88899 = CARTESIAN_POINT ( 'NONE',  ( 3.936874915731437774, 1.117662071392529377, 1.677747830363854664 ) ) ;
#88900 = CARTESIAN_POINT ( 'NONE',  ( 3.697050842446505392, -0.5329721798031424873, 1.762307204009383454 ) ) ;
#88901 = FACE_OUTER_BOUND ( 'NONE', #92384, .T. ) ;
#88902 = CARTESIAN_POINT ( 'NONE',  ( 2.385774557197326562, 2.109090111016972191, -0.9369807928535575092 ) ) ;
#88903 = CARTESIAN_POINT ( 'NONE',  ( 5.246079093845007257, 5.085123462432798114, 0.7998128361456352531 ) ) ;
#88904 = CARTESIAN_POINT ( 'NONE',  ( 3.427187520701843404, 0.04928524951339217919, 2.161187641841005647 ) ) ;
#88906 = CARTESIAN_POINT ( 'NONE',  ( 7.259501185113382604, 10.55683625168592243, -1.199719254218441611 ) ) ;
#88905 = CARTESIAN_POINT ( 'NONE',  ( 3.327361509216096191, -1.530157842762596143, -1.313544516083162028 ) ) ;
#88907 = CARTESIAN_POINT ( 'NONE',  ( -3.750802052474980108, 7.527686161196117887, 1.040834085586084257E-14 ) ) ;
#88908 = CARTESIAN_POINT ( 'NONE',  ( 3.655889646864494580, -0.4445778678274399098, -2.254845314064676032 ) ) ;
#88909 = PLANE ( 'NONE',  #139118 ) ;
#88910 = CARTESIAN_POINT ( 'NONE',  ( 2.518242125168220102, 1.223528130051700025, -1.415109699333151561 ) ) ;
#88911 = CARTESIAN_POINT ( 'NONE',  ( 6.350460794227542394, 0.6179267841925452087, 1.872200446973372179 ) ) ;
#88913 = CARTESIAN_POINT ( 'NONE',  ( -7.774674742793745708, 8.035151719539642912, 0.7998128361456341429 ) ) ;
#88912 = CARTESIAN_POINT ( 'NONE',  ( -1.001543065824772872E-14, 4.321875000341417916, 1.575800808251672791 ) ) ;
#88915 = CARTESIAN_POINT ( 'NONE',  ( 1.454063653991678473, 0.6380318336138122159, -2.112638918738508398 ) ) ;
#88914 = CARTESIAN_POINT ( 'NONE',  ( -4.252453736180621391, 8.112946458852704268, -0.7998128361456281477 ) ) ;
#88916 = CARTESIAN_POINT ( 'NONE',  ( 2.947061413272269004, 6.452339058877361921, 0.1880404715405617766 ) ) ;
#88917 = CARTESIAN_POINT ( 'NONE',  ( 3.832150974156964818, 7.622593236491780999, 1.040834085586084257E-14 ) ) ;
#88918 = CARTESIAN_POINT ( 'NONE',  ( -5.922214171070950606, 5.803671375871217286, -0.7998128361456291469 ) ) ;
#88919 = AXIS2_PLACEMENT_3D ( 'NONE', #205200, #188966, #92577 ) ;
#88920 = CARTESIAN_POINT ( 'NONE',  ( 2.959812437696838661, 6.450877987504894051, 0.3496188560969323289 ) ) ;
#88921 = CARTESIAN_POINT ( 'NONE',  ( 6.157099186568592231, -1.690597638883487797, -1.013973547023840460 ) ) ;
#88922 = CARTESIAN_POINT ( 'NONE',  ( 5.303480822065511191, 1.883932040028640786, 1.332532017187069817 ) ) ;
#88923 = CARTESIAN_POINT ( 'NONE',  ( 0.7484013653801385724, -1.946605496936428370, -0.2438083268051088881 ) ) ;
#88924 = CARTESIAN_POINT ( 'NONE',  ( 2.782143433959896051, -1.183836405090990640, -1.688839807681275174 ) ) ;
#88925 = CARTESIAN_POINT ( 'NONE',  ( 6.860062538834778678, 8.066123052471139587, -1.082531754730543083 ) ) ;
#88926 = CARTESIAN_POINT ( 'NONE',  ( 4.085803189671889157, 5.860132702740892263, -1.599625672291273171 ) ) ;
#88927 = CARTESIAN_POINT ( 'NONE',  ( 6.100805936025112786, 10.06143132543056673, 1.040834085586084257E-14 ) ) ;
#88928 = CARTESIAN_POINT ( 'NONE',  ( 1.364683531249988535, 3.217708333674748289, -0.7879004041258239610 ) ) ;
#88929 = CARTESIAN_POINT ( 'NONE',  ( 5.355107487273504496, 6.310342158982962246, -1.082531754730543083 ) ) ;
#88930 = CARTESIAN_POINT ( 'NONE',  ( 0.3214382364499007161, -1.938747691508705184, -0.9774007134471692781 ) ) ;
#88931 = CARTESIAN_POINT ( 'NONE',  ( 11.89942855770813956, 12.22000000000000064, -0.7000000000000009548 ) ) ;
#88933 = CARTESIAN_POINT ( 'NONE',  ( 4.669393045487420402, 1.064170941109745305, 1.502380130741477693 ) ) ;
#88932 = DIRECTION ( 'NONE',  ( -0.7806247497998004548, 0.000000000000000000, 0.6249999999999992228 ) ) ;
#88934 = B_SPLINE_CURVE_WITH_KNOTS ( 'NONE', 3,
 ( #53533, #24211, #138000, #89258, #69758, #22062, #122907, #57805, #156385, #121821 ),
 .UNSPECIFIED., .F., .F.,
 ( 4, 2, 2, 2, 4 ),
 ( 0.000000000000000000, 0.0002299353307164155296, 0.0004598706614328310592, 0.0006898059921492465888, 0.0009197413228656621184 ),
 .UNSPECIFIED. ) ;
#88935 = CARTESIAN_POINT ( 'NONE',  ( 6.620655732516620873, 0.004685112605665174221, 1.926407831898164558 ) ) ;
#88936 = CARTESIAN_POINT ( 'NONE',  ( 6.620655732516649294, -0.005281389526671945688, 2.273887028200880511 ) ) ;
#88937 = CARTESIAN_POINT ( 'NONE',  ( -11.92619526913699879, 10.19999999999998153, 1.328859060402684644 ) ) ;
#88938 = CARTESIAN_POINT ( 'NONE',  ( 0.9137757228094539608, -0.3311857980235459742, 2.237941903941061739 ) ) ;
#88939 = CARTESIAN_POINT ( 'NONE',  ( -5.408724846006345288, 6.482216231307839749, 1.333832282565196925 ) ) ;
#88940 = CARTESIAN_POINT ( 'NONE',  ( 1.500000000000007105, 10.64264068711930733, 1.214306433183764966E-14 ) ) ;
#88941 = CARTESIAN_POINT ( 'NONE',  ( 6.104935607482663507, 7.108274908414393245, 1.121150977946131722 ) ) ;
#88942 = CARTESIAN_POINT ( 'NONE',  ( 0.02974158317493520720, -1.875378228685410376, 0.3729384364157954379 ) ) ;
#88943 = CARTESIAN_POINT ( 'NONE',  ( 1.533702468213002712, 0.8761213712049474855, -1.537698828099523629 ) ) ;
#88944 = CARTESIAN_POINT ( 'NONE',  ( 6.481113961022470171, -1.841437297342415791, -0.8137991234780891370 ) ) ;
#88946 = CARTESIAN_POINT ( 'NONE',  ( 3.374530662324583652, -0.3768237823980990497, -1.877989258545700535 ) ) ;
#88945 = CARTESIAN_POINT ( 'NONE',  ( -9.480175724453545172, 12.08329098332774265, 1.599625672291281386 ) ) ;
#88947 = CARTESIAN_POINT ( 'NONE',  ( -5.600330155773479035, 5.743136491903856999, -0.2604917703057018641 ) ) ;
#88948 = CARTESIAN_POINT ( 'NONE',  ( 4.809023018811155126, -1.583041700261601958, 1.171600654023413624 ) ) ;
#88949 = CARTESIAN_POINT ( 'NONE',  ( 0.3344391967911933272, -1.139684030083350841, -1.788147294700337397 ) ) ;
#88950 = CARTESIAN_POINT ( 'NONE',  ( -2.785310492603665367, 5.336947110424484109, 1.199719254218462483 ) ) ;
#88951 = CARTESIAN_POINT ( 'NONE',  ( 3.080767038946086611, -0.1360980058115155988, -1.865751385159146070 ) ) ;
#88953 = ORIENTED_EDGE ( 'NONE', *, *, #201515, .T. ) ;
#88952 = CARTESIAN_POINT ( 'NONE',  ( 5.865779507164840645, 1.698138087647281358, -0.3015940010741220978 ) ) ;
#88955 = CARTESIAN_POINT ( 'NONE',  ( 4.717874267875568961, 4.606534188717351874, -0.7216878364870188411 ) ) ;
#88954 = CARTESIAN_POINT ( 'NONE',  ( 2.420803835572300500, 1.440536793087299205, -1.671967039616916617 ) ) ;
#88956 = EDGE_CURVE ( 'NONE', #107948, #75994, #6383, .T. ) ;
#88957 = CARTESIAN_POINT ( 'NONE',  ( -1.201851678989727383E-14, 3.884375000341423689, 1.575800808251672791 ) ) ;
#88958 = CARTESIAN_POINT ( 'NONE',  ( 0.9067701044400799937, 0.5968461685175918685, 1.974459182335401186 ) ) ;
#88959 = CARTESIAN_POINT ( 'NONE',  ( 6.531277313481192337, 8.642909503859968368, 1.599625672291281386 ) ) ;
#88960 = DIRECTION ( 'NONE',  ( 0.000000000000000000, 1.000000000000000000, 0.000000000000000000 ) ) ;
#88961 = FACE_OUTER_BOUND ( 'NONE', #90755, .T. ) ;
#88962 = CARTESIAN_POINT ( 'NONE',  ( 3.834746474454188013E-15, 10.34375000068279782, 1.500000000000001554 ) ) ;
#88963 = CARTESIAN_POINT ( 'NONE',  ( -15.75000000000000000, 12.30000000000000071, -3.200000000000001510 ) ) ;
#88964 = EDGE_LOOP ( 'NONE', ( #154501, #213068, #11940, #41590, #38796 ) ) ;
#88965 = CARTESIAN_POINT ( 'NONE',  ( 2.629418614236479712, 0.1040367438073786233, -2.067886086930009970 ) ) ;
#88966 = CARTESIAN_POINT ( 'NONE',  ( -0.7500000000000215383, 4.441666666666691299, 1.299038105676671107 ) ) ;
#88967 = CARTESIAN_POINT ( 'NONE',  ( 3.985207087413062066, 6.736826471035503694, -1.199719254218452047 ) ) ;
#88968 = CARTESIAN_POINT ( 'NONE',  ( -6.596192096975760144, 6.770415987340496322, 0.2575442448356154990 ) ) ;
#88969 = CARTESIAN_POINT ( 'NONE',  ( 1.260422244424246108, 2.017472913078500518, 0.09673469748067325957 ) ) ;
#88970 = CARTESIAN_POINT ( 'NONE',  ( -11.97929049433705373, 13.88000000000000078, -0.7046979865771834106 ) ) ;
#88971 = CARTESIAN_POINT ( 'NONE',  ( 1.364683531249990311, 3.884375000341417028, 1.214306433183764966E-14 ) ) ;
#88973 = CARTESIAN_POINT ( 'NONE',  ( 8.541273586929342798, 11.94827437051752206, -1.082531754730543083 ) ) ;
#88972 = CARTESIAN_POINT ( 'NONE',  ( 0.07499057489262526965, 5.723988098492513998, -2.549530206576706259 ) ) ;
#88974 = CARTESIAN_POINT ( 'NONE',  ( 4.956407584168041502, 1.492027487219639514, 1.356091576722208369 ) ) ;
#88975 = CARTESIAN_POINT ( 'NONE',  ( 5.788286065124909285, -0.6962570634414954052, -1.784894364769493924 ) ) ;
#88976 = CARTESIAN_POINT ( 'NONE',  ( -1.500000000000039524, 7.378742179571327497, -10.87908636427990139 ) ) ;
#88977 = CARTESIAN_POINT ( 'NONE',  ( 4.247736854543925133, 2.191053489037126045, -0.05455935714590579022 ) ) ;
#88979 = TOROIDAL_SURFACE ( 'NONE', #123692, 11.92000000000000171, 0.08000000000000000167 ) ;
#88978 = CARTESIAN_POINT ( 'NONE',  ( -0.7500000000000006661, 2.139583334016155636, -1.299038105676652011 ) ) ;
#88980 = CARTESIAN_POINT ( 'NONE',  ( 2.021601768330282045, -0.4154675118966509317, 1.866563793090275203 ) ) ;
#88981 = ADVANCED_BREP_SHAPE_REPRESENTATION ( '', ( #91223, #200407 ), #151904 ) ;
#88982 = CARTESIAN_POINT ( 'NONE',  ( -5.205440912643032547, 8.160432600470439723, 1.199719254218452047 ) ) ;
#88984 = CARTESIAN_POINT ( 'NONE',  ( 5.138177029454847222, 6.057256624861201644, 1.082531754730560403 ) ) ;
#88983 = B_SPLINE_CURVE_WITH_KNOTS ( 'NONE', 3,
 ( #93059, #125620, #56274, #140759, #76769, #7495, #24820 ),
 .UNSPECIFIED., .F., .F.,
 ( 4, 3, 4 ),
 ( 0.0001788552925466765887, 0.0009000000022260272806, 0.002103779968145167399 ),
 .UNSPECIFIED. ) ;
#88985 = CARTESIAN_POINT ( 'NONE',  ( 1.001577623981730891, -1.966640429010723112, 0.4445266750975271353 ) ) ;
#88986 = CARTESIAN_POINT ( 'NONE',  ( -1.364683531250000748, 11.67187500034139802, 0.000000000000000000 ) ) ;
#88988 = CARTESIAN_POINT ( 'NONE',  ( -6.642568916052639771, 6.714361588341672515, 0.000000000000000000 ) ) ;
#88987 = CARTESIAN_POINT ( 'NONE',  ( 5.899973326018037589, -0.7874313895239596350, -2.045375389432432467 ) ) ;
#88990 = ORIENTED_EDGE ( 'NONE', *, *, #30234, .T. ) ;
#88989 = CARTESIAN_POINT ( 'NONE',  ( 2.660839013829336075, -1.499436941970986759, -0.8522202921518050589 ) ) ;
#88991 = CARTESIAN_POINT ( 'NONE',  ( 6.082307721193076944, 1.091511717630256673, 1.817998432235830908 ) ) ;
#88992 = CARTESIAN_POINT ( 'NONE',  ( 7.527801604085637699, 9.805521176231838609, 1.599625672291281386 ) ) ;
#88993 = CARTESIAN_POINT ( 'NONE',  ( 3.960953433486789521, 7.772862772376584850, -0.7998128361456221525 ) ) ;
#88994 = DIRECTION ( 'NONE',  ( -1.000000000000000000, 0.000000000000000000, 0.000000000000000000 ) ) ;
#88995 = CARTESIAN_POINT ( 'NONE',  ( 0.2386218892466463737, -1.902018210125755004, -0.4804332253167050149 ) ) ;
#88996 = CARTESIAN_POINT ( 'NONE',  ( -11.84668730067608600, 12.69999999999999929, -1.400000000000001910 ) ) ;
#88997 = CARTESIAN_POINT ( 'NONE',  ( 6.331821432781979730, 7.345878745455822312, -1.199719254218445830 ) ) ;
#88998 = CARTESIAN_POINT ( 'NONE',  ( -0.7500000000000179856, 10.79166666666666430, 1.299038105676658228 ) ) ;
#88999 = EDGE_LOOP ( 'NONE', ( #208004, #12948, #48055, #11541 ) ) ;
#89000 = CARTESIAN_POINT ( 'NONE',  ( 9.498256814137546300, -6.950186805636712428, 0.04218801535506153805 ) ) ;
#89001 = ORIENTED_EDGE ( 'NONE', *, *, #201793, .F. ) ;
#89002 = CARTESIAN_POINT ( 'NONE',  ( 3.193826918316445163, 1.151326796633693084, 1.398496967315324246 ) ) ;
#89003 = ORIENTED_EDGE ( 'NONE', *, *, #213886, .T. ) ;
#89004 = CARTESIAN_POINT ( 'NONE',  ( 10.55232363013785246, 11.20546574478267132, 0.000000000000000000 ) ) ;
#89006 = EDGE_CURVE ( 'NONE', #118697, #172216, #5355, .T. ) ;
#89005 = CARTESIAN_POINT ( 'NONE',  ( 4.869313445963426190, 5.709895770826003414, 1.199719254218452935 ) ) ;
#89007 = CARTESIAN_POINT ( 'NONE',  ( 4.301270310059371660, 1.616194109774160559, -0.8183029847002845081 ) ) ;
#89008 = CARTESIAN_POINT ( 'NONE',  ( 0.4153311931459124917, 3.780327751615584653, 0.5000000000000073275 ) ) ;
#89009 = DIRECTION ( 'NONE',  ( 0.000000000000000000, -1.000000000000000000, 0.000000000000000000 ) ) ;
#89010 = CARTESIAN_POINT ( 'NONE',  ( 5.407503677813131127, 6.286683671216334091, 1.048937882774292785 ) ) ;
#89012 = CARTESIAN_POINT ( 'NONE',  ( 1.364683531249997417, 14.98437500034140157, 2.602085213965210642E-15 ) ) ;
#89011 = CARTESIAN_POINT ( 'NONE',  ( 5.353892109531869004, -0.6699537489362316078, 1.736457084658560079 ) ) ;
#89013 = CARTESIAN_POINT ( 'NONE',  ( 2.231924035814872642, 1.915248681264541508, 0.04463030589317053265 ) ) ;
#89014 = CARTESIAN_POINT ( 'NONE',  ( -10.92050379694822837, 4.688480456342538183, -4.459762147120462039 ) ) ;
#89015 = STYLED_ITEM ( 'NONE', ( #61594 ), #198182 ) ;
#89016 = CARTESIAN_POINT ( 'NONE',  ( -3.673896439623323129, 4.156855427197417185, 2.420000000000010587 ) ) ;
#89017 = CARTESIAN_POINT ( 'NONE',  ( -6.329400247113886380, 6.896658009377570231, 0.7645970852754442326 ) ) ;
#89018 = DIRECTION ( 'NONE',  ( 1.000000000000000000, 0.000000000000000000, 0.000000000000000000 ) ) ;
#89019 = CARTESIAN_POINT ( 'NONE',  ( 7.510853912290742507, 8.825379654836435606, -1.082531754730537976 ) ) ;
#89020 = B_SPLINE_CURVE_WITH_KNOTS ( 'NONE', 3,
 ( #195835, #130899, #214163, #131938, #46396, #98335, #14920, #164401 ),
 .UNSPECIFIED., .F., .F.,
 ( 4, 2, 2, 4 ),
 ( 0.0007320770841321888774, 0.0008843033762534638440, 0.001036529668374738811, 0.001340982252617288093 ),
 .UNSPECIFIED. ) ;
#89021 = CARTESIAN_POINT ( 'NONE',  ( -2.903417451620861289, 6.539070793532962611, 0.7998128361456341429 ) ) ;
#89022 = CARTESIAN_POINT ( 'NONE',  ( -9.584290747383006348, -7.189645481338096111, 0.001121896803080109622 ) ) ;
#89023 = CARTESIAN_POINT ( 'NONE',  ( 1.851626064562774010, 2.084957031469181654, -0.1549042654368226746 ) ) ;
#89024 = CARTESIAN_POINT ( 'NONE',  ( 5.855142236255289845, 7.924361590421551860, -1.599625672291281386 ) ) ;
#89025 = CARTESIAN_POINT ( 'NONE',  ( 6.159198499077391808, -1.652456008184695735, -0.9899348748576908275 ) ) ;
#89026 = CARTESIAN_POINT ( 'NONE',  ( -5.928993247877788697, 5.811580298812519807, 0.7998128361456341429 ) ) ;
#89027 = CARTESIAN_POINT ( 'NONE',  ( 2.151128115021032627, -1.464471472660273665, -1.089769533225225073 ) ) ;
#89028 = CARTESIAN_POINT ( 'NONE',  ( 11.97929049433705551, 12.29999999999999716, 0.7046979865771803020 ) ) ;
#89029 = CARTESIAN_POINT ( 'NONE',  ( 0.7559434568639655794, 0.7726834774516875282, -1.749509110286852742 ) ) ;
#89030 = CARTESIAN_POINT ( 'NONE',  ( 2.084365741702984387, 1.136530121079984301, -1.608336531363078414 ) ) ;
#89031 = CARTESIAN_POINT ( 'NONE',  ( 3.614730616327064716, -0.1400294986239834782, 1.937054734790619293 ) ) ;
#89032 = ORIENTED_EDGE ( 'NONE', *, *, #155084, .T. ) ;
#89033 = DIRECTION ( 'NONE',  ( -0.9632918427306580433, 0.000000000000000000, -0.2684563758389303945 ) ) ;
#89035 = CARTESIAN_POINT ( 'NONE',  ( 0.1505322013598429098, -0.3980627942141829467, -1.824191605747552014 ) ) ;
#89034 = CARTESIAN_POINT ( 'NONE',  ( -3.806807270387036368, 7.663301925418665839, 0.000000000000000000 ) ) ;
#89036 = CARTESIAN_POINT ( 'NONE',  ( 4.278479993564246797, 7.149254538203735798, 1.199719254218452047 ) ) ;
#89037 = CARTESIAN_POINT ( 'NONE',  ( 11.01135777277262306, 10.19999999999998153, 1.399999999999998579 ) ) ;
#89038 = CARTESIAN_POINT ( 'NONE',  ( 8.503988664269582998, 10.94440607977979063, 1.599625672291281386 ) ) ;
#89039 = CARTESIAN_POINT ( 'NONE',  ( -4.423703259808839938, 8.383013913077441259, 0.7998128361456352531 ) ) ;
#89040 = CARTESIAN_POINT ( 'NONE',  ( 4.001749955438753226, 7.811071542261023737, 0.1299566359906061952 ) ) ;
#89041 = ORIENTED_EDGE ( 'NONE', *, *, #60148, .T. ) ;
#89042 = CARTESIAN_POINT ( 'NONE',  ( 5.352436782344940802, 9.466536356036257871, 0.000000000000000000 ) ) ;
#89043 = DIRECTION ( 'NONE',  ( 1.000000000000000000, -0.000000000000000000, -0.000000000000000000 ) ) ;
#89045 = CARTESIAN_POINT ( 'NONE',  ( 5.946499988598237252, -1.422611626450220434, 1.429444749906971790 ) ) ;
#89044 = CARTESIAN_POINT ( 'NONE',  ( 3.949673224339702138, 0.6133576713117370183, -1.719707012317383432 ) ) ;
#89046 = CARTESIAN_POINT ( 'NONE',  ( -10.46653140006992899, 11.31330084294416771, -0.7216878364870267237 ) ) ;
#89047 =( GEOMETRIC_REPRESENTATION_CONTEXT ( 3 ) GLOBAL_UNCERTAINTY_ASSIGNED_CONTEXT ( ( #14236 ) ) GLOBAL_UNIT_ASSIGNED_CONTEXT ( ( #133148, #183987, #166685 ) ) REPRESENTATION_CONTEXT ( 'NONE', 'WORKASPACE' ) );
#89048 = CARTESIAN_POINT ( 'NONE',  ( -5.468737822882341781, 7.600800700804905219, 1.347914668206271038 ) ) ;
#89049 = LINE ( 'NONE', #155106, #56995 ) ;
#89050 = CARTESIAN_POINT ( 'NONE',  ( 5.102362337376947998, -0.6309395149336484154, -1.761181640970375106 ) ) ;
#89051 = CARTESIAN_POINT ( 'NONE',  ( 9.264299036839600987, 9.702770385934682551, -0.7998128361456281477 ) ) ;
#89052 = CARTESIAN_POINT ( 'NONE',  ( 1.682126184939515934, -1.031041751839639087, 1.627202258603721363 ) ) ;
#89053 = CARTESIAN_POINT ( 'NONE',  ( 6.455910365318025868, -0.6640748382394038307, 1.846044136633723243 ) ) ;
#89054 = TOROIDAL_SURFACE ( 'NONE', #51000, 2.149999999999999911, 0.1000000000000000056 ) ;
#89055 = CARTESIAN_POINT ( 'NONE',  ( -8.012344526598182026E-15, 9.609375000341399797, -1.575800808251669460 ) ) ;
#89056 = CARTESIAN_POINT ( 'NONE',  ( -5.819474248763749635, 7.812472595022922128, -1.599625672291256295 ) ) ;
#89057 = CARTESIAN_POINT ( 'NONE',  ( 5.508690485854129903, 5.321227076451600091, 1.040834085586084257E-14 ) ) ;
#89058 = CARTESIAN_POINT ( 'NONE',  ( -5.275531169048911728, 6.287779464379406491, -1.082531754730549967 ) ) ;
#89059 = CARTESIAN_POINT ( 'NONE',  ( 0.1228732512454956405, 0.3668972607131052999, 2.085061435120295847 ) ) ;
#89060 = CARTESIAN_POINT ( 'NONE',  ( -3.314994193297896796, 6.393354490853021765, -0.7784788408506219115 ) ) ;
#89061 = CARTESIAN_POINT ( 'NONE',  ( -1.456019627564700158, 4.349501266769085994, -0.3924612876561416885 ) ) ;
#89062 = CARTESIAN_POINT ( 'NONE',  ( 4.698136132249701724, 0.8899761679339033282, -1.869364561350304488 ) ) ;
#89064 = CARTESIAN_POINT ( 'NONE',  ( 0.6823417656249882723, 2.738541667008084879, -1.181850606188749264 ) ) ;
#89063 = CARTESIAN_POINT ( 'NONE',  ( 0.3800845246329161431, -0.2246070939678334044, -1.827447590993152682 ) ) ;
#89065 = CARTESIAN_POINT ( 'NONE',  ( 5.151170688231202277, 1.131463054214848940, 2.000911673594136797 ) ) ;
#89066 = CARTESIAN_POINT ( 'NONE',  ( 7.646435448427411963, 8.023188899361205273, -0.7216878364870257245 ) ) ;
#89068 = CARTESIAN_POINT ( 'NONE',  ( -8.917737905728749581, 3.447199233515649386, -8.029567276306266876 ) ) ;
#89067 = CARTESIAN_POINT ( 'NONE',  ( 4.909461021924256485, 4.900328411765999981, 0.7216878364870338292 ) ) ;
#89069 = CARTESIAN_POINT ( 'NONE',  ( 0.6742756655733075366, -1.268823270132292791, 1.908895542103898890 ) ) ;
#89070 = CARTESIAN_POINT ( 'NONE',  ( -0.05647967004079332970, -9.990726209582318162, -9.579565160031974003 ) ) ;
#89071 = AXIS2_PLACEMENT_3D ( 'NONE', #69060, #151419, #850 ) ;
#89072 = CARTESIAN_POINT ( 'NONE',  ( -6.424584688029276514, 8.588711117491191871, 1.599625672291269396 ) ) ;
#89073 = CARTESIAN_POINT ( 'NONE',  ( 5.033120997586177481, -1.374529083251808892, -1.372050024763036280 ) ) ;
#89074 = VERTEX_POINT ( 'NONE', #139639 ) ;
#89075 = CARTESIAN_POINT ( 'NONE',  ( 9.259855728009286580, 10.86588177317476855, -1.082531754730543083 ) ) ;
#89076 = ORIENTED_EDGE ( 'NONE', *, *, #72377, .F. ) ;
#89077 = CARTESIAN_POINT ( 'NONE',  ( 6.135011676971934058, 1.786887936952135991, 0.6819008164158719687 ) ) ;
#89078 = CARTESIAN_POINT ( 'NONE',  ( 5.770720322323381168, -0.3006437417610394736, -1.993894057904864514 ) ) ;
#89080 = FILL_AREA_STYLE ('',( #188691 ) ) ;
#89079 = CARTESIAN_POINT ( 'NONE',  ( -9.528683032306089373, 10.01121838064558744, 0.7998128361456462443 ) ) ;
#89081 = CARTESIAN_POINT ( 'NONE',  ( 1.001543065824772753E-15, -2.559374999522041172, 3.793834371823811669 ) ) ;
#89084 = B_SPLINE_CURVE_WITH_KNOTS ( 'NONE', 3,
 ( #126543, #111343, #42032, #77700, #208754, #11626, #108144, #60380, #174170, #4401 ),
 .UNSPECIFIED., .F., .F.,
 ( 4, 3, 3, 4 ),
 ( 3.554236483114673897E-17, 3.125182663314470276E-05, 6.250390969754492131E-05, 0.0001046323561353133347 ),
 .UNSPECIFIED. ) ;
#89083 = CARTESIAN_POINT ( 'NONE',  ( 1.656752475421595872, -1.515787608549432175, -0.9133899773908128461 ) ) ;
#89082 = CARTESIAN_POINT ( 'NONE',  ( 2.414113337891873101, 1.364997783657854846, -1.583610807417460631 ) ) ;
#89085 = CARTESIAN_POINT ( 'NONE',  ( 6.610000000000006537, 0.002781820520842553934, 2.000159646111852929 ) ) ;
#89086 = EDGE_CURVE ( 'NONE', #146443, #140937, #88745, .T. ) ;
#89088 = CARTESIAN_POINT ( 'NONE',  ( 4.347812307665041232, 2.291787294364412642, -0.05403505903618135986 ) ) ;
#89087 = CARTESIAN_POINT ( 'NONE',  ( 3.923105346307896202, 5.670318552149568703, -1.599625672291269396 ) ) ;
#89089 = CARTESIAN_POINT ( 'NONE',  ( 1.798380396644788659, 1.445777515557338688, 0.9684012028719732879 ) ) ;
#89090 = CARTESIAN_POINT ( 'NONE',  ( 3.181359600701000989, 6.863336634126477875, 0.000000000000000000 ) ) ;
#89091 = CARTESIAN_POINT ( 'NONE',  ( -2.671705178897693322, -0.4353224022266648507, -0.1180795802420711998 ) ) ;
#89092 = CARTESIAN_POINT ( 'NONE',  ( 2.547823072707461112, 1.587006686370129316, -0.6987220570618419835 ) ) ;
#89093 = CARTESIAN_POINT ( 'NONE',  ( -9.514659125335341649E-15, 1.359375000341400463, -1.570758158831806250 ) ) ;
#89094 = CARTESIAN_POINT ( 'NONE',  ( 1.679899622522099012, -1.030144609347281026, -1.549723197825584764 ) ) ;
#89095 =( BOUNDED_SURFACE ( )  B_SPLINE_SURFACE ( 3, 2, ( 
 ( #11139, #65995, #127131 ),
 ( #41549, #44752, #110859 ),
 ( #28477, #94568, #200277 ),
 ( #169925, #101732, #134269 ) ),
 .UNSPECIFIED., .F., .F., .F. ) 
 B_SPLINE_SURFACE_WITH_KNOTS ( ( 4, 4 ),
 ( 3, 3 ),
 ( 0.005330693667047302006, 0.008357081610771109614 ),
 ( 0.000000000000000000, 1.000000000000000000 ),
 .UNSPECIFIED. ) 
 GEOMETRIC_REPRESENTATION_ITEM ( )  RATIONAL_B_SPLINE_SURFACE ( (
 ( 1.000000000000000000, 0.7187737999613676987, 1.000000000000000000),
 ( 1.000000000000000000, 0.7186585579881007435, 1.000000000000000000),
 ( 1.000000000000000000, 0.7185467277397570296, 1.000000000000000000),
 ( 1.000000000000000000, 0.7184380228464053442, 1.000000000000000000) ) ) 
 REPRESENTATION_ITEM ( '' )  SURFACE ( )  );
#89096 = CARTESIAN_POINT ( 'NONE',  ( 2.436178610684522461, 1.334241001675811500, 1.712780914784496122 ) ) ;
#89097 = CARTESIAN_POINT ( 'NONE',  ( 5.986088515633498197, 6.942523675449257858, -1.199719254218446718 ) ) ;
#89098 = CARTESIAN_POINT ( 'NONE',  ( 4.259000112335223243, -0.004834882008357410665, -2.016708403958865414 ) ) ;
#89099 = CARTESIAN_POINT ( 'NONE',  ( 3.343750000000002220, 1.895863743164157178, 0.7852924748298092394 ) ) ;
#89100 = CARTESIAN_POINT ( 'NONE',  ( 0.7499999999999902300, 3.014583334016149418, 1.299038105676669330 ) ) ;
#89101 = CARTESIAN_POINT ( 'NONE',  ( 0.5516240470409677910, 0.6072917441693607143, -1.828224634575502883 ) ) ;
#89102 = CARTESIAN_POINT ( 'NONE',  ( 0.6823417656249934904, 14.19270833367473195, 1.181850606188764807 ) ) ;
#89103 = CARTESIAN_POINT ( 'NONE',  ( 4.658541260611516854, 2.215511418189203496, 0.1622135575486300108 ) ) ;
#89104 = ORIENTED_EDGE ( 'NONE', *, *, #201250, .F. ) ;
#89105 = CARTESIAN_POINT ( 'NONE',  ( 0.7499999999999885647, 0.2333333333333562076, 1.299038105676657340 ) ) ;
#89106 = CARTESIAN_POINT ( 'NONE',  ( 6.238723240582662477, 10.43026088065513513, -0.7998128361456291469 ) ) ;
#89107 = CARTESIAN_POINT ( 'NONE',  ( -0.6823417656250246877, 0.05104166700808931978, 1.181850606188755259 ) ) ;
#89108 = CARTESIAN_POINT ( 'NONE',  ( 0.4346306299643958315, -1.193539479193185038, -1.873246666896864143 ) ) ;
#89109 = CARTESIAN_POINT ( 'NONE',  ( 5.248475795274027078, -1.946838731704622072, -0.2419367024937419397 ) ) ;
#89110 = CARTESIAN_POINT ( 'NONE',  ( 7.931156674314368438, 12.19684052010138586, 1.040834085586084257E-14 ) ) ;
#89111 = DIRECTION ( 'NONE',  ( 0.000000000000000000, 0.000000000000000000, 1.000000000000000000 ) ) ;
#89112 = CARTESIAN_POINT ( 'NONE',  ( 6.239586896912570069, -1.632293121298231675, -1.566800261409779349 ) ) ;
#89113 = CARTESIAN_POINT ( 'NONE',  ( -5.655159470675923394, 5.770309935309573923, 0.000000000000000000 ) ) ;
#89114 = CARTESIAN_POINT ( 'NONE',  ( 2.998538507119326901, 2.046783137066817027, 0.2552134970664684532 ) ) ;
#89115 = CARTESIAN_POINT ( 'NONE',  ( -5.904739593951539689, 6.847616600153594746, 1.199719254218450271 ) ) ;
#89116 = EDGE_CURVE ( 'NONE', #62493, #28948, #166783, .T. ) ;
#89117 = CARTESIAN_POINT ( 'NONE',  ( 1.499999999999989120, 2.306250000682817713, 1.214306433183764966E-14 ) ) ;
#89118 = CARTESIAN_POINT ( 'NONE',  ( -1.201851678989727383E-14, 5.259375000341421469, -1.575800808251660134 ) ) ;
#89119 = CARTESIAN_POINT ( 'NONE',  ( 4.921099816907485547, -0.09337705715995943401, 1.868355541605345671 ) ) ;
#89120 = CARTESIAN_POINT ( 'NONE',  ( 3.463219708433932009, -1.672243815576504700, -0.4589255088537134153 ) ) ;
#89121 = CARTESIAN_POINT ( 'NONE',  ( 3.667295640872432649, 0.9703414817801876424, 1.444613691174992720 ) ) ;
#89122 = CARTESIAN_POINT ( 'NONE',  ( 1.171857018789014271, 1.370485515009724820, 1.837452469633732210 ) ) ;
#89123 = CARTESIAN_POINT ( 'NONE',  ( -1.364683531249997417, 4.321875000341417028, 1.214306433183764966E-14 ) ) ;
#89124 = CARTESIAN_POINT ( 'NONE',  ( 4.493745196466782943, -2.090321524099489903, -0.04957026750533782833 ) ) ;
#89125 = CARTESIAN_POINT ( 'NONE',  ( 5.331954954513311584, 1.913531179151845674, 0.3301462080481341599 ) ) ;
#89127 = ORIENTED_EDGE ( 'NONE', *, *, #158166, .F. ) ;
#89126 = CARTESIAN_POINT ( 'NONE',  ( 8.721781227551465676, 14.89250699912923537, 8.248177467968419663 ) ) ;
#89128 = CARTESIAN_POINT ( 'NONE',  ( 0.8092204703840089053, 1.198858234535697065, -1.621184076614573533 ) ) ;
#89129 = CARTESIAN_POINT ( 'NONE',  ( 0.4926326669930108371, -1.172979896111199904, 1.766458537607276114 ) ) ;
#89130 = CARTESIAN_POINT ( 'NONE',  ( -5.232130268375919232E-15, -8.644755361503010604, 10.68216772480111132 ) ) ;
#89131 = DIRECTION ( 'NONE',  ( 0.000000000000000000, -1.000000000000000000, 0.000000000000000000 ) ) ;
#89132 = CARTESIAN_POINT ( 'NONE',  ( -6.842061076390810292, 11.13415502243129218, 0.000000000000000000 ) ) ;
#89133 = CARTESIAN_POINT ( 'NONE',  ( 7.470706336329915764, 8.674577799595093452, -1.199719254218441611 ) ) ;
#89134 = CARTESIAN_POINT ( 'NONE',  ( 2.244932509249154329, 2.057497683098849617, 0.5125483897536405875 ) ) ;
#89135 = DIRECTION ( 'NONE',  ( 0.5038915848600621361, -0.5182601445700819598, -0.6910135261030805331 ) ) ;
#89136 = CARTESIAN_POINT ( 'NONE',  ( 4.072732355924274295, -1.704239406772959153, -0.6552279023967976235 ) ) ;
#89137 = ORIENTED_EDGE ( 'NONE', *, *, #56512, .F. ) ;
#89138 = CARTESIAN_POINT ( 'NONE',  ( -6.257970421159510188, 9.458660037064859694, 1.199719254218452047 ) ) ;
#89139 = CARTESIAN_POINT ( 'NONE',  ( -3.070003471035267939, 6.451017196056028524, -0.6895117023006979151 ) ) ;
#89140 = CARTESIAN_POINT ( 'NONE',  ( -1.642778471875000035, -0.9552083328553742092, -2.845375778867859751 ) ) ;
#89141 = CARTESIAN_POINT ( 'NONE',  ( -6.612626235163205024, 8.737816579155630592, -1.599625672291263179 ) ) ;
#89142 = CARTESIAN_POINT ( 'NONE',  ( 2.074478865019005802, 0.8673736069498124701, 1.824228476594942583 ) ) ;
#89143 = CARTESIAN_POINT ( 'NONE',  ( 5.649526978565787338, -1.736373965863503122, -1.361823127433124725 ) ) ;
#89144 = CARTESIAN_POINT ( 'NONE',  ( -5.307090785106547415, 5.156303768904543894, -0.7998128361456362523 ) ) ;
#89145 = CARTESIAN_POINT ( 'NONE',  ( 3.274093294390582276, -0.9130387472845059582, -1.621452132119176159 ) ) ;
#89146 = CARTESIAN_POINT ( 'NONE',  ( 3.837121167867449945, 4.435395103055503441, 1.199719254218464037 ) ) ;
#89147 = DIRECTION ( 'NONE',  ( 5.578564026256490882E-16, 1.000000000000000000, 9.066213480720158442E-32 ) ) ;
#89148 = EDGE_LOOP ( 'NONE', ( #124838, #182969, #97788 ) ) ;
#89149 = CARTESIAN_POINT ( 'NONE',  ( -5.253948220495577637, 6.088359997788290734, 1.199719254218450271 ) ) ;
#89150 = CARTESIAN_POINT ( 'NONE',  ( -9.332089804907933939, 9.781859615347734405, 1.040834085586084257E-14 ) ) ;
#89151 = CARTESIAN_POINT ( 'NONE',  ( 5.197797600609998625, -0.6536857159176562293, 1.704833070275885598 ) ) ;
#89152 = AXIS2_PLACEMENT_3D ( 'NONE', #184667, #86120, #203041 ) ;
#89154 = CARTESIAN_POINT ( 'NONE',  ( -3.975569122714607495, 7.849474212055944200, 0.02231197147695325456 ) ) ;
#89153 = CARTESIAN_POINT ( 'NONE',  ( -5.887983850084758330, 10.09134126839936840, 0.7998128361456291469 ) ) ;
#89155 = CARTESIAN_POINT ( 'NONE',  ( 6.505076094845553492, 6.832456077006010098, -0.5564590407885674495 ) ) ;
#89156 = CARTESIAN_POINT ( 'NONE',  ( 0.7195771044254402060, -1.460395948178545344, -0.9342476737749583204 ) ) ;
#89157 = CARTESIAN_POINT ( 'NONE',  ( 0.3041415704291222100, 1.511679331021776207, 0.8621369596173468208 ) ) ;
#89158 = CARTESIAN_POINT ( 'NONE',  ( 5.778008146871475681, 1.369946362297723264, 1.856932335381543897 ) ) ;
#89159 = CARTESIAN_POINT ( 'NONE',  ( 5.740951700743842423, 5.662474837148078421, -0.7998128361456481317 ) ) ;
#89160 = CARTESIAN_POINT ( 'NONE',  ( 0.6673476085290538373, 0.2044725723429566266, -2.050631486922994906 ) ) ;
#89161 = CARTESIAN_POINT ( 'NONE',  ( 7.169564303528210836, 7.258913197071374945, -0.7998128361456281477 ) ) ;
#89162 = CARTESIAN_POINT ( 'NONE',  ( 5.167441833834662823, -0.7673274391166631236, -2.166651051963175423 ) ) ;
#89163 = CARTESIAN_POINT ( 'NONE',  ( -9.499700864329909678, -7.154544010627095219, -0.07538891330675229208 ) ) ;
#89164 = CARTESIAN_POINT ( 'NONE',  ( -6.505933609711270549, 8.683618192786854095, -1.599625672291271394 ) ) ;
#89165 = CARTESIAN_POINT ( 'NONE',  ( 5.840666405660361882, 0.3664468388623157158, 1.834233659845653897 ) ) ;
#89166 = CIRCLE ( 'NONE', #47576, 4.500000000000000000 ) ;
#89167 = B_SPLINE_CURVE_WITH_KNOTS ( 'NONE', 3,
 ( #116096, #166935, #69397, #119303, #134463, #18528, #164792, #84605, #117169, #99795 ),
 .UNSPECIFIED., .F., .F.,
 ( 4, 3, 3, 4 ),
 ( 3.757351081995909416E-18, 3.125177024600283269E-05, 5.801553290628923905E-05, 8.478882652531181735E-05 ),
 .UNSPECIFIED. ) ;
#89169 = CARTESIAN_POINT ( 'NONE',  ( -5.157951095356222204, 4.982307464195829816, 0.000000000000000000 ) ) ;
#89168 = CARTESIAN_POINT ( 'NONE',  ( 3.480628297764537304, -1.280852673386581264, 1.420289963180096260 ) ) ;
#89170 = CARTESIAN_POINT ( 'NONE',  ( 5.584669497696876483, -2.152379054646291756, -0.4867646435422824935 ) ) ;
#89171 = CARTESIAN_POINT ( 'NONE',  ( 5.050072346573388771, 1.046394516673061270, 1.840669678815173960 ) ) ;
#89172 = CARTESIAN_POINT ( 'NONE',  ( 0.6124999999999828360, 0.6458333340161465097, 1.060881119635891157 ) ) ;
#89173 = CARTESIAN_POINT ( 'NONE',  ( 4.245111494854632461, 7.966730820723463502, 0.000000000000000000 ) ) ;
#89174 = CARTESIAN_POINT ( 'NONE',  ( 5.058600711230250013, 5.074324715956299414, -0.7216878364870458196 ) ) ;
#89175 = CARTESIAN_POINT ( 'NONE',  ( -4.272227801637618505, 7.998366511970260717, 0.7216878364870338292 ) ) ;
#89176 = CARTESIAN_POINT ( 'NONE',  ( 5.479186192515411946, -1.917069751554843160, -0.9065152316691318379 ) ) ;
#89177 = CARTESIAN_POINT ( 'NONE',  ( 2.327567518148494941, 0.0001997265634129384874, 2.307758715027211416 ) ) ;
#89178 = CARTESIAN_POINT ( 'NONE',  ( 3.455471728117681440, 1.544996161402897528, 1.208956721487665087 ) ) ;
#89179 = DIRECTION ( 'NONE',  ( 0.000000000000000000, 1.000000000000000000, 0.000000000000000000 ) ) ;
#89180 = CARTESIAN_POINT ( 'NONE',  ( 1.305434336737832490, -1.543085766649286317, -1.211208057394968618 ) ) ;
#89181 = CARTESIAN_POINT ( 'NONE',  ( 3.931501358282940117, 4.649468341827285300, -1.082531754730543083 ) ) ;
#89182 = CARTESIAN_POINT ( 'NONE',  ( 4.716257332707354699, 6.595662536282280719, -1.599625672291269396 ) ) ;
#89183 = ORIENTED_EDGE ( 'NONE', *, *, #52019, .T. ) ;
#89184 = CARTESIAN_POINT ( 'NONE',  ( 5.507046092540283766, -0.04465857163906890998, 2.016188657829049991 ) ) ;
#89185 = CARTESIAN_POINT ( 'NONE',  ( -7.797910906154257304, 12.24931315715533486, 0.000000000000000000 ) ) ;
#89186 = CARTESIAN_POINT ( 'NONE',  ( 0.7499999999999920064, 4.233333333333352932, 1.299038105676669330 ) ) ;
#89187 = CARTESIAN_POINT ( 'NONE',  ( -10.45911050446410506, 5.175404930453152197, 5.201426885097844455 ) ) ;
#89188 = CARTESIAN_POINT ( 'NONE',  ( 3.362351297888244606, -2.168775535925556053, 0.1018362995675748534 ) ) ;
#89189 = DIRECTION ( 'NONE',  ( 0.000000000000000000, -1.000000000000000000, 0.000000000000000000 ) ) ;
#89190 = CARTESIAN_POINT ( 'NONE',  ( 0.3520121086563637314, -1.504009422257305495, -1.495223887398588358 ) ) ;
#89191 = CARTESIAN_POINT ( 'NONE',  ( -1.402160292154681736E-14, 2.118750000682816825, -1.732050807568863648 ) ) ;
#89192 = CARTESIAN_POINT ( 'NONE',  ( -9.333041836229170940, 14.55305236563267535, -7.472413793097618218 ) ) ;
#89193 = CARTESIAN_POINT ( 'NONE',  ( 4.352673489508670279, 7.270661361071050877, 1.119103973195253232 ) ) ;
#89194 = CARTESIAN_POINT ( 'NONE',  ( 4.817101577040221905, 8.228953320636518853, 0.8951067572735508238 ) ) ;
#89195 = CARTESIAN_POINT ( 'NONE',  ( 0.8255485222598609729, -1.957653584835903349, 0.6440290526678188465 ) ) ;
#89196 = CARTESIAN_POINT ( 'NONE',  ( -10.64045162862669081, 11.30828174301964140, -0.7998128361456221525 ) ) ;
#89197 = CARTESIAN_POINT ( 'NONE',  ( 1.364683531249988757, 1.134375000341421247, 0.000000000000000000 ) ) ;
#89198 = DIRECTION ( 'NONE',  ( 0.4999999999999917843, 0.000000000000000000, -0.8660254037844433705 ) ) ;
#89199 = VERTEX_POINT ( 'NONE', #154801 ) ;
#89200 = CARTESIAN_POINT ( 'NONE',  ( 2.965378323150099416, -1.564627974442783120, -1.099164922500090347 ) ) ;
#89201 = CARTESIAN_POINT ( 'NONE',  ( 5.295665003108637414, -0.6346038033320391403, 1.652335088206556613 ) ) ;
#89202 = CARTESIAN_POINT ( 'NONE',  ( 4.850785098639300408, 8.881276058379668825, -0.7998128361456481317 ) ) ;
#89203 = CARTESIAN_POINT ( 'NONE',  ( -3.795392936821753604, 6.515376628678959392, -1.199719254218452047 ) ) ;
#89204 = CARTESIAN_POINT ( 'NONE',  ( 0.08776524826303951088, 1.042983370315919478, 1.480986741271082430 ) ) ;
#89206 = CARTESIAN_POINT ( 'NONE',  ( 0.9014164429375628451, -1.868237418080781254, 0.4230343950424199084 ) ) ;
#89205 = DIRECTION ( 'NONE',  ( -5.578564026256490882E-16, -1.000000000000000000, -9.066213480720158442E-32 ) ) ;
#89207 = CARTESIAN_POINT ( 'NONE',  ( 2.506376218629560171, 2.069854378281150709, 0.05321039126485183068 ) ) ;
#89208 = CARTESIAN_POINT ( 'NONE',  ( -1.364683531250014514, 0.05104166700808546175, -0.7879004041258359514 ) ) ;
#89209 = VECTOR ( 'NONE', #192857, 1000.000000000000000 ) ;
#89210 = CARTESIAN_POINT ( 'NONE',  ( 6.174654088403855212, -1.776896415251895789, -0.5849557326117056366 ) ) ;
#89211 = CARTESIAN_POINT ( 'NONE',  ( 2.420285107995377327, 1.192830232448302441, -1.382225081888274643 ) ) ;
#89213 = CARTESIAN_POINT ( 'NONE',  ( 5.614387949662905442, 7.370906683214474953, 1.237392280610301931 ) ) ;
#89212 = CARTESIAN_POINT ( 'NONE',  ( 6.094375512030342001, -2.195847865938059140, -0.2203403561373064590 ) ) ;
#89214 = EDGE_CURVE ( 'NONE', #93709, #1871, #171751, .T. ) ;
#89215 = CARTESIAN_POINT ( 'NONE',  ( -1.364683531250000748, -0.2406249996585799189, 0.000000000000000000 ) ) ;
#89216 = CARTESIAN_POINT ( 'NONE',  ( 3.631348232279749233, 0.05352869315983609100, -2.062151203995182147 ) ) ;
#89217 = CARTESIAN_POINT ( 'NONE',  ( -6.353967546298838087, 10.56471257065732416, 0.000000000000000000 ) ) ;
#89218 = CARTESIAN_POINT ( 'NONE',  ( 7.865701674222579598, 12.32840238656838139, -0.7998128361456352531 ) ) ;
#89219 = CARTESIAN_POINT ( 'NONE',  ( 5.464099601507359516, 6.333536608968757697, 1.199719254218462483 ) ) ;
#89220 = CARTESIAN_POINT ( 'NONE',  ( -0.08522875510949735889, -9.999176759342303100, -10.91956886450204145 ) ) ;
#89221 = CARTESIAN_POINT ( 'NONE',  ( 6.144996677366851401, -0.2998803957653916608, -2.048400609436632269 ) ) ;
#89222 = CARTESIAN_POINT ( 'NONE',  ( -1.201851678989727383E-14, 1.384375000341419693, 1.575800808251672791 ) ) ;
#89223 = CARTESIAN_POINT ( 'NONE',  ( 3.813887338145681927, -2.130327034543195275, 0.3653767458386343314 ) ) ;
#89224 = CARTESIAN_POINT ( 'NONE',  ( 3.756514258062096712, 2.010158954970509892, 0.1956256540626959695 ) ) ;
#89225 = DIRECTION ( 'NONE',  ( 0.000000000000000000, -1.000000000000000000, 0.000000000000000000 ) ) ;
#89226 = B_SPLINE_CURVE_WITH_KNOTS ( 'NONE', 3,
 ( #7789, #173541, #107512, #12069 ),
 .UNSPECIFIED., .F., .F.,
 ( 4, 4 ),
 ( 1.062296840242581388E-18, 0.0002848003335318597751 ),
 .UNSPECIFIED. ) ;
#89227 = EDGE_CURVE ( 'NONE', #80644, #25151, #195981, .T. ) ;
#89230 = CARTESIAN_POINT ( 'NONE',  ( 6.073689629242148058, 8.109057205581079231, -1.443375672974057666 ) ) ;
#89229 = CARTESIAN_POINT ( 'NONE',  ( 3.475000000000000533, -0.1458333333333326765, -2.006292185433951047 ) ) ;
#89228 = PLANE ( 'NONE',  #69666 ) ;
#89231 = CARTESIAN_POINT ( 'NONE',  ( -8.120407659942227241, 8.438506789546210030, 0.7998128361456341429 ) ) ;
#89232 = CARTESIAN_POINT ( 'NONE',  ( 2.712125330650519750, 1.116209241849321465, -1.679223868463100011 ) ) ;
#89234 = CARTESIAN_POINT ( 'NONE',  ( -11.00020965659414784, -5.765528217051525850, -0.01167607004747446206 ) ) ;
#89233 = CARTESIAN_POINT ( 'NONE',  ( -3.391510981712833939, 7.108513245306943062, 0.7998128361456341429 ) ) ;
#89235 = CARTESIAN_POINT ( 'NONE',  ( -1.499999999999997780, 5.681250000682820378, 1.214306433183764966E-14 ) ) ;
#89236 = CARTESIAN_POINT ( 'NONE',  ( 5.590081826628392925, 1.144292256163012667, 1.532101299821154949 ) ) ;
#89237 = CARTESIAN_POINT ( 'NONE',  ( -11.88234649872613602, 12.34339217083249096, 0.9090484974825225883 ) ) ;
#89238 = CARTESIAN_POINT ( 'NONE',  ( 4.636525345749193505, 8.353103970108639587, 1.040834085586084257E-14 ) ) ;
#89240 = CARTESIAN_POINT ( 'NONE',  ( 4.042592340535226647, -1.492244431823461115, 1.356313616978216618 ) ) ;
#89239 = CARTESIAN_POINT ( 'NONE',  ( -8.649738815394339753, 9.193709494155953621, 1.040834085586084257E-14 ) ) ;
#89241 = CARTESIAN_POINT ( 'NONE',  ( -0.7500000000000215383, 3.941666666666690411, 1.299038105676671107 ) ) ;
#89242 = CARTESIAN_POINT ( 'NONE',  ( -1.402160292154681736E-14, 15.23437500034140157, 1.575800808251682339 ) ) ;
#89243 = CARTESIAN_POINT ( 'NONE',  ( 6.317413179709785886, -0.2053877530918957195, 1.712446389806308256 ) ) ;
#89244 = CARTESIAN_POINT ( 'NONE',  ( 5.200434439293556643, 8.224868058221247225, -1.199719254218452047 ) ) ;
#89245 = CARTESIAN_POINT ( 'NONE',  ( 8.378575743565351175, 11.75846021992619406, -1.082531754730543083 ) ) ;
#89246 = CARTESIAN_POINT ( 'NONE',  ( -6.773846765317340868, -7.246166700180801001, -6.773846765317303564 ) ) ;
#89247 = CARTESIAN_POINT ( 'NONE',  ( 4.376139848268215893, -1.078761963904120602, 1.527931137620001989 ) ) ;
#89248 = DIRECTION ( 'NONE',  ( -5.551115123125766062E-17, 0.000000000000000000, 1.000000000000000000 ) ) ;
#89249 = CARTESIAN_POINT ( 'NONE',  ( 1.850524992189076290, -2.059912964915584954, -0.2069831422613493399 ) ) ;
#89250 = CARTESIAN_POINT ( 'NONE',  ( 1.499999999999996891, 12.42708333401612819, -0.8660254037844378194 ) ) ;
#89251 = VERTEX_POINT ( 'NONE', #95145 ) ;
#89252 = CARTESIAN_POINT ( 'NONE',  ( 3.528865121306874464, 7.339036084825155015, -0.7998128361456362523 ) ) ;
#89254 = EDGE_CURVE ( 'NONE', #179210, #155393, #210489, .T. ) ;
#89253 = CARTESIAN_POINT ( 'NONE',  ( 0.3336115229473045618, 0.6298545048411038350, -1.915608025624820909 ) ) ;
#89255 = CARTESIAN_POINT ( 'NONE',  ( 0.8260602286952464235, -0.8153974433127196830, -1.617802387155008681 ) ) ;
#89256 = CARTESIAN_POINT ( 'NONE',  ( 5.546694241322223107, 5.643767167730274537, -0.7216878364870458196 ) ) ;
#89257 = CIRCLE ( 'NONE', #172281, 0.04999999999999969746 ) ;
#89258 = CARTESIAN_POINT ( 'NONE',  ( -0.04208621775141922761, -6.437359833193936787, -10.89523958697327011 ) ) ;
#89259 = CARTESIAN_POINT ( 'NONE',  ( 6.751597309481075726, 10.82068792779586985, 1.040834085586084257E-14 ) ) ;
#89260 = CARTESIAN_POINT ( 'NONE',  ( 7.052212457402625922, 11.37933163361175382, -0.7998128361456291469 ) ) ;
#89262 = CARTESIAN_POINT ( 'NONE',  ( 6.327746003090493510, 0.7280626223893000848, -1.772066133663487530 ) ) ;
#89261 = CARTESIAN_POINT ( 'NONE',  ( -6.287230548435221777, 8.358188277972981695, -1.599625672291263179 ) ) ;
#89263 = CARTESIAN_POINT ( 'NONE',  ( 0.000000000000000000, 13.79999999999998295, 0.000000000000000000 ) ) ;
#89264 = EDGE_CURVE ( 'NONE', #168570, #83886, #8805, .T. ) ;
#89265 = CARTESIAN_POINT ( 'NONE',  ( -1.402160292154681736E-14, -1.115624999658584082, 1.575800808251672791 ) ) ;
#89267 = VERTEX_POINT ( 'NONE', #90883 ) ;
#89266 = CARTESIAN_POINT ( 'NONE',  ( 5.205967797967541166, 5.175976640491323444, -0.7216878364870197293 ) ) ;
#89268 = CARTESIAN_POINT ( 'NONE',  ( -8.026063749610056419, 10.38682701267698150, -1.443375672974059665 ) ) ;
#89269 = CARTESIAN_POINT ( 'NONE',  ( 3.309602206082487008, -0.4233974974612622066, 2.119663826602156131 ) ) ;
#89270 = EDGE_CURVE ( 'NONE', #76877, #167216, #93018, .T. ) ;
#89271 = CARTESIAN_POINT ( 'NONE',  ( -3.363304624641834106, 6.081549941127532222, -1.199719254218452047 ) ) ;
#89272 = CARTESIAN_POINT ( 'NONE',  ( 7.187230829020130329, 7.557726520044554697, 0.7216878364870267237 ) ) ;
#89273 = CARTESIAN_POINT ( 'NONE',  ( 1.019968326173793960, -0.5097545255977400380, 2.058319881341897695 ) ) ;
#89274 = CARTESIAN_POINT ( 'NONE',  ( 5.772426501671442445, -1.156275361458743545, 1.412693073426966039 ) ) ;
#89275 =( BOUNDED_SURFACE ( )  B_SPLINE_SURFACE ( 1, 2, ( 
 ( #29880, #211801, #130645, #79682, #62366, #33067, #113328, #128528, #13607, #80759, #147897, #179335, #14666, #146848, #45079, #63439, #213913, #64502, #48277, #193435, #177191, #114390, #15729, #180385, #98092, #81814, #65536, #131682, #197684, #115448, #99145, #165195, #170520, #36243, #100193, #17849, #133800, #5860, #185692, #166259, #68734, #50382, #103397, #135905, #22102, #199810, #182494, #88215, #51454, #86076, #154286, #52508, #134855, #198735, #83934, #132732, #70860, #116503, #102322, #69796, #201923, #34122, #150024, #1593, #21044, #183569, #67654, #101252, #87141, #186767, #53576, #54642, #85006, #117574, #35175, #169457, #118641, #119710, #167335, #18921, #151097, #2661, #200861, #184626, #168395, #19992, #152151, #3721, #37322, #153212, #4782, #136975, #203002, #120790, #38393, #104473, #111740, #171589, #9894, #75971, #144224, #79165, #28285, #162567, #143152, #209146, #159351, #13085, #71932, #60785, #10948, #142074, #126944, #62910, #208088, #23182, #128021, #192901, #44557, #121861, #175622, #195051, #77022, #158303, #177746, #138042, #59716, #145281, #176673, #210218, #92257, #110673, #94380, #125875, #160420, #12026, #191834, #96519, #204055, #78097, #43497, #109617, #129080, #61854, #193975, #27209, #39459, #55707, #45623, #29361, #95456, #161505, #211287, #46690, #112807, #187832, #178821, #30433, #105554, #93315, #198228, #84487, #16268, #83418, #196128, #100738, #35733, #114928, #184112, #34668, #65030, #1082, #63987, #183054, #148443, #99680, #80233, #32547, #133281, #2140, #166818, #132218, #213408, #67146, #200351, #181979, #66077, #131186, #50932, #199288, #49864, #197175, #130139, #47768, #146331, #82353, #113881, #48811, #115990, #179876, #33610, #101808, #118127, #68217, #13, #165750, #17336, #180926, #150578, #98623, #164685, #117057, #14140, #31501, #149499, #18412, #134347, #52001, #97575, #15214, #212346, #163632, #81305, #147382, #119186, #87688, #188379, #23743, #53052, #187317, #172151, #89848, #122421, #154832, #71414, #55195, #155898, #169995, #103953, #201413, #171066, #168938, #7485, #20540, #22663, #185171, #73567, #40017, #88774, #6416, #139669, #135391, #186242, #205690, #72488, #57326, #56263, #138589, #3209, #86623, #37877, #105028, #54132, #69278, #123490, #21583, #102880, #70343, #121342, #106128, #153762, #5331, #137526, #19475, #202479, #189454, #36795, #203541, #41095, #167876, #136460, #204612, #85551, #38944, #120267, #152691, #151641, #4272, #8563, #107205, #59452, #145008, #10686, #74643, #206760, #108278, #194777, #160157, #140749, #43232, #24808, #77829, #110408, #211014, #174299, #156974, #62636, #25873, #60510, #128795, #26939, #109349, #173228, #58392, #90909, #45353, #124548, #76756, #44287, #176412, #94116, #190506, #42163, #175359, #142878, #143950, #28018, #91984, #158042, #29092, #9629, #192634, #75706, #141821, #93047, #127752, #177477, #207823, #126671, #111472, #95176, #61584, #11755, #208880, #209945, #161225, #159088, #193709, #125609, #12812, #191568, #78885, #113603, #49596, #63713, #166551, #66872, #115720, #99422, #34403, #13879, #64775, #182785, #165476, #100475, #149229, #181710, #96241, #179607, #130916, #197965, #147119, #162292, #18138, #48549, #195854, #163361, #148179, #804, #196909, #98351, #114667, #112530, #81032, #133017, #79958, #180661, #1881, #46414, #14936, #83150, #150315, #32286, #213145, #146060, #134085, #67941, #212074, #178543, #164417, #84227, #16001, #129870, #47494, #31228, #30153, #17072, #97302, #82086, #214180, #199016, #33340, #65808, #131955, #50662, #116788, #52793, #153509, #89590, #120005, #136200, #51743, #19215, #7223, #138331, #73299, #169745, #137270, #54937, #35470, #85294, #117866, #202218, #101548, #168679, #21334, #167617, #37615, #183857, #204347, #121089, #56005, #5078, #200094, #53872, #185981, #70085, #122156, #118932, #203290, #2949, #105860, #6155, #187056, #38688, #188124, #151380, #4016, #39755, #104767, #171886, #88516, #170816, #69021, #184912, #103695, #22407, #86367, #135138, #23483, #87440, #201154, #102623, #71153, #154578, #72224, #155639, #36536, #20282, #152437, #159902 ),
 ( #91733, #177226, #42981, #106946, #24548, #140494, #12567, #192383, #172969, #75453, #57071, #110155, #142620, #28839, #206504, #189200, #94927, #58135, #92795, #160976, #59194, #141566, #205434, #90655, #139401, #77580, #123235, #109091, #76509, #208629, #40837, #156717, #8308, #207574, #74392, #108022, #175107, #124294, #111223, #190253, #10437, #157785, #125350, #26693, #158840, #41911, #209696, #174048, #25621, #126419, #9382, #191313, #60262, #44037, #176168, #27768, #93864, #11509, #61339, #143703, #127498, #193469, #45113, #212900, #99171, #148973, #178303, #98121, #82900, #547, #33096, #65563, #196666, #180417, #66612, #80790, #14695, #112287, #81843, #79711, #147926, #95995, #130677, #64533, #13638, #32035, #164173, #129623, #100220, #210776, #146880, #29912, #162048, #132759, #213942, #15758, #145826, #46173, #166288, #48306, #131710, #114417, #197714, #49356, #115474, #181467, #62397, #198762, #165223, #211831, #195609, #16815, #50411, #116531, #182520, #63468, #34150, #78639, #179364, #144765, #128561, #47245, #194526, #113359, #30986, #97061, #163114, #83962, #36272, #136999, #5885, #104501, #135929, #2688, #4807, #204081, #185716, #69821, #68761, #54668, #203027, #201947, #134881, #120816, #200888, #167362, #52534, #186793, #71958, #21068, #154312, #184651, #151123, #1623, #38421, #152177, #87166, #118668, #117604, #102349, #168421, #20017, #133827, #18950, #86105, #105583, #3746, #51481, #199839, #85034, #170545, #22129, #138068, #150051, #53603, #119737, #55734, #67682, #88242, #153236, #121888, #37349, #17878, #103423, #169484, #70889, #187858, #183596, #39485, #35203, #101279, #157527, #159650, #106679, #122975, #10184, #9122, #75198, #6956, #57872, #77325, #41650, #40573, #60008, #44856, #90386, #175914, #58942, #188934, #141309, #207321, #172702, #125099, #191057, #8041, #193208, #89324, #173790, #56805, #24280, #11247, #174856, #42722, #156455, #139135, #171617, #25366, #108830, #107764, #26434, #76258, #92545, #142367, #155371, #143438, #158584, #205163, #74130, #208376, #27505, #91466, #126161, #140225, #43790, #23211, #124034, #127239, #192125, #206246, #109902, #73037, #93605, #209435, #61079, #190000, #129373, #15503, #98921, #197464, #14438, #95743, #97867, #82649, #64284, #162860, #161794, #147675, #81590, #80528, #13385, #213692, #79461, #45920, #145577, #65314, #164974, #114173, #32844, #63209, #29657, #94673, #131463, #30728, #180167, #211575, #210518, #195352, #46984, #113100, #12309, #112040, #179106, #198518, #96811, #144510, #78390, #178041, #49108, #115228, #16566, #176968, #146625, #212642, #148733, #28585, #181218, #31793, #301, #130430, #110961, #196416, #48060, #163928, #66372, #160715, #132520, #62153, #128312, #194275, #38180, #199587, #1377, #103180, #36028, #168177, #99979, #150876, #170298, #134640, #133583, #152994, #137827, #183352, #54432, #151932, #119489, #52294, #50164, #101027, #83713, #17628, #117354, #4570, #136754, #104252, #116285, #85858, #34956, #21886, #182276, #202782, #185476, #120574, #3507, #33900, #118423, #184409, #200645, #186551, #166043, #102106, #19776, #51230, #69577, #87996, #167118, #67438, #169240, #135688, #201713, #149803, #2439, #154068, #53354, #18705, #70643, #84788, #68513, #5633, #37100, #20828, #86926, #71714, #189749, #138896, #91217, #8867, #40326, #10989, #121647, #205996, #89079, #72796, #191874, #207064, #74946, #204915, #171371, #77064, #57632, #141057, #139974, #107511, #42468, #124842, #108578, #187614, #109657, #58694, #22964, #106431, #173540, #59755, #123791, #190808, #155136, #76010, #203848, #90144, #159390, #9935, #172454, #174606, #39242, #158341, #41401, #26182, #55493, #7788, #92297, #43534, #142113, #25114, #188690, #208126, #175659, #157278, #125915, #24041, #27247, #93353, #105334, #156212, #6718, #73881, #56569, #122727, #64029, #31539, #178862, #113921, #45665, #78137, #60825, #80274, #13130, #30473, #128059, #176712, #210260, #194015, #61898, #192945, #12068, #213446, #44597, #95496, #62951, #146372, #96558, #94421, #144267, #179917, #163672, #46734, #111782, #28325, #161543, #130175, #47808, #110712 ) ),
 .UNSPECIFIED., .F., .F., .T. ) 
 B_SPLINE_SURFACE_WITH_KNOTS ( ( 2, 2 ),
 ( 3, 2, 2, 2, 2, 2, 2, 2, 2, 2, 2, 2, 2, 2, 2, 2, 2, 2, 2, 2, 2, 2, 2, 2, 2, 2, 2, 2, 2, 2, 2, 2, 2, 2, 2, 2, 2, 2, 2, 2, 2, 2, 2, 2, 2, 2, 2, 2, 2, 2, 2, 2, 2, 2, 2, 2, 2, 2, 2, 2, 2, 2, 2, 2, 2, 2, 2, 2, 2, 2, 2, 2, 2, 2, 2, 2, 2, 2, 2, 2, 2, 2, 2, 2, 2, 2, 2, 2, 2, 2, 2, 2, 2, 2, 2, 2, 2, 2, 2, 2, 2, 2, 2, 2, 2, 2, 2, 2, 2, 2, 2, 2, 2, 2, 2, 2, 2, 2, 2, 2, 2, 2, 2, 2, 2, 2, 2, 2, 2, 2, 2, 2, 2, 2, 2, 2, 2, 2, 2, 2, 2, 2, 2, 2, 2, 2, 2, 2, 2, 2, 2, 2, 2, 2, 2, 2, 2, 2, 2, 2, 2, 2, 2, 2, 2, 2, 2, 2, 2, 2, 2, 2, 2, 2, 2, 2, 2, 2, 2, 2, 2, 2, 2, 2, 2, 2, 2, 2, 2, 2, 2, 2, 2, 2, 2, 2, 2, 2, 2, 2, 2, 2, 2, 2, 2, 2, 2, 2, 2, 2, 2, 2, 2, 2, 2, 2, 2, 2, 2, 2, 2, 2, 2, 2, 2, 2, 2, 2, 2, 2, 2, 2, 2, 2, 2, 2, 2, 2, 2, 2, 3 ),
 ( 0.000000000000000000, 1.000000000000000000 ),
 ( 0.000000000000000000, 0.004166666666666666609, 0.008333333333333333218, 0.01250000000000000069, 0.01666666666666666644, 0.02083333333333333218, 0.02500000000000000139, 0.02916666666666666713, 0.03333333333333333287, 0.03749999999999999861, 0.04166666666666666435, 0.04583333333333333010, 0.05000000000000000278, 0.05416666666666666852, 0.05833333333333333426, 0.06250000000000000000, 0.06666666666666666574, 0.07083333333333333148, 0.07499999999999999722, 0.07916666666666666297, 0.08333333333333332871, 0.08749999999999999445, 0.09166666666666666019, 0.09583333333333333981, 0.1000000000000000056, 0.1041666666666666713, 0.1083333333333333370, 0.1125000000000000028, 0.1166666666666666685, 0.1208333333333333343, 0.1250000000000000000, 0.1291666666666666796, 0.1333333333333333315, 0.1375000000000000111, 0.1416666666666666630, 0.1458333333333333426, 0.1499999999999999944, 0.1541666666666666741, 0.1583333333333333259, 0.1625000000000000056, 0.1666666666666666574, 0.1708333333333333370, 0.1749999999999999889, 0.1791666666666666685, 0.1833333333333333204, 0.1875000000000000000, 0.1916666666666666796, 0.1958333333333333315, 0.2000000000000000111, 0.2041666666666666630, 0.2083333333333333426, 0.2124999999999999944, 0.2166666666666666741, 0.2208333333333333259, 0.2250000000000000056, 0.2291666666666666574, 0.2333333333333333370, 0.2374999999999999889, 0.2416666666666666685, 0.2458333333333333204, 0.2500000000000000000, 0.2541666666666666519, 0.2583333333333333592, 0.2625000000000000111, 0.2666666666666666630, 0.2708333333333333148, 0.2750000000000000222, 0.2791666666666666741, 0.2833333333333333259, 0.2874999999999999778, 0.2916666666666666852, 0.2958333333333333370, 0.2999999999999999889, 0.3041666666666666408, 0.3083333333333333481, 0.3125000000000000000, 0.3166666666666666519, 0.3208333333333333592, 0.3250000000000000111, 0.3291666666666666630, 0.3333333333333333148, 0.3375000000000000222, 0.3416666666666666741, 0.3458333333333333259, 0.3499999999999999778, 0.3541666666666666852, 0.3583333333333333370, 0.3624999999999999889, 0.3666666666666666408, 0.3708333333333333481, 0.3750000000000000000, 0.3791666666666666519, 0.3833333333333333592, 0.3875000000000000111, 0.3916666666666666630, 0.3958333333333333148, 0.4000000000000000222, 0.4041666666666666741, 0.4083333333333333259, 0.4124999999999999778, 0.4166666666666666852, 0.4208333333333333370, 0.4249999999999999889, 0.4291666666666666408, 0.4333333333333333481, 0.4375000000000000000, 0.4416666666666666519, 0.4458333333333333592, 0.4500000000000000111, 0.4541666666666666630, 0.4583333333333333148, 0.4625000000000000222, 0.4666666666666666741, 0.4708333333333333259, 0.4749999999999999778, 0.4791666666666666852, 0.4833333333333333370, 0.4874999999999999889, 0.4916666666666666408, 0.4958333333333333481, 0.5000000000000000000, 0.5041666666666666519, 0.5083333333333333037, 0.5124999999999999556, 0.5166666666666667185, 0.5208333333333333703, 0.5250000000000000222, 0.5291666666666666741, 0.5333333333333333259, 0.5374999999999999778, 0.5416666666666666297, 0.5458333333333332815, 0.5500000000000000444, 0.5541666666666666963, 0.5583333333333333481, 0.5625000000000000000, 0.5666666666666666519, 0.5708333333333333037, 0.5749999999999999556, 0.5791666666666667185, 0.5833333333333333703, 0.5875000000000000222, 0.5916666666666666741, 0.5958333333333333259, 0.5999999999999999778, 0.6041666666666666297, 0.6083333333333332815, 0.6125000000000000444, 0.6166666666666666963, 0.6208333333333333481, 0.6250000000000000000, 0.6291666666666666519, 0.6333333333333333037, 0.6374999999999999556, 0.6416666666666667185, 0.6458333333333333703, 0.6500000000000000222, 0.6541666666666666741, 0.6583333333333333259, 0.6624999999999999778, 0.6666666666666666297, 0.6708333333333332815, 0.6750000000000000444, 0.6791666666666666963, 0.6833333333333333481, 0.6875000000000000000, 0.6916666666666666519, 0.6958333333333333037, 0.6999999999999999556, 0.7041666666666667185, 0.7083333333333333703, 0.7125000000000000222, 0.7166666666666666741, 0.7208333333333333259, 0.7249999999999999778, 0.7291666666666666297, 0.7333333333333332815, 0.7375000000000000444, 0.7416666666666666963, 0.7458333333333333481, 0.7500000000000000000, 0.7541666666666666519, 0.7583333333333333037, 0.7624999999999999556, 0.7666666666666667185, 0.7708333333333333703, 0.7750000000000000222, 0.7791666666666666741, 0.7833333333333333259, 0.7874999999999999778, 0.7916666666666666297, 0.7958333333333332815, 0.8000000000000000444, 0.8041666666666666963, 0.8083333333333333481, 0.8125000000000000000, 0.8166666666666666519, 0.8208333333333333037, 0.8249999999999999556, 0.8291666666666667185, 0.8333333333333333703, 0.8375000000000000222, 0.8416666666666666741, 0.8458333333333333259, 0.8499999999999999778, 0.8541666666666666297, 0.8583333333333332815, 0.8625000000000000444, 0.8666666666666666963, 0.8708333333333333481, 0.8750000000000000000, 0.8791666666666666519, 0.8833333333333333037, 0.8874999999999999556, 0.8916666666666667185, 0.8958333333333333703, 0.9000000000000000222, 0.9041666666666666741, 0.9083333333333333259, 0.9124999999999999778, 0.9166666666666666297, 0.9208333333333332815, 0.9250000000000000444, 0.9291666666666666963, 0.9333333333333333481, 0.9375000000000000000, 0.9416666666666666519, 0.9458333333333333037, 0.9499999999999999556, 0.9541666666666667185, 0.9583333333333333703, 0.9625000000000000222, 0.9666666666666666741, 0.9708333333333333259, 0.9749999999999999778, 0.9791666666666666297, 0.9833333333333332815, 0.9875000000000000444, 0.9916666666666666963, 0.9958333333333333481, 1.000000000000000000 ),
 .UNSPECIFIED. ) 
 GEOMETRIC_REPRESENTATION_ITEM ( )  RATIONAL_B_SPLINE_SURFACE ( (
 ( 1.000000000000000000, 0.8660254037844387076, 1.000000000000000000, 0.8660254037844387076, 1.000000000000000000, 0.8660254037844387076, 1.000000000000000000, 0.8660254037844387076, 1.000000000000000000, 0.8660254037844387076, 1.000000000000000000, 0.8660254037844387076, 1.000000000000000000, 0.8660254037844387076, 1.000000000000000000, 0.8660254037844387076, 1.000000000000000000, 0.8660254037844387076, 1.000000000000000000, 0.8660254037844387076, 1.000000000000000000, 0.8660254037844387076, 1.000000000000000000, 0.8660254037844387076, 1.000000000000000000, 0.8660254037844387076, 1.000000000000000000, 0.8660254037844387076, 1.000000000000000000, 0.8660254037844387076, 1.000000000000000000, 0.8660254037844387076, 1.000000000000000000, 0.8660254037844387076, 1.000000000000000000, 0.8660254037844387076, 1.000000000000000000, 0.8660254037844387076, 1.000000000000000000, 0.8660254037844387076, 1.000000000000000000, 0.8660254037844387076, 1.000000000000000000, 0.8660254037844387076, 1.000000000000000000, 0.8660254037844387076, 1.000000000000000000, 0.8660254037844387076, 1.000000000000000000, 0.8660254037844387076, 1.000000000000000000, 0.8660254037844387076, 1.000000000000000000, 0.8660254037844387076, 1.000000000000000000, 0.8660254037844387076, 1.000000000000000000, 0.8660254037844387076, 1.000000000000000000, 0.8660254037844387076, 1.000000000000000000, 0.8660254037844387076, 1.000000000000000000, 0.8660254037844387076, 1.000000000000000000, 0.8660254037844387076, 1.000000000000000000, 0.8660254037844387076, 1.000000000000000000, 0.8660254037844387076, 1.000000000000000000, 0.8660254037844387076, 1.000000000000000000, 0.8660254037844387076, 1.000000000000000000, 0.8660254037844387076, 1.000000000000000000, 0.8660254037844387076, 1.000000000000000000, 0.8660254037844387076, 1.000000000000000000, 0.8660254037844387076, 1.000000000000000000, 0.8660254037844387076, 1.000000000000000000, 0.8660254037844387076, 1.000000000000000000, 0.8660254037844387076, 1.000000000000000000, 0.8660254037844387076, 1.000000000000000000, 0.8660254037844387076, 1.000000000000000000, 0.8660254037844387076, 1.000000000000000000, 0.8660254037844387076, 1.000000000000000000, 0.8660254037844387076, 1.000000000000000000, 0.8660254037844387076, 1.000000000000000000, 0.8660254037844387076, 1.000000000000000000, 0.8660254037844387076, 1.000000000000000000, 0.8660254037844387076, 1.000000000000000000, 0.8660254037844387076, 1.000000000000000000, 0.8660254037844387076, 1.000000000000000000, 0.8660254037844387076, 1.000000000000000000, 0.8660254037844387076, 1.000000000000000000, 0.8660254037844387076, 1.000000000000000000, 0.8660254037844387076, 1.000000000000000000, 0.8660254037844387076, 1.000000000000000000, 0.8660254037844387076, 1.000000000000000000, 0.8660254037844387076, 1.000000000000000000, 0.8660254037844387076, 1.000000000000000000, 0.8660254037844387076, 1.000000000000000000, 0.8660254037844387076, 1.000000000000000000, 0.8660254037844387076, 1.000000000000000000, 0.8660254037844387076, 1.000000000000000000, 0.8660254037844387076, 1.000000000000000000, 0.8660254037844387076, 1.000000000000000000, 0.8660254037844387076, 1.000000000000000000, 0.8660254037844387076, 1.000000000000000000, 0.8660254037844387076, 1.000000000000000000, 0.8660254037844387076, 1.000000000000000000, 0.8660254037844387076, 1.000000000000000000, 0.8660254037844387076, 1.000000000000000000, 0.8660254037844387076, 1.000000000000000000, 0.8660254037844387076, 1.000000000000000000, 0.8660254037844387076, 1.000000000000000000, 0.8660254037844387076, 1.000000000000000000, 0.8660254037844387076, 1.000000000000000000, 0.8660254037844387076, 1.000000000000000000, 0.8660254037844387076, 1.000000000000000000, 0.8660254037844387076, 1.000000000000000000, 0.8660254037844387076, 1.000000000000000000, 0.8660254037844387076, 1.000000000000000000, 0.8660254037844387076, 1.000000000000000000, 0.8660254037844387076, 1.000000000000000000, 0.8660254037844387076, 1.000000000000000000, 0.8660254037844387076, 1.000000000000000000, 0.8660254037844387076, 1.000000000000000000, 0.8660254037844387076, 1.000000000000000000, 0.8660254037844387076, 1.000000000000000000, 0.8660254037844387076, 1.000000000000000000, 0.8660254037844387076, 1.000000000000000000, 0.8660254037844387076, 1.000000000000000000, 0.8660254037844387076, 1.000000000000000000, 0.8660254037844387076, 1.000000000000000000, 0.8660254037844387076, 1.000000000000000000, 0.8660254037844387076, 1.000000000000000000, 0.8660254037844387076, 1.000000000000000000, 0.8660254037844387076, 1.000000000000000000, 0.8660254037844387076, 1.000000000000000000, 0.8660254037844387076, 1.000000000000000000, 0.8660254037844387076, 1.000000000000000000, 0.8660254037844387076, 1.000000000000000000, 0.8660254037844387076, 1.000000000000000000, 0.8660254037844387076, 1.000000000000000000, 0.8660254037844387076, 1.000000000000000000, 0.8660254037844387076, 1.000000000000000000, 0.8660254037844387076, 1.000000000000000000, 0.8660254037844387076, 1.000000000000000000, 0.8660254037844387076, 1.000000000000000000, 0.8660254037844387076, 1.000000000000000000, 0.8660254037844387076, 1.000000000000000000, 0.8660254037844387076, 1.000000000000000000, 0.8660254037844387076, 1.000000000000000000, 0.8660254037844387076, 1.000000000000000000, 0.8660254037844387076, 1.000000000000000000, 0.8660254037844387076, 1.000000000000000000, 0.8660254037844387076, 1.000000000000000000, 0.8660254037844387076, 1.000000000000000000, 0.8660254037844387076, 1.000000000000000000, 0.8660254037844387076, 1.000000000000000000, 0.8660254037844387076, 1.000000000000000000, 0.8660254037844387076, 1.000000000000000000, 0.8660254037844387076, 1.000000000000000000, 0.8660254037844387076, 1.000000000000000000, 0.8660254037844387076, 1.000000000000000000, 0.8660254037844387076, 1.000000000000000000, 0.8660254037844387076, 1.000000000000000000, 0.8660254037844387076, 1.000000000000000000, 0.8660254037844387076, 1.000000000000000000, 0.8660254037844387076, 1.000000000000000000, 0.8660254037844387076, 1.000000000000000000, 0.8660254037844387076, 1.000000000000000000, 0.8660254037844387076, 1.000000000000000000, 0.8660254037844387076, 1.000000000000000000, 0.8660254037844387076, 1.000000000000000000, 0.8660254037844387076, 1.000000000000000000, 0.8660254037844387076, 1.000000000000000000, 0.8660254037844387076, 1.000000000000000000, 0.8660254037844387076, 1.000000000000000000, 0.8660254037844387076, 1.000000000000000000, 0.8660254037844387076, 1.000000000000000000, 0.8660254037844387076, 1.000000000000000000, 0.8660254037844387076, 1.000000000000000000, 0.8660254037844387076, 1.000000000000000000, 0.8660254037844387076, 1.000000000000000000, 0.8660254037844387076, 1.000000000000000000, 0.8660254037844387076, 1.000000000000000000, 0.8660254037844387076, 1.000000000000000000, 0.8660254037844387076, 1.000000000000000000, 0.8660254037844387076, 1.000000000000000000, 0.8660254037844387076, 1.000000000000000000, 0.8660254037844387076, 1.000000000000000000, 0.8660254037844387076, 1.000000000000000000, 0.8660254037844387076, 1.000000000000000000, 0.8660254037844387076, 1.000000000000000000, 0.8660254037844387076, 1.000000000000000000, 0.8660254037844387076, 1.000000000000000000, 0.8660254037844387076, 1.000000000000000000, 0.8660254037844387076, 1.000000000000000000, 0.8660254037844387076, 1.000000000000000000, 0.8660254037844387076, 1.000000000000000000, 0.8660254037844387076, 1.000000000000000000, 0.8660254037844387076, 1.000000000000000000, 0.8660254037844387076, 1.000000000000000000, 0.8660254037844387076, 1.000000000000000000, 0.8660254037844387076, 1.000000000000000000, 0.8660254037844387076, 1.000000000000000000, 0.8660254037844387076, 1.000000000000000000, 0.8660254037844387076, 1.000000000000000000, 0.8660254037844387076, 1.000000000000000000, 0.8660254037844387076, 1.000000000000000000, 0.8660254037844387076, 1.000000000000000000, 0.8660254037844387076, 1.000000000000000000, 0.8660254037844387076, 1.000000000000000000, 0.8660254037844387076, 1.000000000000000000, 0.8660254037844387076, 1.000000000000000000, 0.8660254037844387076, 1.000000000000000000, 0.8660254037844387076, 1.000000000000000000, 0.8660254037844387076, 1.000000000000000000, 0.8660254037844387076, 1.000000000000000000, 0.8660254037844387076, 1.000000000000000000, 0.8660254037844387076, 1.000000000000000000, 0.8660254037844387076, 1.000000000000000000, 0.8660254037844387076, 1.000000000000000000, 0.8660254037844387076, 1.000000000000000000, 0.8660254037844387076, 1.000000000000000000, 0.8660254037844387076, 1.000000000000000000, 0.8660254037844387076, 1.000000000000000000, 0.8660254037844387076, 1.000000000000000000, 0.8660254037844387076, 1.000000000000000000, 0.8660254037844387076, 1.000000000000000000, 0.8660254037844387076, 1.000000000000000000, 0.8660254037844387076, 1.000000000000000000, 0.8660254037844387076, 1.000000000000000000, 0.8660254037844387076, 1.000000000000000000, 0.8660254037844387076, 1.000000000000000000, 0.8660254037844387076, 1.000000000000000000, 0.8660254037844387076, 1.000000000000000000, 0.8660254037844387076, 1.000000000000000000, 0.8660254037844387076, 1.000000000000000000, 0.8660254037844387076, 1.000000000000000000, 0.8660254037844387076, 1.000000000000000000, 0.8660254037844387076, 1.000000000000000000, 0.8660254037844387076, 1.000000000000000000, 0.8660254037844387076, 1.000000000000000000, 0.8660254037844387076, 1.000000000000000000, 0.8660254037844387076, 1.000000000000000000, 0.8660254037844387076, 1.000000000000000000, 0.8660254037844387076, 1.000000000000000000, 0.8660254037844387076, 1.000000000000000000, 0.8660254037844387076, 1.000000000000000000, 0.8660254037844387076, 1.000000000000000000, 0.8660254037844387076, 1.000000000000000000, 0.8660254037844387076, 1.000000000000000000, 0.8660254037844387076, 1.000000000000000000, 0.8660254037844387076, 1.000000000000000000, 0.8660254037844387076, 1.000000000000000000, 0.8660254037844387076, 1.000000000000000000, 0.8660254037844387076, 1.000000000000000000, 0.8660254037844387076, 1.000000000000000000, 0.8660254037844387076, 1.000000000000000000, 0.8660254037844387076, 1.000000000000000000, 0.8660254037844387076, 1.000000000000000000, 0.8660254037844387076, 1.000000000000000000, 0.8660254037844387076, 1.000000000000000000, 0.8660254037844387076, 1.000000000000000000, 0.8660254037844387076, 1.000000000000000000, 0.8660254037844387076, 1.000000000000000000, 0.8660254037844387076, 1.000000000000000000, 0.8660254037844387076, 1.000000000000000000, 0.8660254037844387076, 1.000000000000000000, 0.8660254037844387076, 1.000000000000000000, 0.8660254037844387076, 1.000000000000000000, 0.8660254037844387076, 1.000000000000000000, 0.8660254037844387076, 1.000000000000000000, 0.8660254037844387076, 1.000000000000000000, 0.8660254037844387076, 1.000000000000000000),
 ( 1.000000000000000000, 0.8660254037844387076, 1.000000000000000000, 0.8660254037844387076, 1.000000000000000000, 0.8660254037844387076, 1.000000000000000000, 0.8660254037844387076, 1.000000000000000000, 0.8660254037844387076, 1.000000000000000000, 0.8660254037844387076, 1.000000000000000000, 0.8660254037844387076, 1.000000000000000000, 0.8660254037844387076, 1.000000000000000000, 0.8660254037844387076, 1.000000000000000000, 0.8660254037844387076, 1.000000000000000000, 0.8660254037844387076, 1.000000000000000000, 0.8660254037844387076, 1.000000000000000000, 0.8660254037844387076, 1.000000000000000000, 0.8660254037844387076, 1.000000000000000000, 0.8660254037844387076, 1.000000000000000000, 0.8660254037844387076, 1.000000000000000000, 0.8660254037844387076, 1.000000000000000000, 0.8660254037844387076, 1.000000000000000000, 0.8660254037844387076, 1.000000000000000000, 0.8660254037844387076, 1.000000000000000000, 0.8660254037844387076, 1.000000000000000000, 0.8660254037844387076, 1.000000000000000000, 0.8660254037844387076, 1.000000000000000000, 0.8660254037844387076, 1.000000000000000000, 0.8660254037844387076, 1.000000000000000000, 0.8660254037844387076, 1.000000000000000000, 0.8660254037844387076, 1.000000000000000000, 0.8660254037844387076, 1.000000000000000000, 0.8660254037844387076, 1.000000000000000000, 0.8660254037844387076, 1.000000000000000000, 0.8660254037844387076, 1.000000000000000000, 0.8660254037844387076, 1.000000000000000000, 0.8660254037844387076, 1.000000000000000000, 0.8660254037844387076, 1.000000000000000000, 0.8660254037844387076, 1.000000000000000000, 0.8660254037844387076, 1.000000000000000000, 0.8660254037844387076, 1.000000000000000000, 0.8660254037844387076, 1.000000000000000000, 0.8660254037844387076, 1.000000000000000000, 0.8660254037844387076, 1.000000000000000000, 0.8660254037844387076, 1.000000000000000000, 0.8660254037844387076, 1.000000000000000000, 0.8660254037844387076, 1.000000000000000000, 0.8660254037844387076, 1.000000000000000000, 0.8660254037844387076, 1.000000000000000000, 0.8660254037844387076, 1.000000000000000000, 0.8660254037844387076, 1.000000000000000000, 0.8660254037844387076, 1.000000000000000000, 0.8660254037844387076, 1.000000000000000000, 0.8660254037844387076, 1.000000000000000000, 0.8660254037844387076, 1.000000000000000000, 0.8660254037844387076, 1.000000000000000000, 0.8660254037844387076, 1.000000000000000000, 0.8660254037844387076, 1.000000000000000000, 0.8660254037844387076, 1.000000000000000000, 0.8660254037844387076, 1.000000000000000000, 0.8660254037844387076, 1.000000000000000000, 0.8660254037844387076, 1.000000000000000000, 0.8660254037844387076, 1.000000000000000000, 0.8660254037844387076, 1.000000000000000000, 0.8660254037844387076, 1.000000000000000000, 0.8660254037844387076, 1.000000000000000000, 0.8660254037844387076, 1.000000000000000000, 0.8660254037844387076, 1.000000000000000000, 0.8660254037844387076, 1.000000000000000000, 0.8660254037844387076, 1.000000000000000000, 0.8660254037844387076, 1.000000000000000000, 0.8660254037844387076, 1.000000000000000000, 0.8660254037844387076, 1.000000000000000000, 0.8660254037844387076, 1.000000000000000000, 0.8660254037844387076, 1.000000000000000000, 0.8660254037844387076, 1.000000000000000000, 0.8660254037844387076, 1.000000000000000000, 0.8660254037844387076, 1.000000000000000000, 0.8660254037844387076, 1.000000000000000000, 0.8660254037844387076, 1.000000000000000000, 0.8660254037844387076, 1.000000000000000000, 0.8660254037844387076, 1.000000000000000000, 0.8660254037844387076, 1.000000000000000000, 0.8660254037844387076, 1.000000000000000000, 0.8660254037844387076, 1.000000000000000000, 0.8660254037844387076, 1.000000000000000000, 0.8660254037844387076, 1.000000000000000000, 0.8660254037844387076, 1.000000000000000000, 0.8660254037844387076, 1.000000000000000000, 0.8660254037844387076, 1.000000000000000000, 0.8660254037844387076, 1.000000000000000000, 0.8660254037844387076, 1.000000000000000000, 0.8660254037844387076, 1.000000000000000000, 0.8660254037844387076, 1.000000000000000000, 0.8660254037844387076, 1.000000000000000000, 0.8660254037844387076, 1.000000000000000000, 0.8660254037844387076, 1.000000000000000000, 0.8660254037844387076, 1.000000000000000000, 0.8660254037844387076, 1.000000000000000000, 0.8660254037844387076, 1.000000000000000000, 0.8660254037844387076, 1.000000000000000000, 0.8660254037844387076, 1.000000000000000000, 0.8660254037844387076, 1.000000000000000000, 0.8660254037844387076, 1.000000000000000000, 0.8660254037844387076, 1.000000000000000000, 0.8660254037844387076, 1.000000000000000000, 0.8660254037844387076, 1.000000000000000000, 0.8660254037844387076, 1.000000000000000000, 0.8660254037844387076, 1.000000000000000000, 0.8660254037844387076, 1.000000000000000000, 0.8660254037844387076, 1.000000000000000000, 0.8660254037844387076, 1.000000000000000000, 0.8660254037844387076, 1.000000000000000000, 0.8660254037844387076, 1.000000000000000000, 0.8660254037844387076, 1.000000000000000000, 0.8660254037844387076, 1.000000000000000000, 0.8660254037844387076, 1.000000000000000000, 0.8660254037844387076, 1.000000000000000000, 0.8660254037844387076, 1.000000000000000000, 0.8660254037844387076, 1.000000000000000000, 0.8660254037844387076, 1.000000000000000000, 0.8660254037844387076, 1.000000000000000000, 0.8660254037844387076, 1.000000000000000000, 0.8660254037844387076, 1.000000000000000000, 0.8660254037844387076, 1.000000000000000000, 0.8660254037844387076, 1.000000000000000000, 0.8660254037844387076, 1.000000000000000000, 0.8660254037844387076, 1.000000000000000000, 0.8660254037844387076, 1.000000000000000000, 0.8660254037844387076, 1.000000000000000000, 0.8660254037844387076, 1.000000000000000000, 0.8660254037844387076, 1.000000000000000000, 0.8660254037844387076, 1.000000000000000000, 0.8660254037844387076, 1.000000000000000000, 0.8660254037844387076, 1.000000000000000000, 0.8660254037844387076, 1.000000000000000000, 0.8660254037844387076, 1.000000000000000000, 0.8660254037844387076, 1.000000000000000000, 0.8660254037844387076, 1.000000000000000000, 0.8660254037844387076, 1.000000000000000000, 0.8660254037844387076, 1.000000000000000000, 0.8660254037844387076, 1.000000000000000000, 0.8660254037844387076, 1.000000000000000000, 0.8660254037844387076, 1.000000000000000000, 0.8660254037844387076, 1.000000000000000000, 0.8660254037844387076, 1.000000000000000000, 0.8660254037844387076, 1.000000000000000000, 0.8660254037844387076, 1.000000000000000000, 0.8660254037844387076, 1.000000000000000000, 0.8660254037844387076, 1.000000000000000000, 0.8660254037844387076, 1.000000000000000000, 0.8660254037844387076, 1.000000000000000000, 0.8660254037844387076, 1.000000000000000000, 0.8660254037844387076, 1.000000000000000000, 0.8660254037844387076, 1.000000000000000000, 0.8660254037844387076, 1.000000000000000000, 0.8660254037844387076, 1.000000000000000000, 0.8660254037844387076, 1.000000000000000000, 0.8660254037844387076, 1.000000000000000000, 0.8660254037844387076, 1.000000000000000000, 0.8660254037844387076, 1.000000000000000000, 0.8660254037844387076, 1.000000000000000000, 0.8660254037844387076, 1.000000000000000000, 0.8660254037844387076, 1.000000000000000000, 0.8660254037844387076, 1.000000000000000000, 0.8660254037844387076, 1.000000000000000000, 0.8660254037844387076, 1.000000000000000000, 0.8660254037844387076, 1.000000000000000000, 0.8660254037844387076, 1.000000000000000000, 0.8660254037844387076, 1.000000000000000000, 0.8660254037844387076, 1.000000000000000000, 0.8660254037844387076, 1.000000000000000000, 0.8660254037844387076, 1.000000000000000000, 0.8660254037844387076, 1.000000000000000000, 0.8660254037844387076, 1.000000000000000000, 0.8660254037844387076, 1.000000000000000000, 0.8660254037844387076, 1.000000000000000000, 0.8660254037844387076, 1.000000000000000000, 0.8660254037844387076, 1.000000000000000000, 0.8660254037844387076, 1.000000000000000000, 0.8660254037844387076, 1.000000000000000000, 0.8660254037844387076, 1.000000000000000000, 0.8660254037844387076, 1.000000000000000000, 0.8660254037844387076, 1.000000000000000000, 0.8660254037844387076, 1.000000000000000000, 0.8660254037844387076, 1.000000000000000000, 0.8660254037844387076, 1.000000000000000000, 0.8660254037844387076, 1.000000000000000000, 0.8660254037844387076, 1.000000000000000000, 0.8660254037844387076, 1.000000000000000000, 0.8660254037844387076, 1.000000000000000000, 0.8660254037844387076, 1.000000000000000000, 0.8660254037844387076, 1.000000000000000000, 0.8660254037844387076, 1.000000000000000000, 0.8660254037844387076, 1.000000000000000000, 0.8660254037844387076, 1.000000000000000000, 0.8660254037844387076, 1.000000000000000000, 0.8660254037844387076, 1.000000000000000000, 0.8660254037844387076, 1.000000000000000000, 0.8660254037844387076, 1.000000000000000000, 0.8660254037844387076, 1.000000000000000000, 0.8660254037844387076, 1.000000000000000000, 0.8660254037844387076, 1.000000000000000000, 0.8660254037844387076, 1.000000000000000000, 0.8660254037844387076, 1.000000000000000000, 0.8660254037844387076, 1.000000000000000000, 0.8660254037844387076, 1.000000000000000000, 0.8660254037844387076, 1.000000000000000000, 0.8660254037844387076, 1.000000000000000000, 0.8660254037844387076, 1.000000000000000000, 0.8660254037844387076, 1.000000000000000000, 0.8660254037844387076, 1.000000000000000000, 0.8660254037844387076, 1.000000000000000000, 0.8660254037844387076, 1.000000000000000000, 0.8660254037844387076, 1.000000000000000000, 0.8660254037844387076, 1.000000000000000000, 0.8660254037844387076, 1.000000000000000000, 0.8660254037844387076, 1.000000000000000000, 0.8660254037844387076, 1.000000000000000000, 0.8660254037844387076, 1.000000000000000000, 0.8660254037844387076, 1.000000000000000000, 0.8660254037844387076, 1.000000000000000000, 0.8660254037844387076, 1.000000000000000000, 0.8660254037844387076, 1.000000000000000000, 0.8660254037844387076, 1.000000000000000000, 0.8660254037844387076, 1.000000000000000000, 0.8660254037844387076, 1.000000000000000000, 0.8660254037844387076, 1.000000000000000000, 0.8660254037844387076, 1.000000000000000000, 0.8660254037844387076, 1.000000000000000000, 0.8660254037844387076, 1.000000000000000000, 0.8660254037844387076, 1.000000000000000000, 0.8660254037844387076, 1.000000000000000000, 0.8660254037844387076, 1.000000000000000000, 0.8660254037844387076, 1.000000000000000000, 0.8660254037844387076, 1.000000000000000000, 0.8660254037844387076, 1.000000000000000000, 0.8660254037844387076, 1.000000000000000000, 0.8660254037844387076, 1.000000000000000000, 0.8660254037844387076, 1.000000000000000000, 0.8660254037844387076, 1.000000000000000000, 0.8660254037844387076, 1.000000000000000000, 0.8660254037844387076, 1.000000000000000000, 0.8660254037844387076, 1.000000000000000000) ) ) 
 REPRESENTATION_ITEM ( '' )  SURFACE ( )  );
#89276 = CARTESIAN_POINT ( 'NONE',  ( 2.618384893494442256, 1.290362544248652599, -1.490430290494165755 ) ) ;
#89277 = CARTESIAN_POINT ( 'NONE',  ( 4.341997288149157086, -1.180789491531178292, -1.504210074635865757 ) ) ;
#89278 = ORIENTED_EDGE ( 'NONE', *, *, #3774, .T. ) ;
#89279 = CARTESIAN_POINT ( 'NONE',  ( -1.797304815382257948, 14.48004927659174257, -11.89862588508291275 ) ) ;
#89280 = CARTESIAN_POINT ( 'NONE',  ( 5.178159682156908694, -1.051918566972683600, -1.664904379343169705 ) ) ;
#89281 = CARTESIAN_POINT ( 'NONE',  ( 0.7088029311262042942, -0.2857661853880436031, 1.920690660100693226 ) ) ;
#89282 = VERTEX_POINT ( 'NONE', #207794 ) ;
#89283 = CARTESIAN_POINT ( 'NONE',  ( -4.586401103172829785, 8.572828063668767484, 0.7998128361456281477 ) ) ;
#89285 = CARTESIAN_POINT ( 'NONE',  ( 6.828399852920184365, -6.891066458783410731, -6.756361134959164794 ) ) ;
#89284 = CARTESIAN_POINT ( 'NONE',  ( -3.447516199624892419, 7.244129009529488350, 0.7998128361456352531 ) ) ;
#89286 = CARTESIAN_POINT ( 'NONE',  ( 4.678972410047582464, 8.472901888448573615, -0.7216878364870357165 ) ) ;
#89287 = ORIENTED_EDGE ( 'NONE', *, *, #129217, .T. ) ;
#89288 = CARTESIAN_POINT ( 'NONE',  ( 0.6576010401811819284, -1.865379905010958517, -1.178792301215730642 ) ) ;
#89289 = CARTESIAN_POINT ( 'NONE',  ( 7.462104991928525166, -5.200000000000006395, 8.081892667527540652 ) ) ;
#89290 = CARTESIAN_POINT ( 'NONE',  ( -0.07574839183086683192, -0.8175154495408327726, -1.727131953450977253 ) ) ;
#89291 = CARTESIAN_POINT ( 'NONE',  ( 0.07661050522430808141, 2.897279719329011627, -2.199986835335824953 ) ) ;
#89293 = CARTESIAN_POINT ( 'NONE',  ( 5.717982508692024624, 0.9896897593998502662, -1.756851901128737348 ) ) ;
#89292 = CARTESIAN_POINT ( 'NONE',  ( -5.721691974912406664, 7.393287073457107894, 1.332251608056257641 ) ) ;
#89294 = CARTESIAN_POINT ( 'NONE',  ( 1.943885480841448965, 1.426152643941134501, 1.501071833787496645 ) ) ;
#89295 = CARTESIAN_POINT ( 'NONE',  ( -6.575868197828002693, 7.630599971342813426, 1.199719254218450271 ) ) ;
#89296 = CARTESIAN_POINT ( 'NONE',  ( -4.940673843451318881, 7.995311821131723562, 1.007273293859496155 ) ) ;
#89297 = CARTESIAN_POINT ( 'NONE',  ( 0.3390366800232989530, 0.3710982241871863541, 2.129449491308422537 ) ) ;
#89298 =( LENGTH_UNIT ( ) NAMED_UNIT ( * ) SI_UNIT ( .MILLI., .METRE. ) );
#89299 = B_SPLINE_CURVE_WITH_KNOTS ( 'NONE', 3,
 ( #110379, #140720, #127720, #177447, #206734, #94086, #12783 ),
 .UNSPECIFIED., .F., .F.,
 ( 4, 3, 4 ),
 ( 0.000000000000000000, 0.0008000000000004425012, 0.002977368225425632356 ),
 .UNSPECIFIED. ) ;
#89300 = CARTESIAN_POINT ( 'NONE',  ( 5.234856708652233515, 6.240325927249993576, 1.082531754730549078 ) ) ;
#89301 = CARTESIAN_POINT ( 'NONE',  ( -0.4465194593918104249, 3.080450244942120719, -0.4155024747329819634 ) ) ;
#89302 = CARTESIAN_POINT ( 'NONE',  ( 1.364683531249996529, 12.77604166700806587, 0.7879004041258405033 ) ) ;
#89304 = CARTESIAN_POINT ( 'NONE',  ( -6.363572996767778100, 8.517530811019446091, -1.599625672291271394 ) ) ;
#89303 = CARTESIAN_POINT ( 'NONE',  ( 6.825078400183572036, 7.053423702906556514, 2.353807037893948628 ) ) ;
#89305 = CARTESIAN_POINT ( 'NONE',  ( 4.588316246536889409, -0.4565669943805070186, 1.672893389497135841 ) ) ;
#89306 = CARTESIAN_POINT ( 'NONE',  ( -4.762992037102518950, 4.451245552908022596, -0.7998128361456221525 ) ) ;
#89308 = AXIS2_PLACEMENT_3D ( 'NONE', #118942, #54947, #185991 ) ;
#89307 = AXIS2_PLACEMENT_3D ( 'NONE', #171103, #42199, #37911 ) ;
#89309 = CARTESIAN_POINT ( 'NONE',  ( 2.553653463975919635, 1.597511423921485818, 1.316731848974454833 ) ) ;
#89310 = CARTESIAN_POINT ( 'NONE',  ( 4.833676624637527119, 0.6627930923091308602, -2.010898772050497829 ) ) ;
#89311 = CARTESIAN_POINT ( 'NONE',  ( 7.182068686937156166, 9.402166106225269715, 1.599625672291281386 ) ) ;
#89312 = CARTESIAN_POINT ( 'NONE',  ( -1.201851678989727383E-14, 3.446875000341421469, -1.575800808251660134 ) ) ;
#89313 = CARTESIAN_POINT ( 'NONE',  ( 1.481237898015239418, -0.05359582033081673746, 1.968903824098491073 ) ) ;
#89314 = CARTESIAN_POINT ( 'NONE',  ( 6.067506501917478090, 6.045351875519452634, 0.3962785553160239616 ) ) ;
#89315 = CARTESIAN_POINT ( 'NONE',  ( 11.92619526913699879, 12.57218333338757077, -1.328859060402686199 ) ) ;
#89316 = CARTESIAN_POINT ( 'NONE',  ( 4.523529124507605914, -1.408076564469705527, -1.808723714663774240 ) ) ;
#89317 = CARTESIAN_POINT ( 'NONE',  ( 1.295219883412350503, 1.381147610352757127, 1.194082977437810333 ) ) ;
#89318 = CARTESIAN_POINT ( 'NONE',  ( 5.879395890181562834, 6.888325289080478697, -1.199719254218452047 ) ) ;
#89319 = CARTESIAN_POINT ( 'NONE',  ( 4.324687812634874895, 7.989293514808604613, 0.7216878364870317197 ) ) ;
#89320 = CARTESIAN_POINT ( 'NONE',  ( -7.751511138711140170, 10.06651563329490529, -1.599625672291263179 ) ) ;
#89321 = CARTESIAN_POINT ( 'NONE',  ( 2.672137747239998529, 2.003105221038860684, -0.2016864653290161569 ) ) ;
#89322 = CARTESIAN_POINT ( 'NONE',  ( 3.414850490325722632, -1.488543670003231068, 1.277929504599809585 ) ) ;
#89323 = CARTESIAN_POINT ( 'NONE',  ( -7.971304249830880373, 11.38727316052296601, 1.199719254218453823 ) ) ;
#89324 = CARTESIAN_POINT ( 'NONE',  ( -5.052384799386910430, 9.046199365926717917, 1.214306433183764966E-14 ) ) ;
#89325 = CARTESIAN_POINT ( 'NONE',  ( 0.000000000000000000, 5.499999999999998224, 0.000000000000000000 ) ) ;
#89327 = CARTESIAN_POINT ( 'NONE',  ( 4.293650081035056409, -0.6766669130573493840, 1.635584247362771304 ) ) ;
#89326 = CARTESIAN_POINT ( 'NONE',  ( 5.964805764622640005, 0.1547682761293242837, -2.084958343724970131 ) ) ;
#89328 = ADVANCED_FACE ( 'NONE', ( #143921 ), #173201, .T. ) ;
#89329 = CARTESIAN_POINT ( 'NONE',  ( 1.113517231965298837, -2.137359700923711081, 0.4831916906855234228 ) ) ;
#89330 = CARTESIAN_POINT ( 'NONE',  ( 5.542807930227759527, -1.375536301258666105, -1.066015508636003251 ) ) ;
#89331 = CARTESIAN_POINT ( 'NONE',  ( 8.938903350111612411, 9.323142084752035430, -0.7998128361456221525 ) ) ;
#89332 = CARTESIAN_POINT ( 'NONE',  ( -2.155383234892699562, 5.458438174109348395, 1.040834085586084257E-14 ) ) ;
#89333 = CARTESIAN_POINT ( 'NONE',  ( 6.276074014454348315, 2.002121775873589637, -1.129333029253890341 ) ) ;
#89334 = CARTESIAN_POINT ( 'NONE',  ( -10.44369633504468631, 5.112959841837461994, -5.232137017608345708 ) ) ;
#89335 = CARTESIAN_POINT ( 'NONE',  ( 6.098968314571592053, 0.8511620794300640558, -1.510462927660038090 ) ) ;
#89336 = CARTESIAN_POINT ( 'NONE',  ( 1.717678464306471309, -0.2677704892378242607, 2.190511422692428045 ) ) ;
#89337 = AXIS2_PLACEMENT_3D ( 'NONE', #106093, #205656, #90876 ) ;
#89338 = CARTESIAN_POINT ( 'NONE',  ( 5.424361751532248199, 1.065549429306617446, 1.891644033573415040 ) ) ;
#89339 = CARTESIAN_POINT ( 'NONE',  ( -3.511198596259295535, 6.271927390929313617, -2.420000000000000373 ) ) ;
#89340 = CARTESIAN_POINT ( 'NONE',  ( 0.9193374879241524855, -1.911445915896703207, 0.9111208566532496000 ) ) ;
#89341 = CARTESIAN_POINT ( 'NONE',  ( 4.125000000000001776, -2.052068128417945392, 2.349217982248014418E-13 ) ) ;
#89342 = CARTESIAN_POINT ( 'NONE',  ( 6.827182134110167055, 4.690515317746113411, 2.651606140002475076 ) ) ;
#89343 = CARTESIAN_POINT ( 'NONE',  ( 4.647439542507147081, -1.488915335790324201, -1.222320866314072774 ) ) ;
#89344 = CARTESIAN_POINT ( 'NONE',  ( 1.559560479473407701, -1.874198601735496794, 1.192037787016706485 ) ) ;
#89345 = ORIENTED_EDGE ( 'NONE', *, *, #94477, .F. ) ;
#89346 = CARTESIAN_POINT ( 'NONE',  ( -1.201851678989727383E-14, 3.837500000000021227, -1.732050807568863648 ) ) ;
#89347 = CARTESIAN_POINT ( 'NONE',  ( 4.822949958159288286, 6.649860922651058992, -1.599625672291256295 ) ) ;
#89348 = CARTESIAN_POINT ( 'NONE',  ( 4.306686350635271054, 8.176217842383143974, -0.7998128361456221525 ) ) ;
#89349 = CIRCLE ( 'NONE', #210390, 0.08000000000000040412 ) ;
#89350 = CARTESIAN_POINT ( 'NONE',  ( 3.528187740469524769, -2.188240134182100949, 0.3810097408954765119 ) ) ;
#89351 = CARTESIAN_POINT ( 'NONE',  ( -8.839552966430023417, 9.415159337030921449, -0.7216878364870267237 ) ) ;
#89352 = CARTESIAN_POINT ( 'NONE',  ( 5.775410249741494972, 8.721433810464993996, -1.082531754730537088 ) ) ;
#89353 = CARTESIAN_POINT ( 'NONE',  ( -7.958272981097355370, 12.22847621134819285, 0.7216878364870458196 ) ) ;
#89354 = CARTESIAN_POINT ( 'NONE',  ( 5.560252395380206103, 8.540692657035327429, 1.082531754730547524 ) ) ;
#89355 = ORIENTED_EDGE ( 'NONE', *, *, #52718, .T. ) ;
#89356 = CARTESIAN_POINT ( 'NONE',  ( 2.197888892816081796, 1.802417619043535701, 0.9041091288993635677 ) ) ;
#89358 = CARTESIAN_POINT ( 'NONE',  ( 0.3563950589157930393, -2.062029646941070382, -0.05432448973826872057 ) ) ;
#89357 = CARTESIAN_POINT ( 'NONE',  ( 8.697719238366680372, 10.10609285197134533, 1.199719254218462483 ) ) ;
#89359 = CARTESIAN_POINT ( 'NONE',  ( -10.99180900346419243, -6.701306620466445985, 0.4265819271708525262 ) ) ;
#89360 = CARTESIAN_POINT ( 'NONE',  ( 7.065207446052794715, 9.336104335185329006, -1.443375672974064550 ) ) ;
#89361 = CARTESIAN_POINT ( 'NONE',  ( 0.2394788589213901198, 1.836227513651207177, 0.1364553164684492448 ) ) ;
#89362 =( NAMED_UNIT ( * ) PLANE_ANGLE_UNIT ( ) SI_UNIT ( $, .RADIAN. ) );
#89363 = CARTESIAN_POINT ( 'NONE',  ( 0.6823417656249882723, 1.926041667008083991, -1.181850606188749264 ) ) ;
#89364 = CARTESIAN_POINT ( 'NONE',  ( 1.739140684745379195, -1.277452191371928558, -1.225025713498065549 ) ) ;
#89365 = CARTESIAN_POINT ( 'NONE',  ( 0.5982800022500452952, -0.2930678230431381648, 1.994870242743536304 ) ) ;
#89366 = CARTESIAN_POINT ( 'NONE',  ( 6.392160974223673797, -0.4739405955596608933, -1.674609590779071455 ) ) ;
#89367 = CARTESIAN_POINT ( 'NONE',  ( 4.476316811684385222, -2.223409025971525121, -0.5576598666321966880 ) ) ;
#89368 = CARTESIAN_POINT ( 'NONE',  ( 3.609164914601064922, -1.813629950718143702, 0.3161406477080672128 ) ) ;
#89369 = CARTESIAN_POINT ( 'NONE',  ( 9.043452155515161905, 10.50944792197790889, 1.199719254218453823 ) ) ;
#89370 = CARTESIAN_POINT ( 'NONE',  ( 2.625780896952558674, -1.049238153381076177, -1.493741879923994542 ) ) ;
#89371 = CARTESIAN_POINT ( 'NONE',  ( 3.692029868468839737, 1.730865839653324079, 1.034166058993556181 ) ) ;
#89372 = CARTESIAN_POINT ( 'NONE',  ( -8.829384350997580455, 11.32403438096243775, 1.599625672291269396 ) ) ;
#89374 = CARTESIAN_POINT ( 'NONE',  ( 8.523031442321446605, 14.76712986476217715, -9.394111251778250349 ) ) ;
#89373 = CARTESIAN_POINT ( 'NONE',  ( 3.503020383517113423, 1.785049946035693891, -1.390086647613536952 ) ) ;
#89375 = CARTESIAN_POINT ( 'NONE',  ( 5.245193717270952405, -1.807841653007141947, 1.079916013355223248 ) ) ;
#89376 = CARTESIAN_POINT ( 'NONE',  ( 9.180878539475957112, 14.08084533201349586, 6.958356306020501592 ) ) ;
#89377 = CARTESIAN_POINT ( 'NONE',  ( 3.684089399883890614, -1.230936008959164996, -1.664559344884769088 ) ) ;
#89378 = CARTESIAN_POINT ( 'NONE',  ( 8.380911511541880188, 12.92948053010758258, 0.7998128361456462443 ) ) ;
#89379 = CARTESIAN_POINT ( 'NONE',  ( -0.6801582343750282034, 0.4635416670080716450, 1.178068619123793015 ) ) ;
#89380 = CARTESIAN_POINT ( 'NONE',  ( 5.848313825214911610, 1.045240856298999432, -1.844880668361434939 ) ) ;
#89381 = ITEM_DEFINED_TRANSFORMATION ( 'NONE', 'NONE', #62517,  #200407 ) ;
#89383 = CARTESIAN_POINT ( 'NONE',  ( 1.242661541247750856, 0.3750627104036097781, 1.889477121596821352 ) ) ;
#89382 = CARTESIAN_POINT ( 'NONE',  ( -8.910733272679575379, 11.41894145625809820, -1.599625672291263179 ) ) ;
#89384 = CARTESIAN_POINT ( 'NONE',  ( -4.787964524281469458, 5.614988695530339413, -1.199719254218453823 ) ) ;
#89385 = CARTESIAN_POINT ( 'NONE',  ( 7.747594715205354809, 11.12627870345989756, -1.199719254218446718 ) ) ;
#89386 = CARTESIAN_POINT ( 'NONE',  ( 4.190878879955609371, 7.903459436674603822, -0.7216878364870338292 ) ) ;
#89387 = CARTESIAN_POINT ( 'NONE',  ( 5.197613018050254219, 6.434050360596694773, 1.175743713691650871 ) ) ;
#89388 = CARTESIAN_POINT ( 'NONE',  ( 1.257539916218596732, 3.283837156058347251, -0.7749999999999874767 ) ) ;
#89389 = PRESENTATION_LAYER_ASSIGNMENT (  '', '', ( #96360 ) ) ;
#89390 = CARTESIAN_POINT ( 'NONE',  ( -5.603597561149804562, 5.431951997629870910, 0.7998128361456341429 ) ) ;
#89391 = CARTESIAN_POINT ( 'NONE',  ( 1.037687956146810198, -0.04753379745526563338, 2.221059295257783006 ) ) ;
#89392 = CARTESIAN_POINT ( 'NONE',  ( 2.046058472223175162, 0.8067420340923843192, -1.945513702063914163 ) ) ;
#89393 = CARTESIAN_POINT ( 'NONE',  ( -3.169574050544739841, 6.919863168935977527, -0.7998128361456481317 ) ) ;
#89394 = CARTESIAN_POINT ( 'NONE',  ( 9.250740883225924804, 9.686952540052077509, 1.040834085586084257E-14 ) ) ;
#89395 = CARTESIAN_POINT ( 'NONE',  ( 5.963677626732073023, -0.4536248188283693583, 1.804646041804882195 ) ) ;
#89396 = CARTESIAN_POINT ( 'NONE',  ( 7.182068686937156166, 9.402166106225269715, 1.599625672291281386 ) ) ;
#89397 = FACE_OUTER_BOUND ( 'NONE', #91138, .T. ) ;
#89398 = CARTESIAN_POINT ( 'NONE',  ( -5.465345320084574965, 9.390336950158399532, 0.000000000000000000 ) ) ;
#89399 = CARTESIAN_POINT ( 'NONE',  ( -7.199016379176422120, 11.34267684244042584, 0.000000000000000000 ) ) ;
#89400 = CARTESIAN_POINT ( 'NONE',  ( 0.4574861729177078229, -1.815669959853306370, 1.095388807130371900 ) ) ;
#89401 = CARTESIAN_POINT ( 'NONE',  ( -6.064239847062411926, 10.29697326487330500, 0.000000000000000000 ) ) ;
#89403 = CARTESIAN_POINT ( 'NONE',  ( 3.244534624505683418, -1.932379277470747558, -0.3379807920969243873 ) ) ;
#89402 = CARTESIAN_POINT ( 'NONE',  ( -4.557020949502716471E-14, 0.06250000000002432776, 1.414508159514535457 ) ) ;
#89404 = CARTESIAN_POINT ( 'NONE',  ( 1.639762333045853726, -1.565812861550972324, -1.490595759849028035 ) ) ;
#89405 = CARTESIAN_POINT ( 'NONE',  ( 0.9602180038516641147, -1.664555262390180257, -0.7873027242753791732 ) ) ;
#89407 = CARTESIAN_POINT ( 'NONE',  ( -4.434757016570429755, 7.116138787269118637, -1.097766128466563851 ) ) ;
#89406 = CARTESIAN_POINT ( 'NONE',  ( -4.716257332707368910, 6.595662536282280719, -1.599625672291271394 ) ) ;
#89408 = CARTESIAN_POINT ( 'NONE',  ( 3.099246252510225119, -1.738326302361908882, 0.08608614090572026811 ) ) ;
#89409 = CIRCLE ( 'NONE', #20251, 0.8300000000000008482 ) ;
#89410 = CARTESIAN_POINT ( 'NONE',  ( 7.456621297836082185, 7.801739057004660971, 0.7216878364870317197 ) ) ;
#89411 = CARTESIAN_POINT ( 'NONE',  ( -12.06798728936711385, 5.701251286509326555, 4.345411722927631004 ) ) ;
#89412 = CARTESIAN_POINT ( 'NONE',  ( 0.9717996764858798375, 2.083101276202529384, -0.5774176476955604764 ) ) ;
#89413 = EDGE_CURVE ( 'NONE', #201878, #75836, #47980, .T. ) ;
#89414 = CARTESIAN_POINT ( 'NONE',  ( 2.425157474508771838, 0.8594973679685766754, 1.823840639232063854 ) ) ;
#89415 = DIRECTION ( 'NONE',  ( 0.000000000000000000, 0.000000000000000000, 1.000000000000000000 ) ) ;
#89416 = DIRECTION ( 'NONE',  ( 3.219646771412963434E-15, 1.665334536937739741E-16, 1.000000000000000000 ) ) ;
#89417 = CARTESIAN_POINT ( 'NONE',  ( 2.325019196037684477, -0.001775356835979901692, 1.971640592446997298 ) ) ;
#89418 = CARTESIAN_POINT ( 'NONE',  ( 6.509000000000039421, 2.968845098214093703, 2.453284407971462411 ) ) ;
#89421 = ORIENTED_EDGE ( 'NONE', *, *, #213374, .F. ) ;
#89420 = CARTESIAN_POINT ( 'NONE',  ( -5.153507786970275006, 7.105788066255672497, -1.443375672974066548 ) ) ;
#89419 = CARTESIAN_POINT ( 'NONE',  ( 0.2999999999999842792, 3.975028841772351829, 0.9637995837462106641 ) ) ;
#89422 = CARTESIAN_POINT ( 'NONE',  ( -3.784134271545645412, 7.428924060196286483, 0.7216878364870338292 ) ) ;
#89423 = CARTESIAN_POINT ( 'NONE',  ( 5.468734858265785093, 7.473552982767158070, 1.599625672291269396 ) ) ;
#89424 = CARTESIAN_POINT ( 'NONE',  ( -5.281783360975562225, 8.319775133516907673, 1.199719254218452935 ) ) ;
#89425 = CARTESIAN_POINT ( 'NONE',  ( -6.688968683495758683, 8.897159112202094988, -1.599625672291271394 ) ) ;
#89426 = DIRECTION ( 'NONE',  ( 0.000000000000000000, 8.546850786086437571E-32, 1.000000000000000000 ) ) ;
#89427 = CARTESIAN_POINT ( 'NONE',  ( 5.842881032528668861, 0.4426140756379555730, 2.264596805331307472 ) ) ;
#89428 = CARTESIAN_POINT ( 'NONE',  ( 6.707479306934847507, -1.574971382793718178, -1.169550641929931079 ) ) ;
#89429 = CARTESIAN_POINT ( 'NONE',  ( 4.328923052438288899, -1.828919189252835142, -0.7100325158947774495 ) ) ;
#89430 = CARTESIAN_POINT ( 'NONE',  ( 8.284195553149872993, 9.623648552551724578, -1.199719254218445830 ) ) ;
#89431 = CARTESIAN_POINT ( 'NONE',  ( 0.2291389764034670318, 2.011204493129043591, 0.1455304468792120720 ) ) ;
#89432 = VERTEX_POINT ( 'NONE', #24781 ) ;
#89433 = CARTESIAN_POINT ( 'NONE',  ( 2.466138310383278132, -1.084178177903678320, 1.818555153620523779 ) ) ;
#89434 = CARTESIAN_POINT ( 'NONE',  ( 1.499999999999987121, 1.285416667349485120, 0.8660254037844524744 ) ) ;
#89435 = CARTESIAN_POINT ( 'NONE',  ( -7.528855374290365887, 7.678086112960552434, -0.7998128361456291469 ) ) ;
#89436 = CARTESIAN_POINT ( 'NONE',  ( 2.870863542623874221, 1.748142402769039760, -0.5779331317549916136 ) ) ;
#89437 = ORIENTED_EDGE ( 'NONE', *, *, #58668, .T. ) ;
#89438 = CARTESIAN_POINT ( 'NONE',  ( -9.053093885623068715, 11.58502883802551153, -1.599625672291263179 ) ) ;
#89439 = MANIFOLD_SOLID_BREP ( 'Sweep1[7]', #202089 ) ;
#89440 = CARTESIAN_POINT ( 'NONE',  ( 4.096021571020786567, 1.387573888390711385, 1.603661410755026440 ) ) ;
#89441 = CARTESIAN_POINT ( 'NONE',  ( 6.714805131850001274, -0.1305238817815305985, 1.911932681171425896 ) ) ;
#89442 = CARTESIAN_POINT ( 'NONE',  ( 0.7499999999999902300, 5.347916667349482012, -1.299038105676658228 ) ) ;
#89443 = CARTESIAN_POINT ( 'NONE',  ( 6.564118927310645724, 10.80988918183778225, -0.7998128361456291469 ) ) ;
#89444 = CARTESIAN_POINT ( 'NONE',  ( 5.664274315459256748, 9.830346811336296398, -0.7998128361456481317 ) ) ;
#89445 = EDGE_CURVE ( 'NONE', #181560, #60914, #167899, .T. ) ;
#89446 = CARTESIAN_POINT ( 'NONE',  ( 4.059881558241601240, 2.045671965140416937, -0.2483333800566180083 ) ) ;
#89448 = CARTESIAN_POINT ( 'NONE',  ( 1.206327419354651820, 1.623952629372883427, 0.8676893986077349741 ) ) ;
#89447 = CARTESIAN_POINT ( 'NONE',  ( -5.364222332501225488, 9.410009821226765325, 0.7998128361456481317 ) ) ;
#89449 = CARTESIAN_POINT ( 'NONE',  ( -0.6823417656250212460, 4.301041667008085767, 1.181850606188767472 ) ) ;
#89450 = CARTESIAN_POINT ( 'NONE',  ( -6.010528009390447401, 5.981201532351332339, 0.002814859141863571956 ) ) ;
#89451 = CARTESIAN_POINT ( 'NONE',  ( -15.75000000000000000, 10.90000000000000036, -1.800000000000001155 ) ) ;
#89452 = CARTESIAN_POINT ( 'NONE',  ( 10.99440753328297582, -7.824706741106266072, -0.3572413387871992696 ) ) ;
#89453 = AXIS2_PLACEMENT_3D ( 'NONE', #112538, #77836, #196916 ) ;
#89454 = CARTESIAN_POINT ( 'NONE',  ( 1.629795212970772456, -2.077151576879713080, 0.7458654493318407352 ) ) ;
#89455 = CARTESIAN_POINT ( 'NONE',  ( 3.937032273161138463, 0.3271595461276222139, 2.238503835787652996 ) ) ;
#89456 = CARTESIAN_POINT ( 'NONE',  ( -8.568389894156720032, 10.05917163368005163, 1.082531754730558626 ) ) ;
#89457 = CARTESIAN_POINT ( 'NONE',  ( 3.779414081507098011, 0.2159278537227064809, -1.798573134706340504 ) ) ;
#89458 = CARTESIAN_POINT ( 'NONE',  ( 4.768704397049558175, -0.2406929234074564883, -1.900496090682921579 ) ) ;
#89459 = CARTESIAN_POINT ( 'NONE',  ( 5.564915762860970894, 1.570151797963925455, -1.349580972669261580 ) ) ;
#89460 = CARTESIAN_POINT ( 'NONE',  ( 1.364683531249990311, 3.696875000341416584, 1.214306433183764966E-14 ) ) ;
#89461 = CARTESIAN_POINT ( 'NONE',  ( 2.905103271286565647, 1.664600965932877319, 1.056039161509576108 ) ) ;
#89462 = CARTESIAN_POINT ( 'NONE',  ( 0.9207747878037384481, 1.778742719161881203, 0.7400954639872597829 ) ) ;
#89463 = CARTESIAN_POINT ( 'NONE',  ( 3.871829239884491791, 1.038646522470688671, 1.555605274479121114 ) ) ;
#89464 = CARTESIAN_POINT ( 'NONE',  ( 2.930630293717914725, 1.281480123180640529, -1.919000982882083095 ) ) ;
#89465 = CARTESIAN_POINT ( 'NONE',  ( 4.088223475482699598, 0.9968510564385362205, -1.571365414726686227 ) ) ;
#89466 = CARTESIAN_POINT ( 'NONE',  ( -1.364683531249997417, 4.509375000341424133, 1.214306433183764966E-14 ) ) ;
#89467 = VECTOR ( 'NONE', #71050, 1000.000000000000000 ) ;
#89468 = CARTESIAN_POINT ( 'NONE',  ( -4.436542580169821726, 6.199052314996659874, 1.599625672291267398 ) ) ;
#89469 = CARTESIAN_POINT ( 'NONE',  ( 6.154511665599609493, 9.267681812253174556, 1.199719254218462483 ) ) ;
#89470 = DIRECTION ( 'NONE',  ( 5.578564026256490882E-16, 1.000000000000000000, 9.066213480720158442E-32 ) ) ;
#89471 = CARTESIAN_POINT ( 'NONE',  ( 1.084755975048516285, -2.055113062490296016, -0.4597243831155339300 ) ) ;
#89472 = CARTESIAN_POINT ( 'NONE',  ( 4.839897649954202130, 4.748894801142428790, -0.7216878364870197293 ) ) ;
#89473 = CARTESIAN_POINT ( 'NONE',  ( -0.6823417656250212460, 5.113541667008086655, 1.181850606188767472 ) ) ;
#89474 = CARTESIAN_POINT ( 'NONE',  ( 1.396252044512854118, 4.345153108015988863, -0.1338139928737633322 ) ) ;
#89475 = CARTESIAN_POINT ( 'NONE',  ( 1.916421503514931679, -2.120014230100770725, 0.05699577502370903326 ) ) ;
#89476 = CARTESIAN_POINT ( 'NONE',  ( 3.002403234314147351, 6.387006324390887002, -0.4858955912513076569 ) ) ;
#89477 = CARTESIAN_POINT ( 'NONE',  ( 0.5451830133551841540, 0.1527301869948919366, 2.014097447171578903 ) ) ;
#89478 = CARTESIAN_POINT ( 'NONE',  ( 0.6823417656249882723, 0.3427083336747516196, 1.181850606188755259 ) ) ;
#89479 = CARTESIAN_POINT ( 'NONE',  ( -2.657034918598345730, 5.083329257464595408, -1.082531754730543971 ) ) ;
#89480 = CARTESIAN_POINT ( 'NONE',  ( 3.974511587100456822, 7.788680618259193444, 1.040834085586084257E-14 ) ) ;
#89481 = EDGE_LOOP ( 'NONE', ( #193633, #190912, #27451, #140811, #144690, #49057 ) ) ;
#89482 = EDGE_CURVE ( 'NONE', #145532, #5398, #195587, .T. ) ;
#89483 = CARTESIAN_POINT ( 'NONE',  ( 0.6675187767142229944, 0.2125181155594977611, -2.151144519195991922 ) ) ;
#89484 = CARTESIAN_POINT ( 'NONE',  ( 6.610000000000030518, 1.266345627986571021, 2.115470293623383569 ) ) ;
#89487 = CARTESIAN_POINT ( 'NONE',  ( 3.063779527008304360, 6.518233848244248563, 0.7216878364870317197 ) ) ;
#89486 = CARTESIAN_POINT ( 'NONE',  ( 6.925078400183550364, 2.979478345347879031, 2.309228228758605450 ) ) ;
#89485 = CARTESIAN_POINT ( 'NONE',  ( 5.357406976055401948, 6.279338222599979424, 1.199719254218452935 ) ) ;
#89488 = CARTESIAN_POINT ( 'NONE',  ( -4.842197138736131556, 5.678260079060780008, 1.199719254218452935 ) ) ;
#89489 = CARTESIAN_POINT ( 'NONE',  ( 5.348842313791752900, -1.825074749614737701, -0.8578464102408298597 ) ) ;
#89490 = CARTESIAN_POINT ( 'NONE',  ( -8.731087737520713432, 10.24898578427137963, 1.082531754730558626 ) ) ;
#89492 = B_SPLINE_CURVE_WITH_KNOTS ( 'NONE', 3,
 ( #32716, #119363, #148610, #18586, #98798, #16444, #19654, #82524 ),
 .UNSPECIFIED., .F., .F.,
 ( 4, 2, 2, 4 ),
 ( 0.0001232303426307903009, 0.0004276537133814895756, 0.0005798653987568392265, 0.0007320770841321888774 ),
 .UNSPECIFIED. ) ;
#89491 = CARTESIAN_POINT ( 'NONE',  ( 0.04676574305502099321, -1.756316032869180921, 1.310637071781264984 ) ) ;
#89493 = CARTESIAN_POINT ( 'NONE',  ( -1.138412281109779656E-15, -7.287292266289732368, -9.765991025965622185 ) ) ;
#89495 = CARTESIAN_POINT ( 'NONE',  ( 1.364683531249997417, 10.98437500034139802, 2.602085213965210642E-15 ) ) ;
#89494 = CARTESIAN_POINT ( 'NONE',  ( 6.596550757224428629, -0.5713381284546023009, -2.084776384472402100 ) ) ;
#89496 = CARTESIAN_POINT ( 'NONE',  ( -8.597841969360544567, 13.18256606422934674, 0.7998128361456341429 ) ) ;
#89498 = CARTESIAN_POINT ( 'NONE',  ( 1.036581048048822673, -1.509151586612084373, 1.179680973199858318 ) ) ;
#89497 = CARTESIAN_POINT ( 'NONE',  ( -6.548225005276122168, 6.741943382351338165, 0.7216878364870317197 ) ) ;
#89499 = CARTESIAN_POINT ( 'NONE',  ( -1.402160292154681736E-14, 1.009375000341417916, -1.575800808251659024 ) ) ;
#89500 = CARTESIAN_POINT ( 'NONE',  ( 1.500000000000001332, 9.625000000000001776, 0.000000000000000000 ) ) ;
#89501 = CARTESIAN_POINT ( 'NONE',  ( 2.455304126353729188, 0.4608866456157869607, -1.662088558372651903 ) ) ;
#89502 = CARTESIAN_POINT ( 'NONE',  ( 5.727393547130178675, 5.646656991265468939, 0.000000000000000000 ) ) ;
#89503 = AXIS2_PLACEMENT_3D ( 'NONE', #128671, #127611, #114530 ) ;
#89504 = CARTESIAN_POINT ( 'NONE',  ( 2.407162768383603435, -0.3926560375935496672, 1.725441652247063251 ) ) ;
#89505 = PLANE ( 'NONE',  #209695 ) ;
#89506 = CARTESIAN_POINT ( 'NONE',  ( 5.210101597250164751, -2.196594437182074255, 0.2116553293704941940 ) ) ;
#89507 = VERTEX_POINT ( 'NONE', #175328 ) ;
#89508 = CARTESIAN_POINT ( 'NONE',  ( 4.166274539359494433, 2.019258995967411430, -0.05370046678233526827 ) ) ;
#89509 = CARTESIAN_POINT ( 'NONE',  ( -6.587282531393266360, 8.778525268082516320, 1.599625672291269396 ) ) ;
#89511 = CARTESIAN_POINT ( 'NONE',  ( 4.482046101484723266, -2.016035353076811809, -0.04666016718203602753 ) ) ;
#89510 = CARTESIAN_POINT ( 'NONE',  ( 4.424552244980545446, -0.9075887007226298708, -1.916591080935086788 ) ) ;
#89513 = ORIENTED_EDGE ( 'NONE', *, *, #62276, .T. ) ;
#89512 = CARTESIAN_POINT ( 'NONE',  ( 3.990334445075129466, -1.038098595406260705, 1.484453480236499923 ) ) ;
#89514 = CARTESIAN_POINT ( 'NONE',  ( 6.412080304620304538, 6.445458208337293549, -0.7998128361456481317 ) ) ;
#89515 = ORIENTED_EDGE ( 'NONE', *, *, #116111, .F. ) ;
#89516 = CARTESIAN_POINT ( 'NONE',  ( 1.938157646728836614, 1.849873822469105145, 0.2772664081076986475 ) ) ;
#89517 = CYLINDRICAL_SURFACE ( 'NONE', #172488, 1.250000000000000000 ) ;
#89518 = CARTESIAN_POINT ( 'NONE',  ( 5.988875474321468495, -1.722281623382706073, -0.5616633497566495548 ) ) ;
#89519 = CARTESIAN_POINT ( 'NONE',  ( 5.756345505848640798, 6.148709499980903992, 0.8262799378709930753 ) ) ;
#89520 = DIRECTION ( 'NONE',  ( 0.000000000000000000, 1.000000000000000000, 0.000000000000000000 ) ) ;
#89521 =( NAMED_UNIT ( * ) PLANE_ANGLE_UNIT ( ) SI_UNIT ( $, .RADIAN. ) );
#89522 = EDGE_CURVE ( 'NONE', #182484, #183422, #89299, .T. ) ;
#89523 = CARTESIAN_POINT ( 'NONE',  ( 1.364683531249990311, 2.946875000341416140, 1.214306433183764966E-14 ) ) ;
#89524 = CARTESIAN_POINT ( 'NONE',  ( 6.753369913382843315, 8.011924666102361314, -1.082531754730548412 ) ) ;
#89525 = EDGE_CURVE ( 'NONE', #45420, #117856, #145703, .T. ) ;
#89526 = CARTESIAN_POINT ( 'NONE',  ( -3.174017359375036929, 6.717120995997236221, 0.7216878364870338292 ) ) ;
#89527 = CARTESIAN_POINT ( 'NONE',  ( -6.286140498591554326, 7.362860665558790707, 1.199719254218452047 ) ) ;
#89528 = CARTESIAN_POINT ( 'NONE',  ( 3.955424862866574021, -1.843446357660895041, 1.048082435718917571 ) ) ;
#89530 = CARTESIAN_POINT ( 'NONE',  ( -11.03376256896084584, 6.348997720274319079, -6.086949085616508270 ) ) ;
#89529 = CARTESIAN_POINT ( 'NONE',  ( -0.1294898018152304819, 0.2484418290887774605, -1.961697698124951650 ) ) ;
#89531 = CARTESIAN_POINT ( 'NONE',  ( 5.307875201598577064, -1.962095876955988638, 0.1906144227653387424 ) ) ;
#89532 = CARTESIAN_POINT ( 'NONE',  ( 0.6823417656249899377, 0.5927083336747518416, 1.181850606188755259 ) ) ;
#89533 = CARTESIAN_POINT ( 'NONE',  ( 1.160403428290600392, 2.011073784072180182, 0.09471770850632241223 ) ) ;
#89534 = ORIENTED_EDGE ( 'NONE', *, *, #67920, .T. ) ;
#89535 = CARTESIAN_POINT ( 'NONE',  ( 6.403513597085680686, -2.053302684608013795, 0.5162988180226235624 ) ) ;
#89536 = CARTESIAN_POINT ( 'NONE',  ( 8.998985659026871531, 12.36178301847608196, 7.871464661039776267 ) ) ;
#89537 = CARTESIAN_POINT ( 'NONE',  ( 1.117730493923989599, 0.4056601665377962407, -2.030061024271647252 ) ) ;
#89538 = ORIENTED_EDGE ( 'NONE', *, *, #137200, .F. ) ;
#89539 = CARTESIAN_POINT ( 'NONE',  ( 6.204791576909545192, 7.267953590263130259, -1.199719254218452047 ) ) ;
#89540 = CARTESIAN_POINT ( 'NONE',  ( 5.387385936583818591, 7.378645907471495846, -1.599625672291283607 ) ) ;
#89542 = CARTESIAN_POINT ( 'NONE',  ( 4.333802657862601215, 8.207853534148366492, 0.7998128361456462443 ) ) ;
#89541 = CARTESIAN_POINT ( 'NONE',  ( 3.802746959959231177, 1.793210335683467216, 1.074525653306056316 ) ) ;
#89543 = CARTESIAN_POINT ( 'NONE',  ( 6.875920180786008196, 8.050936961452347163, -1.199719254218452047 ) ) ;
#89546 = ORIENTED_EDGE ( 'NONE', *, *, #34251, .F. ) ;
#89545 = CARTESIAN_POINT ( 'NONE',  ( 1.963241191952873388, -1.455257657876586341, -1.078514734469406600 ) ) ;
#89544 = CARTESIAN_POINT ( 'NONE',  ( 3.205874166558682514, -1.823564452915670042, 0.08818595847179949709 ) ) ;
#89547 = CARTESIAN_POINT ( 'NONE',  ( 6.059228469117068805, -1.890744221452178353, -1.137928576693452820 ) ) ;
#89548 = AXIS2_PLACEMENT_3D ( 'NONE', #60093, #126252, #39575 ) ;
#89549 = CARTESIAN_POINT ( 'NONE',  ( 3.997267248050282884, 1.865803599355109421, -1.178106810156675843 ) ) ;
#89550 = CARTESIAN_POINT ( 'NONE',  ( 8.308449207076147758, 8.587612251210650527, -0.7998128361456281477 ) ) ;
#89551 = DIRECTION ( 'NONE',  ( 1.000000000000000000, 0.000000000000000000, 0.000000000000000000 ) ) ;
#89552 = EDGE_CURVE ( 'NONE', #187716, #169055, #19036, .T. ) ;
#89553 = CARTESIAN_POINT ( 'NONE',  ( 3.299369280271017946, 1.727720890571235124, -0.8199460011262191816 ) ) ;
#89554 = CARTESIAN_POINT ( 'NONE',  ( 7.072549687823125097, 11.40305840243567381, -0.7998128361456291469 ) ) ;
#89555 = CARTESIAN_POINT ( 'NONE',  ( 6.109843426155950219, 0.6047356833836557977, -1.980059631771100781 ) ) ;
#89556 = DIRECTION ( 'NONE',  ( 8.638326563840814399E-31, 0.000000000000000000, 1.000000000000000000 ) ) ;
#89557 = CARTESIAN_POINT ( 'NONE',  ( 5.583573808894983337, -0.9862700065477579825, 1.957137920222583372 ) ) ;
#89558 = CARTESIAN_POINT ( 'NONE',  ( 5.207906507908255378, 7.834591108650524660, -1.266300940072472736 ) ) ;
#89559 = ORIENTED_EDGE ( 'NONE', *, *, #102451, .T. ) ;
#89560 = EDGE_LOOP ( 'NONE', ( #135757, #8427, #204240, #129836 ) ) ;
#89561 = AXIS2_PLACEMENT_3D ( 'NONE', #58588, #205894, #189647 ) ;
#89562 = CARTESIAN_POINT ( 'NONE',  ( 0.3944177863135505113, 2.931182615571563677, 2.025436609040003333 ) ) ;
#89563 = CARTESIAN_POINT ( 'NONE',  ( 4.736594563127852098, 6.619389305106191834, -1.599625672291273171 ) ) ;
#89564 = CARTESIAN_POINT ( 'NONE',  ( 1.850000000000000089, 6.384842951632563950E-31, -5.732590180780448463 ) ) ;
#89565 = FILL_AREA_STYLE_COLOUR ( '', #136518 ) ;
#89566 = B_SPLINE_CURVE_WITH_KNOTS ( 'NONE', 3,
 ( #75184, #141296, #58927, #155359, #204069, #125086, #92530, #6944, #191044, #208362, #126146, #43773, #159634, #105571, #171603, #209419 ),
 .UNSPECIFIED., .F., .F.,
 ( 4, 3, 3, 3, 3, 4 ),
 ( 0.000000000000000000, 6.716675436050588027E-06, 1.344324725954647930E-05, 2.018532118334301782E-05, 2.694176617305359190E-05, 3.135538808398834659E-05 ),
 .UNSPECIFIED. ) ;
#89567 = CARTESIAN_POINT ( 'NONE',  ( -6.697364695470783502, 10.75741654478384035, 0.7216878364870458196 ) ) ;
#89568 = CARTESIAN_POINT ( 'NONE',  ( 3.549202351727371862, 7.362762853649070571, -0.7998128361456362523 ) ) ;
#89569 = CARTESIAN_POINT ( 'NONE',  ( 5.348515126027270306, -2.053966340784090239, -0.2589089449258550890 ) ) ;
#89570 = CARTESIAN_POINT ( 'NONE',  ( 4.125552361149776637, -1.843237290211484192, 0.5602470265201089372 ) ) ;
#89571 = CARTESIAN_POINT ( 'NONE',  ( 1.599232692168949699, -0.2440074622011619843, 2.001515180871694888 ) ) ;
#89572 = CARTESIAN_POINT ( 'NONE',  ( -8.809047120577080392, 11.30030761213851953, 1.599625672291269396 ) ) ;
#89573 = CARTESIAN_POINT ( 'NONE',  ( 6.749980374757213575, 8.968339418673846097, 1.599625672291268286 ) ) ;
#89574 = CARTESIAN_POINT ( 'NONE',  ( 9.367496997597598352, 3.530917816115240804, 7.500000000000001776 ) ) ;
#89575 = CARTESIAN_POINT ( 'NONE',  ( 1.043234067691005684, -1.729537258485489115, -1.345685951901639532 ) ) ;
#89576 = CARTESIAN_POINT ( 'NONE',  ( 5.127504350819418910, -1.732488751877172772, 0.5760870007271365889 ) ) ;
#89577 = CARTESIAN_POINT ( 'NONE',  ( 5.234856708652222856, 8.161064355852680308, 1.082531754730549078 ) ) ;
#89578 = CARTESIAN_POINT ( 'NONE',  ( 8.374132434735052755, 12.92157160716627295, -0.7998128361456352531 ) ) ;
#89579 = CARTESIAN_POINT ( 'NONE',  ( -5.119085517611572378, 8.129960982925583224, 1.199719254218452935 ) ) ;
#89580 = CARTESIAN_POINT ( 'NONE',  ( 3.181359600701000989, 6.863336634126477875, 0.000000000000000000 ) ) ;
#89581 = CARTESIAN_POINT ( 'NONE',  ( 7.675324359112103423, 8.127168971818530707, 0.7216878364870267237 ) ) ;
#89582 = ORIENTED_EDGE ( 'NONE', *, *, #31074, .F. ) ;
#89584 = CARTESIAN_POINT ( 'NONE',  ( 6.469000937953021335, -1.553436082622870140, 1.280157488742767136 ) ) ;
#89583 = CARTESIAN_POINT ( 'NONE',  ( 2.489598673502769977, -1.836455140896048999, -0.1334285330320400531 ) ) ;
#89585 = CARTESIAN_POINT ( 'NONE',  ( 2.161834534229470695, -0.6120774379556602751, -2.215351195248612459 ) ) ;
#89586 = CARTESIAN_POINT ( 'NONE',  ( 6.860214158839045950, -1.961385418603446062, 0.04497666117601883257 ) ) ;
#89587 = CARTESIAN_POINT ( 'NONE',  ( -5.717788096661253761, 7.693838750903348789, 1.599625672291269396 ) ) ;
#89588 = CARTESIAN_POINT ( 'NONE',  ( -5.794181935090157332, 6.277560012370397402, -0.7153197263606870804 ) ) ;
#89589 = CARTESIAN_POINT ( 'NONE',  ( 2.918110517850933672, -1.910018876965378309, 0.09814724848770939314 ) ) ;
#89590 = CARTESIAN_POINT ( 'NONE',  ( -8.296699936558862731, 11.76690146170562201, 1.199719254218453823 ) ) ;
#89591 = CARTESIAN_POINT ( 'NONE',  ( 0.2564123431100414074, -2.069877475643782994, -0.05227228806716639753 ) ) ;
#89592 = CARTESIAN_POINT ( 'NONE',  ( -4.065465959251405081, 5.836405933916976707, -1.599625672291271394 ) ) ;
#89594 = CARTESIAN_POINT ( 'NONE',  ( 1.234984068473435892, -1.692697435815498919, 0.7966027930108383615 ) ) ;
#89593 = CARTESIAN_POINT ( 'NONE',  ( 2.103177918021365223, -0.4551342947399418248, 2.040444103505714146 ) ) ;
#89595 = CARTESIAN_POINT ( 'NONE',  ( 1.968124833515383809, 1.674630251985644414, 1.122327857054454814 ) ) ;
#89596 = CARTESIAN_POINT ( 'NONE',  ( 8.351459436338029008, 10.76645531385962862, -1.443375672974063439 ) ) ;
#89597 = CARTESIAN_POINT ( 'NONE',  ( -1.201851678989727383E-14, 4.509375000341417916, -1.575800808251660134 ) ) ;
#89598 = CARTESIAN_POINT ( 'NONE',  ( 2.964111632446063016, -1.609175542312387908, -0.6635834015607346981 ) ) ;
#89599 = CARTESIAN_POINT ( 'NONE',  ( 5.178324605415663306, 8.128796908705222535, 1.199719254218462483 ) ) ;
#89601 = CARTESIAN_POINT ( 'NONE',  ( 0.2395129731749547353, 2.570475252693285029, -1.989112730403746587 ) ) ;
#89600 =( LENGTH_UNIT ( ) NAMED_UNIT ( * ) SI_UNIT ( .MILLI., .METRE. ) );
#89602 = CARTESIAN_POINT ( 'NONE',  ( 3.299128894759464359, 1.360359547890070964, 1.060362228049552158 ) ) ;
#89603 = CARTESIAN_POINT ( 'NONE',  ( 2.683357600500847262, 1.551837136583393839, 1.547750905674146971 ) ) ;
#89604 = CARTESIAN_POINT ( 'NONE',  ( 5.479209177496175087, -0.05098606815037013545, -2.206463706674952618 ) ) ;
#89605 = CARTESIAN_POINT ( 'NONE',  ( -11.29167836119662738, 5.103960725615834804, -5.764738477843053488 ) ) ;
#89606 = CIRCLE ( 'NONE', #51558, 4.624999999999993783 ) ;
#89607 = CARTESIAN_POINT ( 'NONE',  ( 3.872083141701920805, -2.139866411213369624, 0.3658599195538684290 ) ) ;
#89608 = CARTESIAN_POINT ( 'NONE',  ( 2.525780997283606499, -1.050937884436175418, -1.492673824175783093 ) ) ;
#89609 = CARTESIAN_POINT ( 'NONE',  ( 4.452435347768154195, -1.380274204828018991, 1.605734313660161172 ) ) ;
#89610 = CARTESIAN_POINT ( 'NONE',  ( 6.639320575229274546, 6.037277963978410433, 2.591643891269063360 ) ) ;
#89611 = ORIENTED_EDGE ( 'NONE', *, *, #107594, .T. ) ;
#89613 = CARTESIAN_POINT ( 'NONE',  ( 1.364683531249988757, 1.696875000341414808, 0.000000000000000000 ) ) ;
#89612 = CARTESIAN_POINT ( 'NONE',  ( 5.179329019713509119, 1.537796090523161796, 1.700180828611449035 ) ) ;
#89614 = DIRECTION ( 'NONE',  ( 0.000000000000000000, 1.000000000000000000, 0.000000000000000000 ) ) ;
#89615 = CARTESIAN_POINT ( 'NONE',  ( 10.21336978979620191, 10.81001959771741205, 0.7998128361456462443 ) ) ;
#89616 = CARTESIAN_POINT ( 'NONE',  ( 0.2586463447097427926, 2.115114616003030079, 0.1516365082330217162 ) ) ;
#89617 = CARTESIAN_POINT ( 'NONE',  ( -4.744990575102892905, 8.479646737687938085, 0.7216878364870458196 ) ) ;
#89618 = CARTESIAN_POINT ( 'NONE',  ( 3.063779527008311021, 5.557864633942907417, 1.082531754730546636 ) ) ;
#89619 = CARTESIAN_POINT ( 'NONE',  ( -6.412643469139482910, 7.544134137826577380, 1.082531754730549967 ) ) ;
#89620 = AXIS2_PLACEMENT_3D ( 'NONE', #154326, #186808, #20034 ) ;
#89621 = CARTESIAN_POINT ( 'NONE',  ( 4.095971805104288599, 5.871996087412059140, 1.443375672974058777 ) ) ;
#89622 = EDGE_LOOP ( 'NONE', ( #37051, #31594, #126113, #42382 ) ) ;
#89623 = CARTESIAN_POINT ( 'NONE',  ( 5.344375030997434273, 0.3906003880304632636, -1.978050218768567792 ) ) ;
#89625 = CARTESIAN_POINT ( 'NONE',  ( 3.010651042449908221, 0.6904807078514271224, 1.943715162320960088 ) ) ;
#89624 = CARTESIAN_POINT ( 'NONE',  ( 5.555090253297246150, 7.504024600312024340, 1.599625672291267398 ) ) ;
#89627 = CARTESIAN_POINT ( 'NONE',  ( -0.2411972340276360705, 6.947779742164541972, -2.495493578726155182 ) ) ;
#89626 = CARTESIAN_POINT ( 'NONE',  ( 6.318982112420993502, 9.529840343536603697, -1.199719254218452047 ) ) ;
#89628 = CARTESIAN_POINT ( 'NONE',  ( 8.188198428010544205, 8.517596018959260107, 0.000000000000000000 ) ) ;
#89629 = CARTESIAN_POINT ( 'NONE',  ( -3.285556943750000070, -0.8093749995220431703, 0.000000000000000000 ) ) ;
#89630 = CARTESIAN_POINT ( 'NONE',  ( 3.719872605471109761, 6.605953636083950364, -2.500000000000002220 ) ) ;
#89631 = CARTESIAN_POINT ( 'NONE',  ( 6.650331627364351128, -1.696677047125955795, 1.386650686450926484 ) ) ;
#89632 = CARTESIAN_POINT ( 'NONE',  ( 3.041638857185970046, -1.525043868314728934, 1.319228477497782714 ) ) ;
#89633 = CARTESIAN_POINT ( 'NONE',  ( 2.893917256732419396, -0.5369380550670297403, -1.761199466696103499 ) ) ;
#89634 = CARTESIAN_POINT ( 'NONE',  ( 4.794779880727245036, 8.745660294157122649, -0.7998128361456281477 ) ) ;
#89635 =( NAMED_UNIT ( * ) PLANE_ANGLE_UNIT ( ) SI_UNIT ( $, .RADIAN. ) );
#89636 = CARTESIAN_POINT ( 'NONE',  ( 6.124025070245508573, -1.016541136310184390, -1.516163765885633286 ) ) ;
#89637 = CARTESIAN_POINT ( 'NONE',  ( -5.930802130974132780, 9.006687355190106103, -1.199719254218440723 ) ) ;
#89638 = CARTESIAN_POINT ( 'NONE',  ( 6.491137613139088991, 1.972399245366265985, -1.108330356262598126 ) ) ;
#89639 = CARTESIAN_POINT ( 'NONE',  ( 1.348413808652969337, 2.103741849630758054, 0.1016320799899407962 ) ) ;
#89640 = CARTESIAN_POINT ( 'NONE',  ( -4.423703259808839938, 8.383013913077441259, 0.7998128361456352531 ) ) ;
#89641 = CARTESIAN_POINT ( 'NONE',  ( 5.926885707468349196, 10.06645042535509660, 1.040834085586084257E-14 ) ) ;
#89642 = CARTESIAN_POINT ( 'NONE',  ( 5.682275777458846377, 7.722684055159064975, 1.443375672974064550 ) ) ;
#89643 = DIRECTION ( 'NONE',  ( -2.220446049250313081E-16, 0.000000000000000000, -1.000000000000000000 ) ) ;
#89644 = CARTESIAN_POINT ( 'NONE',  ( -5.689618019229208734, 9.789638122409414223, 0.7998128361456481317 ) ) ;
#89645 = CARTESIAN_POINT ( 'NONE',  ( 7.415946836550727284, 7.754285518838408109, 0.7216878364870317197 ) ) ;
#89646 = CARTESIAN_POINT ( 'NONE',  ( 4.326045746746942200, 7.429495238844160632, 1.107669923005821344 ) ) ;
#89647 = CARTESIAN_POINT ( 'NONE',  ( -3.899941742225307539, 7.701682465904834629, 0.7998128361456341429 ) ) ;
#89648 = CARTESIAN_POINT ( 'NONE',  ( 3.920361760358490599, -2.215291009692350599, 0.1660125995653055075 ) ) ;
#89649 = CARTESIAN_POINT ( 'NONE',  ( 2.396645607016957502, 1.759237466006560391, -1.306522788049699457 ) ) ;
#89650 = CARTESIAN_POINT ( 'NONE',  ( -6.684333426737305572, 7.757142738403693727, -1.199719254218446718 ) ) ;
#89651 = CARTESIAN_POINT ( 'NONE',  ( 6.883263157960367806, 0.5819222519044697783, 1.998722019247618276 ) ) ;
#89653 = MECHANICAL_DESIGN_GEOMETRIC_PRESENTATION_REPRESENTATION (  '', ( #162299 ), #65481 ) ;
#89652 = CARTESIAN_POINT ( 'NONE',  ( -3.461074353238556167, 7.259946855412102273, 0.000000000000000000 ) ) ;
#89654 = CARTESIAN_POINT ( 'NONE',  ( 5.529730448059603454, 1.891198321494348633, -0.5216162335564683561 ) ) ;
#89655 = CARTESIAN_POINT ( 'NONE',  ( 0.000000000000000000, 8.980740528189222971, 0.000000000000000000 ) ) ;
#89656 = CARTESIAN_POINT ( 'NONE',  ( -1.364683531250000748, 2.009375000341421913, 1.214306433183764966E-14 ) ) ;
#89657 = CARTESIAN_POINT ( 'NONE',  ( 6.610000000000030518, 2.992693383986976041, 2.174209315121559349 ) ) ;
#89658 = CARTESIAN_POINT ( 'NONE',  ( -5.910991785878170646, 7.919243054989755670, -1.443375672974059665 ) ) ;
#89659 = CARTESIAN_POINT ( 'NONE',  ( 5.150683391976684788, 2.089615912265533559, 0.3601871064465370087 ) ) ;
#89660 = CARTESIAN_POINT ( 'NONE',  ( -4.981695098378565945, 4.776675467721892332, -0.7998128361456362523 ) ) ;
#89661 = ORIENTED_EDGE ( 'NONE', *, *, #153552, .T. ) ;
#89662 = CARTESIAN_POINT ( 'NONE',  ( 5.928642344448160628, 2.082074431819755045, 0.5810635428650026135 ) ) ;
#89663 = CARTESIAN_POINT ( 'NONE',  ( 6.602984505055297326, 7.662235663108029726, 1.199719254218462483 ) ) ;
#89664 = CARTESIAN_POINT ( 'NONE',  ( 5.126429434416579056, 0.1410513515392505246, 1.835921608166577013 ) ) ;
#89665 = UNCERTAINTY_MEASURE_WITH_UNIT (LENGTH_MEASURE( 1.000000000000000082E-05 ), #88563, 'distance_accuracy_value', 'NONE');
#89666 = CARTESIAN_POINT ( 'NONE',  ( -5.910622443071302357, 6.001017179288033354, 0.07212419881679615896 ) ) ;
#89667 = CARTESIAN_POINT ( 'NONE',  ( -1.402160292154681736E-14, 2.009375000341422801, -1.575800808251660134 ) ) ;
#89668 = CARTESIAN_POINT ( 'NONE',  ( 0.5205769134342881355, -1.653362465512813184, 0.5437448749807861637 ) ) ;
#89670 = EDGE_CURVE ( 'NONE', #152119, #139854, #112366, .T. ) ;
#89669 = CARTESIAN_POINT ( 'NONE',  ( 6.727182134110237577, 2.455520393281558356, 2.294684051055717600 ) ) ;
#89671 = CARTESIAN_POINT ( 'NONE',  ( 4.419594888374914099, 5.218910793601261311, -1.082531754730548412 ) ) ;
#89672 = DIRECTION ( 'NONE',  ( 1.000000000000000000, -0.000000000000000000, -0.000000000000000000 ) ) ;
#89673 = CARTESIAN_POINT ( 'NONE',  ( 4.223607183596161718, -2.069420184152844566, 0.6248923283326962563 ) ) ;
#89674 = EDGE_CURVE ( 'NONE', #109578, #16927, #98810, .T. ) ;
#89675 = CARTESIAN_POINT ( 'NONE',  ( -4.599240423533815125, 6.388866465587984322, 1.599625672291267398 ) ) ;
#89676 = CARTESIAN_POINT ( 'NONE',  ( 6.884150277402729223, -0.1485532345978715640, 1.983297619905934006 ) ) ;
#89677 = CARTESIAN_POINT ( 'NONE',  ( -8.229436053370685400, 10.62409470039771442, 1.443375672974090751 ) ) ;
#89678 = CARTESIAN_POINT ( 'NONE',  ( 4.065412822539622439, 0.2671453805177248508, -2.145074402785766665 ) ) ;
#89679 =( BOUNDED_CURVE ( )  B_SPLINE_CURVE ( 2, ( #204894, #185460, #56547, #122708, #40304, #106411, #103159, #86908, #152976 ),
 .UNSPECIFIED., .F., .T. ) 
 B_SPLINE_CURVE_WITH_KNOTS ( ( 3, 2, 2, 2, 3 ),
 ( 0.5468749999999997780, 0.5520833333333333703, 0.5625000000000000000, 0.5729166666666666297, 0.5781250000000001110 ),
 .UNSPECIFIED. ) 
 CURVE ( )  GEOMETRIC_REPRESENTATION_ITEM ( )  RATIONAL_B_SPLINE_CURVE ( ( 0.9330127018922194093, 0.9330127018922165227, 1.000000000000000000, 0.8660254037844387076, 1.000000000000000000, 0.8660254037844387076, 1.000000000000000000, 0.9330127018922178550, 0.9330127018922192983 ) ) 
 REPRESENTATION_ITEM ( '' )  );
#89680 = CARTESIAN_POINT ( 'NONE',  ( 4.921144022694462272, -0.09977086410491335655, 1.968969177566483042 ) ) ;
#89681 = CARTESIAN_POINT ( 'NONE',  ( 3.391645568799035892, 0.04004947218742663240, 1.733546134666413607 ) ) ;
#89682 = CARTESIAN_POINT ( 'NONE',  ( 0.8729168595149154886, -0.05911722906676297740, -2.190938979806676734 ) ) ;
#89683 = CARTESIAN_POINT ( 'NONE',  ( 1.132322824279883955, -1.466084937595305560, -1.782028031347275832 ) ) ;
#89684 = CARTESIAN_POINT ( 'NONE',  ( 3.409498948718358680, -0.4055148060846422431, 2.020306737620365389 ) ) ;
#89685 = CARTESIAN_POINT ( 'NONE',  ( 5.706574293107399498, 1.714631337756479912, 0.9119185223999854983 ) ) ;
#89686 = CARTESIAN_POINT ( 'NONE',  ( -7.415946836550729948, 9.675023947441092176, 1.443375672974090751 ) ) ;
#89687 = CARTESIAN_POINT ( 'NONE',  ( -4.899292406491858820, 6.809203455697518947, -1.599625672291271394 ) ) ;
#89689 = EDGE_LOOP ( 'NONE', ( #63145, #82342, #125278, #74084 ) ) ;
#89688 = CARTESIAN_POINT ( 'NONE',  ( -3.169574050544739841, 6.919863168935977527, -0.7998128361456481317 ) ) ;
#89690 = CARTESIAN_POINT ( 'NONE',  ( -7.009202228140744673, 10.16085778526412042, -1.082531754730537088 ) ) ;
#89691 = CARTESIAN_POINT ( 'NONE',  ( 2.960231987352707428, 2.196266598062237563, -0.2149427413448631863 ) ) ;
#89692 = CARTESIAN_POINT ( 'NONE',  ( 3.285556943749998737, -3.842708332855377051, -1.896917185911906500 ) ) ;
#89693 = VERTEX_POINT ( 'NONE', #130889 ) ;
#89694 = CARTESIAN_POINT ( 'NONE',  ( 0.7251815698985024650, 0.1899481183357653036, -1.851258252060000498 ) ) ;
#89695 =( BOUNDED_CURVE ( )  B_SPLINE_CURVE ( 2, ( #152303, #3878, #69950, #136062, #202075, #53735, #119866, #106803, #24404 ),
 .UNSPECIFIED., .F., .T. ) 
 B_SPLINE_CURVE_WITH_KNOTS ( ( 3, 2, 2, 2, 3 ),
 ( 0.2708333333333333703, 0.2777777777777777901, 0.2916666666666666852, 0.3055555555555555802, 0.3125000000000000000 ),
 .UNSPECIFIED. ) 
 CURVE ( )  GEOMETRIC_REPRESENTATION_ITEM ( )  RATIONAL_B_SPLINE_CURVE ( ( 0.9330127018922194093, 0.9330127018922196314, 1.000000000000000000, 0.8660254037844387076, 1.000000000000000000, 0.8660254037844387076, 1.000000000000000000, 0.9330127018922194093, 0.9330127018922194093 ) ) 
 REPRESENTATION_ITEM ( '' )  );
#89696 = CARTESIAN_POINT ( 'NONE',  ( -0.1291982275798625457, 2.008329037175633491, -2.487957029800022202 ) ) ;
#89697 = CARTESIAN_POINT ( 'NONE',  ( -0.7499999999999972244, 5.639583334016151639, -1.299038105676652899 ) ) ;
#89698 = CARTESIAN_POINT ( 'NONE',  ( 4.628062896017484995, 7.124942365035781933, -1.349859865738218145 ) ) ;
#89700 = CARTESIAN_POINT ( 'NONE',  ( -4.207966135563093957, 7.175396087857926375, -0.9899555337401829691 ) ) ;
#89699 = CARTESIAN_POINT ( 'NONE',  ( -1.499999999999997780, 5.181250000682820378, 1.214306433183764966E-14 ) ) ;
#89701 = CARTESIAN_POINT ( 'NONE',  ( 6.544863656343847147, -1.481929198830441052, -1.092355128777318107 ) ) ;
#89702 = ORIENTED_EDGE ( 'NONE', *, *, #60337, .T. ) ;
#89703 = CARTESIAN_POINT ( 'NONE',  ( 2.377870294028866294, 1.267006343609432761, 1.625331576946090539 ) ) ;
#89704 = CARTESIAN_POINT ( 'NONE',  ( 0.6801582343749744686, 0.4739583336747441034, 1.178068619123803451 ) ) ;
#89705 = CARTESIAN_POINT ( 'NONE',  ( -6.018930129462987999, 9.109503353427070849, 1.199719254218452047 ) ) ;
#89706 =( NAMED_UNIT ( * ) PLANE_ANGLE_UNIT ( ) SI_UNIT ( $, .RADIAN. ) );
#89707 = CARTESIAN_POINT ( 'NONE',  ( 4.467575310902914154, 5.170924936596891008, 1.199719254218464037 ) ) ;
#89708 = CARTESIAN_POINT ( 'NONE',  ( 0.9540633210794751129, 2.058568143186993105, -0.1002533246910724124 ) ) ;
#89709 = EDGE_CURVE ( 'NONE', #6079, #164652, #15974, .T. ) ;
#89710 =( BOUNDED_SURFACE ( )  B_SPLINE_SURFACE ( 3, 2, ( 
 ( #104418, #156373, #140139 ),
 ( #92461, #171536, #41567 ),
 ( #158500, #22052, #157446 ),
 ( #10099, #72959, #76173 ),
 ( #142279, #208289, #59922 ),
 ( #187779, #105504, #56729 ) ),
 .UNSPECIFIED., .F., .F., .F. ) 
 B_SPLINE_SURFACE_WITH_KNOTS ( ( 4, 2, 4 ),
 ( 3, 3 ),
 ( 0.000000000000000000, 0.0003831327362561331041, 0.0007662654725122662082 ),
 ( 0.000000000000000000, 1.000000000000000000 ),
 .UNSPECIFIED. ) 
 GEOMETRIC_REPRESENTATION_ITEM ( )  RATIONAL_B_SPLINE_SURFACE ( (
 ( 1.000000000000000000, 0.5879095031487548972, 1.000000000000000000),
 ( 1.000000000000000000, 0.5873691247577044194, 1.000000000000000000),
 ( 1.000000000000000000, 0.6054349545499626561, 1.000000000000000000),
 ( 1.000000000000000000, 0.6533334602764224730, 1.000000000000000000),
 ( 1.000000000000000000, 0.6828746263152811746, 1.000000000000000000),
 ( 1.000000000000000000, 0.7071067811865475727, 1.000000000000000000) ) ) 
 REPRESENTATION_ITEM ( '' )  SURFACE ( )  );
#89712 = CARTESIAN_POINT ( 'NONE',  ( 5.267088776126935379, 1.772936381825638952, -0.4966186330585887210 ) ) ;
#89711 = CARTESIAN_POINT ( 'NONE',  ( 0.000000000000000000, 4.000000000000003553, 0.000000000000000000 ) ) ;
#89713 = CARTESIAN_POINT ( 'NONE',  ( 6.174848896020108668, 9.291408581077091000, 1.199719254218460707 ) ) ;
#89714 = CARTESIAN_POINT ( 'NONE',  ( -5.764151584465413869, 6.753873599078290546, -1.199719254218453823 ) ) ;
#89715 = CARTESIAN_POINT ( 'NONE',  ( 4.653060005753134831, -1.773635849817876586, 1.313014255023836618 ) ) ;
#89716 = CARTESIAN_POINT ( 'NONE',  ( 0.2984011986874868794, -2.161112683670802337, -0.05330630956579958390 ) ) ;
#89717 = CIRCLE ( 'NONE', #96197, 9.499999999999992895 ) ;
#89718 = CARTESIAN_POINT ( 'NONE',  ( -5.829642864196175722, 7.824335979694092558, 1.443375672974064550 ) ) ;
#89719 = CARTESIAN_POINT ( 'NONE',  ( 0.01762790050853849447, -0.5081247445114078776, 1.843608005305336528 ) ) ;
#89720 = B_SPLINE_CURVE_WITH_KNOTS ( 'NONE', 3,
 ( #170814, #86364, #2947, #53870 ),
 .UNSPECIFIED., .F., .F.,
 ( 4, 4 ),
 ( 2.718386964177322303E-17, 0.0008010247897357521693 ),
 .UNSPECIFIED. ) ;
#89721 = CARTESIAN_POINT ( 'NONE',  ( 0.8488426437929346147, -1.825078332268307513, -0.8578388575243289793 ) ) ;
#89722 = CARTESIAN_POINT ( 'NONE',  ( 8.122743427918724279, 8.649157885426255632, 0.7216878364870267237 ) ) ;
#89723 = CARTESIAN_POINT ( 'NONE',  ( 1.300659708833833861, -2.077133573725042037, 0.9841232947556498578 ) ) ;
#89724 = STYLED_ITEM ( 'NONE', ( #191580 ), #158197 ) ;
#89725 = CARTESIAN_POINT ( 'NONE',  ( 8.625358771641339573, 15.01266977653634349, -8.344411790353040814 ) ) ;
#89726 = CARTESIAN_POINT ( 'NONE',  ( 6.633470332280523074, -0.1331818211787652029, 1.881796397474523541 ) ) ;
#89727 = FACE_OUTER_BOUND ( 'NONE', #40135, .T. ) ;
#89728 = CARTESIAN_POINT ( 'NONE',  ( 1.305301652190330675, -0.4579020413679709689, 1.813615928118620380 ) ) ;
#89729 = CARTESIAN_POINT ( 'NONE',  ( 2.676970549635893537, 1.727063564601112100, -1.040793759654296213 ) ) ;
#89731 = CARTESIAN_POINT ( 'NONE',  ( -5.960701852718076843, 6.182757358283963889, 0.3440389873682374589 ) ) ;
#89730 = CARTESIAN_POINT ( 'NONE',  ( 0.6823417656249899377, 1.342708333674752508, 1.181850606188755259 ) ) ;
#89733 = CARTESIAN_POINT ( 'NONE',  ( 3.949915024511057471, 0.7098439763573929362, -1.982976504383345162 ) ) ;
#89732 = CARTESIAN_POINT ( 'NONE',  ( -8.365544474831901667, 9.718555627847388578, 1.199719254218462483 ) ) ;
#89734 = CARTESIAN_POINT ( 'NONE',  ( 7.771848369131631351, 10.09024240211882351, -1.599625672291262513 ) ) ;
#89736 = CARTESIAN_POINT ( 'NONE',  ( -8.715193815486133033, 9.062147627688959872, 0.7998128361456462443 ) ) ;
#89735 = CARTESIAN_POINT ( 'NONE',  ( 3.901714345682657292, 7.774026846596938434, 0.7998128361456271485 ) ) ;
#89737 = CARTESIAN_POINT ( 'NONE',  ( 4.166274539359494433, 2.019258995967411430, -0.05370046678233526827 ) ) ;
#89738 = CARTESIAN_POINT ( 'NONE',  ( -0.6823417656249969321, 4.217708333674755394, -1.181850606188749264 ) ) ;
#89739 = CARTESIAN_POINT ( 'NONE',  ( 6.232891784722141892, -1.957473889884550289, -0.6504925196839649315 ) ) ;
#89740 = CARTESIAN_POINT ( 'NONE',  ( 8.107412671292031803, 11.44210330227398487, 1.082531754730557072 ) ) ;
#89741 = ADVANCED_FACE ( 'NONE', ( #128771 ), #70042, .T. ) ;
#89742 = CARTESIAN_POINT ( 'NONE',  ( 4.850933092205481856, -1.739298515662604405, 1.283314429840809234 ) ) ;
#89743 = CARTESIAN_POINT ( 'NONE',  ( 5.501576472095266901, 9.640532660744973725, -0.7998128361456481317 ) ) ;
#89744 = CARTESIAN_POINT ( 'NONE',  ( 1.364683531249986537, -0.5739583329919174526, 0.7879004041258500513 ) ) ;
#89746 = CARTESIAN_POINT ( 'NONE',  ( -9.617648866954043640, -9.063431457505050304, 0.6035590660245172545 ) ) ;
#89745 = CARTESIAN_POINT ( 'NONE',  ( 6.530187263637528439, 7.647581891445782709, -1.199719254218452047 ) ) ;
#89747 = CARTESIAN_POINT ( 'NONE',  ( 8.405692050348340771, 8.908988268268968724, 1.040834085586084257E-14 ) ) ;
#89749 = CARTESIAN_POINT ( 'NONE',  ( 6.882015208740349443, 15.51887838114830132, 9.732639244658489730 ) ) ;
#89748 = CARTESIAN_POINT ( 'NONE',  ( 2.119799831544411095, 0.3726140298815834861, -2.138824928699584405 ) ) ;
#89751 = CARTESIAN_POINT ( 'NONE',  ( 1.294213439101927321, 1.504999338701202394, -1.060447551955064016 ) ) ;
#89750 = CARTESIAN_POINT ( 'NONE',  ( -4.446711195602239819, 8.131654128270509929, -0.7216878364870267237 ) ) ;
#89752 = CARTESIAN_POINT ( 'NONE',  ( -1.364683531250000748, 2.259375000341422357, 1.214306433183764966E-14 ) ) ;
#89753 = CARTESIAN_POINT ( 'NONE',  ( 2.683357600500847262, 1.551837136583393839, 1.547750905674146971 ) ) ;
#89754 = CARTESIAN_POINT ( 'NONE',  ( 3.039828102299942714, 6.452578276080809694, 0.2781515650015949914 ) ) ;
#89755 = CARTESIAN_POINT ( 'NONE',  ( 3.837032359523879332, 0.3291597691741187104, 2.238327980419333674 ) ) ;
#89757 = CARTESIAN_POINT ( 'NONE',  ( -7.379715684540041565, 7.504089808251839244, 1.040834085586084257E-14 ) ) ;
#89756 = B_SPLINE_CURVE_WITH_KNOTS ( 'NONE', 3,
 ( #84678, #30617, #129269, #15394, #100919, #115116, #180059, #181112, #133471, #98811 ),
 .UNSPECIFIED., .F., .F.,
 ( 4, 1, 1, 1, 1, 1, 1, 4 ),
 ( 0.000000000000000000, 0.09183773654504942541, 0.1838067853904964410, 0.2558923657893393822, 0.3606054339151033017, 0.5206678126786191685, 0.7335446035554463728, 1.000000000000000000 ),
 .UNSPECIFIED. ) ;
#89758 = CARTESIAN_POINT ( 'NONE',  ( 4.894543267554960053, 4.887125941896303338, -0.6895117023006970269 ) ) ;
#89759 = CARTESIAN_POINT ( 'NONE',  ( 5.925280661667059690, 7.134359284303951831, -1.114000666120490868 ) ) ;
#89760 = CARTESIAN_POINT ( 'NONE',  ( 1.499999999999997113, 13.14583333333333393, -0.8660254037844378194 ) ) ;
#89761 = CARTESIAN_POINT ( 'NONE',  ( 5.234856708652222856, 8.161064355852680308, 1.082531754730549078 ) ) ;
#89762 = EDGE_CURVE ( 'NONE', #186645, #62746, #71080, .T. ) ;
#89763 = CARTESIAN_POINT ( 'NONE',  ( 5.184699891622216228, -0.2167559868061739725, -1.756304918635148704 ) ) ;
#89764 =( BOUNDED_SURFACE ( )  B_SPLINE_SURFACE ( 3, 3, ( 
 ( #4684, #172571, #139014, #122846, #24153, #73995, #90256, #156324, #57745, #123903, #108694 ),
 ( #189872, #41514, #107627, #173659, #25232, #91335, #58809, #124963, #174722, #26295, #70758 ),
 ( #136871, #202896, #54541, #38291, #104369, #29519, #27370, #129244, #208242, #14301, #59873 ),
 ( #77183, #176831, #78255, #44717, #144379, #63076, #95612, #195217, #112967, #12183, #30593 ),
 ( #50816, #178979, #43652, #45786, #143305, #159509, #67033, #13256, #10050, #127100, #128174 ),
 ( #93470, #109769, #46853, #209296, #133170, #11108, #193065, #161661, #60944, #96679, #116942 ),
 ( #145445, #79328, #211443, #162729, #110823, #80395, #126024, #146490, #191986, #175776, #28445 ) ),
 .UNSPECIFIED., .T., .F., .T. ) 
 B_SPLINE_SURFACE_WITH_KNOTS ( ( 4, 3, 4 ),
 ( 4, 1, 1, 1, 1, 1, 1, 1, 4 ),
 ( 0.000000000000000000, 0.5000000000000000000, 1.000000000000000000 ),
 ( 0.000000000000000000, 0.2254101072112788262, 0.3970395454107691902, 0.5239558410346354389, 0.6152342776129972046, 0.6800502191696807808, 0.7279184599320936977, 0.7685697607527866015, 1.000000000000000000 ),
 .UNSPECIFIED. ) 
 GEOMETRIC_REPRESENTATION_ITEM ( )  RATIONAL_B_SPLINE_SURFACE ( (
 ( 1.000000000000000000, 1.000000000000000000, 1.000000000000000222, 1.000000000000000222, 0.9999999999999996669, 1.000000000000000222, 0.9999999999999994449, 1.000000000000000222, 0.9999999999999992228, 1.000000000000000000, 1.000000000000000000),
 ( 0.3333333333333333703, 0.3333333333333333703, 0.3333333333333334259, 0.3333333333333333703, 0.3333333333333333148, 0.3333333333333334814, 0.3333333333333332593, 0.3333333333333334259, 0.3333333333333330928, 0.3333333333333333703, 0.3333333333333333703),
 ( 0.3333333333333333703, 0.3333333333333333703, 0.3333333333333334259, 0.3333333333333333703, 0.3333333333333333148, 0.3333333333333334814, 0.3333333333333332593, 0.3333333333333334259, 0.3333333333333330928, 0.3333333333333333703, 0.3333333333333333703),
 ( 1.000000000000000000, 1.000000000000000000, 1.000000000000000222, 1.000000000000000222, 0.9999999999999996669, 1.000000000000000222, 0.9999999999999994449, 1.000000000000000222, 0.9999999999999992228, 1.000000000000000000, 1.000000000000000000),
 ( 0.3333333333333333703, 0.3333333333333333703, 0.3333333333333334259, 0.3333333333333333703, 0.3333333333333333148, 0.3333333333333334814, 0.3333333333333332593, 0.3333333333333334259, 0.3333333333333330928, 0.3333333333333333703, 0.3333333333333333703),
 ( 0.3333333333333333703, 0.3333333333333333703, 0.3333333333333334259, 0.3333333333333333703, 0.3333333333333333148, 0.3333333333333334814, 0.3333333333333332593, 0.3333333333333334259, 0.3333333333333330928, 0.3333333333333333703, 0.3333333333333333703),
 ( 1.000000000000000000, 1.000000000000000000, 1.000000000000000222, 1.000000000000000222, 0.9999999999999996669, 1.000000000000000222, 0.9999999999999994449, 1.000000000000000222, 0.9999999999999992228, 1.000000000000000000, 1.000000000000000000) ) ) 
 REPRESENTATION_ITEM ( '' )  SURFACE ( )  );
#89765 = PRESENTATION_LAYER_ASSIGNMENT (  '', '', ( #183110 ) ) ;
#89766 = CARTESIAN_POINT ( 'NONE',  ( 8.796542737168120851, 9.157054702984622097, -0.7998128361456211532 ) ) ;
#89767 = CARTESIAN_POINT ( 'NONE',  ( 1.799976324648028481, -0.7102278526811952597, 1.982709249334560164 ) ) ;
#89769 = CARTESIAN_POINT ( 'NONE',  ( -0.7500000000000215383, 0.9416666666666878571, 1.299038105676659116 ) ) ;
#89768 = CARTESIAN_POINT ( 'NONE',  ( 1.364683531250000303, 10.75520833367473195, -0.7879004041258355073 ) ) ;
#89770 = CARTESIAN_POINT ( 'NONE',  ( 0.7835775553649370062, -1.871284325210004429, 0.6146160330302401498 ) ) ;
#89771 = DIRECTION ( 'NONE',  ( -0.7806247497998005658, 0.000000000000000000, -0.6249999999999988898 ) ) ;
#89772 = CARTESIAN_POINT ( 'NONE',  ( -7.334597915313094241, 9.580116872663850813, 1.040834085586084257E-14 ) ) ;
#89774 = EDGE_LOOP ( 'NONE', ( #36976, #128232, #213614, #119945 ) ) ;
#89773 = CARTESIAN_POINT ( 'NONE',  ( 6.205303291940151844, 1.571521137685438108, -0.9011181087926769528 ) ) ;
#89775 = CARTESIAN_POINT ( 'NONE',  ( 6.304178240674458422, 10.29869901418813782, 1.040834085586084257E-14 ) ) ;
#89776 = CARTESIAN_POINT ( 'NONE',  ( 4.803500792215161574, -0.4985019455652460740, 1.802925825644098534 ) ) ;
#89777 = ORIENTED_EDGE ( 'NONE', *, *, #54037, .T. ) ;
#89778 = CARTESIAN_POINT ( 'NONE',  ( 4.522371119077151391, 0.9712943915625820157, 1.828230030883712498 ) ) ;
#89779 = CARTESIAN_POINT ( 'NONE',  ( 1.224999999999965006, 2.395833333333299286, -0.7072540797573076965 ) ) ;
#89780 = CARTESIAN_POINT ( 'NONE',  ( -4.407809337774280856, 7.196175756495025055, 1.082531754730549967 ) ) ;
#89781 = CARTESIAN_POINT ( 'NONE',  ( 1.689998555091125843, -0.9101070431196979227, -2.859088409908076667 ) ) ;
#89782 = CARTESIAN_POINT ( 'NONE',  ( 7.239163954692881653, 10.53310948286200599, -1.199719254218441611 ) ) ;
#89783 = CARTESIAN_POINT ( 'NONE',  ( -9.501566725078754772, 9.979582688880366703, -0.7998128361456291469 ) ) ;
#89784 = DIRECTION ( 'NONE',  ( 0.000000000000000000, 1.804652791718263484E-16, -1.000000000000000000 ) ) ;
#89785 = FACE_OUTER_BOUND ( 'NONE', #81143, .T. ) ;
#89786 = ADVANCED_FACE ( 'NONE', ( #194747 ), #105790, .T. ) ;
#89787 = CARTESIAN_POINT ( 'NONE',  ( 1.364683531249988757, -0.6156249996585803075, 0.000000000000000000 ) ) ;
#89788 = CARTESIAN_POINT ( 'NONE',  ( -1.500000000000013101, 1.129166666666688634, -0.8660254037844313801 ) ) ;
#89790 = CARTESIAN_POINT ( 'NONE',  ( 6.010342169559767633, 5.906487374108181143, -0.7998128361456281477 ) ) ;
#89789 = CARTESIAN_POINT ( 'NONE',  ( 3.437899435096212208, 1.242623406730450908, 1.518177208742684803 ) ) ;
#89791 = EDGE_CURVE ( 'NONE', #204013, #194558, #79928, .T. ) ;
#89792 = CARTESIAN_POINT ( 'NONE',  ( 2.583361055862750000, 1.319027862724517330, -1.524809160041600498 ) ) ;
#89793 = CARTESIAN_POINT ( 'NONE',  ( -0.1108833634137010582, 5.723767666350643601, -2.491012016648496363 ) ) ;
#89794 = DIRECTION ( 'NONE',  ( -0.9692622846690297500, 0.000000000000000000, 0.2460297208025335747 ) ) ;
#89795 = CARTESIAN_POINT ( 'NONE',  ( 2.161206213664386144, 0.3243885794495802721, -1.842051381961368639 ) ) ;
#89796 = CARTESIAN_POINT ( 'NONE',  ( -0.6823417656250212460, 5.301041667008086655, 1.181850606188767472 ) ) ;
#89797 = CARTESIAN_POINT ( 'NONE',  ( 3.621343358005862267, 1.728792273982106220, 1.031380397273339078 ) ) ;
#89798 = CARTESIAN_POINT ( 'NONE',  ( -8.616370316684697883, 10.01118577667568132, -1.199719254218446718 ) ) ;
#89800 = CARTESIAN_POINT ( 'NONE',  ( 3.866910228754817158, -0.2097145705111657654, -2.106837283413672601 ) ) ;
#89799 = CARTESIAN_POINT ( 'NONE',  ( -4.446711195602245148, 7.171284913969171448, -1.082531754730549967 ) ) ;
#89801 = CARTESIAN_POINT ( 'NONE',  ( -1.001543065824772872E-14, 4.993750000682815937, 1.732050807568877637 ) ) ;
#89802 = CARTESIAN_POINT ( 'NONE',  ( 5.424307079040114665, 1.017280057988108499, 1.803113764695261523 ) ) ;
#89803 = CARTESIAN_POINT ( 'NONE',  ( 4.667750024854814050, 8.667735138964429709, -0.7998128361456381397 ) ) ;
#89805 = CARTESIAN_POINT ( 'NONE',  ( 6.720655732516659597, 0.5653683226944251627, 2.225905711026022971 ) ) ;
#89804 = CARTESIAN_POINT ( 'NONE',  ( 0.8375780558756993344, 0.8438101838260108067, -1.913087135030653974 ) ) ;
#89807 = ORIENTED_EDGE ( 'NONE', *, *, #128175, .T. ) ;
#89806 = CARTESIAN_POINT ( 'NONE',  ( 6.774438514930277933, -1.120217847261167243, 1.442041797927499980 ) ) ;
#89808 = CARTESIAN_POINT ( 'NONE',  ( 7.775764792637399836, 9.030479331953833011, -1.199719254218441611 ) ) ;
#89809 = CARTESIAN_POINT ( 'NONE',  ( -11.97302537858639759, 13.79875989808050107, 0.8111997896468257085 ) ) ;
#89810 = AXIS2_PLACEMENT_3D ( 'NONE', #167230, #118537, #36141 ) ;
#89811 = CARTESIAN_POINT ( 'NONE',  ( -11.60067993250125262, 4.148157162114866736, 5.314938114050354656 ) ) ;
#89812 = CARTESIAN_POINT ( 'NONE',  ( 6.927853306458739979, 10.06595070996845642, 1.082531754730558626 ) ) ;
#89813 = CARTESIAN_POINT ( 'NONE',  ( 5.695833931072550094, 5.817763472438987726, 0.000000000000000000 ) ) ;
#89814 = CARTESIAN_POINT ( 'NONE',  ( 6.147114339676178041, 0.1922309238813116328, 1.902605946959089689 ) ) ;
#89815 = CARTESIAN_POINT ( 'NONE',  ( -8.565000355531095622, 11.01558638625153286, -1.599625672291263179 ) ) ;
#89816 = CARTESIAN_POINT ( 'NONE',  ( 3.981290663907289140, 7.796589541200495965, -0.7998128361456221525 ) ) ;
#89817 = CARTESIAN_POINT ( 'NONE',  ( -9.488725015150309972, -6.691474851359276776, 0.09393477316945002265 ) ) ;
#89818 = DIRECTION ( 'NONE',  ( -1.000000000000000000, 0.000000000000000000, 0.000000000000000000 ) ) ;
#89819 = CARTESIAN_POINT ( 'NONE',  ( 3.334415713957098681, 5.977569868670206787, -1.199719254218446718 ) ) ;
#89820 = ORIENTED_EDGE ( 'NONE', *, *, #124072, .F. ) ;
#89821 = CARTESIAN_POINT ( 'NONE',  ( 6.450795914701256351, -1.844717532910484570, -0.8146137538835170888 ) ) ;
#89822 = DIRECTION ( 'NONE',  ( -8.638326563840814399E-31, 0.000000000000000000, -1.000000000000000000 ) ) ;
#89823 = CARTESIAN_POINT ( 'NONE',  ( -0.1405533004718754753, 0.003749010675345095921, -1.720146753850452681 ) ) ;
#89824 = CARTESIAN_POINT ( 'NONE',  ( -5.422898255786203769, 6.389431388914436738, -1.082531754730544860 ) ) ;
#89825 = CARTESIAN_POINT ( 'NONE',  ( 2.900554798319789906, 5.471398800426671372, 1.199719254218452047 ) ) ;
#89826 = CARTESIAN_POINT ( 'NONE',  ( 2.219528804134728528, 0.3415968887231227713, -1.939435228410562484 ) ) ;
#89827 = CARTESIAN_POINT ( 'NONE',  ( 4.657827466662149973, 1.163286545301238206, 1.646828140416577657 ) ) ;
#89828 = CARTESIAN_POINT ( 'NONE',  ( -6.989391883044787868, 8.113044270762433285, -1.199719254218446718 ) ) ;
#89829 = CARTESIAN_POINT ( 'NONE',  ( -10.96314634606098259, -7.723163831703881321, 0.5532327639488945348 ) ) ;
#89830 = CARTESIAN_POINT ( 'NONE',  ( 4.453197812796324762, 0.4814713343750369190, -2.137748681182354726 ) ) ;
#89831 = DIRECTION ( 'NONE',  ( 0.000000000000000000, 1.000000000000000000, 0.000000000000000000 ) ) ;
#89832 = CARTESIAN_POINT ( 'NONE',  ( 3.170836325157891267, -1.779339148710285867, -0.7386555552950261339 ) ) ;
#89833 = CARTESIAN_POINT ( 'NONE',  ( -8.727698198895085469, 11.20540053684285553, -1.599625672291263179 ) ) ;
#89834 = CARTESIAN_POINT ( 'NONE',  ( -0.1298852118744257267, 5.725805934370246320, -2.320586200942467148 ) ) ;
#89835 = CARTESIAN_POINT ( 'NONE',  ( 0.2763675079364875664, 1.274320874971252460, 1.801605125401319007 ) ) ;
#89836 = CARTESIAN_POINT ( 'NONE',  ( -0.6823417656250003738, 12.90104166700806232, 1.181850606188754593 ) ) ;
#89837 = CARTESIAN_POINT ( 'NONE',  ( 6.335737856287750880, 6.286115675290828264, -0.7998128361456281477 ) ) ;
#89838 = CARTESIAN_POINT ( 'NONE',  ( -3.741371894207415227, 7.428709027653175312, -2.448389769268637384 ) ) ;
#89839 = CARTESIAN_POINT ( 'NONE',  ( 4.909461021924244051, 6.821066840368686712, 1.443375672974065660 ) ) ;
#89840 = ORIENTED_EDGE ( 'NONE', *, *, #117200, .T. ) ;
#89842 = CARTESIAN_POINT ( 'NONE',  ( 3.088541981101311507, -1.197259257089001716, 1.618239360019198880 ) ) ;
#89841 = CARTESIAN_POINT ( 'NONE',  ( 5.847170753249844033, 0.5281823367668266878, -1.763884204139199330 ) ) ;
#89843 = CARTESIAN_POINT ( 'NONE',  ( 4.868718825205943901, -0.6189299756741394321, 2.213421903294809034 ) ) ;
#89845 = CARTESIAN_POINT ( 'NONE',  ( 3.397144026274971029, -1.643366908016094641, 0.8731178804023755902 ) ) ;
#89844 = CARTESIAN_POINT ( 'NONE',  ( 11.88168509644349058, 11.37999999999998302, 1.685788023084328513 ) ) ;
#89846 = CARTESIAN_POINT ( 'NONE',  ( -0.1290005225502676156, 1.324981729379502537, -2.425680704180297464 ) ) ;
#89847 =( LENGTH_UNIT ( ) NAMED_UNIT ( * ) SI_UNIT ( .MILLI., .METRE. ) );
#89848 = CARTESIAN_POINT ( 'NONE',  ( -6.287230548435221777, 8.358188277972981695, -1.599625672291263179 ) ) ;
#89849 = CARTESIAN_POINT ( 'NONE',  ( -4.177320726786328819, 5.966903162707725805, -1.443375672974066548 ) ) ;
#89850 = CARTESIAN_POINT ( 'NONE',  ( 6.304249618663324561, 1.548718018665395713, -1.404690827926929453 ) ) ;
#89851 = CARTESIAN_POINT ( 'NONE',  ( 6.155038550924150087, 7.243595066575396757, 1.082531754730558626 ) ) ;
#89852 = EDGE_LOOP ( 'NONE', ( #103379, #136560, #45580, #179973 ) ) ;
#89853 = CARTESIAN_POINT ( 'NONE',  ( 9.836090041150102437, -8.872041098393760095, -0.1716895903079586339 ) ) ;
#89854 = DIRECTION ( 'NONE',  ( 0.7592566023653005702, -0.6507913734559639396, 0.000000000000000000 ) ) ;
#89855 = CARTESIAN_POINT ( 'NONE',  ( 6.234932630344998117, 0.1766075427261544484, 1.715814389380666327 ) ) ;
#89856 = CARTESIAN_POINT ( 'NONE',  ( -4.791917227426195858, 7.677988301050826969, -1.199719254218452047 ) ) ;
#89857 = CARTESIAN_POINT ( 'NONE',  ( 2.215074966175926363, 1.682300057933778126, 0.4202854259360877531 ) ) ;
#89858 = SURFACE_SIDE_STYLE ('',( #109358 ) ) ;
#89859 = CYLINDRICAL_SURFACE ( 'NONE', #178227, 1.500000000000000222 ) ;
#89860 = ADVANCED_FACE ( 'NONE', ( #129842 ), #31202, .T. ) ;
#89861 = CARTESIAN_POINT ( 'NONE',  ( -7.379715684540041565, 7.504089808251839244, 1.040834085586084257E-14 ) ) ;
#89862 = CARTESIAN_POINT ( 'NONE',  ( -5.000000000000009770, 3.850000000000006306, -0.4999999999999942824 ) ) ;
#89863 = CARTESIAN_POINT ( 'NONE',  ( 0.4794554595633391814, -0.1051018081165492196, 2.067734805981166435 ) ) ;
#89864 = CARTESIAN_POINT ( 'NONE',  ( 5.672426548614882158, -1.154804106291613675, 1.414059844683832834 ) ) ;
#89865 = CARTESIAN_POINT ( 'NONE',  ( 3.854310441289869882, -1.959320932037407426, -0.1006921081871253454 ) ) ;
#89866 = CARTESIAN_POINT ( 'NONE',  ( 1.224999999999976996, -0.5833333326504948069, 0.7072540797572697269 ) ) ;
#89867 = LINE ( 'NONE', #42181, #181775 ) ;
#89868 = CARTESIAN_POINT ( 'NONE',  ( 6.265839547809997079, 10.46189657242035587, 0.7998128361456462443 ) ) ;
#89869 = CARTESIAN_POINT ( 'NONE',  ( 3.299587915756982515, 1.916203934664402198, -0.9084051299479002362 ) ) ;
#89870 = CARTESIAN_POINT ( 'NONE',  ( -0.3769810270648435990, 3.049942316455334090, 0.4288785890452350702 ) ) ;
#89871 =( LENGTH_UNIT ( ) NAMED_UNIT ( * ) SI_UNIT ( .MILLI., .METRE. ) );
#89872 = CARTESIAN_POINT ( 'NONE',  ( 1.850524992189076290, -2.059912964915584954, -0.2069831422613493399 ) ) ;
#89874 = CARTESIAN_POINT ( 'NONE',  ( -1.402160292154681736E-14, -0.7406249996585823059, -1.575800808251665908 ) ) ;
#89873 = FACE_OUTER_BOUND ( 'NONE', #137185, .T. ) ;
#89876 = EDGE_LOOP ( 'NONE', ( #211684, #86775, #26644, #47882 ) ) ;
#89875 = CARTESIAN_POINT ( 'NONE',  ( 3.967602866622577107, -1.847128000506767176, -1.233534119358855152 ) ) ;
#89877 = CARTESIAN_POINT ( 'NONE',  ( 1.460084154473238138, -2.184713004772549372, -0.7151137612169417013 ) ) ;
#89879 = CARTESIAN_POINT ( 'NONE',  ( 0.3034670832338138835, -1.512625156342655819, -1.248876549296701333 ) ) ;
#89878 = CARTESIAN_POINT ( 'NONE',  ( 9.083599731475983319, 11.62061899152058686, 1.443375672974076540 ) ) ;
#89881 = CARTESIAN_POINT ( 'NONE',  ( 3.475000000000000533, -0.5541666666666681396, 2.006292185433948827 ) ) ;
#89880 = CARTESIAN_POINT ( 'NONE',  ( 5.727393547130178675, 5.646656991265468939, 0.000000000000000000 ) ) ;
#89882 = DIRECTION ( 'NONE',  ( 0.000000000000000000, 0.000000000000000000, -1.000000000000000000 ) ) ;
#89883 = CARTESIAN_POINT ( 'NONE',  ( 6.146043377905669125, 0.5841948715668408010, 1.746183665442810007 ) ) ;
#89884 = ORIENTED_EDGE ( 'NONE', *, *, #89762, .F. ) ;
#89885 = CARTESIAN_POINT ( 'NONE',  ( -3.288454681041543370, 6.406095492915408585, 0.7457829957396812093 ) ) ;
#89886 = CARTESIAN_POINT ( 'NONE',  ( 3.427896188528327226, -1.883279545317056547, 0.3315703044584616399 ) ) ;
#89887 = CARTESIAN_POINT ( 'NONE',  ( -0.2104748580754201015, 7.629137130509078268, -2.703678718140526627 ) ) ;
#89888 = CARTESIAN_POINT ( 'NONE',  ( 4.067213672036010585, 0.2104045600922407611, -1.711820660605578137 ) ) ;
#89889 = CARTESIAN_POINT ( 'NONE',  ( 2.378138974734815392, -2.011451771401792321, -0.1435188914247695346 ) ) ;
#89890 = CARTESIAN_POINT ( 'NONE',  ( 4.078954460043759056, -0.8795263853869551562, 2.123946672719174700 ) ) ;
#89891 = CARTESIAN_POINT ( 'NONE',  ( 3.198750403210961490, -0.6533003841502099673, -2.166054703861711506 ) ) ;
#89892 = CARTESIAN_POINT ( 'NONE',  ( 5.320966398826527666, 1.945490409060679049, 0.8070863781705228668 ) ) ;
#89893 = CARTESIAN_POINT ( 'NONE',  ( -5.139949633356594383, 9.010708648975750634, 0.000000000000000000 ) ) ;
#89894 = ORIENTED_EDGE ( 'NONE', *, *, #201380, .T. ) ;
#89895 = CARTESIAN_POINT ( 'NONE',  ( 4.797990518455403475, -1.769373726167685623, -0.04385371103611360177 ) ) ;
#89897 = CARTESIAN_POINT ( 'NONE',  ( 0.6391472400242370622, -1.963128197947199727, 1.183262795983427207 ) ) ;
#89896 = CARTESIAN_POINT ( 'NONE',  ( 7.374709211190586089, 7.568525266002632534, 0.000000000000000000 ) ) ;
#89898 = CARTESIAN_POINT ( 'NONE',  ( 6.052668933152094866, -1.581501214056714177, -0.9424504099920794076 ) ) ;
#89899 = CARTESIAN_POINT ( 'NONE',  ( -3.490334480514268645, 6.159475096320226939, -1.199719254218452935 ) ) ;
#89900 = CARTESIAN_POINT ( 'NONE',  ( 5.964808794498538624, 0.1646014364122504459, -2.185315939793014639 ) ) ;
#89901 = CARTESIAN_POINT ( 'NONE',  ( -3.785751206713858785, 5.439795712631356750, 1.599625672291267398 ) ) ;
#89902 = CARTESIAN_POINT ( 'NONE',  ( -6.739446930247193990, 15.46990418895350849, 9.939002560225588923 ) ) ;
#89903 = CARTESIAN_POINT ( 'NONE',  ( 5.652806998763869828, -0.4994405740583847675, -2.009109930559597856 ) ) ;
#89904 = CARTESIAN_POINT ( 'NONE',  ( -0.2058462039469660110, -0.8663896114125648751, -1.819200108291472606 ) ) ;
#89905 = CARTESIAN_POINT ( 'NONE',  ( 1.364683531249990311, 5.363541667008086655, 0.7879004041258500513 ) ) ;
#89906 = CARTESIAN_POINT ( 'NONE',  ( 4.758382555496592836, 0.7388506920381915366, 1.779377657810585767 ) ) ;
#89907 = CARTESIAN_POINT ( 'NONE',  ( 1.364683531250000303, 10.50520833367473195, -0.7879004041258355073 ) ) ;
#89908 = CARTESIAN_POINT ( 'NONE',  ( 3.469446951953614189E-15, -16.99999999999999645, 6.938893903907228378E-15 ) ) ;
#89909 = CARTESIAN_POINT ( 'NONE',  ( 1.494693441997055894, -1.183060725354843079, 1.879997432091018217 ) ) ;
#89911 = ORIENTED_EDGE ( 'NONE', *, *, #110985, .F. ) ;
#89910 = DIRECTION ( 'NONE',  ( 0.6507913734559640506, -0.7592566023653005702, 0.000000000000000000 ) ) ;
#89912 = CARTESIAN_POINT ( 'NONE',  ( -5.017926250833627755, 5.026871178826882947, 0.7216878364870257245 ) ) ;
#89913 = CARTESIAN_POINT ( 'NONE',  ( 4.715538499454675403, 4.395883092318884522, 1.214306433183764966E-14 ) ) ;
#89914 = DIRECTION ( 'NONE',  ( 0.000000000000000000, 1.000000000000000000, 0.000000000000000000 ) ) ;
#89915 = CARTESIAN_POINT ( 'NONE',  ( -4.370663978927107785, 5.060324124126027279, -2.420000000000000373 ) ) ;
#89916 = DIRECTION ( 'NONE',  ( -0.000000000000000000, -1.000000000000000000, -0.000000000000000000 ) ) ;
#89917 = CARTESIAN_POINT ( 'NONE',  ( 9.910647101465253073, 11.62513837554007168, -1.082531754730537088 ) ) ;
#89919 = ADVANCED_FACE ( 'NONE', ( #66843 ), #115690, .T. ) ;
#89918 = CARTESIAN_POINT ( 'NONE',  ( 1.205434515183744226, -1.544416933936803904, -1.209700862059132964 ) ) ;
#89920 = CARTESIAN_POINT ( 'NONE',  ( -1.364683531250012516, 2.092708333674750953, 0.7879004041258379498 ) ) ;
#89921 = DIRECTION ( 'NONE',  ( 8.638326563840814399E-31, -0.000000000000000000, 1.000000000000000000 ) ) ;
#89922 = CARTESIAN_POINT ( 'NONE',  ( 6.760214184729610665, -1.961454122871961747, 0.04698431645466792650 ) ) ;
#89923 = CARTESIAN_POINT ( 'NONE',  ( -7.645908563102897126, 11.00764485934031889, 1.199719254218453823 ) ) ;
#89924 = CARTESIAN_POINT ( 'NONE',  ( -4.514501963226242864, 7.250374142863800664, 1.082531754730560403 ) ) ;
#89925 = CARTESIAN_POINT ( 'NONE',  ( 0.3743661609300020232, 1.305675439620108458, 1.847588536312362972 ) ) ;
#89927 = ORIENTED_EDGE ( 'NONE', *, *, #95972, .F. ) ;
#89926 = CARTESIAN_POINT ( 'NONE',  ( -4.880045225915050189, 7.780804299287790826, 1.199719254218464037 ) ) ;
#89928 = CARTESIAN_POINT ( 'NONE',  ( -1.500000000000001332, -0.8187499993171781787, 0.000000000000000000 ) ) ;
#89929 = CARTESIAN_POINT ( 'NONE',  ( 1.282252794574537447, -1.823689378192733912, -0.4153219600965887826 ) ) ;
#89930 = CARTESIAN_POINT ( 'NONE',  ( 0.5978079470381278959, -0.2563149341858957930, 1.714925299717950491 ) ) ;
#89932 = CARTESIAN_POINT ( 'NONE',  ( 4.001666433686186686, -2.185622478633037602, 0.1623105178310546570 ) ) ;
#89931 = CARTESIAN_POINT ( 'NONE',  ( 1.360316468749955598, 1.536458333674721288, -0.7853790794159342115 ) ) ;
#89933 = CARTESIAN_POINT ( 'NONE',  ( 3.997355382689435466, 1.951332032848082099, -1.231501813138028423 ) ) ;
#89934 = CARTESIAN_POINT ( 'NONE',  ( 0.2509463769419334467, -1.655472276559850853, 1.227265982703225511 ) ) ;
#89935 = CARTESIAN_POINT ( 'NONE',  ( 2.554547512858021729, -1.689694153139981392, -0.9569994400411386826 ) ) ;
#89936 = CARTESIAN_POINT ( 'NONE',  ( -6.060131475184148186, 6.172500930577367484, 0.7216878364870317197 ) ) ;
#89937 = CARTESIAN_POINT ( 'NONE',  ( -1.403499169896182730, 7.376709478543820531, -4.304123474985523501 ) ) ;
#89939 = EDGE_CURVE ( 'NONE', #86578, #112521, #154550, .T. ) ;
#89938 = CARTESIAN_POINT ( 'NONE',  ( 5.308877466510794285, -0.5174029350529658622, -2.056363676157816123 ) ) ;
#89940 = SURFACE_STYLE_FILL_AREA ( #172246 ) ;
#89941 = CARTESIAN_POINT ( 'NONE',  ( 3.094375128876575065, -0.3905979561782264575, 1.978050703236901686 ) ) ;
#89942 = CARTESIAN_POINT ( 'NONE',  ( -3.578989363883261277, 7.119311991265024453, 1.040834085586084257E-14 ) ) ;
#89943 = CARTESIAN_POINT ( 'NONE',  ( -6.444921918449773024, 8.612437886315108315, 1.599625672291269396 ) ) ;
#89945 =( BOUNDED_CURVE ( )  B_SPLINE_CURVE ( 2, ( #195613, #26699, #146885, #130682, #208634, #126424, #45118 ),
 .UNSPECIFIED., .F., .T. ) 
 B_SPLINE_CURVE_WITH_KNOTS ( ( 3, 2, 2, 3 ),
 ( 0.4137979667686199625, 0.4166666666666666852, 0.4226190476190476164, 0.4254877475170942835 ),
 .UNSPECIFIED. ) 
 CURVE ( )  GEOMETRIC_REPRESENTATION_ITEM ( )  RATIONAL_B_SPLINE_CURVE ( ( 0.9331000818465633451, 0.9354320710352559409, 1.000000000000000000, 0.8660254037844387076, 1.000000000000000000, 0.9354320710352564960, 0.9331000818465632340 ) ) 
 REPRESENTATION_ITEM ( '' )  );
#89944 = CARTESIAN_POINT ( 'NONE',  ( 10.40996301719436090, 11.03937836301526687, 0.000000000000000000 ) ) ;
#89946 = CARTESIAN_POINT ( 'NONE',  ( 0.7678472254676466102, 0.8974085622692473674, 1.589837017038860045 ) ) ;
#89947 = CARTESIAN_POINT ( 'NONE',  ( -5.261446130555064826, 8.296048364692991228, 1.199719254218452935 ) ) ;
#89948 = CARTESIAN_POINT ( 'NONE',  ( -0.07968937631781032593, 15.51803367805782052, 11.99973206003984139 ) ) ;
#89949 = CARTESIAN_POINT ( 'NONE',  ( -11.23957921816311512, 4.929848952671569862, 5.866464787178605533 ) ) ;
#89950 = ORIENTED_EDGE ( 'NONE', *, *, #98152, .T. ) ;
#89951 = CARTESIAN_POINT ( 'NONE',  ( 6.051650376505027573, 0.6007964193008934473, -1.971360088487213780 ) ) ;
#89952 = CARTESIAN_POINT ( 'NONE',  ( -6.658462837642833421, 8.861568958707010779, 1.443375672974064550 ) ) ;
#89953 = CARTESIAN_POINT ( 'NONE',  ( -4.548924232584923288, 5.265832011892554121, -1.199719254218446718 ) ) ;
#89954 = DIRECTION ( 'NONE',  ( -0.6762880771785568790, 0.000000000000000000, -0.7366372490351884572 ) ) ;
#89955 = CARTESIAN_POINT ( 'NONE',  ( 4.459631813825579272, -1.562525726068206833, -1.279702784981617825 ) ) ;
#89957 = VERTEX_POINT ( 'NONE', #137245 ) ;
#89956 = CARTESIAN_POINT ( 'NONE',  ( 5.602238577124374785, -1.000643217919431116, 1.983199510308247815 ) ) ;
#89958 = CARTESIAN_POINT ( 'NONE',  ( -3.817502770699643388, 6.611447778194983194, 1.199719254218452935 ) ) ;
#89959 = CARTESIAN_POINT ( 'NONE',  ( 4.981731378017507872, 7.899438143407371271, -1.199719254218452047 ) ) ;
#89960 = CIRCLE ( 'NONE', #24200, 2.750000000000008438 ) ;
#89961 = CARTESIAN_POINT ( 'NONE',  ( 4.416905344109374632, 1.883477791879540231, 0.8369615876049685266 ) ) ;
#89962 = CARTESIAN_POINT ( 'NONE',  ( 4.430314669760617718, -1.560499787156752971, -1.277043788614096176 ) ) ;
#89963 = ORIENTED_EDGE ( 'NONE', *, *, #213856, .T. ) ;
#89964 = CARTESIAN_POINT ( 'NONE',  ( 4.552840656090682891, 4.206068941727564514, 1.214306433183764966E-14 ) ) ;
#89966 = ORIENTED_EDGE ( 'NONE', *, *, #26877, .T. ) ;
#89965 = CARTESIAN_POINT ( 'NONE',  ( -7.445362632559989535, 8.715286488521982733, 1.199719254218452047 ) ) ;
#89967 = CARTESIAN_POINT ( 'NONE',  ( 5.213898493288036562, 7.712005038449616379, -1.200564631081424416 ) ) ;
#89968 = CARTESIAN_POINT ( 'NONE',  ( 3.919295934624257960, 0.7230291454519314209, 1.882185965797255278 ) ) ;
#89969 = CARTESIAN_POINT ( 'NONE',  ( 3.169683937527142170, -1.096016708463069422, 1.479218548343118389 ) ) ;
#89970 = CARTESIAN_POINT ( 'NONE',  ( 7.015401035077338143, 6.062865449010540253, 2.437084766375293476 ) ) ;
#89971 = CARTESIAN_POINT ( 'NONE',  ( 0.8214423835279326402, 2.134246884609458661, 0.8782244701446385582 ) ) ;
#89972 = CARTESIAN_POINT ( 'NONE',  ( 4.004454267989866700, 5.765225627445230927, 1.599625672291262513 ) ) ;
#89973 = CARTESIAN_POINT ( 'NONE',  ( 3.673254355229157664, 0.05708692194854488033, -2.161017345153878999 ) ) ;
#89974 = CARTESIAN_POINT ( 'NONE',  ( 7.801827329660018684, 11.18955008699033726, 1.199719254218460707 ) ) ;
#89975 = CARTESIAN_POINT ( 'NONE',  ( -3.913499895838973508, 7.717500311787445000, 1.040834085586084257E-14 ) ) ;
#89976 = AXIS2_PLACEMENT_3D ( 'NONE', #52990, #87633, #185107 ) ;
#89977 = CARTESIAN_POINT ( 'NONE',  ( -0.01083140255524777523, -7.162053774861989019, -9.500385102287573602 ) ) ;
#89978 = CARTESIAN_POINT ( 'NONE',  ( 1.902992089709685031, 1.553661375375714471, 1.041555772207984676 ) ) ;
#89979 = CARTESIAN_POINT ( 'NONE',  ( 0.5792891803052163668, 1.841034274367932877, -0.7053527730483382108 ) ) ;
#89981 = CARTESIAN_POINT ( 'NONE',  ( -4.001066012398721838, 7.682011088333574378, -6.818990669119789124E-05 ) ) ;
#89980 = CARTESIAN_POINT ( 'NONE',  ( 0.6823417656249899377, 4.426041667008086655, -1.181850606188754593 ) ) ;
#89983 = CARTESIAN_POINT ( 'NONE',  ( 1.981372325807278623, -0.1102420082176903682, -2.204251428397439483 ) ) ;
#89982 = CARTESIAN_POINT ( 'NONE',  ( -5.738125327081750271, 7.717565519727259904, 1.599625672291269396 ) ) ;
#89984 = CARTESIAN_POINT ( 'NONE',  ( -10.38614328979765489, 3.507114751586604129, -5.996442624206661520 ) ) ;
#89985 = CARTESIAN_POINT ( 'NONE',  ( 5.464099601507359516, 6.333536608968757697, 1.199719254218462483 ) ) ;
#89986 = CARTESIAN_POINT ( 'NONE',  ( -4.924636110261798372, 6.768494766770632332, 1.599625672291267398 ) ) ;
#89987 = CARTESIAN_POINT ( 'NONE',  ( 0.000000000000000000, -0.5000000000000004441, 0.000000000000000000 ) ) ;
#89988 = CARTESIAN_POINT ( 'NONE',  ( 6.051636762666342761, 0.5725952485956290472, -1.886469267683591466 ) ) ;
#89989 = CARTESIAN_POINT ( 'NONE',  ( 5.918676688095830585, 1.554283316268306292, -1.705954940095489203 ) ) ;
#89990 = CARTESIAN_POINT ( 'NONE',  ( 6.637149568644561626, -0.09269223384644230401, -1.858852300295941395 ) ) ;
#89991 = CARTESIAN_POINT ( 'NONE',  ( 3.590735542246026313, 2.011259174285257689, 0.4565010432640480564 ) ) ;
#89992 = CARTESIAN_POINT ( 'NONE',  ( 7.131225611108096274, 8.382479970123348778, 1.082531754730558626 ) ) ;
#89993 = ADVANCED_FACE ( 'NONE', ( #22379 ), #68994, .T. ) ;
#89994 = CARTESIAN_POINT ( 'NONE',  ( 5.657495238652423097, 9.822437888394988548, 0.000000000000000000 ) ) ;
#89995 = CARTESIAN_POINT ( 'NONE',  ( 7.592202833528386208, 7.959917515312338487, 1.040834085586084257E-14 ) ) ;
#89996 = CARTESIAN_POINT ( 'NONE',  ( 1.364683531249988535, 3.176041667008084435, 0.7879004041258500513 ) ) ;
#89997 = CARTESIAN_POINT ( 'NONE',  ( -8.148229011229679131, 14.52979931989257523, 8.855646333722853925 ) ) ;
#89998 = CARTESIAN_POINT ( 'NONE',  ( 5.029711800545521250, 5.930713857800314237, -1.082531754730549078 ) ) ;
#89999 = CARTESIAN_POINT ( 'NONE',  ( 5.477072320546296780, 2.003985016195033886, 0.8359633449262526828 ) ) ;
#90001 = CARTESIAN_POINT ( 'NONE',  ( 5.144037045698616417, 0.5398437887287730330, 1.760322748975438500 ) ) ;
#90000 = CARTESIAN_POINT ( 'NONE',  ( -11.48243876534946040, 9.799999999999998934, -3.200000000000001510 ) ) ;
#90003 = CARTESIAN_POINT ( 'NONE',  ( 9.573337995800486055, -7.550885189219932236, 1.710794795216873110E-15 ) ) ;
#90002 = CARTESIAN_POINT ( 'NONE',  ( -11.84668730067608422, 10.89999999999998259, 1.399999999999998357 ) ) ;
#90004 = DIRECTION ( 'NONE',  ( -1.000000000000000000, 0.000000000000000000, 0.000000000000000000 ) ) ;
#90005 = CARTESIAN_POINT ( 'NONE',  ( 6.754744673581316583, -1.754229693457433736, 1.428470910521584036 ) ) ;
#90006 = CARTESIAN_POINT ( 'NONE',  ( -5.355516094498059765, 6.520963868127283014, 1.360184235745926618 ) ) ;
#90007 = DIRECTION ( 'NONE',  ( -0.000000000000000000, 1.000000000000000000, -0.000000000000000000 ) ) ;
#90008 = CARTESIAN_POINT ( 'NONE',  ( 5.770588788983777917, 7.358121641400980018, 1.301467365913897112 ) ) ;
#90009 = CARTESIAN_POINT ( 'NONE',  ( -5.329763783503577379, 6.351050847909847086, 1.082531754730549078 ) ) ;
#90010 = CARTESIAN_POINT ( 'NONE',  ( -1.346456596051761601, 3.462271664236989288, -0.3357819570988693214 ) ) ;
#90011 = CARTESIAN_POINT ( 'NONE',  ( 2.236828121427667071, -1.582394523617111970, 0.7928310554637070240 ) ) ;
#90012 = CARTESIAN_POINT ( 'NONE',  ( 6.586586637485376983, -1.237022783311360730, 1.588989491490456762 ) ) ;
#90014 = CARTESIAN_POINT ( 'NONE',  ( 3.497576124367638872, -1.886684243562693597, 0.3306681954469546936 ) ) ;
#90013 = CARTESIAN_POINT ( 'NONE',  ( -8.618179199781044630, 13.20629283305325963, 0.7998128361456341429 ) ) ;
#90015 = CARTESIAN_POINT ( 'NONE',  ( 3.022498986271238586, 2.800000000000017586, -2.499999999999995115 ) ) ;
#90016 = CARTESIAN_POINT ( 'NONE',  ( 3.859776292547572929, -0.5741801112500494186, 1.883974994742370068 ) ) ;
#90017 = CARTESIAN_POINT ( 'NONE',  ( 6.363536886121980984, -1.624614756573187435, -1.199887179878684540 ) ) ;
#90018 = CARTESIAN_POINT ( 'NONE',  ( -4.471491734408701291, 4.111161866431900513, 1.214306433183764966E-14 ) ) ;
#90019 = CARTESIAN_POINT ( 'NONE',  ( 2.852262661058731386, 0.6285613048715790185, 1.762029509812724992 ) ) ;
#90021 = ORIENTED_EDGE ( 'NONE', *, *, #53239, .F. ) ;
#90020 = CARTESIAN_POINT ( 'NONE',  ( 6.639270748794153576, -1.536914537172892725, 0.7831451356504478545 ) ) ;
#90023 = CARTESIAN_POINT ( 'NONE',  ( 4.256897045010922476, 5.029096643009940415, -1.082531754730548412 ) ) ;
#90022 = CARTESIAN_POINT ( 'NONE',  ( 2.034064749695370100, -1.442962035976073309, -1.669870808145665020 ) ) ;
#90024 = AXIS2_PLACEMENT_3D ( 'NONE', #37324, #25340, #156427 ) ;
#90025 = CARTESIAN_POINT ( 'NONE',  ( -0.6823417656250212460, 3.113541667008084879, 1.181850606188767472 ) ) ;
#90026 = CARTESIAN_POINT ( 'NONE',  ( 6.162552467866693640, -0.7048080804108979303, -1.831077584432870609 ) ) ;
#90027 = CARTESIAN_POINT ( 'NONE',  ( 8.535021395002688749, 9.916278701380017324, 1.199719254218462483 ) ) ;
#90028 = CARTESIAN_POINT ( 'NONE',  ( 11.87815913191726480, 11.30307820631413307, 1.708869976696563597 ) ) ;
#90029 = CARTESIAN_POINT ( 'NONE',  ( -8.876521693626852283, 3.555461883994700312, -7.992456032239074304 ) ) ;
#90030 = CARTESIAN_POINT ( 'NONE',  ( -3.741160322367112379, 6.452105245148518797, 1.199719254218464037 ) ) ;
#90031 = CARTESIAN_POINT ( 'NONE',  ( -5.019256313770280364, 7.854014895727056356, -1.116509978709074202 ) ) ;
#90032 = CARTESIAN_POINT ( 'NONE',  ( 2.330607996690749140, -1.275545549462468120, 1.630658604070814199 ) ) ;
#90033 = CARTESIAN_POINT ( 'NONE',  ( 0.7499999999999885647, 3.066666666666689522, -1.299038105676658228 ) ) ;
#90034 = CARTESIAN_POINT ( 'NONE',  ( 6.173040012923759257, 6.096301524699504704, -0.7998128361456281477 ) ) ;
#90035 = CARTESIAN_POINT ( 'NONE',  ( 5.225741863424510747, 5.061396693608882558, 0.7998128361456352531 ) ) ;
#90036 = CARTESIAN_POINT ( 'NONE',  ( 6.182307711929101224, 1.089732742074623006, 1.818925385317768928 ) ) ;
#90037 = DIRECTION ( 'NONE',  ( 0.000000000000000000, 0.000000000000000000, 1.000000000000000000 ) ) ;
#90038 = EDGE_CURVE ( 'NONE', #65799, #13808, #103671, .T. ) ;
#90039 = CARTESIAN_POINT ( 'NONE',  ( -1.201851678989727383E-14, 3.696875000341422801, -1.575800808251660134 ) ) ;
#90041 = CARTESIAN_POINT ( 'NONE',  ( 10.07334494527360569, 10.85458331234846696, 0.000000000000000000 ) ) ;
#90040 = CARTESIAN_POINT ( 'NONE',  ( 0.07479286986305545837, 0.7422478802248284602, -1.939684878352589070 ) ) ;
#90042 = CARTESIAN_POINT ( 'NONE',  ( 5.659529772124847646, -0.4871306767523299608, -1.956261131662299535 ) ) ;
#90043 = CARTESIAN_POINT ( 'NONE',  ( 5.858580540861003882, -1.821332666672281553, -0.5942308157336049224 ) ) ;
#90044 = CARTESIAN_POINT ( 'NONE',  ( 6.539320575229258026, 7.052651068779801413, 2.601414540040230428 ) ) ;
#90045 = CARTESIAN_POINT ( 'NONE',  ( 3.579775959861815515, -1.078688530630707243, 1.907616655872627964 ) ) ;
#90046 = CARTESIAN_POINT ( 'NONE',  ( -1.500000000000013101, 1.952083334016152527, 0.8660254037844403729 ) ) ;
#90047 = CARTESIAN_POINT ( 'NONE',  ( 2.004032382285144021, -0.8144628449315849394, 1.730399521388835460 ) ) ;
#90048 = CARTESIAN_POINT ( 'NONE',  ( -6.878064000834399394, 6.918829510595249310, -0.7998128361456291469 ) ) ;
#90049 = EDGE_CURVE ( 'NONE', #44585, #20115, #91603, .T. ) ;
#90050 = CARTESIAN_POINT ( 'NONE',  ( 4.812781342726858647, 6.637997537979888563, 1.443375672974062551 ) ) ;
#90052 = CARTESIAN_POINT ( 'NONE',  ( 6.169547404874395014, 1.460173559465412829, 1.533355976833279621 ) ) ;
#90051 = DIRECTION ( 'NONE',  ( -7.387867266669436732E-31, 1.000000000000000000, 8.546850786086424434E-32 ) ) ;
#90053 = CARTESIAN_POINT ( 'NONE',  ( -0.6823417656250003738, 9.713541667008065872, 1.181850606188754593 ) ) ;
#90055 = CARTESIAN_POINT ( 'NONE',  ( -7.117104292530948229, 7.267986194233038155, -0.7998128361456362523 ) ) ;
#90054 = CARTESIAN_POINT ( 'NONE',  ( 6.497619750234602698, -2.191128968173004843, 0.05151875470104508997 ) ) ;
#90057 = ORIENTED_EDGE ( 'NONE', *, *, #63333, .F. ) ;
#90056 = CARTESIAN_POINT ( 'NONE',  ( 3.346439682166453711, 0.4181539295537542444, 1.673179028346531538 ) ) ;
#90058 = CARTESIAN_POINT ( 'NONE',  ( -1.532927541463133592, -1.041115454748546609, 1.384885517283066525 ) ) ;
#90059 = CARTESIAN_POINT ( 'NONE',  ( 6.259060471003163428, 10.45398764947904624, -0.7998128361456291469 ) ) ;
#90060 = CARTESIAN_POINT ( 'NONE',  ( 3.649115900372475796, 7.409052317076538330, 1.040834085586084257E-14 ) ) ;
#90061 = CARTESIAN_POINT ( 'NONE',  ( 0.2913577194270203785, -1.795273245208812485, 0.7915465721433642132 ) ) ;
#90062 = CARTESIAN_POINT ( 'NONE',  ( 5.727393547130178675, 5.646656991265468939, 0.000000000000000000 ) ) ;
#90063 = CARTESIAN_POINT ( 'NONE',  ( 5.843727902690005749, 6.776436293681846301, -1.199719254218445830 ) ) ;
#90064 = CARTESIAN_POINT ( 'NONE',  ( -3.147653791585729444, 8.920000000000001705, 2.419999999999999485 ) ) ;
#90065 = VERTEX_POINT ( 'NONE', #122132 ) ;
#90066 = ORIENTED_EDGE ( 'NONE', *, *, #211523, .F. ) ;
#90067 = CARTESIAN_POINT ( 'NONE',  ( 2.824650661615616620, 1.310593810787925362, -1.250744805450889618 ) ) ;
#90068 = ORIENTED_EDGE ( 'NONE', *, *, #157243, .F. ) ;
#90069 = CARTESIAN_POINT ( 'NONE',  ( 9.622536337397022521, 12.24937836509514710, 1.599625672291281386 ) ) ;
#90070 = CARTESIAN_POINT ( 'NONE',  ( 4.411198876399872404, 6.239761003923544713, -1.599625672291273171 ) ) ;
#90071 = CARTESIAN_POINT ( 'NONE',  ( 4.020002786455856736, -1.806352922022226304, 0.1370799816429474904 ) ) ;
#90072 = CARTESIAN_POINT ( 'NONE',  ( 7.065207446052794715, 9.336104335185329006, -1.443375672974064550 ) ) ;
#90073 = CARTESIAN_POINT ( 'NONE',  ( 11.01135777277262484, 13.50498644914894086, -1.400000000000001243 ) ) ;
#90074 = CARTESIAN_POINT ( 'NONE',  ( 4.959245870426344460, 6.614204113168008270, 1.243730795111185339 ) ) ;
#90076 = CARTESIAN_POINT ( 'NONE',  ( 0.6823417656249934904, 14.69270833367473195, 1.181850606188764807 ) ) ;
#90075 = CARTESIAN_POINT ( 'NONE',  ( 4.949569884170424316, 1.378596123743974555, 1.250361270004763714 ) ) ;
#90077 = CARTESIAN_POINT ( 'NONE',  ( 2.126450742919711256, 0.4219061677965991741, 1.868383228629175719 ) ) ;
#90078 = CARTESIAN_POINT ( 'NONE',  ( 1.377666516899571647, 1.084121917808708035, 1.468671923017292658 ) ) ;
#90079 = CARTESIAN_POINT ( 'NONE',  ( 4.674980212565337467, 8.274328803998008297, 0.5478015097085631169 ) ) ;
#90080 = CARTESIAN_POINT ( 'NONE',  ( -10.44369227015510404, 5.112964020592957404, 5.232143560358708534 ) ) ;
#90081 = EDGE_CURVE ( 'NONE', #66250, #105059, #209157, .T. ) ;
#90082 = CARTESIAN_POINT ( 'NONE',  ( 6.233692552841108458, 6.917895963632635592, 0.8214459722771473293 ) ) ;
#90083 = CARTESIAN_POINT ( 'NONE',  ( 9.644012019580303630, 13.59213021077435535, 8.211487644058824031 ) ) ;
#90084 = CARTESIAN_POINT ( 'NONE',  ( -3.668686106071647579, 7.354262979464277095, -0.2566626154702719154 ) ) ;
#90085 = CARTESIAN_POINT ( 'NONE',  ( -9.305047017617200211, 15.51845925588232333, -7.449999999995526423 ) ) ;
#90086 = CARTESIAN_POINT ( 'NONE',  ( 6.263503779833467178, 9.290876262238963790, -1.082531754730537088 ) ) ;
#90087 = CARTESIAN_POINT ( 'NONE',  ( -5.278201874421821316, 5.052323696447222900, 0.7998128361456341429 ) ) ;
#90088 = CARTESIAN_POINT ( 'NONE',  ( 1.201248573238463235, -0.5064915201186767080, 2.028225233004859351 ) ) ;
#90089 = CARTESIAN_POINT ( 'NONE',  ( 6.229514091203088633, -1.813738808949336478, 0.6494875524521417365 ) ) ;
#90090 = CARTESIAN_POINT ( 'NONE',  ( -7.040761844198392794, 7.108643661186573759, -0.7998128361456291469 ) ) ;
#90091 = CARTESIAN_POINT ( 'NONE',  ( 2.766400663125650361, -1.260407102598060103, 1.320874842943790872 ) ) ;
#90092 = CARTESIAN_POINT ( 'NONE',  ( 3.053566222061272040, -1.804402116661915967, -1.270350324234906125 ) ) ;
#90093 = CARTESIAN_POINT ( 'NONE',  ( -9.508009452559559094, 15.00000000000599343, 7.612499999990692601 ) ) ;
#90094 = CARTESIAN_POINT ( 'NONE',  ( 1.142663480069527671, 1.843847066288730074, 0.5072560978593986247 ) ) ;
#90095 = CARTESIAN_POINT ( 'NONE',  ( 1.767950473188628857, -1.955055593144053194, 0.2378005183036585035 ) ) ;
#90096 = CARTESIAN_POINT ( 'NONE',  ( 2.313922598539425390, 1.266723153581908567, -1.472183398282415956 ) ) ;
#90097 = ORIENTED_EDGE ( 'NONE', *, *, #15281, .F. ) ;
#90098 = DIRECTION ( 'NONE',  ( -0.1664974550714433121, -0.9062754367152189294, 0.3885143887443193722 ) ) ;
#90100 = CARTESIAN_POINT ( 'NONE',  ( 6.420743829754993470, -1.316656903452334992, 1.315380689086578236 ) ) ;
#90099 = CARTESIAN_POINT ( 'NONE',  ( -3.969505113751027547, 7.853116076009993840, 1.214306433183764966E-14 ) ) ;
#90101 = CARTESIAN_POINT ( 'NONE',  ( 4.050854035433010480, 7.948023151305657841, 0.000000000000000000 ) ) ;
#90102 = CARTESIAN_POINT ( 'NONE',  ( -11.45846087878769559, 13.59311600781440887, -3.566076377698187194 ) ) ;
#90103 = CARTESIAN_POINT ( 'NONE',  ( 1.000000000000003553, 6.180000000000018368, 1.214306433183764966E-14 ) ) ;
#90104 = CARTESIAN_POINT ( 'NONE',  ( -6.459533842268148973, 6.500820668926428958, 0.000000000000000000 ) ) ;
#90105 = CARTESIAN_POINT ( 'NONE',  ( 2.419692422129790632, -1.264489869534379141, -1.789777738334753732 ) ) ;
#90106 = DIRECTION ( 'NONE',  ( -3.451266460341926649E-31, -5.200009205990155575E-32, 1.000000000000000000 ) ) ;
#90107 = EDGE_LOOP ( 'NONE', ( #190086, #6420 ) ) ;
#90108 = CARTESIAN_POINT ( 'NONE',  ( 7.225569521440261767, 7.394528961293920233, -0.7998128361456341429 ) ) ;
#90109 = CARTESIAN_POINT ( 'NONE',  ( -1.219999999999995977, 6.400000000000024336, 1.214306433183764966E-14 ) ) ;
#90110 = CARTESIAN_POINT ( 'NONE',  ( 4.037589748876240670, -1.260430739550026269, -1.321009972365666307 ) ) ;
#90111 = CARTESIAN_POINT ( 'NONE',  ( 3.834746474454188013E-15, 13.09375000068279959, 1.500000000000001554 ) ) ;
#90112 = CARTESIAN_POINT ( 'NONE',  ( -9.002250809793991948, 12.48608113052627289, -1.082531754730543971 ) ) ;
#90113 = CARTESIAN_POINT ( 'NONE',  ( -4.609429383499759503, 8.467968972964683871, -0.3232828671759068739 ) ) ;
#90114 = CARTESIAN_POINT ( 'NONE',  ( -0.02968770228140016343, 1.391517546076680434, -2.083419219542380407 ) ) ;
#90115 = ADVANCED_FACE ( 'NONE', ( #3990 ), #67915, .F. ) ;
#90116 = CARTESIAN_POINT ( 'NONE',  ( 8.911787042884274257, 9.291506392986812912, 0.7998128361456462443 ) ) ;
#90117 = CARTESIAN_POINT ( 'NONE',  ( 2.666528119303875233, -1.328299865307873695, 1.395581591625531193 ) ) ;
#90118 = CARTESIAN_POINT ( 'NONE',  ( 6.983263157960366563, -0.003091553303710344557, 1.945923119799706669 ) ) ;
#90119 = CARTESIAN_POINT ( 'NONE',  ( -6.009258394948636914E-15, 14.43750000000000355, -1.732050807568875195 ) ) ;
#90120 = CARTESIAN_POINT ( 'NONE',  ( -6.738566041191992539, 7.820414121934134322, 1.199719254218450271 ) ) ;
#90121 = CARTESIAN_POINT ( 'NONE',  ( 4.660252114795294887, 6.460046772059735432, -1.599625672291256295 ) ) ;
#90122 = CARTESIAN_POINT ( 'NONE',  ( -5.600926855776901192, 5.707038551260711579, -0.7216878364870338292 ) ) ;
#90123 = CARTESIAN_POINT ( 'NONE',  ( 0.3513568635829470432, 0.2028739153508585802, -2.107475566755373730 ) ) ;
#90124 = CARTESIAN_POINT ( 'NONE',  ( 8.866142388332804103, 12.43125098877526113, -1.199719254218446718 ) ) ;
#90125 = DIRECTION ( 'NONE',  ( 1.000000000000000000, 0.000000000000000000, 0.000000000000000000 ) ) ;
#90126 = CARTESIAN_POINT ( 'NONE',  ( 5.014543041041934046, 0.7873211189074662553, 1.914903133430221338 ) ) ;
#90128 = CARTESIAN_POINT ( 'NONE',  ( -1.364683531249997417, 2.821875000341422801, 1.214306433183764966E-14 ) ) ;
#90127 = CARTESIAN_POINT ( 'NONE',  ( 0.2746299231596514012, 1.718356743839201561, -0.6618312839273902126 ) ) ;
#90129 = ORIENTED_EDGE ( 'NONE', *, *, #117742, .T. ) ;
#90130 = CARTESIAN_POINT ( 'NONE',  ( 5.344470762249110329, 0.4509167475243852086, -2.253899259558800772 ) ) ;
#90131 = CARTESIAN_POINT ( 'NONE',  ( 6.399085315970131305, 8.488685506763726352, -1.443375672974057666 ) ) ;
#90133 = CARTESIAN_POINT ( 'NONE',  ( -1.162044386198238837E-16, 1.437500000000019540, -1.225000000000020739 ) ) ;
#90132 = CARTESIAN_POINT ( 'NONE',  ( 5.777182853198898904, 6.873039762554409293, -1.082531754730548412 ) ) ;
#90134 = CARTESIAN_POINT ( 'NONE',  ( 0.5863596474044476814, -2.275655805637688989, -0.2749888630660061728 ) ) ;
#90135 = LINE ( 'NONE', #157267, #46825 ) ;
#90136 = CARTESIAN_POINT ( 'NONE',  ( -6.587282531393266360, 8.778525268082516320, 1.599625672291269396 ) ) ;
#90137 = CARTESIAN_POINT ( 'NONE',  ( 5.314377360232536596, 1.795021767651948208, 0.7414505486388212052 ) ) ;
#90138 = ORIENTED_EDGE ( 'NONE', *, *, #17565, .F. ) ;
#90139 = CARTESIAN_POINT ( 'NONE',  ( 8.554831740098654436, 11.00372300158037042, 1.443375672974076540 ) ) ;
#90140 = EDGE_LOOP ( 'NONE', ( #101618, #107464, #205281, #30679 ) ) ;
#90141 = CARTESIAN_POINT ( 'NONE',  ( 0.03540237040386850359, -0.09474447662855033092, 2.011072404829179483 ) ) ;
#90142 = CARTESIAN_POINT ( 'NONE',  ( 0.2930059409478984467, 1.274291793118907723, 1.162708412170476713 ) ) ;
#90143 = CARTESIAN_POINT ( 'NONE',  ( 5.507046092540283766, -0.04465857163906890998, 2.016188657829049991 ) ) ;
#90145 = CYLINDRICAL_SURFACE ( 'NONE', #119520, 0.3999999999999993006 ) ;
#90144 = CARTESIAN_POINT ( 'NONE',  ( -8.317037166979361018, 11.79062823052953668, 1.199719254218453823 ) ) ;
#90146 = CARTESIAN_POINT ( 'NONE',  ( 3.285556943750000070, -2.121874999522044281, 0.000000000000000000 ) ) ;
#90148 = CARTESIAN_POINT ( 'NONE',  ( 0.7074158718562081338, -1.761916611671160204, 0.1673130110368889201 ) ) ;
#90147 = CARTESIAN_POINT ( 'NONE',  ( 2.519574111291386309, -1.204466598365286023, -1.708601439550963663 ) ) ;
#90149 = CARTESIAN_POINT ( 'NONE',  ( 11.01135777277262306, 10.19999999999998153, 1.399999999999998579 ) ) ;
#90151 = CARTESIAN_POINT ( 'NONE',  ( 4.242302733825270344, 0.6093012942862492398, 2.209731468575569124 ) ) ;
#90150 = CARTESIAN_POINT ( 'NONE',  ( 4.706615602599436343, 5.520081620234675412, 1.199719254218452935 ) ) ;
#90152 = CARTESIAN_POINT ( 'NONE',  ( 2.730071887686904564, 0.2129287318765031578, 1.727178079207219552 ) ) ;
#90153 = CARTESIAN_POINT ( 'NONE',  ( 3.192055101013606233, 5.811482486902795230, -1.199719254218446718 ) ) ;
#90154 = PRESENTATION_LAYER_ASSIGNMENT (  '', '', ( #183515 ) ) ;
#90155 = CARTESIAN_POINT ( 'NONE',  ( 3.234745892528373634, 1.342314639517484087, -1.641720766639111817 ) ) ;
#90156 = CARTESIAN_POINT ( 'NONE',  ( 11.78331023100045627, 12.22000000000000064, -1.800000000000001155 ) ) ;
#90157 = CARTESIAN_POINT ( 'NONE',  ( 1.791952614948258304, -1.634470817638247642, 0.5789770405969245637 ) ) ;
#90158 = CARTESIAN_POINT ( 'NONE',  ( 0.6801582343749970061, 2.505208333674749266, 1.178068619123801675 ) ) ;
#90159 = CARTESIAN_POINT ( 'NONE',  ( 1.134942894344723507, -0.04051261866679262136, -1.860784445789311903 ) ) ;
#90160 = CARTESIAN_POINT ( 'NONE',  ( 2.453800908837290518, 1.677244079947149302, 1.378686777781912065 ) ) ;
#90161 = CARTESIAN_POINT ( 'NONE',  ( 6.308621549060418054, 6.254479983525607523, 0.7998128361456341429 ) ) ;
#90162 = CARTESIAN_POINT ( 'NONE',  ( 3.942592416894859841, -1.490970858180175940, 1.357867534901323614 ) ) ;
#90163 = CARTESIAN_POINT ( 'NONE',  ( 1.562500000000001554, -1.451031289061184282, -1.451031289061057050 ) ) ;
#90164 = CARTESIAN_POINT ( 'NONE',  ( 0.7499999999999902300, 3.264583334016149418, 1.299038105676669330 ) ) ;
#90165 = CARTESIAN_POINT ( 'NONE',  ( 1.395397119253296569, 1.457039974399224391, 1.260252556074402897 ) ) ;
#90166 = CARTESIAN_POINT ( 'NONE',  ( 1.364683531250000303, 13.75520833367473195, -0.7879004041258355073 ) ) ;
#90167 = CARTESIAN_POINT ( 'NONE',  ( 4.096076364168971473, 1.452574950358286765, 1.680725415074139306 ) ) ;
#90168 = VERTEX_POINT ( 'NONE', #2921 ) ;
#90169 = DIRECTION ( 'NONE',  ( 0.000000000000000000, 0.000000000000000000, -1.000000000000000000 ) ) ;
#90170 = CARTESIAN_POINT ( 'NONE',  ( 1.499999999999985123, 0.5458333333333577064, -0.8660254037844253849 ) ) ;
#90171 = CARTESIAN_POINT ( 'NONE',  ( 8.437251666405968464, 8.737881787095446384, 1.040834085586084257E-14 ) ) ;
#90172 = CARTESIAN_POINT ( 'NONE',  ( -1.364683531250014514, -0.2614583329919080157, -0.7879004041258359514 ) ) ;
#90173 = CARTESIAN_POINT ( 'NONE',  ( 5.871364357536254630, -1.904906058150414472, -1.142540087918672898 ) ) ;
#90176 = EDGE_CURVE ( 'NONE', #211530, #53040, #92263, .T. ) ;
#90175 = CARTESIAN_POINT ( 'NONE',  ( 4.668382477721988444, -0.8370036265390871089, -1.774476930476886594 ) ) ;
#90174 = AXIS2_PLACEMENT_3D ( 'NONE', #127244, #195357, #209440 ) ;
#90177 = PRODUCT_RELATED_PRODUCT_CATEGORY ( 'part', '', ( #29899 ) ) ;
#90178 = CARTESIAN_POINT ( 'NONE',  ( 9.083599731475983319, 11.62061899152058686, 1.443375672974076540 ) ) ;
#90179 = CARTESIAN_POINT ( 'NONE',  ( 0.4917504562594980921, 10.46609003534429050, 2.500000000000000444 ) ) ;
#90180 = CARTESIAN_POINT ( 'NONE',  ( 5.888003241735360938, -1.025016604251761221, 2.016990234832950701 ) ) ;
#90181 = CARTESIAN_POINT ( 'NONE',  ( -4.936577329151611515, 7.813071746435248599, 1.082531754730549967 ) ) ;
#90182 = CARTESIAN_POINT ( 'NONE',  ( 3.455586768955606125, 1.624414792841613941, 1.271063249801159145 ) ) ;
#90183 = CARTESIAN_POINT ( 'NONE',  ( -4.934277840369690971, 7.844075682818238526, -1.199719254218452047 ) ) ;
#90184 = CARTESIAN_POINT ( 'NONE',  ( -1.201851678989727383E-14, 2.493750000682819046, 1.732050807568877637 ) ) ;
#90185 = CARTESIAN_POINT ( 'NONE',  ( -1.364683531249997417, 5.321875000341417916, 1.214306433183764966E-14 ) ) ;
#90186 = CARTESIAN_POINT ( 'NONE',  ( 4.798043669735932326, -1.870115615568968881, -0.04763329477865811679 ) ) ;
#90187 = CARTESIAN_POINT ( 'NONE',  ( 3.199597886960439119, 1.569373658825726769, 0.7380672391785416675 ) ) ;
#90188 = CARTESIAN_POINT ( 'NONE',  ( 3.298151293307958642, 1.369808456162135091, -1.073517941977668588 ) ) ;
#90189 = CARTESIAN_POINT ( 'NONE',  ( 0.7324523162463879578, 2.259705603777485639, 0.3848113418177290801 ) ) ;
#90190 = CARTESIAN_POINT ( 'NONE',  ( 1.061882456046374434, 0.4290601450722114074, -2.164491299336705588 ) ) ;
#90191 = CARTESIAN_POINT ( 'NONE',  ( 4.423432795095141756, -1.287707899167778169, -1.647015592753127589 ) ) ;
#90192 = CARTESIAN_POINT ( 'NONE',  ( 5.683525053321154985, -0.8713906080477454852, 1.735537339962249792 ) ) ;
#90194 = VERTEX_POINT ( 'NONE', #104741 ) ;
#90193 = CARTESIAN_POINT ( 'NONE',  ( 9.181860203497647532, 14.16078059704854653, 7.658820650071877623 ) ) ;
#90195 = CARTESIAN_POINT ( 'NONE',  ( 0.6510177983308338412, 0.9963039324867200008, 1.753029211773032392 ) ) ;
#90196 = DIRECTION ( 'NONE',  ( 0.000000000000000000, -7.228014483236694583E-17, 1.000000000000000000 ) ) ;
#90197 = CARTESIAN_POINT ( 'NONE',  ( 6.592432824109000222, -0.4393352932590722792, 1.975308225066509049 ) ) ;
#90198 = CARTESIAN_POINT ( 'NONE',  ( -7.316596452869116973, 11.68777962832266049, 0.7998128361456481317 ) ) ;
#90199 = CARTESIAN_POINT ( 'NONE',  ( 7.145310649601935182, 8.294949498412453437, -1.199719254218446718 ) ) ;
#90200 = SURFACE_SIDE_STYLE ('',( #24097 ) ) ;
#90201 = CARTESIAN_POINT ( 'NONE',  ( 3.896943178251357054, 1.541351720387572843, -0.9781566455248569270 ) ) ;
#90202 = ORIENTED_EDGE ( 'NONE', *, *, #102912, .F. ) ;
#90203 = CARTESIAN_POINT ( 'NONE',  ( -5.112833325684928987, 5.137596099486740897, -0.7216878364870338292 ) ) ;
#90204 = CARTESIAN_POINT ( 'NONE',  ( -0.09463244300326445479, -8.038540703696433809, -9.499633399276474321 ) ) ;
#90205 = CARTESIAN_POINT ( 'NONE',  ( 3.285556943750000070, -1.771874999522041083, 0.000000000000000000 ) ) ;
#90206 = CARTESIAN_POINT ( 'NONE',  ( -8.193204901359996128, 8.453160561208463264, 1.040834085586084257E-14 ) ) ;
#90207 = CARTESIAN_POINT ( 'NONE',  ( 2.601824576204377681, 1.431331034542600245, 1.425341822903106515 ) ) ;
#90208 = CARTESIAN_POINT ( 'NONE',  ( -3.637330350216213759, 7.465578851886037093, -0.7998128361456481317 ) ) ;
#90209 = CARTESIAN_POINT ( 'NONE',  ( 2.694024576921652425, 0.8818583146339260548, -1.638763372900291726 ) ) ;
#90210 = CARTESIAN_POINT ( 'NONE',  ( 9.622536337397022521, 12.24937836509514710, 1.599625672291281386 ) ) ;
#90211 = CARTESIAN_POINT ( 'NONE',  ( -0.4214947629263258722, 3.038568440852373875, -0.4183962726259458642 ) ) ;
#90212 = CARTESIAN_POINT ( 'NONE',  ( -3.903858165731105778, 6.641919395739846799, 1.199719254218464037 ) ) ;
#90213 = AXIS2_PLACEMENT_3D ( 'NONE', #46227, #62451, #78693 ) ;
#90214 = CARTESIAN_POINT ( 'NONE',  ( -8.779068160048691283, 10.20099992726700933, -1.199719254218446718 ) ) ;
#90215 = CARTESIAN_POINT ( 'NONE',  ( 5.549374350267230582, -1.441814640532925074, -1.119852386600270533 ) ) ;
#90217 = CARTESIAN_POINT ( 'NONE',  ( -4.520189846367452802, 7.221058948360024488, -1.319278014013465894 ) ) ;
#90216 = CARTESIAN_POINT ( 'NONE',  ( -7.587723245503481095, 8.881373870289390737, 1.199719254218452047 ) ) ;
#90218 = CARTESIAN_POINT ( 'NONE',  ( 6.007156502879952953, 7.179297369210805080, -1.191424252104013037 ) ) ;
#90219 = CARTESIAN_POINT ( 'NONE',  ( 0.8074296549154248437, -1.491244094015523602, 0.8842416791710568935 ) ) ;
#90220 = CARTESIAN_POINT ( 'NONE',  ( 0.05802509242504564485, -1.552030147408272054, -0.7874549631982865616 ) ) ;
#90221 = CARTESIAN_POINT ( 'NONE',  ( 5.215558013723960329, -0.3431011331927047991, 2.281934296042067878 ) ) ;
#90222 = CARTESIAN_POINT ( 'NONE',  ( 6.229045230835819069, 6.231917288922055320, -0.7998128361456481317 ) ) ;
#90223 = CARTESIAN_POINT ( 'NONE',  ( 0.3509462063632540763, -1.656586674793923075, 1.225593781303188967 ) ) ;
#90224 = CARTESIAN_POINT ( 'NONE',  ( 4.659198344590585350, 8.587481835331020719, 0.7998128361456462443 ) ) ;
#90225 = CARTESIAN_POINT ( 'NONE',  ( 5.888098204360154853, -0.06530352750959941832, 2.297622472229691404 ) ) ;
#90226 = CARTESIAN_POINT ( 'NONE',  ( 3.642287698956242714, 3.120124397465485533, 2.500000000001089795 ) ) ;
#90227 = CARTESIAN_POINT ( 'NONE',  ( -7.435720902452096936, 7.639705572474380091, 0.000000000000000000 ) ) ;
#90228 = CARTESIAN_POINT ( 'NONE',  ( 5.278141497218024725, -1.038406966791558528, 1.555765341417144842 ) ) ;
#90230 = CARTESIAN_POINT ( 'NONE',  ( -4.228163802615396705, 6.026220084508304708, -1.599625672291271394 ) ) ;
#90229 = CARTESIAN_POINT ( 'NONE',  ( 3.111475685156277038, 1.510342251817019532, 1.173009309769344588 ) ) ;
#90231 = CARTESIAN_POINT ( 'NONE',  ( 5.197975494389605267, -0.7968864405506062010, 2.058166701804148957 ) ) ;
#90232 = CARTESIAN_POINT ( 'NONE',  ( 4.382099326012149909, -2.116931447088743923, -0.04843129487230694169 ) ) ;
#90233 = CARTESIAN_POINT ( 'NONE',  ( -0.6125000000000279110, 1.104166667349484765, 1.060881119635904923 ) ) ;
#90234 = CARTESIAN_POINT ( 'NONE',  ( 6.983263157960393208, 0.5798717822590447879, 1.998431770337566027 ) ) ;
#90235 = CARTESIAN_POINT ( 'NONE',  ( 4.692530563661249765, 8.488719734331187539, 0.000000000000000000 ) ) ;
#90236 = CARTESIAN_POINT ( 'NONE',  ( -6.278834536460198734, 6.497930845391236332, 0.7216878364870257245 ) ) ;
#90237 = CARTESIAN_POINT ( 'NONE',  ( 5.549516566986255839, -1.916978305411633166, 0.9067721062034905799 ) ) ;
#90238 = CARTESIAN_POINT ( 'NONE',  ( 2.310004868091195540, -0.5052997711322243513, 2.251431844744283151 ) ) ;
#90239 = CARTESIAN_POINT ( 'NONE',  ( 3.367582429956605061, -0.3852447139683997657, 1.923494667983568718 ) ) ;
#90240 = CARTESIAN_POINT ( 'NONE',  ( 6.438341905586414171, -1.108352981827376738, 1.739313939070710857 ) ) ;
#90241 = CARTESIAN_POINT ( 'NONE',  ( 4.867013957625893283, 4.780530493426062399, 1.040834085586084257E-14 ) ) ;
#90242 = CARTESIAN_POINT ( 'NONE',  ( 3.390420931869152721, 6.113185632892752075, -1.199719254218452047 ) ) ;
#90243 = EDGE_LOOP ( 'NONE', ( #151294, #125272, #166971, #170213 ) ) ;
#90244 = CARTESIAN_POINT ( 'NONE',  ( 5.876185452347599814, -2.007255679753978228, -0.1928398672442974138 ) ) ;
#90245 = CARTESIAN_POINT ( 'NONE',  ( -9.833741488613570780, 10.36711991300432345, 0.7998128361456462443 ) ) ;
#90246 = CARTESIAN_POINT ( 'NONE',  ( -4.490256990713600516, 8.252036901523048584, -0.03636953492806980354 ) ) ;
#90247 = CARTESIAN_POINT ( 'NONE',  ( -10.45142682343936791, 5.144546645612242841, 5.216777551074719632 ) ) ;
#90248 = CARTESIAN_POINT ( 'NONE',  ( 2.061612764771907802, 1.803244147071264125, 1.208790786097496905 ) ) ;
#90249 = CARTESIAN_POINT ( 'NONE',  ( -1.854512760316423536, 2.488359591189891251, 2.484105960264900936 ) ) ;
#90250 = CARTESIAN_POINT ( 'NONE',  ( -0.7500000000000006661, 1.889583334016155192, -1.299038105676652011 ) ) ;
#90251 = CARTESIAN_POINT ( 'NONE',  ( -4.797639982484825261, 14.48151998951723662, -11.00824919581360817 ) ) ;
#90252 = CARTESIAN_POINT ( 'NONE',  ( -7.960263458884766052, -6.452016312668098941, 7.960263458884793586 ) ) ;
#90253 = CARTESIAN_POINT ( 'NONE',  ( 5.644368669187761256, 7.458116220610145675, 1.329639117314229235 ) ) ;
#90254 = CARTESIAN_POINT ( 'NONE',  ( 1.212264220565926198, -0.9239156619155285410, -1.842110158844072698 ) ) ;
#90256 = CARTESIAN_POINT ( 'NONE',  ( 6.727182134110200273, 2.469373133786161745, 2.195552656936059055 ) ) ;
#90255 = CARTESIAN_POINT ( 'NONE',  ( -10.65400978224035811, 11.32409958890225710, 1.040834085586084257E-14 ) ) ;
#90257 = CARTESIAN_POINT ( 'NONE',  ( -1.402160292154681736E-14, 0.4468750003414233563, -1.575800808251665908 ) ) ;
#90258 =( LENGTH_UNIT ( ) NAMED_UNIT ( * ) SI_UNIT ( .MILLI., .METRE. ) );
#90259 = ORIENTED_EDGE ( 'NONE', *, *, #139074, .F. ) ;
#90260 = CARTESIAN_POINT ( 'NONE',  ( 3.422422624566554994, -0.7774026117220147469, -1.747318718686732497 ) ) ;
#90261 = CARTESIAN_POINT ( 'NONE',  ( 5.348444421042818142, 0.5165251424982686412, 1.692803071163173634 ) ) ;
#90262 = CARTESIAN_POINT ( 'NONE',  ( 6.873057527484919937, 6.983264968346048818, 0.7998128361456352531 ) ) ;
#90263 = CARTESIAN_POINT ( 'NONE',  ( -4.874319919312905647, 5.645460313075203018, -1.199719254218446718 ) ) ;
#90264 = CARTESIAN_POINT ( 'NONE',  ( 0.1404700283944440298, 1.733558474490008772, 0.5260085833052421389 ) ) ;
#90266 = CARTESIAN_POINT ( 'NONE',  ( 6.521099267210373363, -1.708630446951715731, 0.8662611975780337703 ) ) ;
#90265 = DIRECTION ( 'NONE',  ( 3.491481338843133355E-15, 0.000000000000000000, 1.000000000000000000 ) ) ;
#90267 = CARTESIAN_POINT ( 'NONE',  ( 1.275928261265106833, -2.020323679977220621, 0.4517519998969782291 ) ) ;
#90268 = CARTESIAN_POINT ( 'NONE',  ( -0.7499999999999972244, 5.858333333333353821, -1.299038105676652011 ) ) ;
#90269 = CARTESIAN_POINT ( 'NONE',  ( 5.963714631206167738, 1.842656449598079060, -0.3214700631931910468 ) ) ;
#90270 = CARTESIAN_POINT ( 'NONE',  ( 2.859763506297557711, 1.816872213737670938, -0.1792109616642542924 ) ) ;
#90272 = CARTESIAN_POINT ( 'NONE',  ( 6.457572779797339457, 6.769951385671206801, 0.3193968722623799494 ) ) ;
#90271 = CARTESIAN_POINT ( 'NONE',  ( 6.164705905600972535, -1.563586322211576674, 1.557672334054376773 ) ) ;
#90273 = CARTESIAN_POINT ( 'NONE',  ( 0.6823417656249882723, 0.1760416670080894308, -1.181850606188749264 ) ) ;
#90274 = CARTESIAN_POINT ( 'NONE',  ( 3.209489602684848286, -1.684771875651757123, -1.189772946182314106 ) ) ;
#90275 = CARTESIAN_POINT ( 'NONE',  ( -8.037286134802835491, 8.271255333558444889, -0.7998128361456291469 ) ) ;
#90276 = CARTESIAN_POINT ( 'NONE',  ( 8.402302512167096893, 10.82577223566020841, -1.599625672291268286 ) ) ;
#90277 = CARTESIAN_POINT ( 'NONE',  ( 5.542585869888291938, 5.360771691158120689, -0.7998128361456211532 ) ) ;
#90278 = AXIS2_PLACEMENT_3D ( 'NONE', #15514, #134651, #65325 ) ;
#90279 = CARTESIAN_POINT ( 'NONE',  ( 0.3335754702045168330, -1.976410766185803691, 0.8757516042032786885 ) ) ;
#90280 = CARTESIAN_POINT ( 'NONE',  ( 6.566853775770633561, 1.536883091774071453, -1.387433097640700774 ) ) ;
#90281 = CARTESIAN_POINT ( 'NONE',  ( 1.364683531249988757, -0.3031249996585799744, 0.000000000000000000 ) ) ;
#90282 = CARTESIAN_POINT ( 'NONE',  ( 3.972077263441410100, 1.197190051160206936, 1.799587594625361220 ) ) ;
#90284 = CARTESIAN_POINT ( 'NONE',  ( 2.506241959165692812, 1.961374882610424919, 0.05109738790698423877 ) ) ;
#90283 = CARTESIAN_POINT ( 'NONE',  ( 4.582678730018482582, -1.317704446820912700, 1.530705718492784362 ) ) ;
#90285 = PRODUCT_DEFINITION_SHAPE ( 'NONE', 'NONE',  #128970 ) ;
#90288 = CARTESIAN_POINT ( 'NONE',  ( 6.724481002698112775, 8.868313807946373473, -1.443375672974057666 ) ) ;
#90287 = CARTESIAN_POINT ( 'NONE',  ( 1.737500000000001155, -0.2333333333333319215, 3.009438278150922130 ) ) ;
#90286 = DIRECTION ( 'NONE',  ( 0.000000000000000000, 0.000000000000000000, 1.000000000000000000 ) ) ;
#90289 = CARTESIAN_POINT ( 'NONE',  ( -6.957269102468015554, 8.145844036748005834, 1.199719254218452047 ) ) ;
#90290 = CARTESIAN_POINT ( 'NONE',  ( 2.009000277268524481, 0.004839059525654776373, 2.016708403978189956 ) ) ;
#90291 = CARTESIAN_POINT ( 'NONE',  ( -6.254388934605767503, 6.191208599995166040, 0.7998128361456341429 ) ) ;
#90292 = CARTESIAN_POINT ( 'NONE',  ( -1.499999999999997780, 5.431250000682820378, 1.214306433183764966E-14 ) ) ;
#90293 = CARTESIAN_POINT ( 'NONE',  ( 5.484596585704371030, -1.208295678440996390, 1.482354609825987213 ) ) ;
#90294 = CARTESIAN_POINT ( 'NONE',  ( -4.624346020613643304, 4.914118431181374369, -0.7231984802981470395 ) ) ;
#90295 = EDGE_CURVE ( 'NONE', #65269, #180121, #139062, .T. ) ;
#90297 = CARTESIAN_POINT ( 'NONE',  ( 3.181267708840180841, 1.591331833097202830, 1.238305487465785948 ) ) ;
#90296 = CARTESIAN_POINT ( 'NONE',  ( -7.931156673870055407, 11.23647130528163096, 1.082531754730549967 ) ) ;
#90298 = CARTESIAN_POINT ( 'NONE',  ( -1.201851678989727383E-14, 3.712500000000020339, 1.732050807568877637 ) ) ;
#90299 = CARTESIAN_POINT ( 'NONE',  ( -0.6823417656250003738, 14.96354166700806410, 1.181850606188754593 ) ) ;
#90300 = CARTESIAN_POINT ( 'NONE',  ( 6.124008131756068174, -0.9624739961165188484, -1.431025375277717115 ) ) ;
#90301 = CARTESIAN_POINT ( 'NONE',  ( 5.677832469072920496, 9.846164657218904992, 0.000000000000000000 ) ) ;
#90302 = CARTESIAN_POINT ( 'NONE',  ( 9.300530189294644146, 10.91333531134101165, -1.082531754730543083 ) ) ;
#90303 = AXIS2_PLACEMENT_3D ( 'NONE', #68946, #150242, #118855 ) ;
#90304 = DIRECTION ( 'NONE',  ( 1.535693738322999099E-12, 1.000000000000000000, -1.561558963378103181E-12 ) ) ;
#90305 = CARTESIAN_POINT ( 'NONE',  ( 3.901501827272614964, -0.5455803081039903857, 1.789184164884791706 ) ) ;
#90306 = CARTESIAN_POINT ( 'NONE',  ( 0.000000000000000000, -7.699999999999998401, 0.000000000000000000 ) ) ;
#90307 = CARTESIAN_POINT ( 'NONE',  ( 1.709917326824461181, 0.6048241955843024487, -1.979901091156407666 ) ) ;
#90308 = CARTESIAN_POINT ( 'NONE',  ( -7.444835747235459600, 8.818634805597074688, 1.082531754730549078 ) ) ;
#90309 = VERTEX_POINT ( 'NONE', #204321 ) ;
#90310 = CARTESIAN_POINT ( 'NONE',  ( 3.444653546323793947, 6.176457016423196222, 1.199719254218451159 ) ) ;
#90311 = DIRECTION ( 'NONE',  ( -0.9982742078614211811, 0.000000000000000000, -0.05872483221476467591 ) ) ;
#90312 = CARTESIAN_POINT ( 'NONE',  ( 5.383996397958233260, 5.453953017138946535, -0.7216878364870458196 ) ) ;
#90313 = CARTESIAN_POINT ( 'NONE',  ( 5.608569151319391821, 5.681340981270094126, 0.4042273303749412960 ) ) ;
#90314 = COLOUR_RGB ( '', 0.31764706, 0.68627451, 0.89019608) ;
#90315 = CARTESIAN_POINT ( 'NONE',  ( 7.090551149822722721, 11.21613407486112379, 0.7216878364870438212 ) ) ;
#90316 = CARTESIAN_POINT ( 'NONE',  ( 7.076466111328892694, 10.34329533227067799, -1.199719254218441611 ) ) ;
#90318 = CARTESIAN_POINT ( 'NONE',  ( 5.941025102908992217, -1.645668167864361431, -0.9802026474072849105 ) ) ;
#90317 = CARTESIAN_POINT ( 'NONE',  ( -5.717788096661253761, 7.693838750903348789, 1.599625672291269396 ) ) ;
#90319 = CARTESIAN_POINT ( 'NONE',  ( 6.727182134110222478, 0.005875948494733079785, 1.810970247402940547 ) ) ;
#90320 = CARTESIAN_POINT ( 'NONE',  ( 0.000000000000000000, -7.154544010627095219, 0.000000000000000000 ) ) ;
#90321 = EDGE_CURVE ( 'NONE', #205352, #165662, #130403, .T. ) ;
#90322 = CARTESIAN_POINT ( 'NONE',  ( 1.224999999999974998, 0.6041666666666989371, 0.7072540797572456350 ) ) ;
#90324 = ORIENTED_EDGE ( 'NONE', *, *, #25109, .T. ) ;
#90323 = CARTESIAN_POINT ( 'NONE',  ( 3.497640442645619796, 6.064035702186436616, -1.082531754730543083 ) ) ;
#90325 = CARTESIAN_POINT ( 'NONE',  ( -7.537970219518075332, 10.77775377520434574, -1.082531754730543971 ) ) ;
#90326 = CARTESIAN_POINT ( 'NONE',  ( 2.764712544972968811, -1.491509591961352132, 1.564943835847030007 ) ) ;
#90327 = CARTESIAN_POINT ( 'NONE',  ( -5.953438850176548947, 9.959779401932374654, 0.000000000000000000 ) ) ;
#90328 = CARTESIAN_POINT ( 'NONE',  ( 5.076602173674213070, 4.887400388900169368, 0.000000000000000000 ) ) ;
#90329 = CARTESIAN_POINT ( 'NONE',  ( 0.6156802735862786369, 1.737094954450137507, 1.216079458918501333 ) ) ;
#90330 = CARTESIAN_POINT ( 'NONE',  ( 5.456004705108882469, 1.823398332572896186, -0.09148835057352226741 ) ) ;
#90331 = CARTESIAN_POINT ( 'NONE',  ( 9.227664502431396798, 10.66305660167662595, 7.832549530788790015 ) ) ;
#90332 = CARTESIAN_POINT ( 'NONE',  ( 1.458210469330342374, 0.7952313087857125762, 1.804010633499957272 ) ) ;
#90333 = CARTESIAN_POINT ( 'NONE',  ( 3.515784362865181478, -0.5505564139345071606, 1.831456330389509501 ) ) ;
#90334 = ORIENTED_EDGE ( 'NONE', *, *, #137350, .T. ) ;
#90335 = DIRECTION ( 'NONE',  ( -0.000000000000000000, -8.546850786086437571E-32, -1.000000000000000000 ) ) ;
#90336 = CARTESIAN_POINT ( 'NONE',  ( 5.002387483831562953, 1.964158282178072312, 0.1467643733194800570 ) ) ;
#90337 = CARTESIAN_POINT ( 'NONE',  ( 0.3220787244772654323, 1.858110058275804111, 0.5644625801373166496 ) ) ;
#90338 = VERTEX_POINT ( 'NONE', #184885 ) ;
#90339 = CARTESIAN_POINT ( 'NONE',  ( -6.123442655227560927, 7.173046514967467147, 1.199719254218452047 ) ) ;
#90341 = CARTESIAN_POINT ( 'NONE',  ( 6.533471381225442798, -0.1521382079053348602, 2.086446650026114735 ) ) ;
#90340 = CARTESIAN_POINT ( 'NONE',  ( -3.637330350216213759, 7.465578851886037093, -0.7998128361456481317 ) ) ;
#90342 = CARTESIAN_POINT ( 'NONE',  ( 4.841670253411575864, 8.662716039039905169, -0.7216878364870458196 ) ) ;
#90344 = ORIENTED_EDGE ( 'NONE', *, *, #41132, .T. ) ;
#90343 = CARTESIAN_POINT ( 'NONE',  ( 3.527896108305649037, -1.883508717751972705, 0.3295761852530054159 ) ) ;
#90345 = CARTESIAN_POINT ( 'NONE',  ( 0.7806487521475922176, -1.224371414366259625, 1.835764474286231129 ) ) ;
#90346 = CARTESIAN_POINT ( 'NONE',  ( 7.730132016633517011, -5.756136661604418947, 7.730132016633493919 ) ) ;
#90347 = CARTESIAN_POINT ( 'NONE',  ( 6.270187311338969671, 2.007533000635489451, -0.1505373637035074819 ) ) ;
#90349 =( BOUNDED_CURVE ( )  B_SPLINE_CURVE ( 2, ( #208065, #75948, #122665, #23982, #74887, #204850, #8809, #56504, #205939 ),
 .UNSPECIFIED., .F., .T. ) 
 B_SPLINE_CURVE_WITH_KNOTS ( ( 3, 2, 2, 2, 3 ),
 ( 0.5208333333333333703, 0.5277777777777777901, 0.5416666666666666297, 0.5555555555555555802, 0.5625000000000000000 ),
 .UNSPECIFIED. ) 
 CURVE ( )  GEOMETRIC_REPRESENTATION_ITEM ( )  RATIONAL_B_SPLINE_CURVE ( ( 0.9330127018922192983, 0.9330127018922198534, 1.000000000000000000, 0.8660254037844387076, 1.000000000000000000, 0.8660254037844387076, 1.000000000000000000, 0.9330127018922194093, 0.9330127018922194093 ) ) 
 REPRESENTATION_ITEM ( '' )  );
#90348 = CARTESIAN_POINT ( 'NONE',  ( 0.4909899725976942797, 7.342450396234887044, 1.941297109531809006 ) ) ;
#90351 = FACE_OUTER_BOUND ( 'NONE', #15721, .T. ) ;
#90350 = PRODUCT_DEFINITION_FORMATION_WITH_SPECIFIED_SOURCE ( 'ANY', '', #59182, .NOT_KNOWN. ) ;
#90352 = CARTESIAN_POINT ( 'NONE',  ( 6.727182134110201162, 7.629137130509070275, 2.410944104600750038 ) ) ;
#90353 = CARTESIAN_POINT ( 'NONE',  ( 1.996617168637443429, 2.047528291220417351, 0.3059219562495316125 ) ) ;
#90354 = CARTESIAN_POINT ( 'NONE',  ( -5.377780486114890124, 9.425827667109372143, 0.000000000000000000 ) ) ;
#90355 = VECTOR ( 'NONE', #1999, 1000.000000000000000 ) ;
#90356 = CARTESIAN_POINT ( 'NONE',  ( -4.695470500997839025, 8.269974592382618894, -0.5850018098894956831 ) ) ;
#90357 = B_SPLINE_CURVE_WITH_KNOTS ( 'NONE', 3,
 ( #13699, #194590, #178364, #147992, #63533, #12630, #78701, #144827, #163176, #112351 ),
 .UNSPECIFIED., .F., .F.,
 ( 4, 3, 3, 4 ),
 ( 1.474674387456768442E-18, 3.125271361792667814E-05, 6.250516575001786271E-05, 0.0001052821752614775306 ),
 .UNSPECIFIED. ) ;
#90358 = CARTESIAN_POINT ( 'NONE',  ( -3.853570894305263561, 8.531289074211878543, -2.447542183238071711 ) ) ;
#90359 = CARTESIAN_POINT ( 'NONE',  ( 5.769158057814842699, 6.689438141327490150, 1.199719254218462483 ) ) ;
#90360 = AXIS2_PLACEMENT_3D ( 'NONE', #67036, #165638, #100631 ) ;
#90361 = CARTESIAN_POINT ( 'NONE',  ( 4.892487020634524342, 4.880525410245029505, -1.277330582746047388E-09 ) ) ;
#90362 = CARTESIAN_POINT ( 'NONE',  ( 3.743459811148990291, 7.381470523066878009, -0.7216878364870338292 ) ) ;
#90363 = CARTESIAN_POINT ( 'NONE',  ( -11.01135777277262129, 0.000000000000000000, -1.400000000000001910 ) ) ;
#90364 = DIRECTION ( 'NONE',  ( 0.000000000000000000, -1.000000000000000000, 0.000000000000000000 ) ) ;
#90365 = CARTESIAN_POINT ( 'NONE',  ( -1.364683531250014514, 13.15104166700806410, -0.7879004041258335089 ) ) ;
#90367 = CARTESIAN_POINT ( 'NONE',  ( -4.959250327548641479, 9.007818825440551791, -0.7998128361456362523 ) ) ;
#90366 = CARTESIAN_POINT ( 'NONE',  ( 6.825078400183516081, 0.5802287360496224400, 2.007770452540482697 ) ) ;
#90368 = CARTESIAN_POINT ( 'NONE',  ( 4.939963660092479891, -1.468890173064988147, -0.9213945099728354515 ) ) ;
#90369 = CARTESIAN_POINT ( 'NONE',  ( -2.578021764892882040, 6.159442492350315490, 0.7998128361456341429 ) ) ;
#90370 = CARTESIAN_POINT ( 'NONE',  ( 2.957943426865859760, -0.6537446763684885420, 1.964363857337739105 ) ) ;
#90371 = CARTESIAN_POINT ( 'NONE',  ( 3.111064062886280013, 0.05467929133608259024, 2.116691892344662929 ) ) ;
#90372 = CARTESIAN_POINT ( 'NONE',  ( 6.265839547809997079, 10.46189657242035587, 0.7998128361456462443 ) ) ;
#90373 = CARTESIAN_POINT ( 'NONE',  ( -1.364683531250012516, 3.488541667008085767, -0.7879004041258300672 ) ) ;
#90374 = CARTESIAN_POINT ( 'NONE',  ( 1.375766793938013821, -1.922594530582939942, 0.4262983161763284623 ) ) ;
#90375 = CARTESIAN_POINT ( 'NONE',  ( 5.728356146706021335, 6.265246534282280066, 1.050634566151719129 ) ) ;
#90377 = CARTESIAN_POINT ( 'NONE',  ( 0.2110004604562870645, 1.588762659912812403, -1.064147093309028680 ) ) ;
#90376 = CARTESIAN_POINT ( 'NONE',  ( 0.000000000000000000, -3.696874999522040017, -3.793834371823813001 ) ) ;
#90378 = CARTESIAN_POINT ( 'NONE',  ( 3.556809736639905406, -2.021263576298555797, -1.081171400725000398 ) ) ;
#90379 = CARTESIAN_POINT ( 'NONE',  ( 1.558932953716257730, -1.564965500463588732, -0.9399777662534372080 ) ) ;
#90380 = CARTESIAN_POINT ( 'NONE',  ( 4.692003678781083487, 7.631698837623355658, -1.199719254218450271 ) ) ;
#90381 = CARTESIAN_POINT ( 'NONE',  ( 6.683806541412754321, 8.820860269780128604, -1.443375672974058777 ) ) ;
#90382 = CARTESIAN_POINT ( 'NONE',  ( -8.128276786592724790, 9.441743324901704426, -1.199719254218446718 ) ) ;
#90383 = CARTESIAN_POINT ( 'NONE',  ( 3.340093095703601023, -1.202498264213421209, -1.614455356613291093 ) ) ;
#90384 = CARTESIAN_POINT ( 'NONE',  ( 2.975390029205774223, -0.1970676810524821243, 1.951864085487287959 ) ) ;
#90385 = CARTESIAN_POINT ( 'NONE',  ( -7.309817376062285099, 11.67987070538135264, 0.000000000000000000 ) ) ;
#90386 = CARTESIAN_POINT ( 'NONE',  ( -4.903245109636583443, 8.872203061218007392, -0.7998128361456281477 ) ) ;
#90387 = DIRECTION ( 'NONE',  ( -7.993605777301127091E-15, 0.000000000000000000, 1.000000000000000000 ) ) ;
#90389 = CARTESIAN_POINT ( 'NONE',  ( 4.135448415848129500, -1.220878049459400039, -1.281573189658680612 ) ) ;
#90388 = CARTESIAN_POINT ( 'NONE',  ( 6.562449924160270065, -1.910870307864566575, -0.8485530564429457634 ) ) ;
#90390 = CARTESIAN_POINT ( 'NONE',  ( 0.3554123170485725680, 15.00000000000058265, 12.67999999502907649 ) ) ;
#90391 = CARTESIAN_POINT ( 'NONE',  ( 0.5159075615763093481, -1.175655012515547160, -1.849222068403690411 ) ) ;
#90392 = CARTESIAN_POINT ( 'NONE',  ( 6.087833319296645840, -1.732659258567319505, -0.1633284621618599775 ) ) ;
#90393 = CARTESIAN_POINT ( 'NONE',  ( 8.911787042884274257, 9.291506392986812912, 0.7998128361456462443 ) ) ;
#90394 = CARTESIAN_POINT ( 'NONE',  ( 0.2331713839410602396, 2.030351879425442707, -2.369071045443218004 ) ) ;
#90395 = CARTESIAN_POINT ( 'NONE',  ( 6.029976284357474903, -1.944044770632427976, 1.226447132130564999 ) ) ;
#90396 = CARTESIAN_POINT ( 'NONE',  ( -0.1114211809780316365, -0.4883405756051837354, -2.144353428667714390 ) ) ;
#90397 = CARTESIAN_POINT ( 'NONE',  ( 5.132092517088904238, 0.1681052705169924777, -1.725677682095213994 ) ) ;
#90398 = CARTESIAN_POINT ( 'NONE',  ( 2.139570144280181108, -1.970530345926827742, 0.9937953903183869286 ) ) ;
#90399 = CARTESIAN_POINT ( 'NONE',  ( 6.127409529368080143, 0.1660417618732710210, -2.164901972331951363 ) ) ;
#90400 = CARTESIAN_POINT ( 'NONE',  ( -3.563261906135775536, 6.332667919118538435, -2.420000000000000373 ) ) ;
#90401 = CARTESIAN_POINT ( 'NONE',  ( 0.1986506717676014555, 1.455101728037408337, -1.538369530143603559 ) ) ;
#90402 = CARTESIAN_POINT ( 'NONE',  ( 3.500000000000003109, -2.127848526677250785E-13, -2.052068128417947612 ) ) ;
#90403 = CARTESIAN_POINT ( 'NONE',  ( -0.5221183067618221374, 7.970647359860968173, -1.933437843119017563 ) ) ;
#90404 = CARTESIAN_POINT ( 'NONE',  ( 4.366181854897908998, 0.9076448143166337967, 1.699152538019559788 ) ) ;
#90405 = CARTESIAN_POINT ( 'NONE',  ( 0.7500000000000006661, 11.44791666734946212, -1.299038105676657340 ) ) ;
#90406 = CARTESIAN_POINT ( 'NONE',  ( 1.295894383074674749, 2.050542657126565249, -0.8545418985851579441 ) ) ;
#90407 = ORIENTED_EDGE ( 'NONE', *, *, #84784, .F. ) ;
#90408 = CARTESIAN_POINT ( 'NONE',  ( 1.499999999999989120, 4.504166666666688634, 0.8660254037844524744 ) ) ;
#90409 = CARTESIAN_POINT ( 'NONE',  ( 3.323720213644492993, 7.029424015893889433, 1.040834085586084257E-14 ) ) ;
#90410 = CARTESIAN_POINT ( 'NONE',  ( 7.091078035147269532, 8.231678114882006625, 1.199719254218462483 ) ) ;
#90411 = CARTESIAN_POINT ( 'NONE',  ( 4.178555957833706813, 1.047420865545487523, 1.958865958838784005 ) ) ;
#90412 = CARTESIAN_POINT ( 'NONE',  ( -9.490344339885981029, 10.17441593939621924, -0.7216878364870267237 ) ) ;
#90413 = ADVANCED_FACE ( 'NONE', ( #20255 ), #36510, .F. ) ;
#90414 = CARTESIAN_POINT ( 'NONE',  ( 7.483737605063422116, 7.833374748769873719, -0.7216878364870257245 ) ) ;
#90415 = CARTESIAN_POINT ( 'NONE',  ( -7.985389288324692636, 11.29974268881207067, -1.082531754730543083 ) ) ;
#90416 = CIRCLE ( 'NONE', #80040, 0.08000000000000012657 ) ;
#90417 = CARTESIAN_POINT ( 'NONE',  ( 7.377044979611483200, 7.779176362401098999, -0.7216878364870317197 ) ) ;
#90418 = CARTESIAN_POINT ( 'NONE',  ( 2.057267738415057057, -1.238319999287675888, 1.591319116112683618 ) ) ;
#90420 = CARTESIAN_POINT ( 'NONE',  ( 6.830530959611283315, -1.272493244265305634, 1.624195267664030995 ) ) ;
#90419 = CARTESIAN_POINT ( 'NONE',  ( 7.507464373665139412, 9.781794407407920389, 1.599625672291281386 ) ) ;
#90421 = CARTESIAN_POINT ( 'NONE',  ( -11.00057242252814760, -6.459673408256604965, 0.07917133907650250602 ) ) ;
#90422 = CARTESIAN_POINT ( 'NONE',  ( 7.309254211098760834, 8.660456346770972758, 1.082531754730549967 ) ) ;
#90423 = CARTESIAN_POINT ( 'NONE',  ( 6.532745107981281940, -1.550057735787165214, 0.7916670675358824516 ) ) ;
#90424 = FACE_OUTER_BOUND ( 'NONE', #38454, .T. ) ;
#90425 = CARTESIAN_POINT ( 'NONE',  ( -1.201851678989727383E-14, 2.696875000341417916, -1.575800808251660134 ) ) ;
#90426 = CARTESIAN_POINT ( 'NONE',  ( 1.879799676208588899, -0.9517657123069392933, 1.491821474084076726 ) ) ;
#90427 = CARTESIAN_POINT ( 'NONE',  ( -0.1048463755018592264, -0.8645036352170620830, -1.819965476435807306 ) ) ;
#90428 = CARTESIAN_POINT ( 'NONE',  ( 6.585563763084506306, -0.7354652392584435372, 1.576171286539735705 ) ) ;
#90429 = CARTESIAN_POINT ( 'NONE',  ( 4.212625126225740146, 2.095743129530680537, 0.9292526312315220194 ) ) ;
#90430 = CARTESIAN_POINT ( 'NONE',  ( -0.6823417656250003738, -0.03229166632524871350, -1.181850606188749264 ) ) ;
#90431 = CARTESIAN_POINT ( 'NONE',  ( 2.519273208346615167, -1.059988974693906183, -1.505194322970206722 ) ) ;
#90432 = ADVANCED_FACE ( 'NONE', ( #77554 ), #43154, .F. ) ;
#90433 = CARTESIAN_POINT ( 'NONE',  ( 10.24726517383036928, 10.84956421242393887, 0.000000000000000000 ) ) ;
#90434 = DIRECTION ( 'NONE',  ( -0.000000000000000000, 1.000000000000000000, 1.804652791718263484E-16 ) ) ;
#90435 = CARTESIAN_POINT ( 'NONE',  ( 3.276193339942961913, -1.088440757138483539, 1.465454812695582643 ) ) ;
#90436 = CARTESIAN_POINT ( 'NONE',  ( 3.568982563115063567, -0.9913999084223242830, 1.755768870528086056 ) ) ;
#90437 = CARTESIAN_POINT ( 'NONE',  ( -8.130085669689073313, 12.63685038127928806, 0.7998128361456481317 ) ) ;
#90439 = CARTESIAN_POINT ( 'NONE',  ( -9.581972888692712687, -7.217909409572546231, -3.920744210608467172E-13 ) ) ;
#90438 = CARTESIAN_POINT ( 'NONE',  ( 3.573342120354418672, 0.05797898436993471211, -2.261936065680466346 ) ) ;
#90440 = CARTESIAN_POINT ( 'NONE',  ( 5.333084004640892495, 0.1517067650670254342, 2.100546829335631749 ) ) ;
#90441 = CARTESIAN_POINT ( 'NONE',  ( 7.017272423055321617, 15.99342652349251104, 9.336217528587633652 ) ) ;
#90442 = CARTESIAN_POINT ( 'NONE',  ( 1.943885480841448965, 1.426152643941134501, 1.501071833787496645 ) ) ;
#90443 = CARTESIAN_POINT ( 'NONE',  ( 2.869522067586683711, 6.499526178826442013, 0.7998128361456362523 ) ) ;
#90444 = CARTESIAN_POINT ( 'NONE',  ( -3.755786496842897795E-14, -0.01562499965858205574, 1.570758158831768281 ) ) ;
#90445 = CARTESIAN_POINT ( 'NONE',  ( 6.322909428431959356, 1.571596504679906303, -1.423730336690950393 ) ) ;
#90446 = CONTEXT_DEPENDENT_SHAPE_REPRESENTATION ( #202781, #144042 ) ;
#90448 = CARTESIAN_POINT ( 'NONE',  ( 1.453605159173555705, 0.5596597320992221514, -1.843422129977128954 ) ) ;
#90447 = CARTESIAN_POINT ( 'NONE',  ( -10.34217224912604571, 10.96028913360221502, 0.7998128361456462443 ) ) ;
#90449 = UNCERTAINTY_MEASURE_WITH_UNIT (LENGTH_MEASURE( 1.000000000000000082E-05 ), #102775, 'distance_accuracy_value', 'NONE');
#90450 = CARTESIAN_POINT ( 'NONE',  ( -3.871735385154307263, 6.674719161725423788, -1.199719254218450271 ) ) ;
#90451 = CARTESIAN_POINT ( 'NONE',  ( 9.097684769969825780, 10.57271930550834860, -1.199719254218446718 ) ) ;
#90452 = CARTESIAN_POINT ( 'NONE',  ( 5.899206235277530297, 7.015400374979486209, -1.082531754730548412 ) ) ;
#90453 = CARTESIAN_POINT ( 'NONE',  ( 5.134314571617769829, 6.480444997182255307, 1.201143065674977528 ) ) ;
#90454 = CARTESIAN_POINT ( 'NONE',  ( 1.737499999999999378, -0.4229166657107527594, -3.009438278150925683 ) ) ;
#90455 = CARTESIAN_POINT ( 'NONE',  ( -4.925689880466507908, 4.641059703499347044, -0.7998128361456221525 ) ) ;
#90456 = CARTESIAN_POINT ( 'NONE',  ( 0.3170205077604414945, -0.7560223448306638838, -2.088923821510160650 ) ) ;
#90457 = CARTESIAN_POINT ( 'NONE',  ( 2.714012760861806317, -2.083235677042583944, 0.3076118897425133003 ) ) ;
#90458 = CARTESIAN_POINT ( 'NONE',  ( -3.142457743317409680, 6.888227477170756785, 0.7998128361456352531 ) ) ;
#90459 = CARTESIAN_POINT ( 'NONE',  ( 7.670162217029129259, 9.971608557999250166, 1.599625672291281386 ) ) ;
#90460 = CARTESIAN_POINT ( 'NONE',  ( 6.473497990634856869, -0.2285008921534004422, 1.846817554525240990 ) ) ;
#90461 = CARTESIAN_POINT ( 'NONE',  ( 7.949158136313996259, 8.168439335321471262, 1.040834085586084257E-14 ) ) ;
#90462 = CARTESIAN_POINT ( 'NONE',  ( -7.105881907338169157, 8.423188659050232729, -1.082531754730549967 ) ) ;
#90464 = ORIENTED_EDGE ( 'NONE', *, *, #170328, .F. ) ;
#90463 = CARTESIAN_POINT ( 'NONE',  ( -9.015808963407680565, 9.620791333504852716, 1.040834085586084257E-14 ) ) ;
#90465 = CARTESIAN_POINT ( 'NONE',  ( 0.4750491441844888474, -1.531729482103380224, 1.466773057065169361 ) ) ;
#90466 = CYLINDRICAL_SURFACE ( 'NONE', #147362, 0.09999999999999982514 ) ;
#90468 = CARTESIAN_POINT ( 'NONE',  ( 2.822649888979886335, -1.354935067541668259, 1.419045635080482093 ) ) ;
#90467 = CARTESIAN_POINT ( 'NONE',  ( 1.224999999999997202, -0.1458333333333367010, 0.7072540797572898219 ) ) ;
#90469 = CARTESIAN_POINT ( 'NONE',  ( 1.973706723050288936, 2.068691090354588091, -0.6273066937243013674 ) ) ;
#90470 = B_SPLINE_CURVE_WITH_KNOTS ( 'NONE', 3,
 ( #191067, #91477, #9133, #75208, #141319, #10193, #42731, #76267, #142376, #186803 ),
 .UNSPECIFIED., .F., .F.,
 ( 4, 3, 3, 4 ),
 ( 1.654962790341811419E-18, 3.125188815118514071E-05, 5.930006937714327664E-05, 8.735821697256892582E-05 ),
 .UNSPECIFIED. ) ;
#90472 = CARTESIAN_POINT ( 'NONE',  ( -4.965152591087599099, 6.642004417359813395, -1.244917454897740861 ) ) ;
#90471 = CARTESIAN_POINT ( 'NONE',  ( -4.285259070371116863, 7.157163461145040095, 1.199719254218452935 ) ) ;
#90474 = EDGE_CURVE ( 'NONE', #49626, #57984, #195276, .T. ) ;
#90473 = CARTESIAN_POINT ( 'NONE',  ( 1.364683531249988535, 1.363541667008083769, 0.7879004041258500513 ) ) ;
#90475 = CARTESIAN_POINT ( 'NONE',  ( 3.292619090915947844, 1.372597323508369715, 1.069791993016102172 ) ) ;
#90476 = CARTESIAN_POINT ( 'NONE',  ( 6.968527767744109980, 7.232296605230681408, 0.7216878364870317197 ) ) ;
#90477 = CARTESIAN_POINT ( 'NONE',  ( -11.47191357686926771, 5.776505007901941546, -5.393588192467421827 ) ) ;
#90478 = AXIS2_PLACEMENT_3D ( 'NONE', #77545, #171851, #57039 ) ;
#90479 = CARTESIAN_POINT ( 'NONE',  ( 2.020861031540205133, 2.010896488828680440, -0.1455087364366919322 ) ) ;
#90480 = CARTESIAN_POINT ( 'NONE',  ( -9.586610838029429260, -7.161464053357574855, 0.003376046620574835178 ) ) ;
#90481 = CARTESIAN_POINT ( 'NONE',  ( 0.09294085500742564621, -0.4768749645070144982, -2.116232079886640971 ) ) ;
#90482 = CARTESIAN_POINT ( 'NONE',  ( 2.114083122616668309, -0.9278515453300213434, -1.739463596305758974 ) ) ;
#90483 = ADVANCED_FACE ( 'NONE', ( #174026 ), #123212, .T. ) ;
#90486 = VERTEX_POINT ( 'NONE', #193445 ) ;
#90485 = CARTESIAN_POINT ( 'NONE',  ( -5.316205630334268406, 6.335233002545657577, -1.082531754730549967 ) ) ;
#90484 = DIRECTION ( 'NONE',  ( 1.000000000000000000, -7.771561172376097755E-16, -4.440892098500627148E-16 ) ) ;
#90488 = EDGE_CURVE ( 'NONE', #150638, #11451, #28338, .T. ) ;
#90487 = CARTESIAN_POINT ( 'NONE',  ( -6.251718229232867685, 6.466295153626015590, -0.7216878364870338292 ) ) ;
#90489 = CARTESIAN_POINT ( 'NONE',  ( 5.712781623311797397, 7.758274208654143855, -1.599625672291283607 ) ) ;
#90490 = CARTESIAN_POINT ( 'NONE',  ( -4.932134020321308654, 8.976183133675331050, 0.7998128361456291469 ) ) ;
#90491 = CARTESIAN_POINT ( 'NONE',  ( 2.209634141364385851, 1.562563088667227262, 1.279657157811086909 ) ) ;
#90492 = CARTESIAN_POINT ( 'NONE',  ( 0.000000000000000000, 0.2000000000000057288, 11.29999999999998828 ) ) ;
#90493 = CARTESIAN_POINT ( 'NONE',  ( 5.913149109437923379, 2.031366086520134395, 1.094794683655570644 ) ) ;
#90494 = CARTESIAN_POINT ( 'NONE',  ( -10.45361012356095465, 5.194925941179032058, 5.800590495124775536 ) ) ;
#90495 = CARTESIAN_POINT ( 'NONE',  ( 2.588659458060487584, 1.901619664775334728, 0.4814403318105645591 ) ) ;
#90496 = CARTESIAN_POINT ( 'NONE',  ( 9.260382613333817403, 10.76253345609967660, -1.199719254218446718 ) ) ;
#90497 = CARTESIAN_POINT ( 'NONE',  ( 0.7389079861009685279, 2.013985778099684154, -0.1017531103126300962 ) ) ;
#90498 = ORIENTED_EDGE ( 'NONE', *, *, #36673, .T. ) ;
#90499 = CARTESIAN_POINT ( 'NONE',  ( 2.272804288956633112, -0.3671671630497001515, -2.085132402650377248 ) ) ;
#90500 = CARTESIAN_POINT ( 'NONE',  ( -6.880926654135487652, 7.986501503701545879, 1.199719254218450271 ) ) ;
#90501 = CARTESIAN_POINT ( 'NONE',  ( 2.027068592762204080, -1.202062398780713748, -1.394650109237540070 ) ) ;
#90502 = ORIENTED_EDGE ( 'NONE', *, *, #187534, .T. ) ;
#90503 = CARTESIAN_POINT ( 'NONE',  ( -10.14557902172788495, 10.73093036830436553, 1.040834085586084257E-14 ) ) ;
#90504 = DIRECTION ( 'NONE',  ( 0.000000000000000000, 0.000000000000000000, -1.000000000000000000 ) ) ;
#90505 = CARTESIAN_POINT ( 'NONE',  ( 3.885109016898561585, -1.979880364965879380, -0.7601140796509860964 ) ) ;
#90506 = CARTESIAN_POINT ( 'NONE',  ( 0.6207436649305307919, -1.749090901066195691, 0.5750481222980761142 ) ) ;
#90507 = CARTESIAN_POINT ( 'NONE',  ( 1.499999999999989120, 5.077083334016151639, -0.8660254037844323793 ) ) ;
#90508 = CARTESIAN_POINT ( 'NONE',  ( 8.260995669428309540, 8.532249790621511565, 0.7998128361456481317 ) ) ;
#90509 = CARTESIAN_POINT ( 'NONE',  ( 7.862802741282558294, 8.137967717776607657, 0.000000000000000000 ) ) ;
#90510 = CARTESIAN_POINT ( 'NONE',  ( 4.253237527111143557, -1.711175411557999348, -1.148025453137695662 ) ) ;
#90511 = PRODUCT_DEFINITION ( 'UNKNOWN', '', #97314, #35704 ) ;
#90513 = CARTESIAN_POINT ( 'NONE',  ( 1.171164436615620863, 1.096940724416964885, 1.478650282607060662 ) ) ;
#90512 = CARTESIAN_POINT ( 'NONE',  ( -6.177711549321182716, 10.35908057418338402, 0.7998128361456481317 ) ) ;
#90514 = CARTESIAN_POINT ( 'NONE',  ( 1.364683531249990311, 5.134375000341417916, 1.214306433183764966E-14 ) ) ;
#90515 = FACE_BOUND ( 'NONE', #154877, .T. ) ;
#90516 =( LENGTH_UNIT ( ) NAMED_UNIT ( * ) SI_UNIT ( .MILLI., .METRE. ) );
#90517 = CARTESIAN_POINT ( 'NONE',  ( 1.369155121446740960E-15, 0.08000000000000020983, -11.18000000000000149 ) ) ;
#90518 = MECHANICAL_DESIGN_GEOMETRIC_PRESENTATION_REPRESENTATION (  '', ( #14408 ), #163185 ) ;
#90519 = CARTESIAN_POINT ( 'NONE',  ( 0.5400322017136415242, -1.563516176313231920, -1.557742479837947558 ) ) ;
#90520 = CARTESIAN_POINT ( 'NONE',  ( 4.323666171361133514, -2.166671669000098444, 0.6512573085333557277 ) ) ;
#90521 = AXIS2_PLACEMENT_3D ( 'NONE', #201888, #17812, #19955 ) ;
#90522 = CARTESIAN_POINT ( 'NONE',  ( -8.351459436338041442, 9.806086099558291025, -1.082531754730543971 ) ) ;
#90523 = CARTESIAN_POINT ( 'NONE',  ( 3.128980605277735361, 1.639808012139221116, 0.7702280095687010775 ) ) ;
#90524 = CARTESIAN_POINT ( 'NONE',  ( 3.450306162294475065, -1.282734793626014280, 1.423081227541162841 ) ) ;
#90525 = CARTESIAN_POINT ( 'NONE',  ( 4.018080225218490398, 2.055083638104511223, -0.2504045000601487492 ) ) ;
#90526 = CARTESIAN_POINT ( 'NONE',  ( -1.364683531249997417, 3.571875000341423245, 1.214306433183764966E-14 ) ) ;
#90527 = CARTESIAN_POINT ( 'NONE',  ( 2.817209029084859928, -0.1949976385870570150, 1.961808326198757335 ) ) ;
#90528 = CARTESIAN_POINT ( 'NONE',  ( 0.8328817383555222609, 0.1387611642639074438, 1.921445197033289976 ) ) ;
#90529 = CARTESIAN_POINT ( 'NONE',  ( 3.801501934187266230, -0.5436965770258190833, 1.789884385262895616 ) ) ;
#90530 = CARTESIAN_POINT ( 'NONE',  ( 2.280263026629821166, 1.421315682977505546, 1.817977143087915026 ) ) ;
#90531 = CARTESIAN_POINT ( 'NONE',  ( 4.193699477585779434, -1.282400645549033547, -1.348940618851623974 ) ) ;
#90532 = CARTESIAN_POINT ( 'NONE',  ( -1.364683531250010295, 4.530208333674754506, 0.7879004041258379498 ) ) ;
#90533 = CARTESIAN_POINT ( 'NONE',  ( -5.949330478298285207, 5.835307067636438028, 0.7998128361456341429 ) ) ;
#90534 = CARTESIAN_POINT ( 'NONE',  ( 7.637320603199683866, 7.804628880021436288, -0.7998128361456281477 ) ) ;
#90535 = DIRECTION ( 'NONE',  ( 0.000000000000000000, 0.000000000000000000, 1.000000000000000000 ) ) ;
#90536 = CARTESIAN_POINT ( 'NONE',  ( 0.4343773424168140274, 1.080651816385242547, -1.807535387385241776 ) ) ;
#90537 = CARTESIAN_POINT ( 'NONE',  ( 4.053524740361575063, 4.791828954252362216, -1.082531754730543083 ) ) ;
#90539 = CARTESIAN_POINT ( 'NONE',  ( -3.023105066167347310, 5.702484939155337607, 2.500000000000011102 ) ) ;
#90538 = CARTESIAN_POINT ( 'NONE',  ( -1.364683531250010295, 4.092708333674751842, 0.7879004041258379498 ) ) ;
#90540 = CARTESIAN_POINT ( 'NONE',  ( 6.802040682177005415, -2.161276877365316818, 0.04550429416337595928 ) ) ;
#90541 = CARTESIAN_POINT ( 'NONE',  ( 2.109781586379317897, 1.642293606977158538, 1.341614810521203349 ) ) ;
#90542 = FILL_AREA_STYLE_COLOUR ( '', #182740 ) ;
#90543 = CARTESIAN_POINT ( 'NONE',  ( 0.9846354891296082990, -1.278160710921724341, 1.563951078967614094 ) ) ;
#90544 = CARTESIAN_POINT ( 'NONE',  ( -1.364683531250000748, 1.009375000341421247, 0.000000000000000000 ) ) ;
#90545 = CARTESIAN_POINT ( 'NONE',  ( -4.609409038966245653, 6.400729850259146758, -1.443375672974053447 ) ) ;
#90546 = CARTESIAN_POINT ( 'NONE',  ( 3.635557746758808495, 7.393234471193928847, -0.7998128361456291469 ) ) ;
#90547 = CARTESIAN_POINT ( 'NONE',  ( 1.177287030172860183, -0.05180490295666682898, -2.161124318685260004 ) ) ;
#90550 = CARTESIAN_POINT ( 'NONE',  ( 4.555176424511575561, 4.416720038126027426, -0.7216878364870188411 ) ) ;
#90549 = CARTESIAN_POINT ( 'NONE',  ( 6.825078400183575589, 6.038285016609903799, 2.450557349082567171 ) ) ;
#90548 = CARTESIAN_POINT ( 'NONE',  ( 4.552505719138623341, 8.533283448962240669, 0.7998128361456341429 ) ) ;
#90551 =( BOUNDED_SURFACE ( )  B_SPLINE_SURFACE ( 3, 2, ( 
 ( #106640, #125062, #138034 ),
 ( #189965, #25330, #204047 ),
 ( #58908, #208339, #9086 ),
 ( #41614, #107726, #8003 ),
 ( #55697, #75160, #74094 ),
 ( #93564, #6922, #72999 ),
 ( #42686, #141270, #108793 ),
 ( #156416, #43749, #26395 ),
 ( #92508, #121853, #40537 ),
 ( #187824, #172668, #158545 ) ),
 .UNSPECIFIED., .F., .F., .T. ) 
 B_SPLINE_SURFACE_WITH_KNOTS ( ( 4, 2, 2, 2, 4 ),
 ( 3, 3 ),
 ( -6.776263578034402713E-19, 0.0004030251014121639832, 0.0008060502028243286170, 0.001209075304236493197, 0.001612100405648657885 ),
 ( 0.000000000000000000, 1.000000000000000000 ),
 .UNSPECIFIED. ) 
 GEOMETRIC_REPRESENTATION_ITEM ( )  RATIONAL_B_SPLINE_SURFACE ( (
 ( 1.000000000000000000, 0.8509629433967621503, 1.000000000000000000),
 ( 1.000000000000000000, 0.8510310118808769309, 1.000000000000000000),
 ( 1.000000000000000000, 0.8495812529563572246, 1.000000000000000000),
 ( 1.000000000000000000, 0.8465918360525789277, 1.000000000000000000),
 ( 1.000000000000000000, 0.8452340365386274978, 1.000000000000000000),
 ( 1.000000000000000000, 0.8452309425927184705, 1.000000000000000000),
 ( 1.000000000000000000, 0.8465710739603070634, 1.000000000000000000),
 ( 1.000000000000000000, 0.8495952187152705504, 1.000000000000000000),
 ( 1.000000000000000000, 0.8510135196387130785, 1.000000000000000000),
 ( 1.000000000000000000, 0.8509629433966219292, 1.000000000000000000) ) ) 
 REPRESENTATION_ITEM ( '' )  SURFACE ( )  );
#90552 = CARTESIAN_POINT ( 'NONE',  ( -0.2104748580754426390, 2.865278511227669078, -2.591885361450113834 ) ) ;
#90553 = CARTESIAN_POINT ( 'NONE',  ( 5.717982508692024624, 0.9896897593998502662, -1.756851901128737348 ) ) ;
#90555 = CARTESIAN_POINT ( 'NONE',  ( -6.468648687051513413, 7.679749902049126220, 1.082531754730549078 ) ) ;
#90554 = CARTESIAN_POINT ( 'NONE',  ( -8.270110514656041190, 10.67154823856396817, 1.443375672974090751 ) ) ;
#90556 = APPLICATION_CONTEXT ( 'automotive_design' ) ;
#90557 = DIRECTION ( 'NONE',  ( 0.000000000000000000, 1.000000000000000000, 0.000000000000000000 ) ) ;
#90559 = CARTESIAN_POINT ( 'NONE',  ( -1.364683531250010740, 10.63020833367473195, 0.7879004041258445001 ) ) ;
#90558 = CARTESIAN_POINT ( 'NONE',  ( 0.8489190418228099722, 0.6593363751366092540, 2.164330503585075505 ) ) ;
#90560 = CARTESIAN_POINT ( 'NONE',  ( -8.299562589859897699, 12.83457345481192036, -0.7998128361456281477 ) ) ;
#90561 = ADVANCED_FACE ( 'NONE', ( #24523 ), #156693, .T. ) ;
#90563 = CARTESIAN_POINT ( 'NONE',  ( 0.7904806358284102163, 1.449672126929082872, -1.252262404471200075 ) ) ;
#90562 = CARTESIAN_POINT ( 'NONE',  ( -6.195713011320807873, 6.330679389403470303, -0.7216878364870267237 ) ) ;
#90564 = CARTESIAN_POINT ( 'NONE',  ( 0.6823417656249899377, 0.9052083336747520637, 1.181850606188755259 ) ) ;
#90565 = B_SPLINE_CURVE_WITH_KNOTS ( 'NONE', 3,
 ( #57180, #122272, #152540, #88626, #151489, #56115, #153617, #187166, #167725, #5189, #6266, #89701, #188230, #71264, #86476, #154682, #73413, #55047, #137378, #4126, #203394, #104876, #170919, #22515, #135250, #23592, #72337, #138443, #204461, #7336, #139516, #85404, #39870, #189307, #105979, #172002, #101657, #3058, #185020, #201263, #52903, #119037, #102731, #168787, #20392, #128667, #91839, #43090, #208740, #109203, #175216, #127607, #28947, #107052, #26799, #9491, #27875, #173078, #59304, #192491, #141672, #156827, #124401, #160012, #10543, #76618, #60367, #126530, #74500, #210877, #61440, #157897, #93971, #90766, #209805, #92903, #44143, #24659, #125462, #11613, #95031, #75563, #140604, #40946, #144870, #8414, #206616, #207684, #78747, #158949, #191424, #142731, #110264, #58244, #177333, #77687, #176273, #143808, #161081, #12671, #190359, #193572, #45215, #62502, #42021, #108130, #174156, #111330, #25729, #80894, #97166, #96101, #195715, #196772, #67794, #31094, #48415, #148033, #114527, #180521, #66727, #163221, #164275, #162156, #32143, #194635, #84081, #182639, #98223, #15865, #81950, #14803, #50521, #146984, #213001, #181572, #46277, #13743, #214043, #65669, #131817, #34261, #197826, #116644, #17991, #49458, #47350, #145928, #115576, #660, #100333, #79816, #33201, #198874, #166400, #99285, #165332, #150169, #16926, #129731, #132870, #1737, #64638, #112393, #178405, #83006, #30016, #211940, #63575, #149082, #113465, #179470, #130777, #155488, #136048, #153355, #69937, #37462, #122006, #53720, #103540, #7071, #202060, #119853, #3863, #72074, #133944, #185831, #169600, #134994, #23328, #19068, #167472, #4925, #186906, #21184, #87286, #183712, #20132, #39599, #71002, #204194, #85146, #137115, #138184, #55849, #203144, #54786, #171730, #120933, #68874, #6004, #117722, #36390, #38538, #201004, #187972, #52649, #104615, #105702, #89436, #170663, #118778, #101398, #199951, #22250, #88360, #154425, #51598, #86218, #168534, #35319, #102468, #151233, #2802, #184763, #152289, #189049, #156565, #192231, #42833, #143549, #75304, #176021, #190108, #9232, #139249, #107874, #93713, #40686, #91582, #28691, #73143, #41761, #110008, #177075, #157634, #173899, #172817, #160825, #94777, #26542, #125203, #57983, #124146, #140338, #206356, #77432, #90501, #205280, #27613, #61185, #25475, #141419, #207426, #108939, #56919, #142471, #59045, #123092, #24389, #193315, #8160, #43894, #106789, #74244, #191166, #11351, #174960, #92650, #10290, #208479, #158692, #76364, #159754, #60115, #126274, #209543, #127345, #44961, #111069, #161904, #13491, #79566, #99027, #63319, #34007, #144614, #14546, #78497, #132616, #194383, #15610, #97976, #145685, #46026, #100081, #80643, #31899, #162967, #130532, #146735, #195462, #213797, #210629, #30839, #164035, #113209, #62255, #112146, #212753, #114278, #128416, #82759, #64387, #115334, #129480, #196523, #178149, #47091, #32953, #181325, #48166, #81698, #29763, #96916, #131569, #404, #165083, #180275, #211683, #65420, #198623, #147781, #197570, #179214, #49214, #16674, #148832, #66477, #95848, #50270, #116388, #182377, #12417, #88101, #5740, #83818, #200751, #121751, #118527, #186655, #154173, #71817, #35061, #70748, #17729, #199692, #187719, #104358, #39347, #166143, #2544, #168280, #119597, #19880, #85963 ),
 .UNSPECIFIED., .F., .F.,
 ( 4, 1, 1, 1, 1, 1, 1, 1, 1, 1, 1, 1, 1, 1, 1, 1, 1, 1, 1, 1, 1, 1, 1, 1, 1, 1, 1, 1, 1, 1, 1, 1, 1, 1, 1, 1, 1, 1, 1, 1, 1, 1, 1, 1, 1, 1, 1, 1, 1, 1, 1, 1, 1, 1, 1, 1, 1, 1, 1, 1, 1, 1, 1, 1, 1, 1, 1, 1, 1, 1, 1, 1, 1, 1, 1, 1, 1, 1, 1, 1, 1, 1, 1, 1, 1, 1, 1, 1, 1, 1, 1, 1, 1, 1, 1, 1, 1, 1, 1, 1, 1, 1, 1, 1, 1, 1, 1, 1, 1, 1, 1, 1, 1, 1, 1, 1, 1, 1, 1, 1, 1, 1, 1, 1, 1, 1, 1, 1, 1, 1, 1, 1, 1, 1, 1, 1, 1, 1, 1, 1, 1, 1, 1, 1, 1, 1, 1, 1, 1, 1, 1, 1, 1, 1, 1, 1, 1, 1, 1, 1, 1, 1, 1, 1, 1, 1, 1, 1, 1, 1, 1, 1, 1, 1, 1, 1, 1, 1, 1, 1, 1, 1, 1, 1, 1, 1, 1, 1, 1, 1, 1, 1, 1, 1, 1, 1, 1, 1, 1, 1, 1, 1, 1, 1, 1, 1, 1, 1, 1, 1, 1, 1, 1, 1, 1, 1, 1, 1, 1, 1, 1, 1, 1, 1, 1, 1, 1, 1, 1, 1, 1, 1, 1, 1, 1, 1, 1, 1, 1, 1, 1, 1, 1, 1, 1, 1, 1, 1, 1, 1, 1, 1, 1, 1, 1, 1, 1, 1, 1, 1, 1, 1, 1, 1, 1, 1, 1, 1, 1, 1, 1, 1, 1, 1, 1, 1, 1, 1, 1, 1, 1, 1, 1, 1, 1, 1, 1, 1, 1, 1, 1, 1, 1, 1, 1, 1, 1, 1, 1, 1, 1, 1, 1, 1, 1, 1, 1, 1, 1, 1, 1, 1, 1, 1, 1, 1, 1, 1, 1, 1, 1, 1, 1, 1, 1, 1, 1, 1, 1, 1, 1, 1, 1, 1, 1, 1, 1, 1, 1, 1, 1, 1, 1, 1, 1, 1, 1, 1, 1, 1, 1, 1, 1, 1, 1, 1, 1, 1, 1, 1, 1, 1, 1, 1, 1, 1, 1, 1, 1, 1, 1, 1, 1, 1, 1, 1, 1, 1, 1, 1, 1, 1, 1, 1, 4 ),
 ( 0.000000000000000000, 0.002600209826155936224, 0.005208878553436857226, 0.007813350965615119270, 0.01041570154746907992, 0.01302155883015148306, 0.01562460066207539862, 0.01822947720112986364, 0.02083337797298438765, 0.02343721533725894035, 0.02604213897589890969, 0.02864525980212044229, 0.03125073504456635232, 0.03385369766904555017, 0.03645898980682723417, 0.03906240375024701977, 0.04166680464497042602, 0.04427120869897264999, 0.04687461886132015393, 0.04947991130494613921, 0.05208287402783655373, 0.05468834688957619622, 0.05729146186993632622, 0.05989639238693608009, 0.06250023923939096449, 0.06510408216679804128, 0.06770901469741306966, 0.07031212675311915294, 0.07291759917081726272, 0.07552056149378454097, 0.07812585104223603027, 0.08072926279340975064, 0.08333366149866272554, 0.08593806365491549193, 0.08854147146176674643, 0.09114676191340240208, 0.09374972248801059782, 0.09635519323906190092, 0.09895830628708340848, 0.1015632345865536273, 0.1041670796237980645, 0.1067709202568039306, 0.1093758509056654005, 0.1119789607794838548, 0.1145844312107493490, 0.1171873915655986947, 0.1197926790194954738, 0.1223960889855860712, 0.1250004854864837645, 0.1276048858798866925, 0.1302082914968497596, 0.1328135800830011481, 0.1354165386474412147, 0.1380220074263333041, 0.1406251186789811980, 0.1432300448973659046, 0.1458338882574615747, 0.1484377267335943440, 0.1510426556371624596, 0.1536457634674935069, 0.1562512320483212536, 0.1588541905735017246, 0.1614594760690261366, 0.1640628843880489185, 0.1666672788216651824, 0.1692716775892487424, 0.1718750811543677814, 0.1744803680111783883, 0.1770833247038955116, 0.1796887916465979840, 0.1822919012421508056, 0.1848968255159594287, 0.1875006673364670307, 0.1901045037933276616, 0.1927094310880738681, 0.1953125370132051675, 0.1979180038795354257, 0.2005209607134520455, 0.2031262443867272172, 0.2057296511966431873, 0.2083340436999963075, 0.2109384409787386505, 0.2135418426300015604, 0.2161471278935624962, 0.2187500828529475860, 0.2213555480953768861, 0.2239586561720615654, 0.2265635786377499516, 0.2291674190561798496, 0.2317712536313151217, 0.2343761794536610432, 0.2369792836118274071, 0.2395847488995502261, 0.2421877041805577391, 0.2447929861676560459, 0.2473963916063780244, 0.2500007823164346887, 0.2526051782432667259, 0.2552085781186103075, 0.2578138619249652486, 0.2604168152893601151, 0.2630222789673848927, 0.2656253856633817301, 0.2682303064573571261, 0.2708341456111751366, 0.2734379784420828963, 0.2760429029284052760, 0.2786460054577940548, 0.2812514693027542978, 0.2838544231691620401, 0.2864597036061101165, 0.2890631078115080133, 0.2916674968651886135, 0.2942718915769991783, 0.2968752898143142138, 0.2994805722994643427, 0.3020835242071668869, 0.3046889864566129091, 0.3072920919100609050, 0.3098970111686871198, 0.3125008491953192857, 0.3151046804194536644, 0.3177096037060897493, 0.3203127047448455222, 0.3229181672828482230, 0.3255211198729257016, 0.3281263988957095479, 0.3307298020056156362, 0.3333341895397992083, 0.3359385831734401084, 0.3385419799105768290, 0.3411472612104861635, 0.3437502117997557338, 0.3463556727564109927, 0.3489587771054129539, 0.3515636949650152721, 0.3541675320018531359, 0.3567713617566292128, 0.3593762839798815834, 0.3619793836661120978, 0.3645848450329270407, 0.3671877964849088460, 0.3697930742294792128, 0.3723964763816929868, 0.3750008625332226786, 0.3776052552255140804, 0.3802086506002868016, 0.3828139308508870520, 0.3854168802599494681, 0.3880223400595693151, 0.3906254434421968513, 0.3932303600390676390, 0.3958341962234732669, 0.3984380246462727593, 0.4010429459424146859, 0.4036460444141952153, 0.4062515047455624306, 0.4088544551976535102, 0.4114597317999305615, 0.4140631331322238151, 0.4166675180379114662, 0.4192719099256467796, 0.4218753040758395079, 0.4244805834130354061, 0.4270835317800880659, 0.4296889905584002634, 0.4322920931126992272, 0.4348970085831024290, 0.4375008440524135733, 0.4401046712805898320, 0.4427095917858701601, 0.4453126891812490551, 0.4479181486128839262, 0.4505210982032648026, 0.4531263737991432228, 0.4557297744492659897, 0.4583341582458977381, 0.4609385494658484461, 0.4635419425292200413, 0.4661472210888942258, 0.4687501685521111572, 0.4713556264448209299, 0.4739587283088163017, 0.4765636427889929916, 0.4791674776805284197, 0.4817713038514113699, 0.4843762237020596273, 0.4869793201590638665, 0.4895847788266616818, 0.4921877276934932821, 0.4947930024188478271, 0.4973964025245324327, 0.5000007853488734888, 0.5026051760377950872, 0.5052085681520839255, 0.5078138460701020485, 0.5104167927676396266, 0.5130222499104345468, 0.5156253512221359303, 0.5182302648483090302, 0.5208340992993732987, 0.5234379245502747136, 0.5260428438825063280, 0.5286459395391455152, 0.5312513975783873521, 0.5338543458598166147, 0.5364596198505067193, 0.5390630195494738874, 0.5416674015382738627, 0.5442717918329101900, 0.5468751831358398263, 0.5494804605480556603, 0.5520834066180569932, 0.5546888631466128095, 0.5572919640440190392, 0.5598968769523987588, 0.5625007111002878757, 0.5651045355685063720, 0.5677094545185276120, 0.5703125495128006373, 0.5729180070593572482, 0.5755209548935220631, 0.5781262282853970591, 0.5807296277153600750, 0.5833340090053582561, 0.5859383990424469335, 0.5885417896717308750, 0.5911470667139914204, 0.5937500122945923442, 0.5963554683445766447, 0.5989585689656815592, 0.6015634812924701702, 0.6041673152744758690, 0.6067711390973024033, 0.6093760578013157625, 0.6119791522712144660, 0.6145846094607528842, 0.6171875569857874222, 0.6197928299146914233, 0.6223962292133623508, 0.6250006099412922511, 0.6276049998575695676, 0.6302083899509167697, 0.6328136667590675835, 0.6354166119884008257, 0.6380220676954796444, 0.6406251681782773044, 0.6432300800596744139, 0.6458339140130902045, 0.6484377373278128465, 0.6510426559220214848, 0.6536457500055372627, 0.6562512069737248543, 0.6588541543277639523, 0.6614594269295416273, 0.6640628262346358612, 0.6666672065372305500, 0.6692715964694370134, 0.6718749861645568755, 0.6744802628744462902, 0.6770832078906477980, 0.6796886633904898334, 0.6822917638729786294, 0.6848966754451861760, 0.6875005095073121186, 0.6901043324512210475, 0.6927092510718347862, 0.6953123449069624762, 0.6979178017894718256, 0.7005207491106575368, 0.7031260215211581066, 0.7057294209703992571, 0.7083338009843969107, 0.7109381910692819107, 0.7135415805038890502, 0.7161468572513741693, 0.7187498021925872171, 0.7213552576208688283, 0.7239583582410578089, 0.7265632696402853918, 0.7291671039484327599, 0.7317709266588259265, 0.7343758454420658000, 0.7369789391668094547, 0.7395843960993241373, 0.7421873435258099505, 0.7447926158808931829, 0.7473960156120186271, 0.7500003954741673029, 0.7526047858484943287, 0.7552081751603144655, 0.7578134520812660480, 0.7604163970856469001, 0.7630218525780576577, 0.7656249534739711926, 0.7682298648364407345, 0.7708336995279378989, 0.7734375221421257995, 0.7760424412242287184, 0.7786455349766069345, 0.7812509920948264019, 0.7838539397647821261, 0.7864592122003229990, 0.7890626123510894319, 0.7916669921981516200, 0.7942713829987035901, 0.7968747723254782089, 0.7994800495557851105, 0.8020829947615083499, 0.8046884504537559213, 0.8072915517634385862, 0.8098964632253897733, 0.8125002984375870874, 0.8151041210928977598, 0.8177090406101226172, 0.8203121345281733090, 0.8229175919678175521, 0.8255205400194353116, 0.8281258126713292311, 0.8307292133795166622, 0.8333335933482756142, 0.8359379847118599827, 0.8385413741913512187, 0.8411466518669262760, 0.8437495974121898001, 0.8463550534400045011, 0.8489581553015269622, 0.8515630669992224622, 0.8541669028694969246, 0.8567707257032814994, 0.8593756457919137226, 0.8619787400136992295, 0.8645841979105142183, 0.8671871464820134490, 0.8697924194861808012, 0.8723958208895988831, 0.8750002011168627192, 0.8776045931803160283, 0.8802079829503125508, 0.8828132612070975771, 0.8854162072301272612, 0.8880216637292678294, 0.8906247662807315058, 0.8932296783504612980, 0.8958335150162225480, 0.8984373381658604663, 0.9010422589622166800, 0.9036453536258294283, 0.9062508121155921081, 0.9088537613452241093, 0.9114590348376164775, 0.9140624370741091687, 0.9166668176967164294, 0.9192712105969091940, 0.9218746007952320909, 0.9244798797692056480, 0.9270828264082496828, 0.9296882835145078294, 0.9322913868941045124, 0.9348962994721256026, 0.9375001370706889103, 0.9401039606740361210, 0.9427088823143441321, 0.9453119775565693717, 0.9479174367776000976, 0.9505203868030935865, 0.9531256609099927335, 0.9557290641454977420, 0.9583334452981105978, 0.9609378390199675435, 0.9635412300619400350, 0.9661465102466426647, 0.9687494557931184413, 0.9713549143510965544, 0.9739580252604012056, 0.9765629275426017664, 0.9791667581373608709, 0.9817706348486141543, 0.9843755007711335603, 0.9869785191422796311, 0.9895843624858681187, 0.9921867025132995455, 0.9947911529560371502, 0.9973998138561904758, 1.000000000000000000 ),
 .UNSPECIFIED. ) ;
#90566 = CARTESIAN_POINT ( 'NONE',  ( 3.810548893104213963, 8.469546410357091659, 2.499999999999999556 ) ) ;
#90567 = CARTESIAN_POINT ( 'NONE',  ( -1.402160292154681736E-14, 8.562500000000001776, 1.732050807568881190 ) ) ;
#90568 = CARTESIAN_POINT ( 'NONE',  ( 2.842114037233371082, 1.711851238368550909, 0.2109339381748502329 ) ) ;
#90569 = CARTESIAN_POINT ( 'NONE',  ( 3.074666975249065626, 6.809138247757705820, 0.000000000000000000 ) ) ;
#90570 = CARTESIAN_POINT ( 'NONE',  ( 4.016958651398847557, 7.908478536599129249, -0.7998128361456362523 ) ) ;
#90571 = CARTESIAN_POINT ( 'NONE',  ( 0.9129390864682377371, -0.2673504635808711671, 1.749312949811430373 ) ) ;
#90572 = CARTESIAN_POINT ( 'NONE',  ( 1.506495127224609876, -2.003582159550582276, -0.1952931609562995052 ) ) ;
#90573 = DIRECTION ( 'NONE',  ( -1.000000000000000000, 0.000000000000000000, 0.000000000000000000 ) ) ;
#90574 = CARTESIAN_POINT ( 'NONE',  ( 4.050008041959299199, 0.7462531942188169731, -2.076888956485785975 ) ) ;
#90575 = VERTEX_POINT ( 'NONE', #9357 ) ;
#90576 = CARTESIAN_POINT ( 'NONE',  ( 8.392133896734662812, 10.81390885098904420, 1.443375672974076540 ) ) ;
#90577 = CARTESIAN_POINT ( 'NONE',  ( -6.994027139803241866, 9.253060644560830994, -1.599625672291271394 ) ) ;
#90579 = CARTESIAN_POINT ( 'NONE',  ( 4.060172857048785389, -1.158672032380179573, 1.650094836768666084 ) ) ;
#90578 = CARTESIAN_POINT ( 'NONE',  ( 4.336665864168765872, 1.303721989063952424, -1.672289659653345639 ) ) ;
#90581 = ORIENTED_EDGE ( 'NONE', *, *, #210167, .F. ) ;
#90580 = CARTESIAN_POINT ( 'NONE',  ( 3.726654843667742689, 1.277109331127034952, -1.285116454894990268 ) ) ;
#90582 = CARTESIAN_POINT ( 'NONE',  ( 5.520104819419390907, 6.469152373191302985, 1.199719254218452935 ) ) ;
#90583 = VERTEX_POINT ( 'NONE', #177201 ) ;
#90584 = CARTESIAN_POINT ( 'NONE',  ( 1.762360912074714125, -1.325010844092512796, 1.320751239342173200 ) ) ;
#90585 = CIRCLE ( 'NONE', #135574, 0.2000000000000005107 ) ;
#90586 = CARTESIAN_POINT ( 'NONE',  ( 6.217409598193539999, -0.2183660865492654257, 1.812524795094340835 ) ) ;
#90587 = CARTESIAN_POINT ( 'NONE',  ( -2.927671105547157371, 5.503034492191895666, 1.199719254218462483 ) ) ;
#90588 = CARTESIAN_POINT ( 'NONE',  ( 1.284279953904121641, 3.253360285806104812, 0.7750000000000135669 ) ) ;
#90589 = CARTESIAN_POINT ( 'NONE',  ( 1.364683531249988757, 1.446875000341421469, 0.000000000000000000 ) ) ;
#90590 = DIRECTION ( 'NONE',  ( -5.551115123125766062E-17, 0.000000000000000000, 1.000000000000000000 ) ) ;
#90591 = ORIENTED_EDGE ( 'NONE', *, *, #25088, .F. ) ;
#90592 = CARTESIAN_POINT ( 'NONE',  ( 5.546694241766559230, 9.485244025454063532, 0.000000000000000000 ) ) ;
#90593 = CARTESIAN_POINT ( 'NONE',  ( -4.990809943606286048, 5.955604701363006015, -1.082531754730549967 ) ) ;
#90594 = CARTESIAN_POINT ( 'NONE',  ( -5.576146316970437944, 9.727530813099326323, 0.000000000000000000 ) ) ;
#90595 = CARTESIAN_POINT ( 'NONE',  ( 3.902672080109194752, -2.098000727953463151, -0.3078000538283760523 ) ) ;
#90597 = CARTESIAN_POINT ( 'NONE',  ( -11.50790213655337979, 7.746734403679841563, -4.957264960544601529 ) ) ;
#90596 = CARTESIAN_POINT ( 'NONE',  ( -0.02948999725181991258, 7.629137130509059617, -2.526318448094333480 ) ) ;
#90598 = CARTESIAN_POINT ( 'NONE',  ( 3.971915101536928283, 1.092440305464415840, 1.640793377567103528 ) ) ;
#90599 = CARTESIAN_POINT ( 'NONE',  ( -1.402160292154681736E-14, 1.196875000341419026, -1.575800808251659024 ) ) ;
#90600 = CARTESIAN_POINT ( 'NONE',  ( 0.07056460990086978191, 0.7743322593966313061, 1.858523817361916963 ) ) ;
#90601 = ORIENTED_EDGE ( 'NONE', *, *, #139862, .F. ) ;
#90602 = CARTESIAN_POINT ( 'NONE',  ( 0.07011551774125344971, -0.9937341303020963412, 1.869520526064169408 ) ) ;
#90603 = CARTESIAN_POINT ( 'NONE',  ( 8.126867821905964462, 14.19425889842085375, 8.829897715376826994 ) ) ;
#90604 = CARTESIAN_POINT ( 'NONE',  ( 1.328672132201724532, -1.314895749051579132, 1.599177317581280455 ) ) ;
#90605 = CARTESIAN_POINT ( 'NONE',  ( 6.261886844665240481, 8.398896966899865646, 1.599625672291268286 ) ) ;
#90606 = ORIENTED_EDGE ( 'NONE', *, *, #112074, .F. ) ;
#90607 = CARTESIAN_POINT ( 'NONE',  ( 6.215487077222150880, 6.216099443039444949, 0.000000000000000000 ) ) ;
#90608 = CARTESIAN_POINT ( 'NONE',  ( 7.700104897918568447, 7.948153567185284096, 0.000000000000000000 ) ) ;
#90610 = CARTESIAN_POINT ( 'NONE',  ( 6.006425746053997372, 6.966250444273174303, -1.199719254218445830 ) ) ;
#90609 = CARTESIAN_POINT ( 'NONE',  ( 3.591813267288586520, -2.088258123952376977, -0.1022297611361303732 ) ) ;
#90611 = CARTESIAN_POINT ( 'NONE',  ( 6.851666526859736983, 9.086973262793417661, -1.599625672291269396 ) ) ;
#90614 = ORIENTED_EDGE ( 'NONE', *, *, #153040, .F. ) ;
#90613 = CARTESIAN_POINT ( 'NONE',  ( 1.207327558334120754, 1.371319684050668730, 1.183719584703796679 ) ) ;
#90612 = CARTESIAN_POINT ( 'NONE',  ( 2.186296784933777992, -1.789763940591000191, -0.3589617604915079085 ) ) ;
#90615 = B_SPLINE_CURVE_WITH_KNOTS ( 'NONE', 3,
 ( #195156, #82447, #132317, #165845, #30530, #34760, #17431, #83514 ),
 .UNSPECIFIED., .F., .F.,
 ( 4, 2, 2, 4 ),
 ( 0.000000000000000000, 0.0002567066673176301821, 0.0005134133346352603641, 0.001026826669270521596 ),
 .UNSPECIFIED. ) ;
#90616 = CARTESIAN_POINT ( 'NONE',  ( 5.936183876523434932, 1.091049494364674466, -1.918236432931222257 ) ) ;
#90617 = LINE ( 'NONE', #189159, #130396 ) ;
#90618 = CARTESIAN_POINT ( 'NONE',  ( 4.243358471946375943, -1.921622210924242458, 1.084848892642875429 ) ) ;
#90619 = CARTESIAN_POINT ( 'NONE',  ( 5.947222937888848371, 10.09017719417900416, 1.040834085586084257E-14 ) ) ;
#90620 = CARTESIAN_POINT ( 'NONE',  ( 1.364683531250000748, 8.567708333674730170, -0.7879004041258355073 ) ) ;
#90621 = CARTESIAN_POINT ( 'NONE',  ( 2.947808941170467545, -1.285945688040548207, -1.415481726668985196 ) ) ;
#90622 = CARTESIAN_POINT ( 'NONE',  ( 9.236128959407556849, 11.79856975744075598, -1.599625672291262513 ) ) ;
#90623 = CARTESIAN_POINT ( 'NONE',  ( 4.879381568908511824, -0.1049739508458477355, 2.067839077007492143 ) ) ;
#90625 = CARTESIAN_POINT ( 'NONE',  ( -11.41381675112453387, 10.89999999999998259, 3.704697986577180746 ) ) ;
#90624 = CARTESIAN_POINT ( 'NONE',  ( 9.616417370072170456, -9.251786168353179463, -0.2979722244324772840 ) ) ;
#90626 = CARTESIAN_POINT ( 'NONE',  ( 5.653911837654605144, 0.8871495062587383407, 2.004161502255866090 ) ) ;
#90627 = ORIENTED_EDGE ( 'NONE', *, *, #126677, .F. ) ;
#90628 = CARTESIAN_POINT ( 'NONE',  ( -9.555169238417182243, -7.776896528353606897, 0.04234008746932083761 ) ) ;
#90629 = CARTESIAN_POINT ( 'NONE',  ( 4.201496546123638431, 3.900130496719715456, 1.214306433183764966E-14 ) ) ;
#90630 = ADVANCED_FACE ( 'NONE', ( #158817 ), #72610, .T. ) ;
#90631 = CARTESIAN_POINT ( 'NONE',  ( 5.747730777550676073, 5.670383760089384495, 0.000000000000000000 ) ) ;
#90632 = CARTESIAN_POINT ( 'NONE',  ( 3.285556943749998737, -1.042708332855377451, -1.896917185911906722 ) ) ;
#90633 = CARTESIAN_POINT ( 'NONE',  ( -0.1104750535120025967, -0.004616138082884357029, -2.103378236956429337 ) ) ;
#90634 = CARTESIAN_POINT ( 'NONE',  ( -7.863365906246061243, 10.19701286208565705, -1.443375672974059665 ) ) ;
#90635 = CARTESIAN_POINT ( 'NONE',  ( 5.571474780572990504, 5.464751763615448787, 0.7998128361456352531 ) ) ;
#90636 = CARTESIAN_POINT ( 'NONE',  ( 5.524307029080702591, 1.015476208609331188, 1.803995072556117574 ) ) ;
#90637 = CARTESIAN_POINT ( 'NONE',  ( 4.283760221956850245, 1.259274395394771817, 1.458037640750938779 ) ) ;
#90638 = CARTESIAN_POINT ( 'NONE',  ( 0.1754079408978586052, 1.496066871905444629, 1.352139405095334590 ) ) ;
#90639 = DIRECTION ( 'NONE',  ( -8.638326563840814399E-31, 0.000000000000000000, -1.000000000000000000 ) ) ;
#90640 = CARTESIAN_POINT ( 'NONE',  ( 4.085803189671889157, 5.860132702740892263, -1.599625672291273171 ) ) ;
#90641 = CARTESIAN_POINT ( 'NONE',  ( -4.207825419487694063, 3.977679809700697788, -0.5488412742886485951 ) ) ;
#90642 = CARTESIAN_POINT ( 'NONE',  ( 6.685440801012543233, -0.9854850593251741619, 2.067252628450669594 ) ) ;
#90643 = CARTESIAN_POINT ( 'NONE',  ( 5.725187622324654946, -0.04035785615889506128, 1.825416780793003069 ) ) ;
#90644 = CARTESIAN_POINT ( 'NONE',  ( 6.048345925472191631, 7.189396680206621149, 1.082531754730549967 ) ) ;
#90645 = CARTESIAN_POINT ( 'NONE',  ( 2.995988758495615745, 6.439144618312774959, -0.7216878364870267237 ) ) ;
#90646 = CARTESIAN_POINT ( 'NONE',  ( -6.818824913030298696, 6.919993584815607335, 0.7998128361456341429 ) ) ;
#90647 = CARTESIAN_POINT ( 'NONE',  ( 5.529027716274630855, 5.344953845275508542, 1.040834085586084257E-14 ) ) ;
#90648 = CARTESIAN_POINT ( 'NONE',  ( 3.393283585170187688, 7.180857625999046867, 0.7998128361456271485 ) ) ;
#90649 = EDGE_LOOP ( 'NONE', ( #15611, #60807, #121045, #212895 ) ) ;
#90651 = CARTESIAN_POINT ( 'NONE',  ( 6.345953593097265255, -1.318148336383131669, -1.521719194605136494 ) ) ;
#90650 = CARTESIAN_POINT ( 'NONE',  ( 2.243484787601189634, 1.840893492186860492, 0.04347913094143729396 ) ) ;
#90652 = CARTESIAN_POINT ( 'NONE',  ( 0.8436309607196719185, -1.274966737007717343, 1.912178556870794521 ) ) ;
#90653 = CARTESIAN_POINT ( 'NONE',  ( 6.578960362708798471, 1.829258725439562916, 0.7091506158454219388 ) ) ;
#90654 = CARTESIAN_POINT ( 'NONE',  ( -5.904739593951539689, 6.847616600153594746, 1.199719254218450271 ) ) ;
#90655 = CARTESIAN_POINT ( 'NONE',  ( -2.435661151949389147, 5.993355110582911038, 0.7998128361456341429 ) ) ;
#90656 = CARTESIAN_POINT ( 'NONE',  ( 0.4849360239999983557, 1.980737741294085419, 0.6024896509310638804 ) ) ;
#90657 = CARTESIAN_POINT ( 'NONE',  ( -5.939880696562884310, 9.943961556049767836, 0.7216878364870267237 ) ) ;
#90659 = CARTESIAN_POINT ( 'NONE',  ( 1.481098450213329976, 1.729700800547562478, -0.7128637423776186255 ) ) ;
#90658 = CARTESIAN_POINT ( 'NONE',  ( 2.964485117831549665, -1.932750628810533389, -0.7978010075700513459 ) ) ;
#90660 = CARTESIAN_POINT ( 'NONE',  ( 1.598982282203027516, 0.9961506480390787122, -1.752761228829378126 ) ) ;
#90661 = CARTESIAN_POINT ( 'NONE',  ( 9.083599731475988648, 10.66024977721925104, 1.082531754730549967 ) ) ;
#90662 = ORIENTED_EDGE ( 'NONE', *, *, #30212, .T. ) ;
#90663 = CARTESIAN_POINT ( 'NONE',  ( -1.364683531250012516, 4.801041667008083991, -0.7879004041258300672 ) ) ;
#90664 = CARTESIAN_POINT ( 'NONE',  ( 1.645671328968565605, 0.5460171089132167532, 1.652615436037402130 ) ) ;
#90665 = CARTESIAN_POINT ( 'NONE',  ( 4.473300617505036492, 7.306268922809479704, -1.199719254218452047 ) ) ;
#90667 = CARTESIAN_POINT ( 'NONE',  ( 5.490689023410174840, 5.508151403507718591, -0.7216878364870152884 ) ) ;
#90666 =( NAMED_UNIT ( * ) SI_UNIT ( $, .STERADIAN. ) SOLID_ANGLE_UNIT ( ) );
#90668 = CARTESIAN_POINT ( 'NONE',  ( 2.894803161253765467, 1.479297447286776590, -0.8868043451095276586 ) ) ;
#90669 = CARTESIAN_POINT ( 'NONE',  ( 3.140350738262797314, 0.5347024899306859202, 2.125194831261326911 ) ) ;
#90670 = CARTESIAN_POINT ( 'NONE',  ( 5.408869034151480903, 1.673104959687292448, -1.439203791633147267 ) ) ;
#90671 = CARTESIAN_POINT ( 'NONE',  ( -10.96415609372974131, 4.387140345944800401, -6.371816014364277692 ) ) ;
#90672 = VECTOR ( 'NONE', #42230, 1000.000000000000000 ) ;
#90673 = CARTESIAN_POINT ( 'NONE',  ( 2.026474435558190734, 1.113403481674969608, 1.863675736879222278 ) ) ;
#90674 = CARTESIAN_POINT ( 'NONE',  ( 1.172165686010542274, -1.159919637379997814, 1.409874495853599141 ) ) ;
#90675 = SURFACE_SIDE_STYLE ('',( #139421 ) ) ;
#90676 = CARTESIAN_POINT ( 'NONE',  ( 4.522735144945882801, 0.3654406173194921781, 2.085432885242066270 ) ) ;
#90677 = CARTESIAN_POINT ( 'NONE',  ( -0.7500000000000006661, 9.739583334016129967, -1.299038105676657340 ) ) ;
#90678 = EDGE_CURVE ( 'NONE', #180121, #133382, #94789, .T. ) ;
#90679 = ORIENTED_EDGE ( 'NONE', *, *, #213686, .F. ) ;
#90681 = CARTESIAN_POINT ( 'NONE',  ( -1.364683531250000748, 1.321875000341421469, 0.000000000000000000 ) ) ;
#90680 = CARTESIAN_POINT ( 'NONE',  ( 4.247812404936269992, 2.291854478692372687, -0.05604449276840757499 ) ) ;
#90682 = CARTESIAN_POINT ( 'NONE',  ( -5.249999999999987566, 0.9165151389911689872, 1.199999999999999734 ) ) ;
#90683 = CARTESIAN_POINT ( 'NONE',  ( 3.571683402196252910, 6.254382171615883834, 1.199719254218462483 ) ) ;
#90684 = CARTESIAN_POINT ( 'NONE',  ( 0.2762449081346768365, 2.096790360132039233, -0.3154013857558089495 ) ) ;
#90685 = CARTESIAN_POINT ( 'NONE',  ( -4.934804725694212912, 8.701096580044490381, -0.7216878364870207285 ) ) ;
#90686 = ADVANCED_FACE ( 'NONE', ( #123958 ), #116959, .F. ) ;
#90687 = CARTESIAN_POINT ( 'NONE',  ( 5.043269954603547767, 4.986162489899998995, -0.7216878364870197293 ) ) ;
#90688 = CARTESIAN_POINT ( 'NONE',  ( -7.334597914868743018, 7.659378443542744996, -0.7216878364870267237 ) ) ;
#90689 = CARTESIAN_POINT ( 'NONE',  ( 6.825078400183556049, 7.053092130845653784, 2.453807127456457238 ) ) ;
#90690 = EDGE_LOOP ( 'NONE', ( #27433, #120934, #180584, #205922, #128045, #178145, #63161, #158337, #203829, #185589, #7893, #154186, #175580 ) ) ;
#90691 = CARTESIAN_POINT ( 'NONE',  ( 5.713517581197447015, 1.944070655204039433, 0.5350908816983344085 ) ) ;
#90693 = CARTESIAN_POINT ( 'NONE',  ( 3.414939784243501641, -1.565044402038212379, 1.343584798420148774 ) ) ;
#90692 = CARTESIAN_POINT ( 'NONE',  ( 6.335737856287750880, 6.286115675290828264, -0.7998128361456281477 ) ) ;
#90695 = CARTESIAN_POINT ( 'NONE',  ( -0.2408018239684642792, 7.629137130509051623, -2.700476273684692785 ) ) ;
#90694 = CARTESIAN_POINT ( 'NONE',  ( 0.4461838333974484927, 2.877219473291486640, 1.949594826320268481 ) ) ;
#90696 = CARTESIAN_POINT ( 'NONE',  ( 3.729901657090948230, 6.405283462364505631, 1.082531754730549078 ) ) ;
#90697 = CARTESIAN_POINT ( 'NONE',  ( 1.001543065824772753E-15, -3.871874999522043836, 3.793834371823811669 ) ) ;
#90698 = DIRECTION ( 'NONE',  ( 0.2636569930688775210, -0.9646164989289152114, 0.000000000000000000 ) ) ;
#90699 = CARTESIAN_POINT ( 'NONE',  ( 6.492125937493531396, -0.5805207454109837517, -2.113085764653479082 ) ) ;
#90700 = CARTESIAN_POINT ( 'NONE',  ( 3.393204081532863459, -0.8197727808607684352, -1.842447475547980495 ) ) ;
#90701 = CARTESIAN_POINT ( 'NONE',  ( 3.280630368989821743, 1.663260157205956880, -0.7901080472864712156 ) ) ;
#90702 = EDGE_CURVE ( 'NONE', #171990, #11347, #103347, .T. ) ;
#90703 = CARTESIAN_POINT ( 'NONE',  ( 6.958359152311676787, 9.141171649162195934, -1.599625672291262513 ) ) ;
#90704 = SURFACE_SIDE_STYLE ('',( #105910 ) ) ;
#90705 = CARTESIAN_POINT ( 'NONE',  ( 6.809597967592865508, -0.3964169337347979161, 1.788522171948719874 ) ) ;
#90706 = CARTESIAN_POINT ( 'NONE',  ( 0.3175262209036809891, 1.174723722100686762, -1.975753589677962552 ) ) ;
#90707 = CARTESIAN_POINT ( 'NONE',  ( -7.711890448074853133, 7.891627032375787998, -0.7998128361456291469 ) ) ;
#90708 = CARTESIAN_POINT ( 'NONE',  ( 6.825078400183548055, -0.008500281443135982926, 2.244262395727573356 ) ) ;
#90709 = CARTESIAN_POINT ( 'NONE',  ( 2.280028682641733973, 1.296546612978483504, 1.659573824544317455 ) ) ;
#90710 = CARTESIAN_POINT ( 'NONE',  ( -4.827585214917754719, 7.789877296449459365, -1.199719254218453823 ) ) ;
#90711 = CARTESIAN_POINT ( 'NONE',  ( 7.456094412511537151, 10.78619501698377370, 1.199719254218460707 ) ) ;
#90712 = CARTESIAN_POINT ( 'NONE',  ( 6.604230223188150894, 9.758666789477915771, -1.082531754730548412 ) ) ;
#90713 = DIRECTION ( 'NONE',  ( -0.6483454320283801309, 0.000000000000000000, 0.7613463080411788653 ) ) ;
#90714 = CARTESIAN_POINT ( 'NONE',  ( -6.684333426737305572, 7.757142738403693727, -1.199719254218446718 ) ) ;
#90715 = CARTESIAN_POINT ( 'NONE',  ( 6.439759776366758892, 10.45687747249582955, 0.7216878364870438212 ) ) ;
#90716 = CARTESIAN_POINT ( 'NONE',  ( 4.075236096247129680, 7.726954018008360237, 0.5961105570580684798 ) ) ;
#90717 = CARTESIAN_POINT ( 'NONE',  ( -4.252453736180621391, 8.112946458852704268, -0.7998128361456281477 ) ) ;
#90718 = CARTESIAN_POINT ( 'NONE',  ( 4.025785557498418044, -0.3775041287265075152, 2.188942893082143293 ) ) ;
#90719 = CARTESIAN_POINT ( 'NONE',  ( 1.974822964535282610, -0.1094934731284517848, -2.188836591978132518 ) ) ;
#90720 = CIRCLE ( 'NONE', #66381, 11.09999999999999964 ) ;
#90721 = CARTESIAN_POINT ( 'NONE',  ( 0.5224629442122545875, -1.184049029929446828, -1.862174541895257995 ) ) ;
#90722 = CARTESIAN_POINT ( 'NONE',  ( -3.772911886352873445, 7.623757310712140800, 0.7998128361456352531 ) ) ;
#90723 = CARTESIAN_POINT ( 'NONE',  ( 4.545333077707183200, 1.753367681936630840, -0.8802267832125689750 ) ) ;
#90724 = CARTESIAN_POINT ( 'NONE',  ( 8.204655514564224816, 12.72384853363364066, 1.040834085586084257E-14 ) ) ;
#90725 = CARTESIAN_POINT ( 'NONE',  ( 1.364683531249988757, 0.8843750003414210248, 0.000000000000000000 ) ) ;
#90726 = CARTESIAN_POINT ( 'NONE',  ( -5.017926250833627755, 5.026871178826882947, 0.7216878364870257245 ) ) ;
#90728 = VERTEX_POINT ( 'NONE', #20997 ) ;
#90727 = CARTESIAN_POINT ( 'NONE',  ( -4.595850885352567694, 8.305650432979225783, 1.040834085586084257E-14 ) ) ;
#90729 = CARTESIAN_POINT ( 'NONE',  ( 3.041385797112206912, 0.05609166564453024750, 2.120036961950934273 ) ) ;
#90730 = CARTESIAN_POINT ( 'NONE',  ( -3.122120512896910505, 6.864500708346841229, 0.7998128361456352531 ) ) ;
#90731 = CARTESIAN_POINT ( 'NONE',  ( 4.997027575558514734, 1.799266821141291661, -1.197868618907194316 ) ) ;
#90732 = CARTESIAN_POINT ( 'NONE',  ( 4.177188522404684079, 1.205947341878073287, 1.391433828303423326 ) ) ;
#90733 = CARTESIAN_POINT ( 'NONE',  ( -5.638288519115033814, 6.168138913823901781, 0.8326226707794943671 ) ) ;
#90734 = CARTESIAN_POINT ( 'NONE',  ( -1.364683531250012516, 1.092708333674754506, 0.7879004041258379498 ) ) ;
#90735 = CARTESIAN_POINT ( 'NONE',  ( 0.3975144409600079309, -0.5839149016878465437, -1.639678601710597983 ) ) ;
#90736 = CARTESIAN_POINT ( 'NONE',  ( 6.727182134110231360, 6.039168392632435989, 2.405853653942995773 ) ) ;
#90737 = CARTESIAN_POINT ( 'NONE',  ( 2.738383840280328663, 5.178236332760252303, 1.082531754730548412 ) ) ;
#90738 = CARTESIAN_POINT ( 'NONE',  ( -6.468692700515624949, 6.719432036793461904, 1.751973777778555601E-06 ) ) ;
#90739 = CARTESIAN_POINT ( 'NONE',  ( 3.854492016355787420, 0.7758605394001509836, 2.017853709245204463 ) ) ;
#90740 = CARTESIAN_POINT ( 'NONE',  ( -3.750802052474980108, 7.527686161196117887, 1.040834085586084257E-14 ) ) ;
#90741 = AXIS2_PLACEMENT_3D ( 'NONE', #78487, #144604, #179205 ) ;
#90742 = CARTESIAN_POINT ( 'NONE',  ( 5.255232437486731634, -2.000551055875991580, -0.2495666058281582056 ) ) ;
#90743 = CARTESIAN_POINT ( 'NONE',  ( -8.961576348508655698, 9.557519949455999253, -0.7216878364870267237 ) ) ;
#90745 = CARTESIAN_POINT ( 'NONE',  ( 4.012696165952275962, 1.530467462299599513, -1.526897427004340280 ) ) ;
#90744 = CIRCLE ( 'NONE', #211764, 9.579999999999992966 ) ;
#90746 = CARTESIAN_POINT ( 'NONE',  ( 4.218015588379292247, -1.010805368333337562, -1.692340417948991371 ) ) ;
#90747 = ADVANCED_FACE ( 'NONE', ( #87094 ), #161183, .T. ) ;
#90748 = CARTESIAN_POINT ( 'NONE',  ( -0.02351032182101517320, -2.127384168920816165, -0.5261613093957145937 ) ) ;
#90749 = CARTESIAN_POINT ( 'NONE',  ( 0.5698726823011552867, 0.2221484770595567870, -2.296888066578778087 ) ) ;
#90750 = CARTESIAN_POINT ( 'NONE',  ( 4.024726114628586870, 1.955573890245201785, 0.6501785607586229032 ) ) ;
#90751 = CARTESIAN_POINT ( 'NONE',  ( 5.636261916347573120, 0.3829244189050336478, 1.903776902374450630 ) ) ;
#90752 = CARTESIAN_POINT ( 'NONE',  ( -8.988692655735990300, 9.589155641221221771, 0.7216878364870438212 ) ) ;
#90754 = EDGE_CURVE ( 'NONE', #187511, #134057, #8956, .T. ) ;
#90753 = CARTESIAN_POINT ( 'NONE',  ( -6.095272577795516789, 9.268845886473535245, 1.199719254218452047 ) ) ;
#90755 = EDGE_LOOP ( 'NONE', ( #114514, #13203 ) ) ;
#90756 = CARTESIAN_POINT ( 'NONE',  ( -7.334597914868727919, 10.54048608644677465, -1.082531754730543083 ) ) ;
#90757 = CARTESIAN_POINT ( 'NONE',  ( 2.204404769108789797, -2.206272049354717879, 0.05393164079612459277 ) ) ;
#90758 = CARTESIAN_POINT ( 'NONE',  ( 0.000000000000000000, -0.1968749995220437643, -3.793834371823813001 ) ) ;
#90759 = ORIENTED_EDGE ( 'NONE', *, *, #64317, .T. ) ;
#90760 = CARTESIAN_POINT ( 'NONE',  ( 6.420756404446519738, -1.389671697431221542, 1.384925340169262054 ) ) ;
#90761 = CARTESIAN_POINT ( 'NONE',  ( -0.02880301295726198432, 6.946859453142047336, -2.868871865197111681 ) ) ;
#90762 = CARTESIAN_POINT ( 'NONE',  ( -1.499999999999997780, 4.931250000682820378, 1.214306433183764966E-14 ) ) ;
#90763 = CARTESIAN_POINT ( 'NONE',  ( -9.488641820551103834, -8.233137084989849086, 0.4644097342743111478 ) ) ;
#90765 = CARTESIAN_POINT ( 'NONE',  ( 0.3999999999999663824, 2.999999999999995559, 0.3423093779009733773 ) ) ;
#90764 = CARTESIAN_POINT ( 'NONE',  ( 1.419999999999989049, 6.280000000000042881, -2.873333333333328632 ) ) ;
#90766 = CARTESIAN_POINT ( 'NONE',  ( 5.454971364017034752, 0.3553261626877933788, -1.806350769464920569 ) ) ;
#90767 = VERTEX_POINT ( 'NONE', #192042 ) ;
#90768 = CARTESIAN_POINT ( 'NONE',  ( 2.659116476608857305, -1.792500920499852546, -1.016832356063899656 ) ) ;
#90769 = CARTESIAN_POINT ( 'NONE',  ( 1.360316468749968033, 1.015625000341371820, -4.163336342344337027E-14 ) ) ;
#90770 = CARTESIAN_POINT ( 'NONE',  ( -6.856673000209188906, 9.022537805042615489, 1.599625672291283607 ) ) ;
#90771 = CARTESIAN_POINT ( 'NONE',  ( -11.94105721237523277, 19.00000000000000000, 1.187919463087248273 ) ) ;
#90772 = CARTESIAN_POINT ( 'NONE',  ( 5.606460214450851964, 6.499623990736163037, 1.199719254218462483 ) ) ;
#90773 = AXIS2_PLACEMENT_3D ( 'NONE', #67209, #198287, #183121 ) ;
#90774 = CARTESIAN_POINT ( 'NONE',  ( 0.7255486961553169190, -1.957115920898297112, 0.6459669076722980297 ) ) ;
#90776 = CARTESIAN_POINT ( 'NONE',  ( 4.792441439910442469, 1.527937338083688923, -1.027124420945781935 ) ) ;
#90775 = DIRECTION ( 'NONE',  ( -0.6507913734559658270, 0.7592566023652989049, 0.000000000000000000 ) ) ;
#90777 = CARTESIAN_POINT ( 'NONE',  ( 8.145751363712157911, 8.397798100619326078, -0.7998128361456281477 ) ) ;
#90778 = CARTESIAN_POINT ( 'NONE',  ( -5.875479466675803231, 7.948088359245467416, -1.599625672291271394 ) ) ;
#90780 = EDGE_LOOP ( 'NONE', ( #61181, #42085, #92063, #74776 ) ) ;
#90779 = CARTESIAN_POINT ( 'NONE',  ( -0.2409995289980246258, 2.020898751655671788, -2.415740196953279462 ) ) ;
#90781 = CARTESIAN_POINT ( 'NONE',  ( 4.160898416275903067, -1.636102012888400292, 1.481223685352812680 ) ) ;
#90782 = CARTESIAN_POINT ( 'NONE',  ( 0.4917760118960182170, 1.601382895956671826, 1.452064325093614716 ) ) ;
#90783 = CARTESIAN_POINT ( 'NONE',  ( -6.236387472606166327, 6.378132927569716060, -0.7216878364870278340 ) ) ;
#90784 = CARTESIAN_POINT ( 'NONE',  ( 0.6856317642073318508, 1.842354612247762091, -0.5124485439033445999 ) ) ;
#90785 = CARTESIAN_POINT ( 'NONE',  ( 0.7785302072789467287, -0.4946362931835950327, -1.954778448132548752 ) ) ;
#90786 = CARTESIAN_POINT ( 'NONE',  ( 6.743451144134843922, 15.00000000000000000, -9.536680065235831449 ) ) ;
#90787 = CARTESIAN_POINT ( 'NONE',  ( 7.504827820433121133, 15.48994999688346574, -9.370061686304214987 ) ) ;
#90788 = CARTESIAN_POINT ( 'NONE',  ( 6.305323439471717251, 1.661359358424657318, -0.9468341723649562613 ) ) ;
#90789 = CARTESIAN_POINT ( 'NONE',  ( 0.6724591444495706671, -1.759989063064151038, -0.6342292696241008665 ) ) ;
#90790 = CARTESIAN_POINT ( 'NONE',  ( 1.850796360583713884, -1.845628094615419768, -0.8128149310912060610 ) ) ;
#90792 = CARTESIAN_POINT ( 'NONE',  ( -4.943116297174857898, 7.129802832403653312, 1.247573795494796078 ) ) ;
#90791 = CARTESIAN_POINT ( 'NONE',  ( 1.364683531249986537, 0.6135416670080880985, 0.7879004041258500513 ) ) ;
#90794 = CARTESIAN_POINT ( 'NONE',  ( 3.598352328373265685, -2.103663943315597251, -0.1031874809700270568 ) ) ;
#90793 = CARTESIAN_POINT ( 'NONE',  ( -7.666245793523398078, 11.03137162816423356, 1.199719254218453823 ) ) ;
#90795 = CARTESIAN_POINT ( 'NONE',  ( 6.825640269476072497, 10.05066518344239412, 1.199719254218460707 ) ) ;
#90797 = CARTESIAN_POINT ( 'NONE',  ( -7.069687034522070590, 10.33538640932937724, -1.199719254218440723 ) ) ;
#90796 = CARTESIAN_POINT ( 'NONE',  ( 3.576318658954677598, 7.394398545414291313, 0.7998128361456281477 ) ) ;
#90798 = CARTESIAN_POINT ( 'NONE',  ( 11.43190902327452108, 9.944778717421318248, 3.649704988378163595 ) ) ;
#90799 = CARTESIAN_POINT ( 'NONE',  ( 3.726823374262774990, 1.425363347867984798, -1.431309510556647346 ) ) ;
#90800 = CARTESIAN_POINT ( 'NONE',  ( -1.364683531249997417, 5.259375000341425022, 1.214306433183764966E-14 ) ) ;
#90801 = CARTESIAN_POINT ( 'NONE',  ( 8.107412671292022921, 12.40247251657532956, 0.7216878364870438212 ) ) ;
#90802 = CARTESIAN_POINT ( 'NONE',  ( 4.130267194010744269, 1.160198474277823300, -1.823679694223250491 ) ) ;
#90803 = CARTESIAN_POINT ( 'NONE',  ( 6.038177310039780643, 8.137902509836795417, -1.599625672291283607 ) ) ;
#90804 = CARTESIAN_POINT ( 'NONE',  ( -0.6823417656250003738, 0.03020833367475134201, -1.181850606188749264 ) ) ;
#90806 = CARTESIAN_POINT ( 'NONE',  ( -9.620809655836554342, -9.180994456877138887, 0.3503521373105362158 ) ) ;
#90805 = CARTESIAN_POINT ( 'NONE',  ( 7.042534447655770080, 7.180988041878682004, -0.7998128361456341429 ) ) ;
#90807 = CARTESIAN_POINT ( 'NONE',  ( 8.636180661780656465, 11.09863007687603087, -1.443375672974052559 ) ) ;
#90809 = CARTESIAN_POINT ( 'NONE',  ( -0.03146710860974352708, -8.100320323339552431, 10.94525894661336274 ) ) ;
#90808 = CARTESIAN_POINT ( 'NONE',  ( 2.313135284333038832, -1.679484837851461965, 1.376015783590480934 ) ) ;
#90811 = CARTESIAN_POINT ( 'NONE',  ( 1.223879446662301307, 1.774596971308094018, 0.4907264878865265634 ) ) ;
#90810 = CARTESIAN_POINT ( 'NONE',  ( -4.758548728716557541, 8.495464583570553785, 1.040834085586084257E-14 ) ) ;
#90812 = CARTESIAN_POINT ( 'NONE',  ( -1.364683531250014514, 1.488541667008084435, -0.7879004041258289570 ) ) ;
#90813 = CARTESIAN_POINT ( 'NONE',  ( 3.280998142716429200, 1.980384277226649559, -0.9389412094223739125 ) ) ;
#90814 = CARTESIAN_POINT ( 'NONE',  ( -0.06290936665214684476, -8.043994141378487228, 10.94971099608171627 ) ) ;
#90815 = CARTESIAN_POINT ( 'NONE',  ( 4.153392199625399073, -1.879142691831453105, -1.259808711832038464 ) ) ;
#90816 = CARTESIAN_POINT ( 'NONE',  ( -5.845536785786364931, 9.971543350059432598, 0.000000000000000000 ) ) ;
#90817 = CARTESIAN_POINT ( 'NONE',  ( 4.645720405014278853, 1.993893748393640086, -0.3006458143828410479 ) ) ;
#90818 = CARTESIAN_POINT ( 'NONE',  ( -1.364683531250010295, 4.592708333674755394, 0.7879004041258379498 ) ) ;
#90819 = CARTESIAN_POINT ( 'NONE',  ( 6.053075614097062740, 7.042710966267798689, -1.019147762646470001 ) ) ;
#90820 = CARTESIAN_POINT ( 'NONE',  ( -6.009258394948636914E-15, 12.93749999999999822, -1.732050807568875195 ) ) ;
#90821 = CARTESIAN_POINT ( 'NONE',  ( 4.570507181582611267, 8.346359121906111511, 0.000000000000000000 ) ) ;
#90822 = CARTESIAN_POINT ( 'NONE',  ( 4.833122733705673468, -1.618250600028045216, 0.7167863974541763827 ) ) ;
#90823 = CARTESIAN_POINT ( 'NONE',  ( 7.422199028477372451, 10.74665040227725044, -1.199719254218441611 ) ) ;
#90824 = CARTESIAN_POINT ( 'NONE',  ( 0.2882880397960294605, -0.9922573751702695732, 1.857558580286112981 ) ) ;
#90825 = PRESENTATION_LAYER_ASSIGNMENT (  '', '', ( #194545 ) ) ;
#90827 = CARTESIAN_POINT ( 'NONE',  ( -1.500000000000001332, 0.9000000000000187850, 0.000000000000000000 ) ) ;
#90826 = CARTESIAN_POINT ( 'NONE',  ( 0.6823417656249934904, 11.19270833367473550, 1.181850606188764807 ) ) ;
#90828 = CARTESIAN_POINT ( 'NONE',  ( 0.7659823462377189918, -1.960405762330315049, 0.1893847968462581133 ) ) ;
#90829 = CARTESIAN_POINT ( 'NONE',  ( -5.008811405605897882, 4.808311159487113073, 0.7998128361456281477 ) ) ;
#90830 = CARTESIAN_POINT ( 'NONE',  ( -0.1467296397388559992, 8.209138825498280667, -2.038183423090501378 ) ) ;
#90832 = VERTEX_POINT ( 'NONE', #27425 ) ;
#90831 = CARTESIAN_POINT ( 'NONE',  ( 5.607607993782223410, 1.377354484090735243, 1.176896650239395603 ) ) ;
#90833 = CARTESIAN_POINT ( 'NONE',  ( 5.802526556968819804, 9.713438716531550554, -0.7216878364870267237 ) ) ;
#90834 = CARTESIAN_POINT ( 'NONE',  ( 8.387690588348714726, 12.93738945304888333, 1.040834085586084257E-14 ) ) ;
#90835 = CARTESIAN_POINT ( 'NONE',  ( 5.172658500931742509, -1.761684834526537680, -0.6294727512598657926 ) ) ;
#90836 = CARTESIAN_POINT ( 'NONE',  ( 4.701980345841006326, 4.380065246436280368, 0.7998128361456341429 ) ) ;
#90837 = CARTESIAN_POINT ( 'NONE',  ( 4.012602964903419611, 0.7404812365185128309, 1.933494928807255153 ) ) ;
#90838 = CARTESIAN_POINT ( 'NONE',  ( -0.6125000000000019318, 1.458333333333332371, -1.060881119635941339 ) ) ;
#90839 = CARTESIAN_POINT ( 'NONE',  ( -5.763624699140883934, 6.857221916153382502, -1.082531754730549967 ) ) ;
#90840 = CARTESIAN_POINT ( 'NONE',  ( 3.028508906271001777, -0.9278780887907630559, -1.428417487556953525 ) ) ;
#90841 = CARTESIAN_POINT ( 'NONE',  ( 8.914649696185335870, 10.35917838609310593, -1.199719254218446718 ) ) ;
#90842 = CARTESIAN_POINT ( 'NONE',  ( -9.317477881089553549, 11.89347683273641820, 1.599625672291281386 ) ) ;
#90843 = CARTESIAN_POINT ( 'NONE',  ( 6.210516883511641772, 9.403297576475722508, 1.199719254218452047 ) ) ;
#90844 = CARTESIAN_POINT ( 'NONE',  ( -4.910477722004077172, 4.678539768940303212, -0.3136693401591003072 ) ) ;
#90845 = CARTESIAN_POINT ( 'NONE',  ( 1.364683531249988757, -0.3656249996585800299, 0.000000000000000000 ) ) ;
#90846 = CARTESIAN_POINT ( 'NONE',  ( 0.7499999999999867883, 0.3166666666666873020, -1.299038105676652899 ) ) ;
#90847 = CARTESIAN_POINT ( 'NONE',  ( 4.422284181769401634, 0.9229163912191931107, 1.731201473044993167 ) ) ;
#90848 = ADVANCED_FACE ( 'NONE', ( #181924 ), #43705, .F. ) ;
#90849 = CARTESIAN_POINT ( 'NONE',  ( 2.161482305958133399, -0.5350050527693461788, -1.943774068525660148 ) ) ;
#90850 = CARTESIAN_POINT ( 'NONE',  ( -2.324088772396477673E-16, -2.143749999044084031, -3.475000000000000089 ) ) ;
#90851 = CARTESIAN_POINT ( 'NONE',  ( -11.33772463945037323, 10.09097530385347774, 3.599999999999998312 ) ) ;
#90852 = CARTESIAN_POINT ( 'NONE',  ( -11.84668730067608600, 10.19999999999998153, 1.399999999999998357 ) ) ;
#90853 = CARTESIAN_POINT ( 'NONE',  ( 1.651402116136031051, 0.5479989942898423338, -1.788454331708405620 ) ) ;
#90854 = CARTESIAN_POINT ( 'NONE',  ( -0.6823417656250212460, 5.551041667008087543, 1.181850606188767472 ) ) ;
#90855 = CARTESIAN_POINT ( 'NONE',  ( 3.797138801009732667, -0.2017130330635922841, -2.003102573442970158 ) ) ;
#90857 = CARTESIAN_POINT ( 'NONE',  ( 3.445011857661818944, -1.868279436719679110, -0.9960484452814029055 ) ) ;
#90856 = CARTESIAN_POINT ( 'NONE',  ( -6.738039156311804945, 6.963393225226301553, 1.040834085586084257E-14 ) ) ;
#90858 = CARTESIAN_POINT ( 'NONE',  ( 6.825078400183544503, 3.684911640780349718, 2.658296617506946458 ) ) ;
#90859 = CARTESIAN_POINT ( 'NONE',  ( 4.439934286204096914, 1.349936692791346093, 1.569845735447549906 ) ) ;
#90860 = CARTESIAN_POINT ( 'NONE',  ( 6.530187263637528439, 7.647581891445782709, -1.199719254218452047 ) ) ;
#90862 = DIRECTION ( 'NONE',  ( -0.000000000000000000, -1.000000000000000000, -0.000000000000000000 ) ) ;
#90861 = CARTESIAN_POINT ( 'NONE',  ( 0.2750908068406934803, 1.949304727321942599, -0.7563943737528535660 ) ) ;
#90864 = VERTEX_POINT ( 'NONE', #164629 ) ;
#90863 = CARTESIAN_POINT ( 'NONE',  ( 5.807590115592688562, -0.4411735188285180187, 1.771332044933016547 ) ) ;
#90865 = CARTESIAN_POINT ( 'NONE',  ( 9.077347539549325717, 10.54899253668443393, -1.199719254218446718 ) ) ;
#90866 = CARTESIAN_POINT ( 'NONE',  ( -0.4019237886466871523, 11.97991455036742714, -1.499999999999998668 ) ) ;
#90868 = AXIS2_PLACEMENT_3D ( 'NONE', #113586, #13860, #149209 ) ;
#90867 = CARTESIAN_POINT ( 'NONE',  ( -11.94105721839851952, 13.52698343341134191, 1.187919402540718927 ) ) ;
#90869 = CARTESIAN_POINT ( 'NONE',  ( -10.57368757801325820, 3.061359382655743033, 7.009609602318408683 ) ) ;
#90870 = CARTESIAN_POINT ( 'NONE',  ( 8.242994206984347372, 8.719174117677642499, 1.040834085586084257E-14 ) ) ;
#90871 = CARTESIAN_POINT ( 'NONE',  ( -1.364683531250010740, 11.44270833367472839, 0.7879004041258445001 ) ) ;
#90872 = CARTESIAN_POINT ( 'NONE',  ( 5.760397938718036848, 1.910310778393434106, 0.08934430699411573251 ) ) ;
#90873 = CARTESIAN_POINT ( 'NONE',  ( -9.996439331977562404, 10.55693406359564790, 0.7998128361456462443 ) ) ;
#90874 = CARTESIAN_POINT ( 'NONE',  ( 7.657657833620182153, 7.828355648845348291, -0.7998128361456281477 ) ) ;
#90875 = CARTESIAN_POINT ( 'NONE',  ( -1.360316468750026875, 2.671875000341383810, -2.602085213965210642E-14 ) ) ;
#90876 = DIRECTION ( 'NONE',  ( 0.000000000000000000, 0.000000000000000000, -1.000000000000000000 ) ) ;
#90877 = CARTESIAN_POINT ( 'NONE',  ( 5.007038802148489509, 4.735966778795008381, 0.7998128361456341429 ) ) ;
#90878 = ORIENTED_EDGE ( 'NONE', *, *, #201515, .F. ) ;
#90879 = CARTESIAN_POINT ( 'NONE',  ( -7.123883369337781879, 7.275895117174344229, 0.7998128361456341429 ) ) ;
#90880 = ADVANCED_FACE ( 'NONE', ( #125020 ), #32493, .T. ) ;
#90881 = CARTESIAN_POINT ( 'NONE',  ( 5.378529868213833609, -0.4926607797600784933, -1.955169007017331317 ) ) ;
#90882 = CARTESIAN_POINT ( 'NONE',  ( 4.627371609795830371E-16, 1.999999999999999556, -2.600000000000008082 ) ) ;
#90883 = CARTESIAN_POINT ( 'NONE',  ( 11.40591166468351503, 3.507114751586604129, -3.706005353348470255 ) ) ;
#90884 = CIRCLE ( 'NONE', #160126, 0.08000000000000020983 ) ;
#90885 = CARTESIAN_POINT ( 'NONE',  ( -0.1399997263889611598, 6.947783040739049731, -2.595329734540325006 ) ) ;
#90886 = CARTESIAN_POINT ( 'NONE',  ( -4.256897045010916258, 7.910204285913967404, 0.7216878364870317197 ) ) ;
#90887 = CARTESIAN_POINT ( 'NONE',  ( 8.419250204406344196, 12.76628297187536809, 1.040834085586084257E-14 ) ) ;
#90888 = CARTESIAN_POINT ( 'NONE',  ( 2.571101405699018017, 1.757081157110135017, 0.8898057773328130748 ) ) ;
#90889 = CARTESIAN_POINT ( 'NONE',  ( 4.728138764314923748, 2.011206665557175199, 0.1455158850461671372 ) ) ;
#90890 = CARTESIAN_POINT ( 'NONE',  ( -7.217017841176048165, 7.314275657660511243, 1.040834085586084257E-14 ) ) ;
#90891 = CARTESIAN_POINT ( 'NONE',  ( 6.827182134110238110, -0.009824402486291110986, 2.288967694407703313 ) ) ;
#90892 = CARTESIAN_POINT ( 'NONE',  ( 4.242245924764226572, 0.5834501570099770440, 2.112278566661344392 ) ) ;
#90893 = CARTESIAN_POINT ( 'NONE',  ( 2.819263867200746176, -0.1907306445340165024, 1.916936124417574661 ) ) ;
#90894 = CARTESIAN_POINT ( 'NONE',  ( -7.862839020921525091, 11.26073039346208660, -1.199719254218446718 ) ) ;
#90895 = CARTESIAN_POINT ( 'NONE',  ( 1.257539916218598286, 3.047412844624492134, 0.7750000000000100142 ) ) ;
#90896 = DIRECTION ( 'NONE',  ( 0.000000000000000000, 0.000000000000000000, -1.000000000000000000 ) ) ;
#90897 = CARTESIAN_POINT ( 'NONE',  ( -5.991201117307169532, 15.51884043567246962, -10.40697266434820634 ) ) ;
#90898 = CARTESIAN_POINT ( 'NONE',  ( 1.364683531250000748, 12.75520833367473372, -0.7879004041258355073 ) ) ;
#90899 = MECHANICAL_DESIGN_GEOMETRIC_PRESENTATION_REPRESENTATION (  '', ( #73555 ), #94468 ) ;
#90900 = CARTESIAN_POINT ( 'NONE',  ( 4.852928918687680948, 7.749168607522574526, 1.199719254218462483 ) ) ;
#90901 = CARTESIAN_POINT ( 'NONE',  ( 4.855228407469603269, 7.718164671139588151, -1.082531754730548412 ) ) ;
#90903 = CARTESIAN_POINT ( 'NONE',  ( 3.369792252087350892, 0.4868432662692974144, -1.953231169037449533 ) ) ;
#90902 = CARTESIAN_POINT ( 'NONE',  ( 5.794452930745782382, 1.501506822132542718, -1.065412412061928160 ) ) ;
#90904 = CARTESIAN_POINT ( 'NONE',  ( 5.747524558462486333, -2.240600987983232262, -0.5116226552598357458 ) ) ;
#90906 = CARTESIAN_POINT ( 'NONE',  ( 2.799463494909336880, -1.375353214051901807, -1.253764128285854706 ) ) ;
#90905 = CARTESIAN_POINT ( 'NONE',  ( -7.957709816578236506, 8.248692638954882028, 0.7998128361456341429 ) ) ;
#90907 = CARTESIAN_POINT ( 'NONE',  ( 3.285556943749998737, -0.2552083328553768071, -1.896917185911906500 ) ) ;
#90908 = LINE ( 'NONE', #140747, #15596 ) ;
#90909 = CARTESIAN_POINT ( 'NONE',  ( -6.886651960737580680, 10.12184548991413457, -1.199719254218440723 ) ) ;
#90910 = CARTESIAN_POINT ( 'NONE',  ( -4.123088112331656951, 6.864000993478624579, 1.082531754730549967 ) ) ;
#90911 = CARTESIAN_POINT ( 'NONE',  ( 6.515180868147061766, -2.027822497041928518, 0.5085933055150316795 ) ) ;
#90912 = CARTESIAN_POINT ( 'NONE',  ( 4.677199807034550183, 8.400557508274889784, 1.040834085586084257E-14 ) ) ;
#90913 = ORIENTED_EDGE ( 'NONE', *, *, #175999, .F. ) ;
#90914 = TOROIDAL_SURFACE ( 'NONE', #118631, 7.049999999999999822, 0.9999999999999997780 ) ;
#90915 = CARTESIAN_POINT ( 'NONE',  ( 5.573523442662557059, 5.863030555295438262, 0.6332236521834158083 ) ) ;
#90917 = CARTESIAN_POINT ( 'NONE',  ( 5.203632029546647608, 4.965325544092860532, 1.040834085586084257E-14 ) ) ;
#90916 = CARTESIAN_POINT ( 'NONE',  ( -1.499999999999946709, 7.750000000000000000, 15.75000000000000711 ) ) ;
#90918 = CARTESIAN_POINT ( 'NONE',  ( 6.393153111415212031, 1.496800677787715639, -0.8570667202875602575 ) ) ;
#90919 = CARTESIAN_POINT ( 'NONE',  ( -4.388035272317281077, 8.271124917678806199, 0.7998128361456481317 ) ) ;
#90920 = CARTESIAN_POINT ( 'NONE',  ( 1.441630353877725979, -1.487241779905050576, -0.8915045353455192112 ) ) ;
#90921 = CARTESIAN_POINT ( 'NONE',  ( -3.529886618686457478, 14.55202822082756065, 11.43118357259692708 ) ) ;
#90922 = DIRECTION ( 'NONE',  ( -0.000000000000000000, 1.000000000000000000, -0.000000000000000000 ) ) ;
#90923 = DIRECTION ( 'NONE',  ( -1.561251128379126077E-17, -1.301042606982605475E-17, -1.000000000000000000 ) ) ;
#90924 = CARTESIAN_POINT ( 'NONE',  ( 6.403213944470495633, -1.838587781526521248, 1.154350301468348272 ) ) ;
#90925 = CARTESIAN_POINT ( 'NONE',  ( 4.617693566336190436, -1.789886777702164089, 0.3589094947460610974 ) ) ;
#90926 = CARTESIAN_POINT ( 'NONE',  ( 2.518345088137901477, 0.8342845254802437882, 1.775630740545742992 ) ) ;
#90927 = DIRECTION ( 'NONE',  ( 0.000000000000000000, 1.000000000000000000, 0.000000000000000000 ) ) ;
#90928 = CARTESIAN_POINT ( 'NONE',  ( -9.938290294017125603, 11.55342575023019691, -1.199719254218441611 ) ) ;
#90929 = CARTESIAN_POINT ( 'NONE',  ( 7.456094412511537151, 10.78619501698377370, 1.199719254218460707 ) ) ;
#90930 = CARTESIAN_POINT ( 'NONE',  ( 3.229257539231108698, 1.917844101178723504, 0.9048822562475050679 ) ) ;
#90931 = CARTESIAN_POINT ( 'NONE',  ( -0.08058608058608696112, -6.134628647623513231, 10.99970480893081870 ) ) ;
#90932 = DIRECTION ( 'NONE',  ( 1.000000000000000000, -0.000000000000000000, -0.000000000000000000 ) ) ;
#90933 = CARTESIAN_POINT ( 'NONE',  ( -4.373759202716216876, 7.180157790548314267, -1.044885312346154782 ) ) ;
#90934 = CARTESIAN_POINT ( 'NONE',  ( 1.481394567461959522, -0.05474761849930119550, 2.069712792878583230 ) ) ;
#90936 = CARTESIAN_POINT ( 'NONE',  ( -0.6823417656250246877, -1.136458332991911790, 1.181850606188755259 ) ) ;
#90935 = CARTESIAN_POINT ( 'NONE',  ( 3.469446951953614189E-15, 6.400000000000023448, 1.214306433183764966E-14 ) ) ;
#90938 = ORIENTED_EDGE ( 'NONE', *, *, #159606, .T. ) ;
#90937 = CARTESIAN_POINT ( 'NONE',  ( 3.651236063859903069, 0.3270389233705518484, 2.196992388787385231 ) ) ;
#90939 = CARTESIAN_POINT ( 'NONE',  ( 1.741309990946012132, 2.292119649597070374, -0.1747640694012199680 ) ) ;
#90941 = CARTESIAN_POINT ( 'NONE',  ( 6.315292642669888323, -1.766025379077978741, -1.065358839237473099 ) ) ;
#90940 = CARTESIAN_POINT ( 'NONE',  ( 8.541273586929342798, 11.94827437051752206, -1.082531754730543083 ) ) ;
#90943 = CARTESIAN_POINT ( 'NONE',  ( -1.642778471875000035, -4.017708332855376874, -2.845375778867859751 ) ) ;
#90942 = CARTESIAN_POINT ( 'NONE',  ( 5.401997860402196316, 5.267028690082820930, 0.000000000000000000 ) ) ;
#90944 = DIRECTION ( 'NONE',  ( 0.000000000000000000, -1.000000000000000000, 0.000000000000000000 ) ) ;
#90945 = CARTESIAN_POINT ( 'NONE',  ( 4.837112831242089683, 4.711959172683063635, 0.000000000000000000 ) ) ;
#90946 = CARTESIAN_POINT ( 'NONE',  ( -9.906083622534515243, -9.418601272609036457, 0.1729113328156593465 ) ) ;
#90947 = EDGE_CURVE ( 'NONE', #204424, #80409, #101935, .T. ) ;
#90948 = CARTESIAN_POINT ( 'NONE',  ( -0.1104750535120268828, 2.006893987364383403, -2.517811492722863864 ) ) ;
#90949 = CARTESIAN_POINT ( 'NONE',  ( 3.328823242065849008, 0.04121275867331047893, 1.724443917160731976 ) ) ;
#90950 = CARTESIAN_POINT ( 'NONE',  ( 2.659388954101277847, 1.913261587491304150, -0.6371546050257800298 ) ) ;
#90951 = CARTESIAN_POINT ( 'NONE',  ( 3.323114718373169740, 1.032193166631629078, -2.053959190227053533 ) ) ;
#90952 =( BOUNDED_SURFACE ( )  B_SPLINE_SURFACE ( 3, 3, ( 
 ( #106772, #69916, #8143, #72055, #119833, #185812, #37444, #169580, #104597, #21163, #54766, #38519, #207410, #79551, #11335, #61169, #193299, #44944, #59029, #174944, #161888, #26526, #25458, #145669, #125187, #127330, #92634, #176004, #208463, #211666, #78481, #112129, #143531, #10272, #12400, #129462, #28675, #158675, #94762, #91565, #191148, #42817, #29747, #76348, #142455, #95831, #126256, #210613, #9215, #160809, #144598, #46008, #63302, #47075, #62240, #108922, #157618, #60098, #192215, #13475, #209527, #111052, #177058, #128399, #75286, #194366, #178132, #27596, #113193, #141401, #195446, #43878, #109992, #93695, #159737, #77416, #387, #2527, #166127, #99008, #101114, #181307, #67527, #167201, #197552, #82742, #182360, #15591, #146718, #18790, #165064, #66459, #132600, #198606, #212734, #114261, #84873, #180258, #179198, #150962, #64371, #50252, #31882, #115317, #147764, #68602, #17713, #51317, #148815, #164017, #83801, #134725, #33989, #97959, #100064, #30822, #130517, #196506, #183439, #81677, #213780, #35043, #65403, #149894, #162951, #1462, #133670, #199674, #200731, #52382, #117444, #48148, #96900, #131550, #49196, #14529, #116372, #80626, #32934, #16656, #184494, #203932, #23050, #120658, #206083, #36113, #6801, #69668, #185562, #119578, #205006, #85948, #136841, #104340, #38263, #202866, #155220, #56653, #103267, #55580, #4656, #121735, #135775, #118510, #186637, #54514, #37191, #70728, #24127, #169329, #20913, #201798, #187701, #156294, #72877, #89168, #153079, #170384, #21972, #7878, #53440, #88082, #122816, #19863, #87008, #152023, #154155, #5722, #138985, #71801, #188774, #40413, #102196, #106516, #140061, #168262, #90229, #3591, #172542, #73966, #137912, #39329, #105425, #171462, #91307, #158421, #61991, #175749, #143279, #77157, #209270, #123876, #60915, #176801, #59845, #145417, #189841, #160549, #8958, #124934, #58780, #144350, #25202, #76096, #43623, #191956, #142199, #94511, #210352, #42561, #127074, #10020, #193036, #75033, #57717, #125997, #208214, #190897, #109738, #177879, #108663, #174694, #141147, #44690, #95584, #12157, #28418, #92385, #27340, #93442, #161633, #207157, #159481, #128147, #173631, #26268, #157364, #11081, #110798, #78228, #194107, #45756, #111875, #41488, #29492, #79301, #107600, #13227, #178952, #141, #97706, #115064, #65157, #81434, #99816, #32678, #34795, #198357, #131313, #133416, #213534, #165881, #199422, #15342, #181060, #66207, #47902, #30566, #51066, #197305, #98757, #164813, #16405, #96646, #146463, #117189, #212480, #211417, #183189, #162700, #82485, #64123, #147513, #180007, #100869, #49997, #83551, #148572, #196255, #116120, #166956, #132354, #130266, #182108, #63049, #14272, #80367, #1214, #114012, #31629, #67277, #163764, #33737, #195190, #17467, #149633, #48944, #18546, #84622, #129214, #46826, #112939, #24678, #39888, #90784, #170935, #150714, #7353, #23610, #154700, #105998, #59327, #6283, #204478, #22534, #156847, #191446, #108152, #124422, #188247, #205560, #73432, #43111, #88643, #172019, #91862, #55064, #72356, #187183, #57200, #138459, #174178, #189325, #157917, #25749, #68350, #190380, #175236, #2274, #125484, #121214, #8431, #89719, #123360, #139535, #155769, #42040, #40966, #109226, #140622, #107074, #75584, #173097, #9512, #141694, #74519, #206634 ),
 ( #56131, #134483, #26820, #38810, #58265, #122290, #207707, #203411, #104896, #145947, #179491, #210897, #77708, #79839, #196792, #96121, #93992, #162176, #92924, #44164, #192512, #97187, #143828, #11635, #163240, #193591, #63596, #76639, #13762, #211958, #113484, #64657, #114549, #129751, #110284, #158970, #126551, #45235, #14822, #62524, #178426, #112414, #30035, #10564, #195736, #47371, #95052, #180540, #142753, #31113, #176293, #160033, #209825, #80914, #60387, #111350, #177355, #128686, #147004, #61461, #27897, #213022, #78767, #194655, #46299, #130798, #127627, #28969, #48433, #161103, #208762, #12691, #144890, #67814, #181591, #182659, #681, #86236, #85167, #118796, #150188, #16946, #19087, #136066, #35339, #33220, #101419, #32163, #197844, #131837, #36409, #83025, #165352, #102488, #132889, #2820, #15884, #167491, #151251, #52667, #3884, #53739, #68891, #49477, #98240, #65689, #198892, #168552, #1757, #117740, #51617, #183733, #164295, #135010, #201024, #34279, #119871, #81968, #184783, #115597, #99304, #149102, #20151, #214061, #50538, #18012, #166420, #116661, #152307, #69954, #66748, #202079, #100352, #148055, #84101, #133961, #199969, #55869, #186926, #138204, #91602, #38558, #22268, #203162, #56939, #9251, #140356, #156585, #6024, #23346, #105721, #75322, #54807, #72094, #124165, #87304, #120955, #4944, #89457, #170681, #206374, #7091, #190127, #58001, #103559, #8179, #207445, #37482, #157653, #153373, #189069, #204216, #155509, #39617, #122025, #74263, #73164, #141439, #172837, #171750, #107895, #187992, #41781, #173922, #25495, #71020, #139270, #205300, #123111, #40704, #59064, #185850, #88377, #106808, #24408, #90523, #104634, #169618, #21202, #137133, #154444, #77448, #30857, #192248, #176038, #142490, #210646, #162984, #79584, #95865, #159770, #177093, #44978, #14565, #208496, #11369, #63338, #26559, #60131, #158710, #28708, #110024, #145702, #160842, #129497, #211702, #42850, #161921, #146752, #191182, #96934, #92666, #128433, #143566, #94794, #193332, #209559, #13512, #12434, #80661, #112163, #111086, #47111, #127362, #195478, #113227, #61204, #78514, #194400, #27630, #10307, #179231, #144631, #62272, #46042, #178166, #76381, #126289, #212770, #43910, #125224, #108957, #93730, #29781, #174977, #424, #32971, #118547, #117483, #150999, #182399, #49234, #51359, #168302, #67564, #65437, #133707, #64406, #15632, #164053, #68638, #115353, #197590, #134762, #165102, #35081, #48184, #199713, #183474, #84911, #36151, #85982, #101153, #81719, #130550, #97995, #16693, #200770, #34028, #149929, #83839, #1498, #196541, #167238, #18827, #66497, #152058, #114296, #2567, #147801, #131588, #181344, #213819, #99047, #52421, #180294, #82779, #148851, #116409, #132636, #184529, #100102, #102231, #19898, #31917, #198642, #50290, #166162, #17749, #119615, #187739, #54550, #5759, #170424, #38299, #6839, #71838, #24161, #171498, #22011, #122856, #104377, #155257, #188817, #186672, #137947, #39367, #70765, #185600, #40451, #88121, #203969, #55615, #121770, #37231, #20949, #106553, #87046, #3628, #172580, #103302, #105464, #153119, #154191, #120697, #90264, #23089, #56689, #89204, #136879, #72917, #156332, #139022, #4690, #205046, #69706, #202905, #169364, #7917, #135810, #201833, #53478, #22328, #104692, #6082, #11164, #192044 ),
 ( #170743, #43707, #94592, #76179, #77241, #158506, #121017, #185904, #186983, #88442, #72153, #28501, #109825, #204275, #21259, #142286, #208296, #143358, #39679, #93525, #23405, #209354, #175836, #59928, #105788, #12235, #37540, #138262, #171814, #136124, #202138, #126083, #55931, #122086, #27427, #71078, #53797, #188048, #89518, #119929, #193128, #5005, #159567, #10106, #61001, #103619, #154504, #127157, #160634, #44777, #110883, #176889, #38615, #169672, #87365, #153434, #137196, #203219, #54864, #146552, #177963, #81518, #147596, #82572, #196340, #32768, #180090, #148659, #115150, #213615, #47984, #165966, #194196, #80454, #114099, #78309, #144433, #65241, #212570, #64209, #15429, #13311, #210435, #130350, #31715, #62076, #132446, #49031, #113026, #164898, #128233, #98847, #226, #96737, #161719, #162785, #97789, #50090, #131392, #163850, #46909, #197389, #45841, #181146, #66298, #33827, #16491, #198445, #116213, #182200, #99906, #111961, #29577, #79384, #95667, #145503, #211501, #63137, #129300, #195275, #179033, #30651, #14363, #170227, #21811, #4494, #67361, #87916, #19704, #120499, #134571, #100952, #53282, #200572, #85783, #185402, #202707, #133506, #169162, #70563, #201634, #52218, #18634, #118347, #117277, #105254, #121569, #167041, #51155, #54358, #136681, #184333, #17551, #149724, #37020, #103104, #153989, #151863, #35958, #102035, #168105, #104178, #186470, #137752, #1302, #187540, #3439, #5558, #203771, #183275, #71639, #69506, #38106, #55415, #39170, #83637, #199510, #152916, #20757, #34879, #84714, #150801, #2365, #68442, #135614, #119414, #86851, #175579, #74870, #42392, #190729, #108501, #22886, #174525, #75931, #173457, #44517, #89002, #59675, #122647, #23965, #172376, #43453, #138815, #189673, #157194, #91137, #41323, #208048, #109575, #156130, #26102, #57554, #92215, #188609, #171294, #25037, #107433, #90067, #123711, #76983, #7712, #73795, #40242, #158266, #209101, #125834, #142033, #205920, #8790, #140976, #60738, #106353, #206985, #27169, #72721, #139890, #204836, #58614, #124770, #191793, #9855, #93274, #159310, #155055, #10907, #192859, #6642, #143109, #56488, #126901, #211243, #14099, #178779, #195011, #213367, #146294, #148404, #97533, #30391, #32506, #112766, #64988, #98581, #129035, #80189, #113839, #161463, #78058, #164642, #96479, #212306, #63941, #130095, #144184, #45583, #16226, #111700, #110633, #82309, #210175, #196090, #177707, #46644, #79122, #214403, #163590, #197132, #47722, #95411, #15173, #66033, #179835, #29317, #31456, #176635, #61815, #13043, #132181, #145238, #28247, #198187, #127983, #81260, #62868, #162526, #147338, #94340, #131143, #48770, #114885, #180884, #160382, #11982, #193936, #50890, #53014, #49822, #1039, #149456, #54091, #84449, #152651, #102841, #5294, #20500, #33567, #185130, #119148, #70305, #21545, #71372, #168897, #67102, #115947, #83372, #150537, #120229, #167836, #135356, #69239, #201373, #181936, #36755, #86585, #51964, #137488, #99638, #4235, #133238, #117013, #183012, #136421, #17295, #68175, #35692, #184073, #134305, #202437, #186202, #34629, #37837, #2100, #103913, #199243, #165706, #118087, #200313, #100699, #101768, #169958, #166776, #18372, #19434, #87656, #153725, #85514, #151600, #3168, #41055, #123451, #26901, #6378, #23704, #141776, #104988, #72449 ),
 ( #125567, #159050, #156934, #207783, #91942, #93005, #108237, #158003, #171029, #204572, #174261, #175314, #59410, #25833, #22625, #189413, #191528, #56221, #73526, #43192, #109305, #190465, #38904, #10642, #205651, #9592, #106088, #75668, #42124, #89814, #203503, #121302, #8523, #74604, #76718, #57288, #155859, #172111, #139628, #55155, #187276, #88735, #154791, #138549, #7446, #122384, #188341, #39980, #107164, #173189, #24769, #90872, #140708, #206723, #58350, #124506, #80991, #162251, #127707, #192591, #193668, #29051, #78844, #32242, #47448, #210970, #27979, #146022, #212033, #147079, #46372, #97261, #30111, #213101, #179567, #63675, #112491, #15962, #44246, #144964, #178502, #142835, #208841, #129829, #62598, #128760, #79914, #77789, #60471, #194734, #96202, #126628, #196869, #113564, #177434, #14897, #110367, #163315, #64731, #161184, #11715, #12769, #13838, #114627, #195812, #31188, #111429, #130876, #176373, #48507, #180617, #98313, #164377, #94072, #160113, #143910, #209903, #61541, #45311, #95134, #52753, #53834, #20240, #118888, #197923, #67903, #3976, #149189, #166509, #86325, #152397, #68980, #131914, #70044, #84187, #184873, #198976, #165435, #117828, #50621, #150274, #35430, #36499, #49551, #19176, #135099, #51706, #116746, #83109, #182746, #181671, #169706, #185940, #17031, #115677, #201113, #200057, #168637, #33298, #34364, #102577, #37575, #85251, #136159, #101507, #66831, #99382, #132974, #100438, #18099, #103655, #202177, #1844, #764, #151338, #2908, #119965, #183819, #82045, #167577, #148139, #214141, #65767, #134047, #109051, #137232, #23442, #57035, #21296, #87401, #24511, #89553, #155603, #172934, #170776, #153467, #7188, #123202, #5040, #75419, #206470, #55967, #107987, #71116, #190217, #157749, #39714, #104728, #105822, #73260, #207539, #90621, #189163, #204310, #139365, #203253, #40801, #9347, #191275, #106909, #174014, #124258, #59159, #140458, #41876, #54897, #22365, #58097, #125317, #25585, #91696, #121050, #205396, #141531, #88477, #171848, #42942, #187017, #8271, #38650, #154537, #156678, #6117, #138294, #72186, #74354, #122119, #188084, #128525, #145792, #76473, #112253, #13604, #144727, #77542, #176132, #143664, #60224, #48273, #64498, #44001, #208591, #211797, #79678, #61299, #175069, #92758, #194494, #46137, #179331, #177188, #127460, #209658, #45075, #47210, #63433, #80754, #158803, #130640, #193432, #163081, #146843, #110120, #111185, #129585, #195572, #196632, #113324, #10400, #95961, #178266, #30952, #212862, #26656, #97026, #126383, #142584, #192343, #28803, #14662, #78606, #29877, #162015, #27731, #93826, #159867, #11470, #94888, #160940, #12533, #210739, #62362, #181432, #115441, #200852, #81810, #132725, #100188, #34117, #198730, #151089, #52501, #99140, #199803, #515, #51448, #131678, #114386, #182488, #50376, #33062, #66583, #19984, #165189, #16783, #197680, #117568, #152145, #68727, #84998, #148943, #166253, #17843, #3712, #49325, #116499, #118634, #15724, #82867, #147893, #83928, #150017, #134848, #1587, #184619, #36236, #32005, #2653, #135897, #180381, #86069, #213909, #183563, #67648, #133794, #35169, #101246, #102314, #167328, #69789, #18914, #168388, #201915, #98086, #164140, #65532, #71925, #171581, #56774, #104466, #21035, #107727, #39451, #89290, #6923, #73000, #87134 ),
 ( #106641, #140187, #23176, #38384, #40538, #157493, #122939, #54634, #188896, #53568, #4775, #153205, #57836, #172669, #120782, #24246, #119702, #70853, #136967, #123998, #88208, #156417, #90347, #9087, #8004, #37314, #74095, #206208, #189966, #25331, #75161, #41615, #202995, #185685, #186760, #154279, #173754, #155341, #139103, #205130, #91431, #103389, #141271, #169450, #55698, #170513, #22095, #5853, #138035, #204048, #121854, #187825, #105546, #11207, #193169, #127202, #77289, #29620, #79425, #192084, #78350, #93565, #144473, #10144, #207281, #61041, #143400, #208340, #159610, #113066, #59970, #43750, #76219, #210478, #30693, #161759, #178004, #27467, #44818, #110924, #96775, #142328, #209396, #145543, #108794, #126124, #26396, #176928, #109863, #13350, #28546, #211540, #63175, #125063, #95705, #14402, #58909, #179072, #174820, #62116, #94635, #160679, #12274, #128276, #129340, #194237, #162826, #45882, #112003, #195318, #46949, #80494, #191020, #42687, #92509, #158546, #175877, #114139, #203535, #135385, #185164, #102872, #168931, #180131, #81554, #71406, #147637, #146591, #55188, #31758, #36788, #213655, #82612, #115191, #121335, #202471, #21576, #53045, #131428, #136453, #38938, #212609, #3202, #16530, #65281, #98885, #187311, #197430, #49071, #163894, #20534, #105021, #103948, #120260, #181184, #201406, #69271, #171060, #15470, #32810, #87682, #48023, #164937, #97829, #119178, #148697, #169990, #86616, #153755, #5326, #64249, #186236, #22656, #130391, #196382, #152684, #4266, #70336, #54124, #37870, #137518, #191561, #124541, #126663, #75699, #8557, #10679, #90903, #43225, #76750, #107197, #206754, #91977, #139662, #56256, #142871, #74636, #190498, #42156, #108271, #122413, #23736, #208873, #89842, #88767, #60503, #188372, #174292, #155891, #24801, #57319, #192628, #141813, #175352, #58385, #73561, #207816, #44280, #158035, #7479, #9622, #154824, #40010, #106121, #93040, #123484, #109342, #59444, #110401, #125601, #72481, #26932, #159082, #176405, #6409, #138582, #204605, #172144, #205683, #189447, #41089, #173222, #25867, #156966, #140743, #113597, #94109, #179600, #147112, #30146, #115712, #160150, #130910, #193702, #95169, #29085, #114660, #209939, #46407, #13873, #162285, #112523, #64768, #180654, #12805, #31221, #128789, #97295, #45346, #196902, #143943, #161218, #213138, #214174, #32279, #48541, #61577, #79951, #164410, #78878, #178536, #98345, #146054, #28011, #63706, #195846, #47487, #127745, #177471, #15994, #145001, #11747, #148172, #111465, #129863, #211006, #96235, #62629, #82079, #81024, #65801, #212068, #194770, #14929, #131948, #163354, #197959, #49588, #77822, #133009, #66864, #185974, #1873, #70078, #20274, #137263, #152429, #165468, #102615, #184904, #202210, #153501, #203283, #86358, #199009, #33332, #796, #67933, #37607, #85286, #52785, #201147, #118924, #99414, #36528, #4008, #183850, #54930, #17064, #136192, #50654, #34395, #182777, #53864, #149221, #200086, #167609, #101540, #51735, #119997, #103688, #166542, #168670, #134078, #169737, #116780, #181702, #35462, #117858, #100467, #19207, #87433, #18130, #84219, #150307, #21326, #5071, #71146, #83143, #151372, #2941, #69013, #135130, #138324, #155633, #59190, #22400, #204340, #154571, #172964, #105853, #75448, #156712, #125345, #207569, #38681, #157779 ),
 ( #123230, #9377, #23477, #55998, #8303, #89584, #189195, #74387, #91728, #88509, #58130, #174043, #90651, #7218, #122149, #73292, #6147, #208623, #10432, #188117, #72217, #141561, #25616, #139395, #121082, #104760, #140488, #206499, #191308, #40832, #205428, #57066, #106941, #42976, #109086, #26688, #170809, #76504, #24543, #175101, #92790, #39748, #158835, #124289, #142615, #171880, #190248, #187049, #41906, #108017, #212896, #79707, #45108, #110150, #111218, #160971, #210771, #164168, #179360, #128556, #159897, #63464, #129618, #64528, #178299, #14691, #162044, #130673, #97057, #195605, #29906, #147922, #176163, #62391, #95991, #60257, #126414, #47240, #194521, #46169, #211827, #209690, #192377, #112283, #13634, #44032, #114413, #30982, #94922, #146875, #27763, #80786, #196661, #78635, #143698, #144760, #145822, #32031, #113355, #163110, #28834, #48302, #93859, #180413, #98117, #15754, #81838, #11504, #77575, #61334, #127493, #193464, #177221, #12561, #184648, #185712, #152174, #36268, #115471, #199836, #135926, #66609, #83958, #2685, #119734, #116527, #182517, #53599, #52531, #86102, #117601, #198759, #200885, #103420, #68757, #544, #134878, #213938, #165220, #99167, #3743, #34147, #102346, #118665, #169481, #168417, #197710, #20014, #69818, #201944, #37346, #21065, #87163, #16812, #65559, #33093, #100217, #131706, #183593, #85031, #18946, #151119, #49352, #181463, #82897, #1619, #148970, #132756, #50408, #166285, #17874, #150048, #67679, #133823, #51478, #35200, #101275, #167359, #189997, #25363, #138065, #24277, #39482, #90383, #170542, #153233, #6953, #23207, #154309, #105580, #58939, #5881, #204078, #22126, #156452, #191054, #107761, #124031, #187855, #205160, #73034, #42719, #88239, #171614, #91463, #54665, #71955, #186790, #56802, #55731, #173787, #188931, #157524, #9119, #70885, #41647, #174853, #4804, #125096, #120813, #8036, #89321, #122972, #139132, #155368, #75194, #40570, #108827, #140222, #106676, #141306, #172699, #207317, #26431, #74127, #206243, #57868, #136996, #203023, #38417, #104498, #121885, #45917, #112036, #126158, #27502, #14435, #93602, #92541, #212639, #192121, #128309, #159647, #28582, #78387, #12306, #176965, #129370, #179103, #77322, #178038, #193205, #29654, #109899, #158581, #160712, #94670, #11244, #44852, #64281, #143435, #209432, #175911, #95740, #130427, #46981, #63206, #127236, #144507, #210515, #196412, #61076, #110958, #30725, #208373, #62150, #43787, #194272, #161791, #113097, #13382, #96808, #162857, #10181, #195349, #114170, #76255, #48057, #60005, #79458, #145574, #211572, #80525, #146622, #180164, #142364, #69575, #18702, #166041, #168175, #33897, #134638, #19774, #50161, #149800, #34953, #52292, #15500, #83710, #31790, #67435, #199584, #51227, #65311, #181215, #85856, #32841, #97864, #151930, #131460, #133580, #98918, #182273, #298, #3505, #84785, #118421, #1374, #16563, #150873, #135686, #101024, #164971, #167115, #163925, #197461, #49104, #36026, #66369, #200643, #2437, #201711, #68511, #81587, #184407, #102104, #53353, #119487, #147672, #213689, #115225, #82646, #148730, #132517, #198515, #117351, #183349, #116282, #99976, #17625, #56566, #90141, #187612, #58691, #37098, #73878, #136752, #38178, #186549, #57629, #152992, #203845, #54430, #6716, #154066, #39240, #138894 ),
 ( #188687, #104250, #40323, #185474, #202779, #70641, #189746, #5631, #139971, #24038, #141054, #156209, #169238, #106428, #172451, #205993, #157275, #207061, #7785, #120572, #103177, #4568, #71712, #41398, #89077, #122725, #204913, #123788, #20826, #107508, #173537, #105332, #86924, #170296, #25111, #21884, #87993, #137825, #91214, #55491, #121645, #171369, #22962, #155134, #8864, #74943, #72794, #210254, #10985, #61892, #142110, #124839, #192940, #209180, #125912, #77059, #30466, #191871, #175656, #208123, #128054, #162599, #79203, #95491, #159387, #176707, #44592, #14174, #59752, #143189, #62945, #26179, #43531, #158338, #28320, #109654, #145319, #160455, #129114, #211321, #42465, #161537, #146366, #190805, #96552, #92294, #194009, #60820, #94416, #110707, #126981, #13124, #12063, #80267, #111776, #78131, #46727, #144261, #195090, #112839, #45658, #177782, #29398, #178855, #108575, #212380, #174603, #9932, #76007, #27244, #93350, #213439, #101844, #18448, #34701, #98659, #116024, #198259, #167914, #81335, #164714, #2175, #179910, #147414, #97608, #182009, #48846, #84525, #99714, #68251, #150614, #196160, #100770, #85588, #130168, #184146, #31533, #67182, #16303, #33640, #132252, #148478, #166852, #165786, #19511, #50967, #49902, #200387, #66110, #134384, #52035, #82388, #17369, #133318, #118161, #47801, #83453, #64022, #149533, #1119, #199320, #163665, #65062, #35770, #131218, #113914, #151676, #15248, #117089, #197206, #46, #32582, #114960, #183089, #180961, #5372, #4306, #171106, #89886, #38983, #86658, #105068, #3246, #168973, #102913, #188419, #120303, #138626, #88811, #73606, #6452, #201446, #22699, #154869, #204650, #155937, #69314, #72529, #20574, #135424, #152725, #103989, #172191, #55233, #56299, #122461, #40055, #53089, #106164, #23780, #71451, #119222, #36830, #7523, #70378, #186278, #54165, #185206, #37915, #136494, #202516, #170033, #21619, #87727, #153799, #137564, #203581, #121380, #187353, #214110, #196840, #50587, #66797, #197893, #149152, #102540, #49522, #33267, #65737, #67866, #83074, #100404, #116710, #132937, #85217, #18064, #20205, #183785, #182711, #118852, #198943, #151303, #184835, #731, #166472, #200020, #2873, #180588, #34329, #48480, #84152, #150239, #1808, #15933, #131885, #36465, #115644, #114597, #168603, #82016, #134013, #181639, #51672, #165402, #86292, #35393, #68943, #117793, #99351, #101470, #152363, #167541, #16998, #19140, #32211, #148107, #135065, #201078, #52719, #3940, #70008, #98285, #164344, #150040, #166275, #185706, #88232, #17866, #138059, #134872, #170535, #154301, #51469, #87156, #86092, #54659, #83949, #2678, #153227, #204072, #119727, #120807, #201937, #167351, #1611, #18938, #68750, #118657, #71949, #4797, #36261, #67670, #37340, #103414, #186784, #152168, #136990, #69812, #38410, #70877, #169474, #3737, #55724, #133814, #184642, #135918, #182509, #34139, #21059, #102339, #168411, #203017, #117593, #100208, #20008, #53593, #199828, #22120, #104492, #200879, #5875, #183584, #35192, #101267, #52524, #85023, #151112, #189990, #93595, #58932, #157517, #90377, #124024, #39475, #141300, #43778, #77315, #206235, #122965, #74120, #27495, #188924, #172693, #139126, #207309, #159639, #76248, #92535, #156446, #173781, #41641, #11236, #205153, #8030, #59998, #23200, #56796 ) ),
 .UNSPECIFIED., .T., .F., .F. ) 
 B_SPLINE_SURFACE_WITH_KNOTS ( ( 4, 3, 4 ),
 ( 4, 1, 1, 1, 1, 1, 1, 1, 1, 1, 1, 1, 1, 1, 1, 1, 1, 1, 1, 1, 1, 1, 1, 1, 1, 1, 1, 1, 1, 1, 1, 1, 1, 1, 1, 1, 1, 1, 1, 1, 1, 1, 1, 1, 1, 1, 1, 1, 1, 1, 1, 1, 1, 1, 1, 1, 1, 1, 1, 1, 1, 1, 1, 1, 1, 1, 1, 1, 1, 1, 1, 1, 1, 1, 1, 1, 1, 1, 1, 1, 1, 1, 1, 1, 1, 1, 1, 1, 1, 1, 1, 1, 1, 1, 1, 1, 1, 1, 1, 1, 1, 1, 1, 1, 1, 1, 1, 1, 1, 1, 1, 1, 1, 1, 1, 1, 1, 1, 1, 1, 1, 1, 1, 1, 1, 1, 1, 1, 1, 1, 1, 1, 1, 1, 1, 1, 1, 1, 1, 1, 1, 1, 1, 1, 1, 1, 1, 1, 1, 1, 1, 1, 1, 1, 1, 1, 1, 1, 1, 1, 1, 1, 1, 1, 1, 1, 1, 1, 1, 1, 1, 1, 1, 1, 1, 1, 1, 1, 1, 1, 1, 1, 1, 1, 1, 1, 1, 1, 1, 1, 1, 1, 1, 1, 1, 1, 1, 1, 1, 1, 1, 1, 1, 1, 1, 1, 1, 1, 1, 1, 1, 1, 1, 1, 1, 1, 1, 1, 1, 1, 1, 1, 1, 1, 1, 1, 1, 1, 1, 1, 1, 1, 1, 1, 1, 1, 1, 1, 1, 1, 1, 1, 1, 1, 1, 1, 1, 1, 1, 1, 1, 1, 1, 1, 1, 1, 1, 1, 1, 1, 1, 1, 1, 1, 1, 1, 1, 1, 1, 1, 1, 1, 1, 1, 1, 1, 1, 1, 1, 1, 1, 1, 1, 1, 1, 1, 1, 1, 1, 1, 1, 1, 1, 1, 1, 1, 1, 1, 1, 1, 1, 1, 1, 1, 1, 1, 1, 1, 1, 1, 1, 1, 1, 1, 1, 1, 1, 1, 1, 1, 1, 1, 1, 1, 1, 1, 1, 1, 1, 1, 1, 1, 1, 1, 1, 1, 1, 1, 1, 1, 1, 1, 1, 1, 1, 1, 1, 1, 1, 1, 1, 1, 1, 1, 1, 1, 1, 1, 1, 1, 1, 1, 1, 1, 1, 1, 1, 1, 1, 1, 1, 1, 1, 1, 1, 1, 1, 1, 1, 1, 1, 1, 1, 1, 4 ),
 ( 0.000000000000000000, 0.5000000000000000000, 1.000000000000000000 ),
 ( 0.000000000000000000, 0.002600137934918278840, 0.005208846947063642402, 0.007813284371963545236, 0.01041597565644012714, 0.01302123463190214131, 0.01562472912267370319, 0.01822934229245065652, 0.02083335053635077330, 0.02343730581734793095, 0.02604195799539401474, 0.02864545692284610826, 0.03125045498156164142, 0.03385385361191795006, 0.03645873261014952182, 0.03906243010681619693, 0.04166674480109257978, 0.04427107247243720900, 0.04687475664952634596, 0.04947964045798968619, 0.05208303702386667122, 0.05468803228817373241, 0.05729153353077973132, 0.05989618223844375006, 0.06250015876865079589, 0.06510412050499821135, 0.06770877833268285073, 0.07031227041168378045, 0.07291726700687002627, 0.07552066596874357218, 0.07812554330212571896, 0.08072923942118487295, 0.08333355289058355653, 0.08593787945419822938, 0.08854156225015286097, 0.09114644488045960113, 0.09374984019314609729, 0.09635483420994474246, 0.09895833431534489799, 0.1015629817166532611, 0.1041669571688737805, 0.1067709175595765864, 0.1093755742645453749, 0.1119790650618166516, 0.1145840604711090005, 0.1171874582687142119, 0.1197923343547293018, 0.1223960294069747767, 0.1250003415701952669, 0.1276046670722256471, 0.1302083485727723866, 0.1328132300777099817, 0.1354166241949035232, 0.1380216170238739992, 0.1406251160503516617, 0.1432297622036773077, 0.1458337366370238142, 0.1484376957407889386, 0.1510423513813509144, 0.1536458409560605698, 0.1562508352375901466, 0.1588542319300798034, 0.1614591068269417562, 0.1640628008713490293, 0.1666671117869774343, 0.1692714362859856492, 0.1718751165501164191, 0.1744799969878772505, 0.1770833899687347668, 0.1796883816679979429, 0.1822918796746371972, 0.1848965246383280081, 0.1875004981115827030, 0.1901044559872153150, 0.1927091106216977379, 0.1953125990329364348, 0.1979175922448092595, 0.2005209878913200294, 0.2031258616572126918, 0.2057295547527302204, 0.2083338644793258920, 0.2109381880338489224, 0.2135418671205281671, 0.2161467465492790951, 0.2187501384529311477, 0.2213551290805818306, 0.2239586261264417955, 0.2265632699588193688, 0.2291672425307399730, 0.2317711992370185270, 0.2343758529237242316, 0.2369793402305566954, 0.2395843324308542799, 0.2421877270904984059, 0.2447925997835804779, 0.2473962919891333490, 0.2500006005852301039, 0.2526049232537817546, 0.2552086012219486610, 0.2578134796998332035, 0.2604168705853860954, 0.2630218601994954719, 0.2656253563436123954, 0.2682299991029740149, 0.2708339708322964334, 0.2734379264279751531, 0.2760425792251849364, 0.2786460654866522724, 0.2812510567334335909, 0.2838544504653006673, 0.2864593221437078951, 0.2890630135181997962, 0.2916673210423081364, 0.2942716428833813125, 0.2968753197919519748, 0.2994801973770923054, 0.3020835873036303854, 0.3046885759622478540, 0.3072920712636373342, 0.3098967130082584398, 0.3125006839536987324, 0.3151046384975096371, 0.3177092904634842285, 0.3203127757386058927, 0.3229177660899096303, 0.3255211589530693228, 0.3281260296749167193, 0.3307297202772326306, 0.3333340267878420748, 0.3359383478599109463, 0.3385420237677806976, 0.3411469005182800607, 0.3437502895448679152, 0.3463552773060237788, 0.3489587718236830116, 0.3515634126118191150, 0.3541673828320756612, 0.3567713363827305639, 0.3593759875757128741, 0.3619794719234893932, 0.3645844614373360826, 0.3671878534908398217, 0.3697927233142242476, 0.3723964132032320795, 0.3750007187588132451, 0.3776050391203355505, 0.3802087140863810166, 0.3828135900603256703, 0.3854169782460106219, 0.3880219651677176973, 0.3906254589606275029, 0.3932300988505167960, 0.3958340684042725433, 0.3984380210204655492, 0.4010426714986830565, 0.4036461549780977487, 0.4062511437124918245, 0.4088545350153757196, 0.4114594039983773821, 0.4140630932329303349, 0.4166673978919369636, 0.4192717176013560643, 0.4218753916844373286, 0.4244802669398990425, 0.4270836543437129262, 0.4296886404839689866, 0.4322921336110964741, 0.4348967726609613837, 0.4375007416068860122, 0.4401046933472957945, 0.4427093431689624881, 0.4453128258389836835, 0.4479178138519160357, 0.4505212044632024293, 0.4531260726638874359, 0.4557297613028266636, 0.4583340651236982866, 0.4609383842394453867, 0.4635420574984087105, 0.4661469320934465421, 0.4687503187744080368, 0.4713553041911981989, 0.4739587967114984313, 0.4765634349795482838, 0.4791674033763006491, 0.4817713542995921694, 0.4843760035229108252, 0.4869794854424946973, 0.4895844727919445583, 0.4921878627706443576, 0.4947927302470669919, 0.4973964183492232127, 0.5000007213903868708, 0.5026050399708832384, 0.5052087124645624483, 0.5078135864572254077, 0.5104169724743423675, 0.5130219572256408123, 0.5156254491980594157, 0.5182300867424926016, 0.5208340546487225664, 0.5234380048135498509, 0.5260426534967141965, 0.5286461347248060383, 0.5312511214687432037, 0.5338545108738584899, 0.5364593776840630435, 0.5390630653082590928, 0.5416673676281316130, 0.5442716857317909662, 0.5468753575190105076, 0.5494802309673390006, 0.5520836163796108975, 0.5546886005233833128, 0.5572920920068584749, 0.5598967288858642810, 0.5625006963602153798, 0.5651046458252231286, 0.5677092940264200083, 0.5703127746219572858, 0.5729177608183441128, 0.5755211497088699169, 0.5781260159108934094, 0.5807297031159460721, 0.5833340047729366207, 0.5859383224581667937, 0.5885419935977430628, 0.5911468665597719996, 0.5937502514261915332, 0.5963552350203973340, 0.5989587260738620245, 0.6015633623456233536, 0.6041673294467342359, 0.6067712782705607655, 0.6093759260479724160, 0.6119794060698863225, 0.6145843917766802278, 0.6171877802116071399, 0.6197926458634805957, 0.6223963327082033814, 0.6250006337607152407, 0.6276049510859208480, 0.6302086216366651339, 0.6328134941704254279, 0.6354168785499811900, 0.6380218616525755726, 0.6406253523349600965, 0.6432299880576550777, 0.6458339548441623945, 0.6484379030854412473, 0.6510425504972472410, 0.6536460300044655281, 0.6562510152796211527, 0.6588544033179367654, 0.6614592684776883225, 0.6640629550208935195, 0.6666672555273263079, 0.6692715725509107427, 0.6718752425716313370, 0.6744801147351520143, 0.6770834986868305982, 0.6796884813557668714, 0.6822919717260003125, 0.6848966069578048543, 0.6875005734883452568, 0.6901045212057073108, 0.6927091683100871089, 0.6953126473615357517, 0.6979176322630067375, 0.7005210199636988655, 0.7031258846893556624, 0.7057295709898557812, 0.7083338710086078960, 0.7109381877889758838, 0.7135418573384794128, 0.7161467291897904985, 0.7187501127725786088, 0.7213550950658099703, 0.7239585851828231888, 0.7265632199819130888, 0.7291671863151253374, 0.7317711335672014705, 0.7343757804223364216, 0.7369792590769420615, 0.7395842436626837157, 0.7421876310847422831, 0.7447924954343322357, 0.7473961815509432283, 0.7500004811404139549, 0.7526047977359727748, 0.7552084668730677519, 0.7578133384702019359, 0.7604167217430886083, 0.7630217037185706985, 0.7656251936412983294, 0.7682298280658512724, 0.7708337942603785686, 0.7734377411058018792, 0.7760423877698768846, 0.7786458660865690495, 0.7812508504145402322, 0.7838542376169586046, 0.7864591016485131814, 0.7890627876400562180, 0.7916670868586475063, 0.7942714033278103214, 0.7968750721113085911, 0.7994799435123028930, 0.8020833265342820484, 0.8046883082499752815, 0.8072917980373575109, 0.8098964321455554005, 0.8125003982600473851, 0.8151043447574546352, 0.8177089912886614798, 0.8203124693263749156, 0.8229174534545398156, 0.8255208404963184643, 0.8281257042678743518, 0.8307293901931780411, 0.8333336890992975032, 0.8359380055004849153, 0.8385416739892034288, 0.8411465452521027508, 0.8437499280821748604, 0.8463549095960458679, 0.8489583993070312085, 0.8515630331570626099, 0.8541669992501779163, 0.8567709454582125295, 0.8593755919147509914, 0.8619790697324273276, 0.8645840537187589048, 0.8671874406589066275, 0.8697923042285079509, 0.8723959901464106714, 0.8750002887984731359, 0.8776046051901155165, 0.8802082734428797739, 0.8828131446257380111, 0.8854165273229123168, 0.8880215086929368340, 0.8906249983864840125, 0.8932296320365455955, 0.8958335981669537373, 0.8984375441442679078, 0.9010421905843485346, 0.9036456682409392815, 0.9062506521434200435, 0.9088540390409564074, 0.9114589024666573946, 0.9140625884360091824, 0.9166668868924389146, 0.9192712033329777377, 0.9218748714086243412, 0.9244797425695093773, 0.9270831251927963423, 0.9296881064769593195, 0.9322915962120889022, 0.9348962297203436966, 0.9375001959466012780, 0.9401041417521586174, 0.9427087882339971747, 0.9453122657876905643, 0.9479172496658602176, 0.9505206365780075606, 0.9531254999124115779, 0.9557291860198475764, 0.9583334843266348990, 0.9609378007344983041, 0.9635414689593263526, 0.9661463405142474148, 0.9687497214891268582, 0.9713547029754164841, 0.9739581985331400293, 0.9765628250748574768, 0.9791667834374845336, 0.9817707607320566021, 0.9843753697534296521, 0.9869788348889786400, 0.9895840831931937975, 0.9921867700316038263, 0.9947911815772807476, 0.9973998924267860611, 1.000000000000000000 ),
 .UNSPECIFIED. ) 
 GEOMETRIC_REPRESENTATION_ITEM ( )  RATIONAL_B_SPLINE_SURFACE ( (
 ( 1.000000000000000000, 1.000000000000000000, 1.000000000000000000, 1.000000000000000222, 0.9999999999999996669, 1.000000000000000222, 0.9999999999999997780, 1.000000000000000000, 0.9999999999999997780, 1.000000000000000444, 1.000000000000000000, 0.9999999999999997780, 1.000000000000000222, 1.000000000000000000, 0.9999999999999997780, 1.000000000000000222, 0.9999999999999996669, 1.000000000000000000, 1.000000000000000222, 1.000000000000000000, 1.000000000000000000, 1.000000000000000444, 0.9999999999999994449, 1.000000000000000444, 0.9999999999999996669, 1.000000000000000222, 1.000000000000000000, 1.000000000000000444, 1.000000000000000000, 0.9999999999999997780, 1.000000000000000000, 1.000000000000000222, 0.9999999999999997780, 0.9999999999999997780, 1.000000000000000444, 0.9999999999999997780, 1.000000000000000444, 1.000000000000000222, 0.9999999999999996669, 1.000000000000000222, 1.000000000000000000, 1.000000000000000444, 0.9999999999999997780, 1.000000000000000222, 1.000000000000000222, 1.000000000000000222, 0.9999999999999997780, 1.000000000000000000, 1.000000000000000000, 1.000000000000000000, 0.9999999999999994449, 1.000000000000000444, 0.9999999999999997780, 1.000000000000000444, 0.9999999999999997780, 1.000000000000000000, 1.000000000000000000, 0.9999999999999997780, 1.000000000000000444, 0.9999999999999996669, 1.000000000000000444, 0.9999999999999996669, 1.000000000000000222, 0.9999999999999994449, 1.000000000000000222, 1.000000000000000000, 1.000000000000000000, 1.000000000000000000, 1.000000000000000000, 1.000000000000000222, 1.000000000000000000, 1.000000000000000222, 0.9999999999999996669, 1.000000000000000222, 1.000000000000000000, 1.000000000000000444, 1.000000000000000000, 1.000000000000000000, 0.9999999999999997780, 1.000000000000000222, 0.9999999999999997780, 0.9999999999999997780, 1.000000000000000444, 1.000000000000000000, 1.000000000000000222, 0.9999999999999996669, 1.000000000000000444, 0.9999999999999997780, 1.000000000000000222, 0.9999999999999997780, 1.000000000000000222, 1.000000000000000000, 1.000000000000000000, 1.000000000000000000, 1.000000000000000000, 1.000000000000000222, 1.000000000000000222, 0.9999999999999997780, 1.000000000000000222, 1.000000000000000000, 1.000000000000000222, 0.9999999999999997780, 1.000000000000000222, 1.000000000000000000, 1.000000000000000000, 0.9999999999999997780, 1.000000000000000000, 1.000000000000000000, 0.9999999999999997780, 1.000000000000000222, 0.9999999999999997780, 1.000000000000000222, 0.9999999999999997780, 1.000000000000000444, 1.000000000000000000, 0.9999999999999996669, 1.000000000000000444, 1.000000000000000000, 0.9999999999999997780, 1.000000000000000000, 0.9999999999999996669, 1.000000000000000000, 1.000000000000000222, 0.9999999999999996669, 1.000000000000000222, 0.9999999999999997780, 1.000000000000000000, 1.000000000000000222, 0.9999999999999997780, 1.000000000000000222, 0.9999999999999997780, 1.000000000000000222, 1.000000000000000000, 1.000000000000000000, 1.000000000000000000, 0.9999999999999997780, 1.000000000000000222, 0.9999999999999997780, 1.000000000000000222, 1.000000000000000000, 1.000000000000000000, 1.000000000000000000, 1.000000000000000000, 1.000000000000000444, 0.9999999999999997780, 1.000000000000000444, 0.9999999999999997780, 1.000000000000000222, 1.000000000000000000, 1.000000000000000000, 1.000000000000000000, 1.000000000000000000, 0.9999999999999997780, 1.000000000000000000, 1.000000000000000222, 0.9999999999999997780, 1.000000000000000222, 1.000000000000000000, 1.000000000000000000, 1.000000000000000222, 0.9999999999999997780, 1.000000000000000222, 0.9999999999999996669, 1.000000000000000444, 0.9999999999999994449, 1.000000000000000444, 0.9999999999999997780, 0.9999999999999997780, 1.000000000000000000, 1.000000000000000000, 1.000000000000000222, 1.000000000000000000, 1.000000000000000000, 1.000000000000000000, 1.000000000000000000, 1.000000000000000222, 1.000000000000000444, 0.9999999999999997780, 1.000000000000000222, 1.000000000000000000, 0.9999999999999996669, 1.000000000000000222, 1.000000000000000222, 1.000000000000000222, 1.000000000000000222, 1.000000000000000000, 1.000000000000000000, 1.000000000000000222, 1.000000000000000000, 1.000000000000000222, 1.000000000000000000, 1.000000000000000000, 1.000000000000000000, 1.000000000000000222, 0.9999999999999997780, 1.000000000000000000, 1.000000000000000222, 1.000000000000000000, 1.000000000000000222, 1.000000000000000000, 0.9999999999999997780, 1.000000000000000444, 1.000000000000000000, 0.9999999999999996669, 1.000000000000000222, 0.9999999999999997780, 1.000000000000000222, 1.000000000000000000, 1.000000000000000000, 1.000000000000000444, 0.9999999999999996669, 1.000000000000000000, 0.9999999999999997780, 1.000000000000000000, 0.9999999999999997780, 0.9999999999999997780, 1.000000000000000000, 1.000000000000000000, 1.000000000000000000, 0.9999999999999997780, 1.000000000000000000, 1.000000000000000222, 1.000000000000000222, 1.000000000000000000, 0.9999999999999997780, 1.000000000000000222, 1.000000000000000000, 1.000000000000000000, 1.000000000000000222, 1.000000000000000222, 1.000000000000000222, 1.000000000000000000, 0.9999999999999997780, 1.000000000000000444, 0.9999999999999997780, 1.000000000000000444, 0.9999999999999997780, 1.000000000000000000, 1.000000000000000222, 0.9999999999999997780, 1.000000000000000222, 0.9999999999999997780, 1.000000000000000222, 0.9999999999999997780, 1.000000000000000222, 0.9999999999999996669, 1.000000000000000222, 0.9999999999999997780, 1.000000000000000444, 1.000000000000000000, 1.000000000000000000, 0.9999999999999997780, 1.000000000000000222, 1.000000000000000000, 0.9999999999999996669, 1.000000000000000222, 0.9999999999999997780, 1.000000000000000000, 1.000000000000000222, 1.000000000000000000, 1.000000000000000222, 0.9999999999999996669, 1.000000000000000444, 0.9999999999999996669, 1.000000000000000000, 1.000000000000000000, 1.000000000000000000, 0.9999999999999997780, 1.000000000000000444, 1.000000000000000000, 1.000000000000000000, 1.000000000000000000, 1.000000000000000000, 0.9999999999999997780, 1.000000000000000222, 1.000000000000000222, 1.000000000000000222, 1.000000000000000000, 1.000000000000000222, 1.000000000000000000, 0.9999999999999997780, 1.000000000000000444, 1.000000000000000000, 0.9999999999999997780, 1.000000000000000222, 0.9999999999999996669, 1.000000000000000222, 1.000000000000000000, 1.000000000000000444, 1.000000000000000222, 0.9999999999999996669, 1.000000000000000222, 0.9999999999999997780, 1.000000000000000222, 1.000000000000000222, 0.9999999999999997780, 1.000000000000000222, 1.000000000000000000, 1.000000000000000222, 1.000000000000000222, 0.9999999999999997780, 1.000000000000000444, 0.9999999999999996669, 1.000000000000000222, 1.000000000000000222, 1.000000000000000000, 1.000000000000000000, 1.000000000000000000, 1.000000000000000222, 1.000000000000000000, 1.000000000000000000, 1.000000000000000222, 0.9999999999999996669, 1.000000000000000444, 1.000000000000000222, 0.9999999999999997780, 1.000000000000000222, 0.9999999999999997780, 1.000000000000000444, 0.9999999999999996669, 1.000000000000000666, 0.9999999999999994449, 1.000000000000000222, 0.9999999999999997780, 1.000000000000000444, 1.000000000000000000, 1.000000000000000222, 1.000000000000000222, 1.000000000000000000, 0.9999999999999997780, 0.9999999999999997780, 1.000000000000000444, 1.000000000000000000, 1.000000000000000000, 1.000000000000000000, 0.9999999999999997780, 1.000000000000000222, 1.000000000000000222, 0.9999999999999997780, 1.000000000000000222, 1.000000000000000000, 1.000000000000000444, 0.9999999999999996669, 1.000000000000000444, 0.9999999999999997780, 1.000000000000000000, 0.9999999999999997780, 1.000000000000000444, 0.9999999999999996669, 1.000000000000000444, 1.000000000000000000, 1.000000000000000000, 1.000000000000000000, 0.9999999999999997780, 1.000000000000000444, 1.000000000000000222, 0.9999999999999997780, 1.000000000000000444, 1.000000000000000000, 0.9999999999999996669, 1.000000000000000444, 1.000000000000000000, 1.000000000000000000, 1.000000000000000000, 0.9999999999999997780, 1.000000000000000222, 0.9999999999999997780, 1.000000000000000000, 1.000000000000000222, 0.9999999999999997780, 1.000000000000000000, 1.000000000000000000, 0.9999999999999997780, 1.000000000000000444, 0.9999999999999997780, 1.000000000000000444, 0.9999999999999994449, 1.000000000000000444, 0.9999999999999997780, 1.000000000000000444, 0.9999999999999997780, 1.000000000000000000, 0.9999999999999997780, 1.000000000000000222, 1.000000000000000222, 1.000000000000000000, 1.000000000000000000),
 ( 0.3333333333333333703, 0.3333333333333333703, 0.3333333333333333703, 0.3333333333333335369, 0.3333333333333333148, 0.3333333333333333703, 0.3333333333333333703, 0.3333333333333333148, 0.3333333333333333148, 0.3333333333333334259, 0.3333333333333333703, 0.3333333333333333148, 0.3333333333333334259, 0.3333333333333333148, 0.3333333333333334259, 0.3333333333333333148, 0.3333333333333333703, 0.3333333333333333148, 0.3333333333333334814, 0.3333333333333333148, 0.3333333333333334814, 0.3333333333333334814, 0.3333333333333333148, 0.3333333333333334259, 0.3333333333333333148, 0.3333333333333333703, 0.3333333333333333148, 0.3333333333333334814, 0.3333333333333333703, 0.3333333333333333703, 0.3333333333333333703, 0.3333333333333334259, 0.3333333333333333148, 0.3333333333333333148, 0.3333333333333334259, 0.3333333333333333703, 0.3333333333333334259, 0.3333333333333334259, 0.3333333333333332038, 0.3333333333333334814, 0.3333333333333333703, 0.3333333333333334814, 0.3333333333333332593, 0.3333333333333334259, 0.3333333333333333703, 0.3333333333333334259, 0.3333333333333333148, 0.3333333333333333703, 0.3333333333333334259, 0.3333333333333333148, 0.3333333333333332038, 0.3333333333333335369, 0.3333333333333332593, 0.3333333333333334814, 0.3333333333333333148, 0.3333333333333333703, 0.3333333333333334259, 0.3333333333333333703, 0.3333333333333334814, 0.3333333333333333703, 0.3333333333333334259, 0.3333333333333333148, 0.3333333333333334814, 0.3333333333333332038, 0.3333333333333334259, 0.3333333333333333148, 0.3333333333333333703, 0.3333333333333333703, 0.3333333333333334259, 0.3333333333333333148, 0.3333333333333333703, 0.3333333333333334259, 0.3333333333333333148, 0.3333333333333333703, 0.3333333333333333703, 0.3333333333333335369, 0.3333333333333333148, 0.3333333333333333703, 0.3333333333333333703, 0.3333333333333333703, 0.3333333333333333148, 0.3333333333333333703, 0.3333333333333334814, 0.3333333333333333148, 0.3333333333333334814, 0.3333333333333333703, 0.3333333333333334259, 0.3333333333333333148, 0.3333333333333334259, 0.3333333333333333148, 0.3333333333333334259, 0.3333333333333333148, 0.3333333333333333703, 0.3333333333333333703, 0.3333333333333333703, 0.3333333333333334259, 0.3333333333333334259, 0.3333333333333332593, 0.3333333333333334259, 0.3333333333333333703, 0.3333333333333334259, 0.3333333333333333148, 0.3333333333333334259, 0.3333333333333333703, 0.3333333333333333703, 0.3333333333333333148, 0.3333333333333334259, 0.3333333333333333703, 0.3333333333333333148, 0.3333333333333334259, 0.3333333333333332038, 0.3333333333333334814, 0.3333333333333333148, 0.3333333333333335369, 0.3333333333333334259, 0.3333333333333332038, 0.3333333333333334814, 0.3333333333333333703, 0.3333333333333332593, 0.3333333333333333703, 0.3333333333333332593, 0.3333333333333333703, 0.3333333333333334814, 0.3333333333333333148, 0.3333333333333334814, 0.3333333333333333148, 0.3333333333333334259, 0.3333333333333334259, 0.3333333333333333148, 0.3333333333333334259, 0.3333333333333333148, 0.3333333333333334259, 0.3333333333333333703, 0.3333333333333333703, 0.3333333333333334259, 0.3333333333333332593, 0.3333333333333334814, 0.3333333333333333148, 0.3333333333333333703, 0.3333333333333333703, 0.3333333333333333703, 0.3333333333333334259, 0.3333333333333334259, 0.3333333333333334814, 0.3333333333333333703, 0.3333333333333334259, 0.3333333333333333703, 0.3333333333333333703, 0.3333333333333333148, 0.3333333333333333703, 0.3333333333333334259, 0.3333333333333333148, 0.3333333333333333148, 0.3333333333333333148, 0.3333333333333334259, 0.3333333333333333148, 0.3333333333333334814, 0.3333333333333333148, 0.3333333333333334259, 0.3333333333333334259, 0.3333333333333333148, 0.3333333333333334814, 0.3333333333333333148, 0.3333333333333334814, 0.3333333333333332593, 0.3333333333333335369, 0.3333333333333333148, 0.3333333333333333703, 0.3333333333333333703, 0.3333333333333334259, 0.3333333333333333703, 0.3333333333333333703, 0.3333333333333333148, 0.3333333333333333703, 0.3333333333333332593, 0.3333333333333335369, 0.3333333333333334259, 0.3333333333333333703, 0.3333333333333334259, 0.3333333333333334259, 0.3333333333333332038, 0.3333333333333334814, 0.3333333333333333703, 0.3333333333333334259, 0.3333333333333333703, 0.3333333333333333703, 0.3333333333333333148, 0.3333333333333334814, 0.3333333333333333148, 0.3333333333333334814, 0.3333333333333334259, 0.3333333333333333148, 0.3333333333333333703, 0.3333333333333333703, 0.3333333333333333703, 0.3333333333333333703, 0.3333333333333334259, 0.3333333333333333148, 0.3333333333333334814, 0.3333333333333333148, 0.3333333333333333703, 0.3333333333333334814, 0.3333333333333332593, 0.3333333333333333148, 0.3333333333333334259, 0.3333333333333332593, 0.3333333333333335369, 0.3333333333333333703, 0.3333333333333334259, 0.3333333333333335369, 0.3333333333333333148, 0.3333333333333333703, 0.3333333333333333148, 0.3333333333333333703, 0.3333333333333333148, 0.3333333333333333148, 0.3333333333333333703, 0.3333333333333333703, 0.3333333333333333703, 0.3333333333333333148, 0.3333333333333333703, 0.3333333333333333703, 0.3333333333333334259, 0.3333333333333333703, 0.3333333333333333148, 0.3333333333333333703, 0.3333333333333333703, 0.3333333333333333703, 0.3333333333333334259, 0.3333333333333334259, 0.3333333333333334814, 0.3333333333333332593, 0.3333333333333334259, 0.3333333333333334259, 0.3333333333333333148, 0.3333333333333334259, 0.3333333333333333703, 0.3333333333333333148, 0.3333333333333334814, 0.3333333333333333703, 0.3333333333333334259, 0.3333333333333332593, 0.3333333333333334259, 0.3333333333333332593, 0.3333333333333334814, 0.3333333333333332593, 0.3333333333333334259, 0.3333333333333333148, 0.3333333333333334259, 0.3333333333333333703, 0.3333333333333334259, 0.3333333333333333703, 0.3333333333333333703, 0.3333333333333333703, 0.3333333333333333148, 0.3333333333333334259, 0.3333333333333333703, 0.3333333333333333148, 0.3333333333333334259, 0.3333333333333333148, 0.3333333333333333703, 0.3333333333333333148, 0.3333333333333334814, 0.3333333333333332593, 0.3333333333333333703, 0.3333333333333333703, 0.3333333333333334259, 0.3333333333333332593, 0.3333333333333335369, 0.3333333333333333703, 0.3333333333333333703, 0.3333333333333333703, 0.3333333333333333148, 0.3333333333333333148, 0.3333333333333334259, 0.3333333333333334814, 0.3333333333333334259, 0.3333333333333333703, 0.3333333333333334259, 0.3333333333333334259, 0.3333333333333333703, 0.3333333333333334814, 0.3333333333333333148, 0.3333333333333333148, 0.3333333333333334259, 0.3333333333333332038, 0.3333333333333334814, 0.3333333333333333148, 0.3333333333333335369, 0.3333333333333334259, 0.3333333333333333148, 0.3333333333333334814, 0.3333333333333333703, 0.3333333333333333703, 0.3333333333333334259, 0.3333333333333333703, 0.3333333333333334259, 0.3333333333333333703, 0.3333333333333334259, 0.3333333333333333148, 0.3333333333333333703, 0.3333333333333335369, 0.3333333333333332038, 0.3333333333333334814, 0.3333333333333333703, 0.3333333333333333148, 0.3333333333333334259, 0.3333333333333333703, 0.3333333333333333148, 0.3333333333333334259, 0.3333333333333333703, 0.3333333333333334259, 0.3333333333333332593, 0.3333333333333335369, 0.3333333333333334814, 0.3333333333333333148, 0.3333333333333334259, 0.3333333333333333148, 0.3333333333333335369, 0.3333333333333332593, 0.3333333333333335924, 0.3333333333333332593, 0.3333333333333333703, 0.3333333333333333703, 0.3333333333333334814, 0.3333333333333333703, 0.3333333333333334814, 0.3333333333333333703, 0.3333333333333334259, 0.3333333333333332593, 0.3333333333333334259, 0.3333333333333335369, 0.3333333333333333148, 0.3333333333333334814, 0.3333333333333333148, 0.3333333333333333703, 0.3333333333333334259, 0.3333333333333334259, 0.3333333333333332593, 0.3333333333333334259, 0.3333333333333333148, 0.3333333333333335369, 0.3333333333333332593, 0.3333333333333335369, 0.3333333333333333148, 0.3333333333333333148, 0.3333333333333333703, 0.3333333333333334814, 0.3333333333333333148, 0.3333333333333334259, 0.3333333333333333148, 0.3333333333333334259, 0.3333333333333333703, 0.3333333333333333148, 0.3333333333333334259, 0.3333333333333334814, 0.3333333333333333148, 0.3333333333333334814, 0.3333333333333333703, 0.3333333333333332593, 0.3333333333333334259, 0.3333333333333333703, 0.3333333333333334259, 0.3333333333333333703, 0.3333333333333333148, 0.3333333333333334259, 0.3333333333333333703, 0.3333333333333333148, 0.3333333333333334259, 0.3333333333333333148, 0.3333333333333333148, 0.3333333333333333703, 0.3333333333333333703, 0.3333333333333334259, 0.3333333333333333148, 0.3333333333333334259, 0.3333333333333332593, 0.3333333333333334259, 0.3333333333333333703, 0.3333333333333334259, 0.3333333333333333703, 0.3333333333333333703, 0.3333333333333333148, 0.3333333333333334814, 0.3333333333333334259, 0.3333333333333333703, 0.3333333333333333703),
 ( 0.3333333333333333703, 0.3333333333333333703, 0.3333333333333333703, 0.3333333333333335369, 0.3333333333333333148, 0.3333333333333333703, 0.3333333333333333703, 0.3333333333333333148, 0.3333333333333333148, 0.3333333333333334259, 0.3333333333333333703, 0.3333333333333333148, 0.3333333333333334259, 0.3333333333333333148, 0.3333333333333334259, 0.3333333333333333148, 0.3333333333333333703, 0.3333333333333333148, 0.3333333333333334814, 0.3333333333333333148, 0.3333333333333334814, 0.3333333333333334814, 0.3333333333333333148, 0.3333333333333334259, 0.3333333333333333148, 0.3333333333333333703, 0.3333333333333333148, 0.3333333333333334814, 0.3333333333333333703, 0.3333333333333333703, 0.3333333333333333703, 0.3333333333333334259, 0.3333333333333333148, 0.3333333333333333148, 0.3333333333333334259, 0.3333333333333333703, 0.3333333333333334259, 0.3333333333333334259, 0.3333333333333332038, 0.3333333333333334814, 0.3333333333333333703, 0.3333333333333334814, 0.3333333333333332593, 0.3333333333333334259, 0.3333333333333333703, 0.3333333333333334259, 0.3333333333333333148, 0.3333333333333333703, 0.3333333333333334259, 0.3333333333333333148, 0.3333333333333332038, 0.3333333333333335369, 0.3333333333333332593, 0.3333333333333334814, 0.3333333333333333148, 0.3333333333333333703, 0.3333333333333334259, 0.3333333333333333703, 0.3333333333333334814, 0.3333333333333333703, 0.3333333333333334259, 0.3333333333333333148, 0.3333333333333334814, 0.3333333333333332038, 0.3333333333333334259, 0.3333333333333333148, 0.3333333333333333703, 0.3333333333333333703, 0.3333333333333334259, 0.3333333333333333148, 0.3333333333333333703, 0.3333333333333334259, 0.3333333333333333148, 0.3333333333333333703, 0.3333333333333333703, 0.3333333333333335369, 0.3333333333333333148, 0.3333333333333333703, 0.3333333333333333703, 0.3333333333333333703, 0.3333333333333333148, 0.3333333333333333703, 0.3333333333333334814, 0.3333333333333333148, 0.3333333333333334814, 0.3333333333333333703, 0.3333333333333334259, 0.3333333333333333148, 0.3333333333333334259, 0.3333333333333333148, 0.3333333333333334259, 0.3333333333333333148, 0.3333333333333333703, 0.3333333333333333703, 0.3333333333333333703, 0.3333333333333334259, 0.3333333333333334259, 0.3333333333333332593, 0.3333333333333334259, 0.3333333333333333703, 0.3333333333333334259, 0.3333333333333333148, 0.3333333333333334259, 0.3333333333333333703, 0.3333333333333333703, 0.3333333333333333148, 0.3333333333333334259, 0.3333333333333333703, 0.3333333333333333148, 0.3333333333333334259, 0.3333333333333332038, 0.3333333333333334814, 0.3333333333333333148, 0.3333333333333335369, 0.3333333333333334259, 0.3333333333333332038, 0.3333333333333334814, 0.3333333333333333703, 0.3333333333333332593, 0.3333333333333333703, 0.3333333333333332593, 0.3333333333333333703, 0.3333333333333334814, 0.3333333333333333148, 0.3333333333333334814, 0.3333333333333333148, 0.3333333333333334259, 0.3333333333333334259, 0.3333333333333333148, 0.3333333333333334259, 0.3333333333333333148, 0.3333333333333334259, 0.3333333333333333703, 0.3333333333333333703, 0.3333333333333334259, 0.3333333333333332593, 0.3333333333333334814, 0.3333333333333333148, 0.3333333333333333703, 0.3333333333333333703, 0.3333333333333333703, 0.3333333333333334259, 0.3333333333333334259, 0.3333333333333334814, 0.3333333333333333703, 0.3333333333333334259, 0.3333333333333333703, 0.3333333333333333703, 0.3333333333333333148, 0.3333333333333333703, 0.3333333333333334259, 0.3333333333333333148, 0.3333333333333333148, 0.3333333333333333148, 0.3333333333333334259, 0.3333333333333333148, 0.3333333333333334814, 0.3333333333333333148, 0.3333333333333334259, 0.3333333333333334259, 0.3333333333333333148, 0.3333333333333334814, 0.3333333333333333148, 0.3333333333333334814, 0.3333333333333332593, 0.3333333333333335369, 0.3333333333333333148, 0.3333333333333333703, 0.3333333333333333703, 0.3333333333333334259, 0.3333333333333333703, 0.3333333333333333703, 0.3333333333333333148, 0.3333333333333333703, 0.3333333333333332593, 0.3333333333333335369, 0.3333333333333334259, 0.3333333333333333703, 0.3333333333333334259, 0.3333333333333334259, 0.3333333333333332038, 0.3333333333333334814, 0.3333333333333333703, 0.3333333333333334259, 0.3333333333333333703, 0.3333333333333333703, 0.3333333333333333148, 0.3333333333333334814, 0.3333333333333333148, 0.3333333333333334814, 0.3333333333333334259, 0.3333333333333333148, 0.3333333333333333703, 0.3333333333333333703, 0.3333333333333333703, 0.3333333333333333703, 0.3333333333333334259, 0.3333333333333333148, 0.3333333333333334814, 0.3333333333333333148, 0.3333333333333333703, 0.3333333333333334814, 0.3333333333333332593, 0.3333333333333333148, 0.3333333333333334259, 0.3333333333333332593, 0.3333333333333335369, 0.3333333333333333703, 0.3333333333333334259, 0.3333333333333335369, 0.3333333333333333148, 0.3333333333333333703, 0.3333333333333333148, 0.3333333333333333703, 0.3333333333333333148, 0.3333333333333333148, 0.3333333333333333703, 0.3333333333333333703, 0.3333333333333333703, 0.3333333333333333148, 0.3333333333333333703, 0.3333333333333333703, 0.3333333333333334259, 0.3333333333333333703, 0.3333333333333333148, 0.3333333333333333703, 0.3333333333333333703, 0.3333333333333333703, 0.3333333333333334259, 0.3333333333333334259, 0.3333333333333334814, 0.3333333333333332593, 0.3333333333333334259, 0.3333333333333334259, 0.3333333333333333148, 0.3333333333333334259, 0.3333333333333333703, 0.3333333333333333148, 0.3333333333333334814, 0.3333333333333333703, 0.3333333333333334259, 0.3333333333333332593, 0.3333333333333334259, 0.3333333333333332593, 0.3333333333333334814, 0.3333333333333332593, 0.3333333333333334259, 0.3333333333333333148, 0.3333333333333334259, 0.3333333333333333703, 0.3333333333333334259, 0.3333333333333333703, 0.3333333333333333703, 0.3333333333333333703, 0.3333333333333333148, 0.3333333333333334259, 0.3333333333333333703, 0.3333333333333333148, 0.3333333333333334259, 0.3333333333333333148, 0.3333333333333333703, 0.3333333333333333148, 0.3333333333333334814, 0.3333333333333332593, 0.3333333333333333703, 0.3333333333333333703, 0.3333333333333334259, 0.3333333333333332593, 0.3333333333333335369, 0.3333333333333333703, 0.3333333333333333703, 0.3333333333333333703, 0.3333333333333333148, 0.3333333333333333148, 0.3333333333333334259, 0.3333333333333334814, 0.3333333333333334259, 0.3333333333333333703, 0.3333333333333334259, 0.3333333333333334259, 0.3333333333333333703, 0.3333333333333334814, 0.3333333333333333148, 0.3333333333333333148, 0.3333333333333334259, 0.3333333333333332038, 0.3333333333333334814, 0.3333333333333333148, 0.3333333333333335369, 0.3333333333333334259, 0.3333333333333333148, 0.3333333333333334814, 0.3333333333333333703, 0.3333333333333333703, 0.3333333333333334259, 0.3333333333333333703, 0.3333333333333334259, 0.3333333333333333703, 0.3333333333333334259, 0.3333333333333333148, 0.3333333333333333703, 0.3333333333333335369, 0.3333333333333332038, 0.3333333333333334814, 0.3333333333333333703, 0.3333333333333333148, 0.3333333333333334259, 0.3333333333333333703, 0.3333333333333333148, 0.3333333333333334259, 0.3333333333333333703, 0.3333333333333334259, 0.3333333333333332593, 0.3333333333333335369, 0.3333333333333334814, 0.3333333333333333148, 0.3333333333333334259, 0.3333333333333333148, 0.3333333333333335369, 0.3333333333333332593, 0.3333333333333335924, 0.3333333333333332593, 0.3333333333333333703, 0.3333333333333333703, 0.3333333333333334814, 0.3333333333333333703, 0.3333333333333334814, 0.3333333333333333703, 0.3333333333333334259, 0.3333333333333332593, 0.3333333333333334259, 0.3333333333333335369, 0.3333333333333333148, 0.3333333333333334814, 0.3333333333333333148, 0.3333333333333333703, 0.3333333333333334259, 0.3333333333333334259, 0.3333333333333332593, 0.3333333333333334259, 0.3333333333333333148, 0.3333333333333335369, 0.3333333333333332593, 0.3333333333333335369, 0.3333333333333333148, 0.3333333333333333148, 0.3333333333333333703, 0.3333333333333334814, 0.3333333333333333148, 0.3333333333333334259, 0.3333333333333333148, 0.3333333333333334259, 0.3333333333333333703, 0.3333333333333333148, 0.3333333333333334259, 0.3333333333333334814, 0.3333333333333333148, 0.3333333333333334814, 0.3333333333333333703, 0.3333333333333332593, 0.3333333333333334259, 0.3333333333333333703, 0.3333333333333334259, 0.3333333333333333703, 0.3333333333333333148, 0.3333333333333334259, 0.3333333333333333703, 0.3333333333333333148, 0.3333333333333334259, 0.3333333333333333148, 0.3333333333333333148, 0.3333333333333333703, 0.3333333333333333703, 0.3333333333333334259, 0.3333333333333333148, 0.3333333333333334259, 0.3333333333333332593, 0.3333333333333334259, 0.3333333333333333703, 0.3333333333333334259, 0.3333333333333333703, 0.3333333333333333703, 0.3333333333333333148, 0.3333333333333334814, 0.3333333333333334259, 0.3333333333333333703, 0.3333333333333333703),
 ( 1.000000000000000000, 1.000000000000000000, 1.000000000000000000, 1.000000000000000222, 0.9999999999999996669, 1.000000000000000222, 0.9999999999999997780, 1.000000000000000000, 0.9999999999999997780, 1.000000000000000444, 1.000000000000000000, 0.9999999999999997780, 1.000000000000000222, 1.000000000000000000, 0.9999999999999997780, 1.000000000000000222, 0.9999999999999996669, 1.000000000000000000, 1.000000000000000222, 1.000000000000000000, 1.000000000000000000, 1.000000000000000444, 0.9999999999999994449, 1.000000000000000444, 0.9999999999999996669, 1.000000000000000222, 1.000000000000000000, 1.000000000000000444, 1.000000000000000000, 0.9999999999999997780, 1.000000000000000000, 1.000000000000000222, 0.9999999999999997780, 0.9999999999999997780, 1.000000000000000444, 0.9999999999999997780, 1.000000000000000444, 1.000000000000000222, 0.9999999999999996669, 1.000000000000000222, 1.000000000000000000, 1.000000000000000444, 0.9999999999999997780, 1.000000000000000222, 1.000000000000000222, 1.000000000000000222, 0.9999999999999997780, 1.000000000000000000, 1.000000000000000000, 1.000000000000000000, 0.9999999999999994449, 1.000000000000000444, 0.9999999999999997780, 1.000000000000000444, 0.9999999999999997780, 1.000000000000000000, 1.000000000000000000, 0.9999999999999997780, 1.000000000000000444, 0.9999999999999996669, 1.000000000000000444, 0.9999999999999996669, 1.000000000000000222, 0.9999999999999994449, 1.000000000000000222, 1.000000000000000000, 1.000000000000000000, 1.000000000000000000, 1.000000000000000000, 1.000000000000000222, 1.000000000000000000, 1.000000000000000222, 0.9999999999999996669, 1.000000000000000222, 1.000000000000000000, 1.000000000000000444, 1.000000000000000000, 1.000000000000000000, 0.9999999999999997780, 1.000000000000000222, 0.9999999999999997780, 0.9999999999999997780, 1.000000000000000444, 1.000000000000000000, 1.000000000000000222, 0.9999999999999996669, 1.000000000000000444, 0.9999999999999997780, 1.000000000000000222, 0.9999999999999997780, 1.000000000000000222, 1.000000000000000000, 1.000000000000000000, 1.000000000000000000, 1.000000000000000000, 1.000000000000000222, 1.000000000000000222, 0.9999999999999997780, 1.000000000000000222, 1.000000000000000000, 1.000000000000000222, 0.9999999999999997780, 1.000000000000000222, 1.000000000000000000, 1.000000000000000000, 0.9999999999999997780, 1.000000000000000000, 1.000000000000000000, 0.9999999999999997780, 1.000000000000000222, 0.9999999999999997780, 1.000000000000000222, 0.9999999999999997780, 1.000000000000000444, 1.000000000000000000, 0.9999999999999996669, 1.000000000000000444, 1.000000000000000000, 0.9999999999999997780, 1.000000000000000000, 0.9999999999999996669, 1.000000000000000000, 1.000000000000000222, 0.9999999999999996669, 1.000000000000000222, 0.9999999999999997780, 1.000000000000000000, 1.000000000000000222, 0.9999999999999997780, 1.000000000000000222, 0.9999999999999997780, 1.000000000000000222, 1.000000000000000000, 1.000000000000000000, 1.000000000000000000, 0.9999999999999997780, 1.000000000000000222, 0.9999999999999997780, 1.000000000000000222, 1.000000000000000000, 1.000000000000000000, 1.000000000000000000, 1.000000000000000000, 1.000000000000000444, 0.9999999999999997780, 1.000000000000000444, 0.9999999999999997780, 1.000000000000000222, 1.000000000000000000, 1.000000000000000000, 1.000000000000000000, 1.000000000000000000, 0.9999999999999997780, 1.000000000000000000, 1.000000000000000222, 0.9999999999999997780, 1.000000000000000222, 1.000000000000000000, 1.000000000000000000, 1.000000000000000222, 0.9999999999999997780, 1.000000000000000222, 0.9999999999999996669, 1.000000000000000444, 0.9999999999999994449, 1.000000000000000444, 0.9999999999999997780, 0.9999999999999997780, 1.000000000000000000, 1.000000000000000000, 1.000000000000000222, 1.000000000000000000, 1.000000000000000000, 1.000000000000000000, 1.000000000000000000, 1.000000000000000222, 1.000000000000000444, 0.9999999999999997780, 1.000000000000000222, 1.000000000000000000, 0.9999999999999996669, 1.000000000000000222, 1.000000000000000222, 1.000000000000000222, 1.000000000000000222, 1.000000000000000000, 1.000000000000000000, 1.000000000000000222, 1.000000000000000000, 1.000000000000000222, 1.000000000000000000, 1.000000000000000000, 1.000000000000000000, 1.000000000000000222, 0.9999999999999997780, 1.000000000000000000, 1.000000000000000222, 1.000000000000000000, 1.000000000000000222, 1.000000000000000000, 0.9999999999999997780, 1.000000000000000444, 1.000000000000000000, 0.9999999999999996669, 1.000000000000000222, 0.9999999999999997780, 1.000000000000000222, 1.000000000000000000, 1.000000000000000000, 1.000000000000000444, 0.9999999999999996669, 1.000000000000000000, 0.9999999999999997780, 1.000000000000000000, 0.9999999999999997780, 0.9999999999999997780, 1.000000000000000000, 1.000000000000000000, 1.000000000000000000, 0.9999999999999997780, 1.000000000000000000, 1.000000000000000222, 1.000000000000000222, 1.000000000000000000, 0.9999999999999997780, 1.000000000000000222, 1.000000000000000000, 1.000000000000000000, 1.000000000000000222, 1.000000000000000222, 1.000000000000000222, 1.000000000000000000, 0.9999999999999997780, 1.000000000000000444, 0.9999999999999997780, 1.000000000000000444, 0.9999999999999997780, 1.000000000000000000, 1.000000000000000222, 0.9999999999999997780, 1.000000000000000222, 0.9999999999999997780, 1.000000000000000222, 0.9999999999999997780, 1.000000000000000222, 0.9999999999999996669, 1.000000000000000222, 0.9999999999999997780, 1.000000000000000444, 1.000000000000000000, 1.000000000000000000, 0.9999999999999997780, 1.000000000000000222, 1.000000000000000000, 0.9999999999999996669, 1.000000000000000222, 0.9999999999999997780, 1.000000000000000000, 1.000000000000000222, 1.000000000000000000, 1.000000000000000222, 0.9999999999999996669, 1.000000000000000444, 0.9999999999999996669, 1.000000000000000000, 1.000000000000000000, 1.000000000000000000, 0.9999999999999997780, 1.000000000000000444, 1.000000000000000000, 1.000000000000000000, 1.000000000000000000, 1.000000000000000000, 0.9999999999999997780, 1.000000000000000222, 1.000000000000000222, 1.000000000000000222, 1.000000000000000000, 1.000000000000000222, 1.000000000000000000, 0.9999999999999997780, 1.000000000000000444, 1.000000000000000000, 0.9999999999999997780, 1.000000000000000222, 0.9999999999999996669, 1.000000000000000222, 1.000000000000000000, 1.000000000000000444, 1.000000000000000222, 0.9999999999999996669, 1.000000000000000222, 0.9999999999999997780, 1.000000000000000222, 1.000000000000000222, 0.9999999999999997780, 1.000000000000000222, 1.000000000000000000, 1.000000000000000222, 1.000000000000000222, 0.9999999999999997780, 1.000000000000000444, 0.9999999999999996669, 1.000000000000000222, 1.000000000000000222, 1.000000000000000000, 1.000000000000000000, 1.000000000000000000, 1.000000000000000222, 1.000000000000000000, 1.000000000000000000, 1.000000000000000222, 0.9999999999999996669, 1.000000000000000444, 1.000000000000000222, 0.9999999999999997780, 1.000000000000000222, 0.9999999999999997780, 1.000000000000000444, 0.9999999999999996669, 1.000000000000000666, 0.9999999999999994449, 1.000000000000000222, 0.9999999999999997780, 1.000000000000000444, 1.000000000000000000, 1.000000000000000222, 1.000000000000000222, 1.000000000000000000, 0.9999999999999997780, 0.9999999999999997780, 1.000000000000000444, 1.000000000000000000, 1.000000000000000000, 1.000000000000000000, 0.9999999999999997780, 1.000000000000000222, 1.000000000000000222, 0.9999999999999997780, 1.000000000000000222, 1.000000000000000000, 1.000000000000000444, 0.9999999999999996669, 1.000000000000000444, 0.9999999999999997780, 1.000000000000000000, 0.9999999999999997780, 1.000000000000000444, 0.9999999999999996669, 1.000000000000000444, 1.000000000000000000, 1.000000000000000000, 1.000000000000000000, 0.9999999999999997780, 1.000000000000000444, 1.000000000000000222, 0.9999999999999997780, 1.000000000000000444, 1.000000000000000000, 0.9999999999999996669, 1.000000000000000444, 1.000000000000000000, 1.000000000000000000, 1.000000000000000000, 0.9999999999999997780, 1.000000000000000222, 0.9999999999999997780, 1.000000000000000000, 1.000000000000000222, 0.9999999999999997780, 1.000000000000000000, 1.000000000000000000, 0.9999999999999997780, 1.000000000000000444, 0.9999999999999997780, 1.000000000000000444, 0.9999999999999994449, 1.000000000000000444, 0.9999999999999997780, 1.000000000000000444, 0.9999999999999997780, 1.000000000000000000, 0.9999999999999997780, 1.000000000000000222, 1.000000000000000222, 1.000000000000000000, 1.000000000000000000),
 ( 0.3333333333333333703, 0.3333333333333333703, 0.3333333333333333703, 0.3333333333333335369, 0.3333333333333333148, 0.3333333333333333703, 0.3333333333333333703, 0.3333333333333333148, 0.3333333333333333148, 0.3333333333333334259, 0.3333333333333333703, 0.3333333333333333148, 0.3333333333333334259, 0.3333333333333333148, 0.3333333333333334259, 0.3333333333333333148, 0.3333333333333333703, 0.3333333333333333148, 0.3333333333333334814, 0.3333333333333333148, 0.3333333333333334814, 0.3333333333333334814, 0.3333333333333333148, 0.3333333333333334259, 0.3333333333333333148, 0.3333333333333333703, 0.3333333333333333148, 0.3333333333333334814, 0.3333333333333333703, 0.3333333333333333703, 0.3333333333333333703, 0.3333333333333334259, 0.3333333333333333148, 0.3333333333333333148, 0.3333333333333334259, 0.3333333333333333703, 0.3333333333333334259, 0.3333333333333334259, 0.3333333333333332038, 0.3333333333333334814, 0.3333333333333333703, 0.3333333333333334814, 0.3333333333333332593, 0.3333333333333334259, 0.3333333333333333703, 0.3333333333333334259, 0.3333333333333333148, 0.3333333333333333703, 0.3333333333333334259, 0.3333333333333333148, 0.3333333333333332038, 0.3333333333333335369, 0.3333333333333332593, 0.3333333333333334814, 0.3333333333333333148, 0.3333333333333333703, 0.3333333333333334259, 0.3333333333333333703, 0.3333333333333334814, 0.3333333333333333703, 0.3333333333333334259, 0.3333333333333333148, 0.3333333333333334814, 0.3333333333333332038, 0.3333333333333334259, 0.3333333333333333148, 0.3333333333333333703, 0.3333333333333333703, 0.3333333333333334259, 0.3333333333333333148, 0.3333333333333333703, 0.3333333333333334259, 0.3333333333333333148, 0.3333333333333333703, 0.3333333333333333703, 0.3333333333333335369, 0.3333333333333333148, 0.3333333333333333703, 0.3333333333333333703, 0.3333333333333333703, 0.3333333333333333148, 0.3333333333333333703, 0.3333333333333334814, 0.3333333333333333148, 0.3333333333333334814, 0.3333333333333333703, 0.3333333333333334259, 0.3333333333333333148, 0.3333333333333334259, 0.3333333333333333148, 0.3333333333333334259, 0.3333333333333333148, 0.3333333333333333703, 0.3333333333333333703, 0.3333333333333333703, 0.3333333333333334259, 0.3333333333333334259, 0.3333333333333332593, 0.3333333333333334259, 0.3333333333333333703, 0.3333333333333334259, 0.3333333333333333148, 0.3333333333333334259, 0.3333333333333333703, 0.3333333333333333703, 0.3333333333333333148, 0.3333333333333334259, 0.3333333333333333703, 0.3333333333333333148, 0.3333333333333334259, 0.3333333333333332038, 0.3333333333333334814, 0.3333333333333333148, 0.3333333333333335369, 0.3333333333333334259, 0.3333333333333332038, 0.3333333333333334814, 0.3333333333333333703, 0.3333333333333332593, 0.3333333333333333703, 0.3333333333333332593, 0.3333333333333333703, 0.3333333333333334814, 0.3333333333333333148, 0.3333333333333334814, 0.3333333333333333148, 0.3333333333333334259, 0.3333333333333334259, 0.3333333333333333148, 0.3333333333333334259, 0.3333333333333333148, 0.3333333333333334259, 0.3333333333333333703, 0.3333333333333333703, 0.3333333333333334259, 0.3333333333333332593, 0.3333333333333334814, 0.3333333333333333148, 0.3333333333333333703, 0.3333333333333333703, 0.3333333333333333703, 0.3333333333333334259, 0.3333333333333334259, 0.3333333333333334814, 0.3333333333333333703, 0.3333333333333334259, 0.3333333333333333703, 0.3333333333333333703, 0.3333333333333333148, 0.3333333333333333703, 0.3333333333333334259, 0.3333333333333333148, 0.3333333333333333148, 0.3333333333333333148, 0.3333333333333334259, 0.3333333333333333148, 0.3333333333333334814, 0.3333333333333333148, 0.3333333333333334259, 0.3333333333333334259, 0.3333333333333333148, 0.3333333333333334814, 0.3333333333333333148, 0.3333333333333334814, 0.3333333333333332593, 0.3333333333333335369, 0.3333333333333333148, 0.3333333333333333703, 0.3333333333333333703, 0.3333333333333334259, 0.3333333333333333703, 0.3333333333333333703, 0.3333333333333333148, 0.3333333333333333703, 0.3333333333333332593, 0.3333333333333335369, 0.3333333333333334259, 0.3333333333333333703, 0.3333333333333334259, 0.3333333333333334259, 0.3333333333333332038, 0.3333333333333334814, 0.3333333333333333703, 0.3333333333333334259, 0.3333333333333333703, 0.3333333333333333703, 0.3333333333333333148, 0.3333333333333334814, 0.3333333333333333148, 0.3333333333333334814, 0.3333333333333334259, 0.3333333333333333148, 0.3333333333333333703, 0.3333333333333333703, 0.3333333333333333703, 0.3333333333333333703, 0.3333333333333334259, 0.3333333333333333148, 0.3333333333333334814, 0.3333333333333333148, 0.3333333333333333703, 0.3333333333333334814, 0.3333333333333332593, 0.3333333333333333148, 0.3333333333333334259, 0.3333333333333332593, 0.3333333333333335369, 0.3333333333333333703, 0.3333333333333334259, 0.3333333333333335369, 0.3333333333333333148, 0.3333333333333333703, 0.3333333333333333148, 0.3333333333333333703, 0.3333333333333333148, 0.3333333333333333148, 0.3333333333333333703, 0.3333333333333333703, 0.3333333333333333703, 0.3333333333333333148, 0.3333333333333333703, 0.3333333333333333703, 0.3333333333333334259, 0.3333333333333333703, 0.3333333333333333148, 0.3333333333333333703, 0.3333333333333333703, 0.3333333333333333703, 0.3333333333333334259, 0.3333333333333334259, 0.3333333333333334814, 0.3333333333333332593, 0.3333333333333334259, 0.3333333333333334259, 0.3333333333333333148, 0.3333333333333334259, 0.3333333333333333703, 0.3333333333333333148, 0.3333333333333334814, 0.3333333333333333703, 0.3333333333333334259, 0.3333333333333332593, 0.3333333333333334259, 0.3333333333333332593, 0.3333333333333334814, 0.3333333333333332593, 0.3333333333333334259, 0.3333333333333333148, 0.3333333333333334259, 0.3333333333333333703, 0.3333333333333334259, 0.3333333333333333703, 0.3333333333333333703, 0.3333333333333333703, 0.3333333333333333148, 0.3333333333333334259, 0.3333333333333333703, 0.3333333333333333148, 0.3333333333333334259, 0.3333333333333333148, 0.3333333333333333703, 0.3333333333333333148, 0.3333333333333334814, 0.3333333333333332593, 0.3333333333333333703, 0.3333333333333333703, 0.3333333333333334259, 0.3333333333333332593, 0.3333333333333335369, 0.3333333333333333703, 0.3333333333333333703, 0.3333333333333333703, 0.3333333333333333148, 0.3333333333333333148, 0.3333333333333334259, 0.3333333333333334814, 0.3333333333333334259, 0.3333333333333333703, 0.3333333333333334259, 0.3333333333333334259, 0.3333333333333333703, 0.3333333333333334814, 0.3333333333333333148, 0.3333333333333333148, 0.3333333333333334259, 0.3333333333333332038, 0.3333333333333334814, 0.3333333333333333148, 0.3333333333333335369, 0.3333333333333334259, 0.3333333333333333148, 0.3333333333333334814, 0.3333333333333333703, 0.3333333333333333703, 0.3333333333333334259, 0.3333333333333333703, 0.3333333333333334259, 0.3333333333333333703, 0.3333333333333334259, 0.3333333333333333148, 0.3333333333333333703, 0.3333333333333335369, 0.3333333333333332038, 0.3333333333333334814, 0.3333333333333333703, 0.3333333333333333148, 0.3333333333333334259, 0.3333333333333333703, 0.3333333333333333148, 0.3333333333333334259, 0.3333333333333333703, 0.3333333333333334259, 0.3333333333333332593, 0.3333333333333335369, 0.3333333333333334814, 0.3333333333333333148, 0.3333333333333334259, 0.3333333333333333148, 0.3333333333333335369, 0.3333333333333332593, 0.3333333333333335924, 0.3333333333333332593, 0.3333333333333333703, 0.3333333333333333703, 0.3333333333333334814, 0.3333333333333333703, 0.3333333333333334814, 0.3333333333333333703, 0.3333333333333334259, 0.3333333333333332593, 0.3333333333333334259, 0.3333333333333335369, 0.3333333333333333148, 0.3333333333333334814, 0.3333333333333333148, 0.3333333333333333703, 0.3333333333333334259, 0.3333333333333334259, 0.3333333333333332593, 0.3333333333333334259, 0.3333333333333333148, 0.3333333333333335369, 0.3333333333333332593, 0.3333333333333335369, 0.3333333333333333148, 0.3333333333333333148, 0.3333333333333333703, 0.3333333333333334814, 0.3333333333333333148, 0.3333333333333334259, 0.3333333333333333148, 0.3333333333333334259, 0.3333333333333333703, 0.3333333333333333148, 0.3333333333333334259, 0.3333333333333334814, 0.3333333333333333148, 0.3333333333333334814, 0.3333333333333333703, 0.3333333333333332593, 0.3333333333333334259, 0.3333333333333333703, 0.3333333333333334259, 0.3333333333333333703, 0.3333333333333333148, 0.3333333333333334259, 0.3333333333333333703, 0.3333333333333333148, 0.3333333333333334259, 0.3333333333333333148, 0.3333333333333333148, 0.3333333333333333703, 0.3333333333333333703, 0.3333333333333334259, 0.3333333333333333148, 0.3333333333333334259, 0.3333333333333332593, 0.3333333333333334259, 0.3333333333333333703, 0.3333333333333334259, 0.3333333333333333703, 0.3333333333333333703, 0.3333333333333333148, 0.3333333333333334814, 0.3333333333333334259, 0.3333333333333333703, 0.3333333333333333703),
 ( 0.3333333333333333703, 0.3333333333333333703, 0.3333333333333333703, 0.3333333333333335369, 0.3333333333333333148, 0.3333333333333333703, 0.3333333333333333703, 0.3333333333333333148, 0.3333333333333333148, 0.3333333333333334259, 0.3333333333333333703, 0.3333333333333333148, 0.3333333333333334259, 0.3333333333333333148, 0.3333333333333334259, 0.3333333333333333148, 0.3333333333333333703, 0.3333333333333333148, 0.3333333333333334814, 0.3333333333333333148, 0.3333333333333334814, 0.3333333333333334814, 0.3333333333333333148, 0.3333333333333334259, 0.3333333333333333148, 0.3333333333333333703, 0.3333333333333333148, 0.3333333333333334814, 0.3333333333333333703, 0.3333333333333333703, 0.3333333333333333703, 0.3333333333333334259, 0.3333333333333333148, 0.3333333333333333148, 0.3333333333333334259, 0.3333333333333333703, 0.3333333333333334259, 0.3333333333333334259, 0.3333333333333332038, 0.3333333333333334814, 0.3333333333333333703, 0.3333333333333334814, 0.3333333333333332593, 0.3333333333333334259, 0.3333333333333333703, 0.3333333333333334259, 0.3333333333333333148, 0.3333333333333333703, 0.3333333333333334259, 0.3333333333333333148, 0.3333333333333332038, 0.3333333333333335369, 0.3333333333333332593, 0.3333333333333334814, 0.3333333333333333148, 0.3333333333333333703, 0.3333333333333334259, 0.3333333333333333703, 0.3333333333333334814, 0.3333333333333333703, 0.3333333333333334259, 0.3333333333333333148, 0.3333333333333334814, 0.3333333333333332038, 0.3333333333333334259, 0.3333333333333333148, 0.3333333333333333703, 0.3333333333333333703, 0.3333333333333334259, 0.3333333333333333148, 0.3333333333333333703, 0.3333333333333334259, 0.3333333333333333148, 0.3333333333333333703, 0.3333333333333333703, 0.3333333333333335369, 0.3333333333333333148, 0.3333333333333333703, 0.3333333333333333703, 0.3333333333333333703, 0.3333333333333333148, 0.3333333333333333703, 0.3333333333333334814, 0.3333333333333333148, 0.3333333333333334814, 0.3333333333333333703, 0.3333333333333334259, 0.3333333333333333148, 0.3333333333333334259, 0.3333333333333333148, 0.3333333333333334259, 0.3333333333333333148, 0.3333333333333333703, 0.3333333333333333703, 0.3333333333333333703, 0.3333333333333334259, 0.3333333333333334259, 0.3333333333333332593, 0.3333333333333334259, 0.3333333333333333703, 0.3333333333333334259, 0.3333333333333333148, 0.3333333333333334259, 0.3333333333333333703, 0.3333333333333333703, 0.3333333333333333148, 0.3333333333333334259, 0.3333333333333333703, 0.3333333333333333148, 0.3333333333333334259, 0.3333333333333332038, 0.3333333333333334814, 0.3333333333333333148, 0.3333333333333335369, 0.3333333333333334259, 0.3333333333333332038, 0.3333333333333334814, 0.3333333333333333703, 0.3333333333333332593, 0.3333333333333333703, 0.3333333333333332593, 0.3333333333333333703, 0.3333333333333334814, 0.3333333333333333148, 0.3333333333333334814, 0.3333333333333333148, 0.3333333333333334259, 0.3333333333333334259, 0.3333333333333333148, 0.3333333333333334259, 0.3333333333333333148, 0.3333333333333334259, 0.3333333333333333703, 0.3333333333333333703, 0.3333333333333334259, 0.3333333333333332593, 0.3333333333333334814, 0.3333333333333333148, 0.3333333333333333703, 0.3333333333333333703, 0.3333333333333333703, 0.3333333333333334259, 0.3333333333333334259, 0.3333333333333334814, 0.3333333333333333703, 0.3333333333333334259, 0.3333333333333333703, 0.3333333333333333703, 0.3333333333333333148, 0.3333333333333333703, 0.3333333333333334259, 0.3333333333333333148, 0.3333333333333333148, 0.3333333333333333148, 0.3333333333333334259, 0.3333333333333333148, 0.3333333333333334814, 0.3333333333333333148, 0.3333333333333334259, 0.3333333333333334259, 0.3333333333333333148, 0.3333333333333334814, 0.3333333333333333148, 0.3333333333333334814, 0.3333333333333332593, 0.3333333333333335369, 0.3333333333333333148, 0.3333333333333333703, 0.3333333333333333703, 0.3333333333333334259, 0.3333333333333333703, 0.3333333333333333703, 0.3333333333333333148, 0.3333333333333333703, 0.3333333333333332593, 0.3333333333333335369, 0.3333333333333334259, 0.3333333333333333703, 0.3333333333333334259, 0.3333333333333334259, 0.3333333333333332038, 0.3333333333333334814, 0.3333333333333333703, 0.3333333333333334259, 0.3333333333333333703, 0.3333333333333333703, 0.3333333333333333148, 0.3333333333333334814, 0.3333333333333333148, 0.3333333333333334814, 0.3333333333333334259, 0.3333333333333333148, 0.3333333333333333703, 0.3333333333333333703, 0.3333333333333333703, 0.3333333333333333703, 0.3333333333333334259, 0.3333333333333333148, 0.3333333333333334814, 0.3333333333333333148, 0.3333333333333333703, 0.3333333333333334814, 0.3333333333333332593, 0.3333333333333333148, 0.3333333333333334259, 0.3333333333333332593, 0.3333333333333335369, 0.3333333333333333703, 0.3333333333333334259, 0.3333333333333335369, 0.3333333333333333148, 0.3333333333333333703, 0.3333333333333333148, 0.3333333333333333703, 0.3333333333333333148, 0.3333333333333333148, 0.3333333333333333703, 0.3333333333333333703, 0.3333333333333333703, 0.3333333333333333148, 0.3333333333333333703, 0.3333333333333333703, 0.3333333333333334259, 0.3333333333333333703, 0.3333333333333333148, 0.3333333333333333703, 0.3333333333333333703, 0.3333333333333333703, 0.3333333333333334259, 0.3333333333333334259, 0.3333333333333334814, 0.3333333333333332593, 0.3333333333333334259, 0.3333333333333334259, 0.3333333333333333148, 0.3333333333333334259, 0.3333333333333333703, 0.3333333333333333148, 0.3333333333333334814, 0.3333333333333333703, 0.3333333333333334259, 0.3333333333333332593, 0.3333333333333334259, 0.3333333333333332593, 0.3333333333333334814, 0.3333333333333332593, 0.3333333333333334259, 0.3333333333333333148, 0.3333333333333334259, 0.3333333333333333703, 0.3333333333333334259, 0.3333333333333333703, 0.3333333333333333703, 0.3333333333333333703, 0.3333333333333333148, 0.3333333333333334259, 0.3333333333333333703, 0.3333333333333333148, 0.3333333333333334259, 0.3333333333333333148, 0.3333333333333333703, 0.3333333333333333148, 0.3333333333333334814, 0.3333333333333332593, 0.3333333333333333703, 0.3333333333333333703, 0.3333333333333334259, 0.3333333333333332593, 0.3333333333333335369, 0.3333333333333333703, 0.3333333333333333703, 0.3333333333333333703, 0.3333333333333333148, 0.3333333333333333148, 0.3333333333333334259, 0.3333333333333334814, 0.3333333333333334259, 0.3333333333333333703, 0.3333333333333334259, 0.3333333333333334259, 0.3333333333333333703, 0.3333333333333334814, 0.3333333333333333148, 0.3333333333333333148, 0.3333333333333334259, 0.3333333333333332038, 0.3333333333333334814, 0.3333333333333333148, 0.3333333333333335369, 0.3333333333333334259, 0.3333333333333333148, 0.3333333333333334814, 0.3333333333333333703, 0.3333333333333333703, 0.3333333333333334259, 0.3333333333333333703, 0.3333333333333334259, 0.3333333333333333703, 0.3333333333333334259, 0.3333333333333333148, 0.3333333333333333703, 0.3333333333333335369, 0.3333333333333332038, 0.3333333333333334814, 0.3333333333333333703, 0.3333333333333333148, 0.3333333333333334259, 0.3333333333333333703, 0.3333333333333333148, 0.3333333333333334259, 0.3333333333333333703, 0.3333333333333334259, 0.3333333333333332593, 0.3333333333333335369, 0.3333333333333334814, 0.3333333333333333148, 0.3333333333333334259, 0.3333333333333333148, 0.3333333333333335369, 0.3333333333333332593, 0.3333333333333335924, 0.3333333333333332593, 0.3333333333333333703, 0.3333333333333333703, 0.3333333333333334814, 0.3333333333333333703, 0.3333333333333334814, 0.3333333333333333703, 0.3333333333333334259, 0.3333333333333332593, 0.3333333333333334259, 0.3333333333333335369, 0.3333333333333333148, 0.3333333333333334814, 0.3333333333333333148, 0.3333333333333333703, 0.3333333333333334259, 0.3333333333333334259, 0.3333333333333332593, 0.3333333333333334259, 0.3333333333333333148, 0.3333333333333335369, 0.3333333333333332593, 0.3333333333333335369, 0.3333333333333333148, 0.3333333333333333148, 0.3333333333333333703, 0.3333333333333334814, 0.3333333333333333148, 0.3333333333333334259, 0.3333333333333333148, 0.3333333333333334259, 0.3333333333333333703, 0.3333333333333333148, 0.3333333333333334259, 0.3333333333333334814, 0.3333333333333333148, 0.3333333333333334814, 0.3333333333333333703, 0.3333333333333332593, 0.3333333333333334259, 0.3333333333333333703, 0.3333333333333334259, 0.3333333333333333703, 0.3333333333333333148, 0.3333333333333334259, 0.3333333333333333703, 0.3333333333333333148, 0.3333333333333334259, 0.3333333333333333148, 0.3333333333333333148, 0.3333333333333333703, 0.3333333333333333703, 0.3333333333333334259, 0.3333333333333333148, 0.3333333333333334259, 0.3333333333333332593, 0.3333333333333334259, 0.3333333333333333703, 0.3333333333333334259, 0.3333333333333333703, 0.3333333333333333703, 0.3333333333333333148, 0.3333333333333334814, 0.3333333333333334259, 0.3333333333333333703, 0.3333333333333333703),
 ( 1.000000000000000000, 1.000000000000000000, 1.000000000000000000, 1.000000000000000222, 0.9999999999999996669, 1.000000000000000222, 0.9999999999999997780, 1.000000000000000000, 0.9999999999999997780, 1.000000000000000444, 1.000000000000000000, 0.9999999999999997780, 1.000000000000000222, 1.000000000000000000, 0.9999999999999997780, 1.000000000000000222, 0.9999999999999996669, 1.000000000000000000, 1.000000000000000222, 1.000000000000000000, 1.000000000000000000, 1.000000000000000444, 0.9999999999999994449, 1.000000000000000444, 0.9999999999999996669, 1.000000000000000222, 1.000000000000000000, 1.000000000000000444, 1.000000000000000000, 0.9999999999999997780, 1.000000000000000000, 1.000000000000000222, 0.9999999999999997780, 0.9999999999999997780, 1.000000000000000444, 0.9999999999999997780, 1.000000000000000444, 1.000000000000000222, 0.9999999999999996669, 1.000000000000000222, 1.000000000000000000, 1.000000000000000444, 0.9999999999999997780, 1.000000000000000222, 1.000000000000000222, 1.000000000000000222, 0.9999999999999997780, 1.000000000000000000, 1.000000000000000000, 1.000000000000000000, 0.9999999999999994449, 1.000000000000000444, 0.9999999999999997780, 1.000000000000000444, 0.9999999999999997780, 1.000000000000000000, 1.000000000000000000, 0.9999999999999997780, 1.000000000000000444, 0.9999999999999996669, 1.000000000000000444, 0.9999999999999996669, 1.000000000000000222, 0.9999999999999994449, 1.000000000000000222, 1.000000000000000000, 1.000000000000000000, 1.000000000000000000, 1.000000000000000000, 1.000000000000000222, 1.000000000000000000, 1.000000000000000222, 0.9999999999999996669, 1.000000000000000222, 1.000000000000000000, 1.000000000000000444, 1.000000000000000000, 1.000000000000000000, 0.9999999999999997780, 1.000000000000000222, 0.9999999999999997780, 0.9999999999999997780, 1.000000000000000444, 1.000000000000000000, 1.000000000000000222, 0.9999999999999996669, 1.000000000000000444, 0.9999999999999997780, 1.000000000000000222, 0.9999999999999997780, 1.000000000000000222, 1.000000000000000000, 1.000000000000000000, 1.000000000000000000, 1.000000000000000000, 1.000000000000000222, 1.000000000000000222, 0.9999999999999997780, 1.000000000000000222, 1.000000000000000000, 1.000000000000000222, 0.9999999999999997780, 1.000000000000000222, 1.000000000000000000, 1.000000000000000000, 0.9999999999999997780, 1.000000000000000000, 1.000000000000000000, 0.9999999999999997780, 1.000000000000000222, 0.9999999999999997780, 1.000000000000000222, 0.9999999999999997780, 1.000000000000000444, 1.000000000000000000, 0.9999999999999996669, 1.000000000000000444, 1.000000000000000000, 0.9999999999999997780, 1.000000000000000000, 0.9999999999999996669, 1.000000000000000000, 1.000000000000000222, 0.9999999999999996669, 1.000000000000000222, 0.9999999999999997780, 1.000000000000000000, 1.000000000000000222, 0.9999999999999997780, 1.000000000000000222, 0.9999999999999997780, 1.000000000000000222, 1.000000000000000000, 1.000000000000000000, 1.000000000000000000, 0.9999999999999997780, 1.000000000000000222, 0.9999999999999997780, 1.000000000000000222, 1.000000000000000000, 1.000000000000000000, 1.000000000000000000, 1.000000000000000000, 1.000000000000000444, 0.9999999999999997780, 1.000000000000000444, 0.9999999999999997780, 1.000000000000000222, 1.000000000000000000, 1.000000000000000000, 1.000000000000000000, 1.000000000000000000, 0.9999999999999997780, 1.000000000000000000, 1.000000000000000222, 0.9999999999999997780, 1.000000000000000222, 1.000000000000000000, 1.000000000000000000, 1.000000000000000222, 0.9999999999999997780, 1.000000000000000222, 0.9999999999999996669, 1.000000000000000444, 0.9999999999999994449, 1.000000000000000444, 0.9999999999999997780, 0.9999999999999997780, 1.000000000000000000, 1.000000000000000000, 1.000000000000000222, 1.000000000000000000, 1.000000000000000000, 1.000000000000000000, 1.000000000000000000, 1.000000000000000222, 1.000000000000000444, 0.9999999999999997780, 1.000000000000000222, 1.000000000000000000, 0.9999999999999996669, 1.000000000000000222, 1.000000000000000222, 1.000000000000000222, 1.000000000000000222, 1.000000000000000000, 1.000000000000000000, 1.000000000000000222, 1.000000000000000000, 1.000000000000000222, 1.000000000000000000, 1.000000000000000000, 1.000000000000000000, 1.000000000000000222, 0.9999999999999997780, 1.000000000000000000, 1.000000000000000222, 1.000000000000000000, 1.000000000000000222, 1.000000000000000000, 0.9999999999999997780, 1.000000000000000444, 1.000000000000000000, 0.9999999999999996669, 1.000000000000000222, 0.9999999999999997780, 1.000000000000000222, 1.000000000000000000, 1.000000000000000000, 1.000000000000000444, 0.9999999999999996669, 1.000000000000000000, 0.9999999999999997780, 1.000000000000000000, 0.9999999999999997780, 0.9999999999999997780, 1.000000000000000000, 1.000000000000000000, 1.000000000000000000, 0.9999999999999997780, 1.000000000000000000, 1.000000000000000222, 1.000000000000000222, 1.000000000000000000, 0.9999999999999997780, 1.000000000000000222, 1.000000000000000000, 1.000000000000000000, 1.000000000000000222, 1.000000000000000222, 1.000000000000000222, 1.000000000000000000, 0.9999999999999997780, 1.000000000000000444, 0.9999999999999997780, 1.000000000000000444, 0.9999999999999997780, 1.000000000000000000, 1.000000000000000222, 0.9999999999999997780, 1.000000000000000222, 0.9999999999999997780, 1.000000000000000222, 0.9999999999999997780, 1.000000000000000222, 0.9999999999999996669, 1.000000000000000222, 0.9999999999999997780, 1.000000000000000444, 1.000000000000000000, 1.000000000000000000, 0.9999999999999997780, 1.000000000000000222, 1.000000000000000000, 0.9999999999999996669, 1.000000000000000222, 0.9999999999999997780, 1.000000000000000000, 1.000000000000000222, 1.000000000000000000, 1.000000000000000222, 0.9999999999999996669, 1.000000000000000444, 0.9999999999999996669, 1.000000000000000000, 1.000000000000000000, 1.000000000000000000, 0.9999999999999997780, 1.000000000000000444, 1.000000000000000000, 1.000000000000000000, 1.000000000000000000, 1.000000000000000000, 0.9999999999999997780, 1.000000000000000222, 1.000000000000000222, 1.000000000000000222, 1.000000000000000000, 1.000000000000000222, 1.000000000000000000, 0.9999999999999997780, 1.000000000000000444, 1.000000000000000000, 0.9999999999999997780, 1.000000000000000222, 0.9999999999999996669, 1.000000000000000222, 1.000000000000000000, 1.000000000000000444, 1.000000000000000222, 0.9999999999999996669, 1.000000000000000222, 0.9999999999999997780, 1.000000000000000222, 1.000000000000000222, 0.9999999999999997780, 1.000000000000000222, 1.000000000000000000, 1.000000000000000222, 1.000000000000000222, 0.9999999999999997780, 1.000000000000000444, 0.9999999999999996669, 1.000000000000000222, 1.000000000000000222, 1.000000000000000000, 1.000000000000000000, 1.000000000000000000, 1.000000000000000222, 1.000000000000000000, 1.000000000000000000, 1.000000000000000222, 0.9999999999999996669, 1.000000000000000444, 1.000000000000000222, 0.9999999999999997780, 1.000000000000000222, 0.9999999999999997780, 1.000000000000000444, 0.9999999999999996669, 1.000000000000000666, 0.9999999999999994449, 1.000000000000000222, 0.9999999999999997780, 1.000000000000000444, 1.000000000000000000, 1.000000000000000222, 1.000000000000000222, 1.000000000000000000, 0.9999999999999997780, 0.9999999999999997780, 1.000000000000000444, 1.000000000000000000, 1.000000000000000000, 1.000000000000000000, 0.9999999999999997780, 1.000000000000000222, 1.000000000000000222, 0.9999999999999997780, 1.000000000000000222, 1.000000000000000000, 1.000000000000000444, 0.9999999999999996669, 1.000000000000000444, 0.9999999999999997780, 1.000000000000000000, 0.9999999999999997780, 1.000000000000000444, 0.9999999999999996669, 1.000000000000000444, 1.000000000000000000, 1.000000000000000000, 1.000000000000000000, 0.9999999999999997780, 1.000000000000000444, 1.000000000000000222, 0.9999999999999997780, 1.000000000000000444, 1.000000000000000000, 0.9999999999999996669, 1.000000000000000444, 1.000000000000000000, 1.000000000000000000, 1.000000000000000000, 0.9999999999999997780, 1.000000000000000222, 0.9999999999999997780, 1.000000000000000000, 1.000000000000000222, 0.9999999999999997780, 1.000000000000000000, 1.000000000000000000, 0.9999999999999997780, 1.000000000000000444, 0.9999999999999997780, 1.000000000000000444, 0.9999999999999994449, 1.000000000000000444, 0.9999999999999997780, 1.000000000000000444, 0.9999999999999997780, 1.000000000000000000, 0.9999999999999997780, 1.000000000000000222, 1.000000000000000222, 1.000000000000000000, 1.000000000000000000) ) ) 
 REPRESENTATION_ITEM ( '' )  SURFACE ( )  );
#90953 = CARTESIAN_POINT ( 'NONE',  ( 3.884249253383244227, -1.119368145229171052, 1.966044450452981929 ) ) ;
#90954 = CARTESIAN_POINT ( 'NONE',  ( 5.127606433170654121, -2.000101594804974514, 0.6598296307055817600 ) ) ;
#90955 = CARTESIAN_POINT ( 'NONE',  ( -7.593975437430151132, 8.032261896522864930, -0.7216878364870338292 ) ) ;
#90956 = CARTESIAN_POINT ( 'NONE',  ( 3.075218854414006220, 1.681628227459546432, -0.5517178611392310472 ) ) ;
#90958 = CARTESIAN_POINT ( 'NONE',  ( 6.269073568569841548, 2.194993726949866719, -0.6609628413071825248 ) ) ;
#90957 = CARTESIAN_POINT ( 'NONE',  ( 4.543390873910913896, 5.433615786718446472, 1.082531754730549078 ) ) ;
#90959 = CARTESIAN_POINT ( 'NONE',  ( 5.261588992693945421, 0.9106475924270783784, 1.600083007495013643 ) ) ;
#90960 = CARTESIAN_POINT ( 'NONE',  ( -4.796887421136680985, 4.490790167614548523, 1.214306433183764966E-14 ) ) ;
#90961 = CARTESIAN_POINT ( 'NONE',  ( -0.7499999999999972244, 3.608333333333359150, -1.299038105676652011 ) ) ;
#90962 = CARTESIAN_POINT ( 'NONE',  ( 5.419949545929089396, 1.307550890958172785, -1.758484179531449421 ) ) ;
#90963 = CARTESIAN_POINT ( 'NONE',  ( -2.300079615812729905, 5.835176651756807331, -0.7998128361456281477 ) ) ;
#90964 = CARTESIAN_POINT ( 'NONE',  ( -6.714337407434930682, 15.44785316226682603, 9.902284344783144121 ) ) ;
#90965 =( BOUNDED_SURFACE ( )  B_SPLINE_SURFACE ( 1, 2, ( 
 ( #93562, #44817, #113065, #160677, #27464, #26394, #92507, #158544, #159608, #96773, #110922, #128274, #178003, #176927, #28544, #161758, #29618, #94634, #95704, #13349, #79424, #145541, #63173, #15468, #32808, #133543, #97827, #197427, #199551, #162825, #116250, #100991, #81553, #132481, #65280, #163892, #31756, #16528, #149764, #48022, #182238, #130389, #18672, #147636, #33863, #213654, #183312, #99942, #82611, #131427, #196380, #98883, #180130, #114137, #166006, #17590, #49069, #14400, #146590, #66335, #115188, #67403, #83674, #51194, #181183, #164936, #117316, #1341, #34918, #148695, #167081, #80492, #212608, #64247, #265, #198483, #50128, #207972, #192782, #127906, #63866, #209027, #11909, #130021, #141960, #62791, #31379, #126825, #12969, #176559, #60662, #76906, #45507, #162448, #27093, #128953, #109496, #163510, #80110, #196012, #59599, #79045, #161385, #47648, #110558, #77982, #97455, #145161, #143032, #211166, #125757, #93200, #159231, #146215, #29244, #144105, #194932, #44440, #112688, #191718, #46569, #178699, #15096, #210099, #193858, #61739, #10832, #43375, #175503, #28169, #212233, #111623, #30313, #96398, #177636, #95336, #14024, #94265, #113759, #160305, #179763, #184001, #105733, #82236, #51889, #150465, #19361, #3095, #201299, #35616, #135285, #122037, #69165, #50812, #166701, #181859, #18292, #98504, #81185, #149382, #165632, #148327, #85441, #214327, #133166, #65959, #118012, #147263, #2026, #167764, #101694, #115874, #199166, #964, #151526, #39628, #188002, #132108, #197059, #164566, #114811, #116938, #198116, #55879, #182938, #171762, #34554, #213295, #83297, #67029, #64921, #32436, #100625, #131071, #48697, #84378, #68095, #134230, #180810, #200239, #16151, #49747, #33495, #99568, #17220, #128473, #28750, #190171, #92704, #74304, #62314, #208537, #26603, #158750, #127402, #60173, #194441, #11414, #175016, #192289, #111129, #43949, #12480, #42890, #142529, #27675, #193374, #108999, #126330, #159810, #112202, #110065, #59106, #210685, #25536, #140400, #93770, #156630, #144672, #176077, #160885 ),
 ( #207487, #10345, #46083, #77489, #91644, #143608, #24455, #41825, #124208, #94834, #209601, #76419, #61245, #157697, #45019, #8219, #177132, #78554, #90569, #206419, #58043, #107938, #173963, #9294, #75367, #125266, #141479, #191227, #49271, #197627, #180330, #65478, #148892, #96975, #31952, #51399, #29825, #66534, #199754, #179275, #465, #33009, #116445, #100137, #83877, #132676, #17790, #1538, #166200, #147840, #115393, #64446, #181386, #195517, #178209, #98037, #48222, #30898, #182439, #163023, #15671, #14605, #198682, #95908, #99088, #50327, #34066, #212809, #81758, #164090, #149969, #133746, #67600, #80703, #79623, #47154, #211742, #213858, #146793, #161961, #131628, #114335, #16731, #130591, #13551, #145742, #165140, #82816, #63381, #129536, #113270, #196580, #2608, #183512, #151039, #3666, #121809, #20989, #202946, #136919, #119653, #4731, #88160, #36190, #185638, #205085, #35121, #5800, #139058, #118582, #154228, #186710, #55653, #39408, #23127, #71877, #171534, #155295, #105502, #87086, #54590, #69743, #120737, #134800, #117519, #37270, #201871, #184570, #187776, #102266, #169403, #168341, #137987, #101192, #38339, #204004, #89244, #152095, #153156, #103340, #6878, #72956, #167281, #19936, #18866, #200806, #68677, #70806, #86022, #84950, #104415, #52457, #170464, #135848, #53519, #22049, #60994, #7955, #125013, #106595, #94584, #26346, #58857, #190970, #159558, #92459, #160627, #43699, #207233, #10097, #143351, #76171, #44768, #75112, #174771, #59919, #11155, #141224, #158498, #192036, #144426, #142276, #91384, #28493, #57791, #172622, #126075, #188854, #176881, #208287, #193120, #110876, #209346, #12228, #122895, #109816, #175826, #78301, #25282, #42636, #56727, #27418, #123951, #93516, #40490, #74047, #156371, #127147, #77232, #24198, #90301, #140137, #206163, #108745, #189920, #41565, #107678, #173707, #157444, #9038, #83630, #114093, #30644, #182189, #211491, #111953, #213608, #128225, #116202, #147590, #132434, #198435, #148650, #50081, #62070, #81511, #15421, #33817, #179026, #80445, #99896 ) ),
 .UNSPECIFIED., .F., .F., .T. ) 
 B_SPLINE_SURFACE_WITH_KNOTS ( ( 2, 2 ),
 ( 3, 2, 2, 2, 2, 2, 2, 2, 2, 2, 2, 2, 2, 2, 2, 2, 2, 2, 2, 2, 2, 2, 2, 2, 2, 2, 2, 2, 2, 2, 2, 2, 2, 2, 2, 2, 2, 2, 2, 2, 2, 2, 2, 2, 2, 2, 2, 2, 2, 2, 2, 2, 2, 2, 2, 2, 2, 2, 2, 2, 2, 2, 2, 2, 2, 2, 2, 2, 2, 2, 2, 2, 2, 2, 2, 2, 2, 2, 2, 2, 2, 2, 2, 2, 2, 2, 2, 2, 2, 2, 2, 2, 2, 2, 2, 2, 2, 2, 2, 2, 2, 2, 2, 2, 2, 2, 2, 2, 2, 2, 2, 2, 2, 2, 2, 2, 2, 2, 2, 2, 3 ),
 ( 0.000000000000000000, 1.000000000000000000 ),
 ( 0.000000000000000000, 0.008333333333333333218, 0.01666666666666666644, 0.02500000000000000139, 0.03333333333333333287, 0.04166666666666666435, 0.05000000000000000278, 0.05833333333333333426, 0.06666666666666666574, 0.07499999999999999722, 0.08333333333333332871, 0.09166666666666666019, 0.1000000000000000056, 0.1083333333333333370, 0.1166666666666666685, 0.1250000000000000000, 0.1333333333333333315, 0.1416666666666666630, 0.1499999999999999944, 0.1583333333333333259, 0.1666666666666666574, 0.1749999999999999889, 0.1833333333333333204, 0.1916666666666666796, 0.2000000000000000111, 0.2083333333333333426, 0.2166666666666666741, 0.2250000000000000056, 0.2333333333333333370, 0.2416666666666666685, 0.2500000000000000000, 0.2583333333333333592, 0.2666666666666666630, 0.2750000000000000222, 0.2833333333333333259, 0.2916666666666666852, 0.2999999999999999889, 0.3083333333333333481, 0.3166666666666666519, 0.3250000000000000111, 0.3333333333333333148, 0.3416666666666666741, 0.3499999999999999778, 0.3583333333333333370, 0.3666666666666666408, 0.3750000000000000000, 0.3833333333333333592, 0.3916666666666666630, 0.4000000000000000222, 0.4083333333333333259, 0.4166666666666666852, 0.4249999999999999889, 0.4333333333333333481, 0.4416666666666666519, 0.4500000000000000111, 0.4583333333333333148, 0.4666666666666666741, 0.4749999999999999778, 0.4833333333333333370, 0.4916666666666666408, 0.5000000000000000000, 0.5083333333333333037, 0.5166666666666667185, 0.5250000000000000222, 0.5333333333333333259, 0.5416666666666666297, 0.5500000000000000444, 0.5583333333333333481, 0.5666666666666666519, 0.5749999999999999556, 0.5833333333333333703, 0.5916666666666666741, 0.5999999999999999778, 0.6083333333333332815, 0.6166666666666666963, 0.6250000000000000000, 0.6333333333333333037, 0.6416666666666667185, 0.6500000000000000222, 0.6583333333333333259, 0.6666666666666666297, 0.6750000000000000444, 0.6833333333333333481, 0.6916666666666666519, 0.6999999999999999556, 0.7083333333333333703, 0.7166666666666666741, 0.7249999999999999778, 0.7333333333333332815, 0.7416666666666666963, 0.7500000000000000000, 0.7583333333333333037, 0.7666666666666667185, 0.7750000000000000222, 0.7833333333333333259, 0.7916666666666666297, 0.8000000000000000444, 0.8083333333333333481, 0.8166666666666666519, 0.8249999999999999556, 0.8333333333333333703, 0.8416666666666666741, 0.8499999999999999778, 0.8583333333333332815, 0.8666666666666666963, 0.8750000000000000000, 0.8833333333333333037, 0.8916666666666667185, 0.9000000000000000222, 0.9083333333333333259, 0.9166666666666666297, 0.9250000000000000444, 0.9333333333333333481, 0.9416666666666666519, 0.9499999999999999556, 0.9583333333333333703, 0.9666666666666666741, 0.9749999999999999778, 0.9833333333333332815, 0.9916666666666666963, 1.000000000000000000 ),
 .UNSPECIFIED. ) 
 GEOMETRIC_REPRESENTATION_ITEM ( )  RATIONAL_B_SPLINE_SURFACE ( (
 ( 1.000000000000000000, 0.8660254037844387076, 1.000000000000000000, 0.8660254037844387076, 1.000000000000000000, 0.8660254037844387076, 1.000000000000000000, 0.8660254037844387076, 1.000000000000000000, 0.8660254037844387076, 1.000000000000000000, 0.8660254037844387076, 1.000000000000000000, 0.8660254037844387076, 1.000000000000000000, 0.8660254037844387076, 1.000000000000000000, 0.8660254037844387076, 1.000000000000000000, 0.8660254037844387076, 1.000000000000000000, 0.8660254037844387076, 1.000000000000000000, 0.8660254037844387076, 1.000000000000000000, 0.8660254037844387076, 1.000000000000000000, 0.8660254037844387076, 1.000000000000000000, 0.8660254037844387076, 1.000000000000000000, 0.8660254037844387076, 1.000000000000000000, 0.8660254037844387076, 1.000000000000000000, 0.8660254037844387076, 1.000000000000000000, 0.8660254037844387076, 1.000000000000000000, 0.8660254037844387076, 1.000000000000000000, 0.8660254037844387076, 1.000000000000000000, 0.8660254037844387076, 1.000000000000000000, 0.8660254037844387076, 1.000000000000000000, 0.8660254037844387076, 1.000000000000000000, 0.8660254037844387076, 1.000000000000000000, 0.8660254037844387076, 1.000000000000000000, 0.8660254037844387076, 1.000000000000000000, 0.8660254037844387076, 1.000000000000000000, 0.8660254037844387076, 1.000000000000000000, 0.8660254037844387076, 1.000000000000000000, 0.8660254037844387076, 1.000000000000000000, 0.8660254037844387076, 1.000000000000000000, 0.8660254037844387076, 1.000000000000000000, 0.8660254037844387076, 1.000000000000000000, 0.8660254037844387076, 1.000000000000000000, 0.8660254037844387076, 1.000000000000000000, 0.8660254037844387076, 1.000000000000000000, 0.8660254037844387076, 1.000000000000000000, 0.8660254037844387076, 1.000000000000000000, 0.8660254037844387076, 1.000000000000000000, 0.8660254037844387076, 1.000000000000000000, 0.8660254037844387076, 1.000000000000000000, 0.8660254037844387076, 1.000000000000000000, 0.8660254037844387076, 1.000000000000000000, 0.8660254037844387076, 1.000000000000000000, 0.8660254037844387076, 1.000000000000000000, 0.8660254037844387076, 1.000000000000000000, 0.8660254037844387076, 1.000000000000000000, 0.8660254037844387076, 1.000000000000000000, 0.8660254037844387076, 1.000000000000000000, 0.8660254037844387076, 1.000000000000000000, 0.8660254037844387076, 1.000000000000000000, 0.8660254037844387076, 1.000000000000000000, 0.8660254037844387076, 1.000000000000000000, 0.8660254037844387076, 1.000000000000000000, 0.8660254037844387076, 1.000000000000000000, 0.8660254037844387076, 1.000000000000000000, 0.8660254037844387076, 1.000000000000000000, 0.8660254037844387076, 1.000000000000000000, 0.8660254037844387076, 1.000000000000000000, 0.8660254037844387076, 1.000000000000000000, 0.8660254037844387076, 1.000000000000000000, 0.8660254037844387076, 1.000000000000000000, 0.8660254037844387076, 1.000000000000000000, 0.8660254037844387076, 1.000000000000000000, 0.8660254037844387076, 1.000000000000000000, 0.8660254037844387076, 1.000000000000000000, 0.8660254037844387076, 1.000000000000000000, 0.8660254037844387076, 1.000000000000000000, 0.8660254037844387076, 1.000000000000000000, 0.8660254037844387076, 1.000000000000000000, 0.8660254037844387076, 1.000000000000000000, 0.8660254037844387076, 1.000000000000000000, 0.8660254037844387076, 1.000000000000000000, 0.8660254037844387076, 1.000000000000000000, 0.8660254037844387076, 1.000000000000000000, 0.8660254037844387076, 1.000000000000000000, 0.8660254037844387076, 1.000000000000000000, 0.8660254037844387076, 1.000000000000000000, 0.8660254037844387076, 1.000000000000000000, 0.8660254037844387076, 1.000000000000000000, 0.8660254037844387076, 1.000000000000000000, 0.8660254037844387076, 1.000000000000000000, 0.8660254037844387076, 1.000000000000000000, 0.8660254037844387076, 1.000000000000000000, 0.8660254037844387076, 1.000000000000000000, 0.8660254037844387076, 1.000000000000000000, 0.8660254037844387076, 1.000000000000000000, 0.8660254037844387076, 1.000000000000000000, 0.8660254037844387076, 1.000000000000000000, 0.8660254037844387076, 1.000000000000000000, 0.8660254037844387076, 1.000000000000000000, 0.8660254037844387076, 1.000000000000000000, 0.8660254037844387076, 1.000000000000000000, 0.8660254037844387076, 1.000000000000000000, 0.8660254037844387076, 1.000000000000000000, 0.8660254037844387076, 1.000000000000000000, 0.8660254037844387076, 1.000000000000000000, 0.8660254037844387076, 1.000000000000000000, 0.8660254037844387076, 1.000000000000000000, 0.8660254037844387076, 1.000000000000000000, 0.8660254037844387076, 1.000000000000000000, 0.8660254037844387076, 1.000000000000000000, 0.8660254037844387076, 1.000000000000000000, 0.8660254037844387076, 1.000000000000000000, 0.8660254037844387076, 1.000000000000000000, 0.8660254037844387076, 1.000000000000000000, 0.8660254037844387076, 1.000000000000000000, 0.8660254037844387076, 1.000000000000000000, 0.8660254037844387076, 1.000000000000000000, 0.8660254037844387076, 1.000000000000000000, 0.8660254037844387076, 1.000000000000000000, 0.8660254037844387076, 1.000000000000000000, 0.8660254037844387076, 1.000000000000000000, 0.8660254037844387076, 1.000000000000000000, 0.8660254037844387076, 1.000000000000000000, 0.8660254037844387076, 1.000000000000000000, 0.8660254037844387076, 1.000000000000000000, 0.8660254037844387076, 1.000000000000000000, 0.8660254037844387076, 1.000000000000000000),
 ( 1.000000000000000000, 0.8660254037844387076, 1.000000000000000000, 0.8660254037844387076, 1.000000000000000000, 0.8660254037844387076, 1.000000000000000000, 0.8660254037844387076, 1.000000000000000000, 0.8660254037844387076, 1.000000000000000000, 0.8660254037844387076, 1.000000000000000000, 0.8660254037844387076, 1.000000000000000000, 0.8660254037844387076, 1.000000000000000000, 0.8660254037844387076, 1.000000000000000000, 0.8660254037844387076, 1.000000000000000000, 0.8660254037844387076, 1.000000000000000000, 0.8660254037844387076, 1.000000000000000000, 0.8660254037844387076, 1.000000000000000000, 0.8660254037844387076, 1.000000000000000000, 0.8660254037844387076, 1.000000000000000000, 0.8660254037844387076, 1.000000000000000000, 0.8660254037844387076, 1.000000000000000000, 0.8660254037844387076, 1.000000000000000000, 0.8660254037844387076, 1.000000000000000000, 0.8660254037844387076, 1.000000000000000000, 0.8660254037844387076, 1.000000000000000000, 0.8660254037844387076, 1.000000000000000000, 0.8660254037844387076, 1.000000000000000000, 0.8660254037844387076, 1.000000000000000000, 0.8660254037844387076, 1.000000000000000000, 0.8660254037844387076, 1.000000000000000000, 0.8660254037844387076, 1.000000000000000000, 0.8660254037844387076, 1.000000000000000000, 0.8660254037844387076, 1.000000000000000000, 0.8660254037844387076, 1.000000000000000000, 0.8660254037844387076, 1.000000000000000000, 0.8660254037844387076, 1.000000000000000000, 0.8660254037844387076, 1.000000000000000000, 0.8660254037844387076, 1.000000000000000000, 0.8660254037844387076, 1.000000000000000000, 0.8660254037844387076, 1.000000000000000000, 0.8660254037844387076, 1.000000000000000000, 0.8660254037844387076, 1.000000000000000000, 0.8660254037844387076, 1.000000000000000000, 0.8660254037844387076, 1.000000000000000000, 0.8660254037844387076, 1.000000000000000000, 0.8660254037844387076, 1.000000000000000000, 0.8660254037844387076, 1.000000000000000000, 0.8660254037844387076, 1.000000000000000000, 0.8660254037844387076, 1.000000000000000000, 0.8660254037844387076, 1.000000000000000000, 0.8660254037844387076, 1.000000000000000000, 0.8660254037844387076, 1.000000000000000000, 0.8660254037844387076, 1.000000000000000000, 0.8660254037844387076, 1.000000000000000000, 0.8660254037844387076, 1.000000000000000000, 0.8660254037844387076, 1.000000000000000000, 0.8660254037844387076, 1.000000000000000000, 0.8660254037844387076, 1.000000000000000000, 0.8660254037844387076, 1.000000000000000000, 0.8660254037844387076, 1.000000000000000000, 0.8660254037844387076, 1.000000000000000000, 0.8660254037844387076, 1.000000000000000000, 0.8660254037844387076, 1.000000000000000000, 0.8660254037844387076, 1.000000000000000000, 0.8660254037844387076, 1.000000000000000000, 0.8660254037844387076, 1.000000000000000000, 0.8660254037844387076, 1.000000000000000000, 0.8660254037844387076, 1.000000000000000000, 0.8660254037844387076, 1.000000000000000000, 0.8660254037844387076, 1.000000000000000000, 0.8660254037844387076, 1.000000000000000000, 0.8660254037844387076, 1.000000000000000000, 0.8660254037844387076, 1.000000000000000000, 0.8660254037844387076, 1.000000000000000000, 0.8660254037844387076, 1.000000000000000000, 0.8660254037844387076, 1.000000000000000000, 0.8660254037844387076, 1.000000000000000000, 0.8660254037844387076, 1.000000000000000000, 0.8660254037844387076, 1.000000000000000000, 0.8660254037844387076, 1.000000000000000000, 0.8660254037844387076, 1.000000000000000000, 0.8660254037844387076, 1.000000000000000000, 0.8660254037844387076, 1.000000000000000000, 0.8660254037844387076, 1.000000000000000000, 0.8660254037844387076, 1.000000000000000000, 0.8660254037844387076, 1.000000000000000000, 0.8660254037844387076, 1.000000000000000000, 0.8660254037844387076, 1.000000000000000000, 0.8660254037844387076, 1.000000000000000000, 0.8660254037844387076, 1.000000000000000000, 0.8660254037844387076, 1.000000000000000000, 0.8660254037844387076, 1.000000000000000000, 0.8660254037844387076, 1.000000000000000000, 0.8660254037844387076, 1.000000000000000000, 0.8660254037844387076, 1.000000000000000000, 0.8660254037844387076, 1.000000000000000000, 0.8660254037844387076, 1.000000000000000000, 0.8660254037844387076, 1.000000000000000000, 0.8660254037844387076, 1.000000000000000000, 0.8660254037844387076, 1.000000000000000000, 0.8660254037844387076, 1.000000000000000000, 0.8660254037844387076, 1.000000000000000000, 0.8660254037844387076, 1.000000000000000000, 0.8660254037844387076, 1.000000000000000000, 0.8660254037844387076, 1.000000000000000000, 0.8660254037844387076, 1.000000000000000000, 0.8660254037844387076, 1.000000000000000000, 0.8660254037844387076, 1.000000000000000000, 0.8660254037844387076, 1.000000000000000000, 0.8660254037844387076, 1.000000000000000000, 0.8660254037844387076, 1.000000000000000000, 0.8660254037844387076, 1.000000000000000000, 0.8660254037844387076, 1.000000000000000000, 0.8660254037844387076, 1.000000000000000000, 0.8660254037844387076, 1.000000000000000000, 0.8660254037844387076, 1.000000000000000000, 0.8660254037844387076, 1.000000000000000000, 0.8660254037844387076, 1.000000000000000000, 0.8660254037844387076, 1.000000000000000000, 0.8660254037844387076, 1.000000000000000000, 0.8660254037844387076, 1.000000000000000000, 0.8660254037844387076, 1.000000000000000000, 0.8660254037844387076, 1.000000000000000000, 0.8660254037844387076, 1.000000000000000000) ) ) 
 REPRESENTATION_ITEM ( '' )  SURFACE ( )  );
#90966 = ADVANCED_FACE ( 'NONE', ( #158504 ), #92467, .F. ) ;
#90967 = CARTESIAN_POINT ( 'NONE',  ( 5.828598057497599960, -1.316348130051235410, 1.597988563933512074 ) ) ;
#90968 = CARTESIAN_POINT ( 'NONE',  ( -0.2409995289980038091, -0.004801160710915519658, -2.000252362011435636 ) ) ;
#90969 = AXIS2_PLACEMENT_3D ( 'NONE', #122459, #107245, #72528 ) ;
#90970 = CARTESIAN_POINT ( 'NONE',  ( -1.500000000000015099, -1.089583332650509773, -0.8660254037844383745 ) ) ;
#90971 = CARTESIAN_POINT ( 'NONE',  ( 4.107974109700462506, -1.921244671385572422, 0.1431019773510885384 ) ) ;
#90972 = CARTESIAN_POINT ( 'NONE',  ( -1.364683531250014514, 10.83854166700806942, -0.7879004041258335089 ) ) ;
#90973 = DIRECTION ( 'NONE',  ( 0.000000000000000000, 0.000000000000000000, -1.000000000000000000 ) ) ;
#90974 = CARTESIAN_POINT ( 'NONE',  ( 0.1413017363236251933, 2.128265657893123386, 0.6366465052881072895 ) ) ;
#90976 = ORIENTED_EDGE ( 'NONE', *, *, #96602, .F. ) ;
#90975 = DIRECTION ( 'NONE',  ( -0.000000000000000000, 1.000000000000000000, -0.000000000000000000 ) ) ;
#90979 = TOROIDAL_SURFACE ( 'NONE', #63289, 6.330000000000000959, 0.08000000000000000167 ) ;
#90978 = DIRECTION ( 'NONE',  ( 0.000000000000000000, 0.000000000000000000, 1.000000000000000000 ) ) ;
#90977 = CARTESIAN_POINT ( 'NONE',  ( -3.174017359375036929, 6.717120995997236221, 0.7216878364870338292 ) ) ;
#90980 = CARTESIAN_POINT ( 'NONE',  ( 9.622536337397022521, 12.24937836509514710, 1.599625672291281386 ) ) ;
#90981 = DIRECTION ( 'NONE',  ( -1.000000000000000000, 7.387867266669436732E-31, 0.000000000000000000 ) ) ;
#90982 = CARTESIAN_POINT ( 'NONE',  ( 3.895595285070167169, 2.800000000000017586, -0.7749999999999935829 ) ) ;
#90983 = CARTESIAN_POINT ( 'NONE',  ( 10.18181017373857600, 10.98112607889092907, 0.7216878364870438212 ) ) ;
#90984 = CARTESIAN_POINT ( 'NONE',  ( 0.8714495147512548723, -0.2914478312704605889, 1.939986204769503786 ) ) ;
#90985 = CARTESIAN_POINT ( 'NONE',  ( -1.364683531250000748, 1.821875000341421913, 0.000000000000000000 ) ) ;
#90986 = CARTESIAN_POINT ( 'NONE',  ( 0.000000000000000000, 0.000000000000000000, 0.000000000000000000 ) ) ;
#90987 = CARTESIAN_POINT ( 'NONE',  ( 5.213317179658601752, -1.656387821537348426, -1.051046178410528942 ) ) ;
#90988 = CARTESIAN_POINT ( 'NONE',  ( -8.320953590485107298, 10.73086516036454618, 1.599625672291269396 ) ) ;
#90989 = CARTESIAN_POINT ( 'NONE',  ( -5.382223794500843539, 7.302347065049529462, -1.443375672974051449 ) ) ;
#90990 = CARTESIAN_POINT ( 'NONE',  ( 6.819229411136438657, -0.1619093195798972928, 2.126376854085454404 ) ) ;
#90992 = ORIENTED_EDGE ( 'NONE', *, *, #134087, .F. ) ;
#90991 = CARTESIAN_POINT ( 'NONE',  ( -5.096975683733680818, 8.033889833409558534, -1.199719254218452047 ) ) ;
#90993 = CARTESIAN_POINT ( 'NONE',  ( 1.364683531249990311, 5.113541667008084879, 0.7879004041258500513 ) ) ;
#90994 = CARTESIAN_POINT ( 'NONE',  ( 0.6318452133688509109, 0.9670987946563678328, -1.601024004909731513 ) ) ;
#90995 = CARTESIAN_POINT ( 'NONE',  ( 0.2286474287733000488, 1.729290747967014097, 0.1301698663358965002 ) ) ;
#90996 = EDGE_CURVE ( 'NONE', #117856, #43490, #68122, .T. ) ;
#90998 = CARTESIAN_POINT ( 'NONE',  ( 4.071962858106247474, -1.261020321617589479, 1.792237525612811355 ) ) ;
#90997 = CARTESIAN_POINT ( 'NONE',  ( -5.358255402162534516E-14, 1.328125000341440431, -1.570758158831820239 ) ) ;
#90999 = CARTESIAN_POINT ( 'NONE',  ( 3.944573596103123414, 2.296136059628416604, 0.2296890760785547936 ) ) ;
#91000 = CARTESIAN_POINT ( 'NONE',  ( 0.2685257609614790097, -1.346659848514593305, 1.560126313484144545 ) ) ;
#91001 = CARTESIAN_POINT ( 'NONE',  ( 2.167823750104383773, -1.194498894885902329, 1.531050872003832497 ) ) ;
#91002 = CARTESIAN_POINT ( 'NONE',  ( -6.385527161912131433, 6.552129231760014605, 0.7216878364870317197 ) ) ;
#91003 = EDGE_CURVE ( 'NONE', #142577, #150798, #62074, .T. ) ;
#91004 = CARTESIAN_POINT ( 'NONE',  ( -0.4702634422474149534, 7.494255424139877775, -4.464191613397623826 ) ) ;
#91005 = CARTESIAN_POINT ( 'NONE',  ( 5.396778611113259849, -2.069399493756381769, -0.4625044129713885011 ) ) ;
#91006 = CARTESIAN_POINT ( 'NONE',  ( 0.6124999999999793943, 2.833333333333354354, 1.060881119635899816 ) ) ;
#91007 = CARTESIAN_POINT ( 'NONE',  ( 3.410779880581996437, -1.203353552534730309, -1.617818353255597863 ) ) ;
#91008 = CARTESIAN_POINT ( 'NONE',  ( -5.870317324592829067, 5.951051088220814300, -0.7216878364870197293 ) ) ;
#91009 = CARTESIAN_POINT ( 'NONE',  ( -5.935437387732586778, 10.14670372898850381, -0.7998128361456362523 ) ) ;
#91010 = CARTESIAN_POINT ( 'NONE',  ( 10.55910270694468345, 11.21337466772398095, 0.7998128361456462443 ) ) ;
#91011 = CARTESIAN_POINT ( 'NONE',  ( 1.189776066567624691, -0.8228614858879386151, 1.629801898503015156 ) ) ;
#91012 = CARTESIAN_POINT ( 'NONE',  ( -4.925354943514475003, 8.968274210734028529, 0.000000000000000000 ) ) ;
#91013 = CARTESIAN_POINT ( 'NONE',  ( -0.01853512708398871028, 15.45720132225713961, 11.97163374478179243 ) ) ;
#91014 = CARTESIAN_POINT ( 'NONE',  ( -9.968679514594425584, 5.546356146656833630, 6.001058933476985935 ) ) ;
#91015 = ORIENTED_EDGE ( 'NONE', *, *, #57465, .F. ) ;
#91016 = CARTESIAN_POINT ( 'NONE',  ( 5.893449486436047380, 1.558864155394885875, 1.348126965055055804 ) ) ;
#91017 = CARTESIAN_POINT ( 'NONE',  ( -7.404161286394468355, 7.810812053647902431, 0.000000000000000000 ) ) ;
#91018 = CARTESIAN_POINT ( 'NONE',  ( -0.7500000000000179856, 11.82291666734946389, 1.299038105676658228 ) ) ;
#91019 = CARTESIAN_POINT ( 'NONE',  ( -3.846762897975357198, 5.510976019103107859, -1.599625672291256295 ) ) ;
#91020 = CARTESIAN_POINT ( 'NONE',  ( -4.735978408342542245, 7.017321386899737057, 1.427696578792345683 ) ) ;
#91021 = CARTESIAN_POINT ( 'NONE',  ( 4.811197383834631580, 1.677940508811623710, -1.123774901704529317 ) ) ;
#91022 = CARTESIAN_POINT ( 'NONE',  ( 5.514381189547274076, -2.221473413594120760, -0.001881066846495804690 ) ) ;
#91024 = CARTESIAN_POINT ( 'NONE',  ( 7.931156674314368438, 12.19684052010138586, 1.040834085586084257E-14 ) ) ;
#91023 = CARTESIAN_POINT ( 'NONE',  ( -4.004454267989906668, 5.765225627445230927, 1.599625672291270506 ) ) ;
#91025 = CIRCLE ( 'NONE', #21695, 0.5000000000000004441 ) ;
#91026 = CARTESIAN_POINT ( 'NONE',  ( 5.469824908109481854, 8.468880595181346393, -1.199719254218446718 ) ) ;
#91027 = CARTESIAN_POINT ( 'NONE',  ( 3.942301955389547974, 2.050809467686238285, 0.2036389587714466376 ) ) ;
#91028 = CARTESIAN_POINT ( 'NONE',  ( 4.008435526009396455, -1.928752077057366732, 0.5880193435906442279 ) ) ;
#91029 = ORIENTED_EDGE ( 'NONE', *, *, #67872, .F. ) ;
#91030 = CARTESIAN_POINT ( 'NONE',  ( 11.86239285000045740, 13.88000000000000078, -1.812080536912752837 ) ) ;
#91031 = CARTESIAN_POINT ( 'NONE',  ( 4.111146893441827821, 5.819424013814004759, 1.599625672291267398 ) ) ;
#91032 =( BOUNDED_CURVE ( )  B_SPLINE_CURVE ( 2, ( #209642, #61283, #193415, #45058, #168374, #34102, #201903 ),
 .UNSPECIFIED., .F., .T. ) 
 B_SPLINE_CURVE_WITH_KNOTS ( ( 3, 2, 2, 3 ),
 ( 0.3999999999999997446, 0.4083333333333331039, 0.4166666666666665741, 0.4249999999999999334 ),
 .UNSPECIFIED. ) 
 CURVE ( )  GEOMETRIC_REPRESENTATION_ITEM ( )  RATIONAL_B_SPLINE_CURVE ( ( 1.000000000000004441, 0.8660254037844342667, 1.000000000000000000, 0.8660254037844387076, 1.000000000000000000, 0.8660254037844395958, 0.9999999999999991118 ) ) 
 REPRESENTATION_ITEM ( '' )  );
#91034 = ORIENTED_EDGE ( 'NONE', *, *, #73451, .T. ) ;
#91033 = CARTESIAN_POINT ( 'NONE',  ( -6.851666526859749418, 9.086973262793417661, -1.599625672291271394 ) ) ;
#91035 = CARTESIAN_POINT ( 'NONE',  ( 5.142555292688428814, 7.778213139218437711, -1.168464917166486039 ) ) ;
#91036 = CARTESIAN_POINT ( 'NONE',  ( 3.514999820297697308, 2.016288306963448296, 0.002811503506894295987 ) ) ;
#91037 = CARTESIAN_POINT ( 'NONE',  ( 2.712652182946372559, -0.1802803596865458491, 1.832282175343015407 ) ) ;
#91038 = CARTESIAN_POINT ( 'NONE',  ( 1.577271561783103460, -2.192461267746559361, -0.7203256085408450415 ) ) ;
#91039 = CARTESIAN_POINT ( 'NONE',  ( 8.154303043976348420, 8.478051404252736845, 0.7998128361456281477 ) ) ;
#91040 = CARTESIAN_POINT ( 'NONE',  ( 3.866626755795209203, -1.454868229745639008, 1.598846606682593929 ) ) ;
#91041 = CARTESIAN_POINT ( 'NONE',  ( -6.087774667736030487, 7.061157519568837415, 1.199719254218450271 ) ) ;
#91042 = CARTESIAN_POINT ( 'NONE',  ( 3.497717624726462748, 2.241670729410083940, 0.5068476239948813689 ) ) ;
#91043 = VERTEX_POINT ( 'NONE', #76177 ) ;
#91044 = DIRECTION ( 'NONE',  ( 0.000000000000000000, 0.000000000000000000, 1.000000000000000000 ) ) ;
#91045 = COLOUR_RGB ( '', 0.09019608, 0.27058824, 0.51372549) ;
#91046 = CARTESIAN_POINT ( 'NONE',  ( 2.113927203836548419, -0.8795192785214582809, -1.650985937663045577 ) ) ;
#91047 = CARTESIAN_POINT ( 'NONE',  ( 5.805538644497215017, -0.4794378417142564075, 1.912156289036368806 ) ) ;
#91049 = CARTESIAN_POINT ( 'NONE',  ( 9.856414487010592751, 10.60149777770828194, 0.7216878364870438212 ) ) ;
#91048 = CARTESIAN_POINT ( 'NONE',  ( 1.364683531249988535, 4.655208333674755394, -0.7879004041258300672 ) ) ;
#91051 = CARTESIAN_POINT ( 'NONE',  ( 0.2763675079364875664, 1.274320874971252460, 1.801605125401319007 ) ) ;
#91050 = CARTESIAN_POINT ( 'NONE',  ( -5.280010757518168063, 8.247430752824802980, -1.199719254218446718 ) ) ;
#91052 = DIRECTION ( 'NONE',  ( -1.000000000000000000, 0.000000000000000000, 0.000000000000000000 ) ) ;
#91053 = CARTESIAN_POINT ( 'NONE',  ( 4.330940004561544043, 7.140181541042074365, -1.199719254218452047 ) ) ;
#91054 = CARTESIAN_POINT ( 'NONE',  ( -6.423865854776591000, 6.388931673527803667, 1.040834085586084257E-14 ) ) ;
#91055 = CARTESIAN_POINT ( 'NONE',  ( 11.94105721237523277, 13.40000000000000036, 1.187919463087245386 ) ) ;
#91056 = CARTESIAN_POINT ( 'NONE',  ( 5.577018171352951192, -0.04780089932613153236, -1.971040553531088868 ) ) ;
#91057 = CARTESIAN_POINT ( 'NONE',  ( 5.461655971716653291, 0.4551397948197592469, -2.262217722918384410 ) ) ;
#91058 = CARTESIAN_POINT ( 'NONE',  ( 5.846130809274892925, -0.8361890816445856078, 1.662715158673214066 ) ) ;
#91059 = CARTESIAN_POINT ( 'NONE',  ( 3.537984270275731369, 1.304693584366970249, 1.597530370294945046 ) ) ;
#91060 = CARTESIAN_POINT ( 'NONE',  ( 5.802526556968819804, 9.713438716531550554, -0.7216878364870267237 ) ) ;
#91061 = AXIS2_PLACEMENT_3D ( 'NONE', #78944, #81090, #97364 ) ;
#91062 = CARTESIAN_POINT ( 'NONE',  ( 5.481239241674765950, 9.616805891921051952, -0.7998128361456481317 ) ) ;
#91063 = CARTESIAN_POINT ( 'NONE',  ( 6.114364089638782751, 9.116879957011832403, 1.082531754730558626 ) ) ;
#91064 = CARTESIAN_POINT ( 'NONE',  ( 1.364683531249988535, 3.717708333674750953, -0.7879004041258239610 ) ) ;
#91065 = CARTESIAN_POINT ( 'NONE',  ( -5.941061940081919346, 14.53065791113160365, 10.43603815422727443 ) ) ;
#91066 = CARTESIAN_POINT ( 'NONE',  ( 6.277061933002788585, 6.425586464699131639, 0.7216878364870317197 ) ) ;
#91068 = CARTESIAN_POINT ( 'NONE',  ( 2.993375309983861143, -0.3886322325962355273, 1.978555244300662874 ) ) ;
#91067 = CARTESIAN_POINT ( 'NONE',  ( 5.090355501040885855, 1.120491699331874536, -1.859593947532897973 ) ) ;
#91069 = CARTESIAN_POINT ( 'NONE',  ( 5.530750200611445067, -1.661959182355336795, 0.7928504710919548337 ) ) ;
#91071 = CARTESIAN_POINT ( 'NONE',  ( 6.620655732516647518, 0.5865983125455545011, 1.978983952526007339 ) ) ;
#91070 = CARTESIAN_POINT ( 'NONE',  ( -11.78331023100045449, 11.29999999999998117, 1.799999999999999600 ) ) ;
#91072 = CARTESIAN_POINT ( 'NONE',  ( 6.567925981381852907, -1.350348970527824211, 1.726830949945204363 ) ) ;
#91073 = CARTESIAN_POINT ( 'NONE',  ( 0.6670070365902281972, 0.1896921041569209765, -1.860926112923621201 ) ) ;
#91074 = CARTESIAN_POINT ( 'NONE',  ( 0.9489188801723142941, 0.6573868573102136237, 2.164820675142268058 ) ) ;
#91076 = CARTESIAN_POINT ( 'NONE',  ( -4.153809255294044434, 7.618134729639562508, -0.8777755718400248597 ) ) ;
#91075 = VECTOR ( 'NONE', #30527, 1000.000000000000000 ) ;
#91077 = SURFACE_SIDE_STYLE ('',( #143046 ) ) ;
#91078 = CARTESIAN_POINT ( 'NONE',  ( 6.536750166778501736, 6.811520125210166476, 0.4662371894542677864 ) ) ;
#91079 = CARTESIAN_POINT ( 'NONE',  ( -4.868786560638931782, 6.773613302202437403, 1.443375672974058777 ) ) ;
#91080 = CARTESIAN_POINT ( 'NONE',  ( 0.4164788467995068078, -0.6444665046171775824, -1.800526059235994403 ) ) ;
#91081 = CARTESIAN_POINT ( 'NONE',  ( 2.219294626563913297, -1.717429429511443173, 0.4269959701016200482 ) ) ;
#91082 = CARTESIAN_POINT ( 'NONE',  ( 5.320952465583661528, 1.522972439820569956, -1.316545952364375438 ) ) ;
#91083 = CARTESIAN_POINT ( 'NONE',  ( 4.645640190976921602, 8.571663989448405019, 1.040834085586084257E-14 ) ) ;
#91084 = CARTESIAN_POINT ( 'NONE',  ( 3.768672590584824178, -1.415924365303207644, 1.559078948506262385 ) ) ;
#91086 = CARTESIAN_POINT ( 'NONE',  ( 3.110843951327123325, 0.04995152196871639055, 1.915135415325731394 ) ) ;
#91085 = CARTESIAN_POINT ( 'NONE',  ( -4.419594887930571758, 4.258541578781506409, 1.214306433183764966E-14 ) ) ;
#91087 = CARTESIAN_POINT ( 'NONE',  ( 3.816783937446950770, 4.411668334231586996, 1.199719254218464037 ) ) ;
#91088 = CARTESIAN_POINT ( 'NONE',  ( 3.789471415310685654, -1.820739144500636231, 0.7515243927636706678 ) ) ;
#91089 = CARTESIAN_POINT ( 'NONE',  ( 0.2465380642357860586, 1.084720387836759725, -1.822023332652397354 ) ) ;
#91090 = CARTESIAN_POINT ( 'NONE',  ( -2.462777459176719308, 6.024990802348131780, -0.7998128361456281477 ) ) ;
#91091 = CARTESIAN_POINT ( 'NONE',  ( 2.711613914024712191, -1.850561042518297672, 0.2725550856255419818 ) ) ;
#91093 = VERTEX_POINT ( 'NONE', #143356 ) ;
#91092 = CARTESIAN_POINT ( 'NONE',  ( 5.584504578548418863, -1.684151958202559252, -0.3718293602123431962 ) ) ;
#91095 = CARTESIAN_POINT ( 'NONE',  ( 5.070386261830877928, 5.978167395966564435, -1.082531754730548412 ) ) ;
#91094 = CARTESIAN_POINT ( 'NONE',  ( 1.946200625105892312, 0.8427435547867198062, -2.039832142532324255 ) ) ;
#91096 = CARTESIAN_POINT ( 'NONE',  ( -1.201851678989727383E-14, 3.509375000341421469, -1.575800808251660134 ) ) ;
#91097 = CARTESIAN_POINT ( 'NONE',  ( 0.1333542156527478262, 0.001576319744088505292, -2.046049510433409768 ) ) ;
#91098 = CARTESIAN_POINT ( 'NONE',  ( 7.670162217029129259, 9.971608557999250166, 1.599625672291281386 ) ) ;
#91099 = CARTESIAN_POINT ( 'NONE',  ( 1.608462485350599769, 8.735270501766756013, 2.463594439587641904 ) ) ;
#91100 = CARTESIAN_POINT ( 'NONE',  ( -3.420040343843560926, -0.02845264914099391793, -0.3063276076694415595 ) ) ;
#91101 = VERTEX_POINT ( 'NONE', #209352 ) ;
#91102 = CARTESIAN_POINT ( 'NONE',  ( 7.752014238602739730E-16, 0.9200000000000041478, -6.329999999999995630 ) ) ;
#91103 = ORIENTED_EDGE ( 'NONE', *, *, #88030, .F. ) ;
#91104 = CARTESIAN_POINT ( 'NONE',  ( 2.172408243068229439, -0.9739482337229148357, -1.826950231780352762 ) ) ;
#91105 = CARTESIAN_POINT ( 'NONE',  ( 0.7499999999999885647, 3.566666666666690411, -1.299038105676658228 ) ) ;
#91106 = CARTESIAN_POINT ( 'NONE',  ( 6.636879889089462026, 7.701780277814560982, -1.199719254218446718 ) ) ;
#91107 = CARTESIAN_POINT ( 'NONE',  ( 3.902768115887398803, 5.646591783325653147, -1.599625672291269396 ) ) ;
#91108 = CARTESIAN_POINT ( 'NONE',  ( 6.322909428431959356, 1.571596504679906303, -1.423730336690950393 ) ) ;
#91109 = FILL_AREA_STYLE_COLOUR ( '', #170563 ) ;
#91110 = CARTESIAN_POINT ( 'NONE',  ( -0.6823417656249969321, 3.717708333674754506, -1.181850606188749264 ) ) ;
#91111 = CARTESIAN_POINT ( 'NONE',  ( 8.419250204406344196, 12.76628297187536809, 1.040834085586084257E-14 ) ) ;
#91112 = ADVANCED_FACE ( 'NONE', ( #214391 ), #13143, .T. ) ;
#91113 = CARTESIAN_POINT ( 'NONE',  ( 5.800157620552712778, -1.823839058171864203, 0.8595007112896931867 ) ) ;
#91114 = CARTESIAN_POINT ( 'NONE',  ( 5.014804717692854297, 0.1473437859633792701, 1.910143238840347868 ) ) ;
#91115 = CARTESIAN_POINT ( 'NONE',  ( -1.500000000000039524, 6.999999999999999112, -10.89724735885167739 ) ) ;
#91116 = CARTESIAN_POINT ( 'NONE',  ( 2.437293137456029157, -1.626093413141915134, -1.469474007205706645 ) ) ;
#91117 = CARTESIAN_POINT ( 'NONE',  ( 1.499999999999987121, 2.577083334016147198, -0.8660254037844262731 ) ) ;
#91118 = CARTESIAN_POINT ( 'NONE',  ( 1.863391182279940494, -1.538030936729195552, -1.136358088520472931 ) ) ;
#91119 = CARTESIAN_POINT ( 'NONE',  ( -5.392392409933270514, 7.314210449720692786, 1.599625672291269396 ) ) ;
#91120 = CARTESIAN_POINT ( 'NONE',  ( 6.222275945484236459, 2.094208529755392068, 0.3105017025616888526 ) ) ;
#91121 = CARTESIAN_POINT ( 'NONE',  ( 0.6823417656249969321, 10.08854166700806587, -1.181850606188757036 ) ) ;
#91123 = CARTESIAN_POINT ( 'NONE',  ( -5.956828388357799042, 8.042995434541133193, 1.599625672291263179 ) ) ;
#91122 = CARTESIAN_POINT ( 'NONE',  ( 2.982061477060811150, -2.060241282245252048, -0.3548380112704754286 ) ) ;
#91125 = ORIENTED_EDGE ( 'NONE', *, *, #118482, .F. ) ;
#91124 = CARTESIAN_POINT ( 'NONE',  ( 2.643205280608558194, -1.276243157467608302, -1.160367288944160968 ) ) ;
#91126 = CARTESIAN_POINT ( 'NONE',  ( 6.539320575229233157, 0.001224430076711413356, 2.103502572931112091 ) ) ;
#91127 = CARTESIAN_POINT ( 'NONE',  ( 4.852928918687680948, 7.749168607522574526, 1.199719254218462483 ) ) ;
#91128 = EDGE_CURVE ( 'NONE', #128658, #80820, #143518, .T. ) ;
#91129 = FACE_BOUND ( 'NONE', #173153, .T. ) ;
#91130 = DIRECTION ( 'NONE',  ( 0.000000000000000000, -1.000000000000000000, 0.000000000000000000 ) ) ;
#91131 = CARTESIAN_POINT ( 'NONE',  ( 11.52888687719590521, 9.805768748949638791, -3.331331986263459388 ) ) ;
#91132 = CARTESIAN_POINT ( 'NONE',  ( 5.575427483717746213, 7.527751369135936343, 1.599625672291267398 ) ) ;
#91133 = ORIENTED_EDGE ( 'NONE', *, *, #130231, .F. ) ;
#91135 = TOROIDAL_SURFACE ( 'NONE', #118839, 0.05000000000000000278, 0.05000000000000000278 ) ;
#91134 = CARTESIAN_POINT ( 'NONE',  ( -11.89839339040395316, 13.82877468403921561, -1.560885614203537219 ) ) ;
#91136 = ORIENTED_EDGE ( 'NONE', *, *, #185057, .T. ) ;
#91137 = CARTESIAN_POINT ( 'NONE',  ( 3.035611470257699285, -1.745090209790541191, 0.4855505718092138490 ) ) ;
#91138 = EDGE_LOOP ( 'NONE', ( #103274, #40046, #171802, #90759, #185544, #102981, #195169, #114957, #24236, #18417, #106699, #210794, #64303 ) ) ;
#91139 = CARTESIAN_POINT ( 'NONE',  ( 8.191097360950562845, 12.70803068775103739, -0.7998128361456352531 ) ) ;
#91140 = PRESENTATION_LAYER_ASSIGNMENT (  '', '', ( #118843 ) ) ;
#91141 = CARTESIAN_POINT ( 'NONE',  ( 4.923546060418115822, 5.773167154356443120, -1.199719254218452047 ) ) ;
#91142 = CARTESIAN_POINT ( 'NONE',  ( 3.932113804724958417, -0.9344168170181254007, -1.551720482391373057 ) ) ;
#91143 = CARTESIAN_POINT ( 'NONE',  ( 6.539320575229292665, 7.052829955583200139, 2.594893642179775028 ) ) ;
#91144 = CARTESIAN_POINT ( 'NONE',  ( -10.99665086521320490, -7.860092950639682385, 0.2746580110251921614 ) ) ;
#91145 = CARTESIAN_POINT ( 'NONE',  ( 5.846986258851572416, 6.004518191619921730, 0.3586427151269864222 ) ) ;
#91146 = ADVANCED_FACE ( 'NONE', ( #120193 ), #168065, .T. ) ;
#91148 = CARTESIAN_POINT ( 'NONE',  ( 1.364683531249997417, 14.73437500034140157, 2.602085213965210642E-15 ) ) ;
#91147 = CARTESIAN_POINT ( 'NONE',  ( 4.316758383393053400, -1.379848157930125829, 1.249026149535825914 ) ) ;
#91149 = EDGE_CURVE ( 'NONE', #123257, #89199, #42494, .T. ) ;
#91150 = CARTESIAN_POINT ( 'NONE',  ( 1.300237133077002394, 1.285435684207901774, -1.420472988465313557 ) ) ;
#91151 = CARTESIAN_POINT ( 'NONE',  ( 1.254616015376356586, -1.441780481750528420, 1.119729341354458452 ) ) ;
#91152 = CARTESIAN_POINT ( 'NONE',  ( 4.764469552112262640, 8.169203124620777245, 0.7669358090897534508 ) ) ;
#91153 = CARTESIAN_POINT ( 'NONE',  ( -10.56580427165518721, 4.154138811340903459, -5.596901375327959727 ) ) ;
#91154 =( GEOMETRIC_REPRESENTATION_CONTEXT ( 3 ) GLOBAL_UNCERTAINTY_ASSIGNED_CONTEXT ( ( #114474 ) ) GLOBAL_UNIT_ASSIGNED_CONTEXT ( ( #130764, #143792, #127592 ) ) REPRESENTATION_CONTEXT ( 'NONE', 'WORKASPACE' ) );
#91155 = CARTESIAN_POINT ( 'NONE',  ( 4.990887655837901171, 7.926359819171765686, 1.063311220390166234 ) ) ;
#91156 = DIRECTION ( 'NONE',  ( 0.000000000000000000, -2.190088388420720976E-12, -1.000000000000000000 ) ) ;
#91157 = CARTESIAN_POINT ( 'NONE',  ( -10.99944088594793179, -9.904389777384739801, 0.1109062511178791205 ) ) ;
#91158 = CARTESIAN_POINT ( 'NONE',  ( 7.795575138177731844, 8.197185204069915798, 1.040834085586084257E-14 ) ) ;
#91159 = CARTESIAN_POINT ( 'NONE',  ( 6.174653332693735841, 1.325436276047034179, -1.456821488112548080 ) ) ;
#91160 = CARTESIAN_POINT ( 'NONE',  ( -3.228813138348844536, 6.918699094715619502, 0.7998128361456341429 ) ) ;
#91161 = CARTESIAN_POINT ( 'NONE',  ( 11.86145016429272836, 12.69999999999999929, -1.100000000000000311 ) ) ;
#91162 = CARTESIAN_POINT ( 'NONE',  ( 1.535224857807856669, -1.515203476157600537, -1.440707689706053563 ) ) ;
#91163 = CARTESIAN_POINT ( 'NONE',  ( 0.1822601575737579360, -1.769359155225664226, -0.4491840103194589817 ) ) ;
#91164 = CARTESIAN_POINT ( 'NONE',  ( -6.013204822860843457, 6.974159367214481264, -1.199719254218446718 ) ) ;
#91165 = CARTESIAN_POINT ( 'NONE',  ( 1.377666516899571647, 1.084121917808708035, 1.468671923017292658 ) ) ;
#91166 = CARTESIAN_POINT ( 'NONE',  ( 3.088704478669739739, -2.174299887604825177, -0.3769171259565203269 ) ) ;
#91167 = CARTESIAN_POINT ( 'NONE',  ( 0.4019237886466816012, 9.957585450998168497, -1.499999999999998668 ) ) ;
#91168 = CARTESIAN_POINT ( 'NONE',  ( 1.195406425308798148, 1.765864799226088744, -0.7346160280939582066 ) ) ;
#91169 = CARTESIAN_POINT ( 'NONE',  ( 1.926157630473192217, 1.009716079121532495, 1.690873403599216562 ) ) ;
#91170 = CARTESIAN_POINT ( 'NONE',  ( 2.753386078659710190, 1.932462020465589125, -0.1930240951200749566 ) ) ;
#91171 = EDGE_LOOP ( 'NONE', ( #52566, #200084, #176905, #202778 ) ) ;
#91172 = DIRECTION ( 'NONE',  ( 0.000000000000000000, -1.000000000000000000, 0.000000000000000000 ) ) ;
#91174 = CARTESIAN_POINT ( 'NONE',  ( 0.2384088454224670139, -1.803645845812065440, -0.4582378156636581767 ) ) ;
#91173 = CARTESIAN_POINT ( 'NONE',  ( -6.140917232347002042, 6.129101290685087911, -0.7998128361456362523 ) ) ;
#91175 = CARTESIAN_POINT ( 'NONE',  ( 5.194709132691408549, 6.089524072008651423, 1.199719254218452935 ) ) ;
#91176 = CARTESIAN_POINT ( 'NONE',  ( -11.41108574530281494, 13.75836855377625589, -3.405883542057589253 ) ) ;
#91177 = CARTESIAN_POINT ( 'NONE',  ( 8.374132434735052755, 12.92157160716627295, -0.7998128361456352531 ) ) ;
#91178 = CARTESIAN_POINT ( 'NONE',  ( -4.613517410400161722, 8.604463755433990002, -0.7998128361456362523 ) ) ;
#91179 = CARTESIAN_POINT ( 'NONE',  ( 2.120887600855193345, 0.003649250790785373531, 2.191739723551556551 ) ) ;
#91180 = CARTESIAN_POINT ( 'NONE',  ( -1.115562610750309283E-14, 11.59375000068279604, 1.500000000000001554 ) ) ;
#91181 = CARTESIAN_POINT ( 'NONE',  ( 4.028709946750490545, 3.988235255965033588, -0.8025987720412866011 ) ) ;
#91182 = CARTESIAN_POINT ( 'NONE',  ( 2.824607995650964209, 1.719152210223941823, 0.6149139946348627372 ) ) ;
#91183 = CARTESIAN_POINT ( 'NONE',  ( -2.252626078164912560, 5.779814191167667481, 0.7998128361456341429 ) ) ;
#91184 = CARTESIAN_POINT ( 'NONE',  ( -4.595593225409446703, 8.485229224138180371, -0.2149309537713070539 ) ) ;
#91185 = CARTESIAN_POINT ( 'NONE',  ( 0.000000000000000000, -0.5000000000000004441, 0.000000000000000000 ) ) ;
#91186 = CARTESIAN_POINT ( 'NONE',  ( 7.944187942603509356, 11.35563746875774882, 1.199719254218460707 ) ) ;
#91187 = CARTESIAN_POINT ( 'NONE',  ( 1.945805723040757051, 0.7375614711745586138, -1.779911670397672951 ) ) ;
#91188 = CARTESIAN_POINT ( 'NONE',  ( 5.998874280538830206, 0.3792253423284037139, 1.924579554046601970 ) ) ;
#91189 = CARTESIAN_POINT ( 'NONE',  ( 1.499999999999993117, 15.35416666666666430, 0.8660254037844409281 ) ) ;
#91190 = CARTESIAN_POINT ( 'NONE',  ( -8.227100285394159940, 8.492705175914988303, 0.7998128361456602331 ) ) ;
#91191 = CARTESIAN_POINT ( 'NONE',  ( 4.521807925357579805, 5.234196320127330715, -1.199719254218452047 ) ) ;
#91192 = CARTESIAN_POINT ( 'NONE',  ( -5.194182247366913252, 7.153241603385088965, 1.443375672974058777 ) ) ;
#91193 = PRESENTATION_LAYER_ASSIGNMENT (  '', '', ( #187945 ) ) ;
#91194 = STYLED_ITEM ( 'NONE', ( #21876 ), #114086 ) ;
#91195 = CARTESIAN_POINT ( 'NONE',  ( -2.129434811653636128, 5.532128030284154008, 1.040834085586084257E-14 ) ) ;
#91196 = CARTESIAN_POINT ( 'NONE',  ( -2.765500147507697459, 5.209872024525476597, 1.082531754730560403 ) ) ;
#91197 = CARTESIAN_POINT ( 'NONE',  ( 5.207906454484914072, 0.6546344234062730916, -1.964071172066352400 ) ) ;
#91199 = CARTESIAN_POINT ( 'NONE',  ( 0.6823417656249899377, 2.405208333674753618, 1.181850606188767472 ) ) ;
#91198 = CARTESIAN_POINT ( 'NONE',  ( -2.189868734255737248, 1.000000000000000888, 11.69137891449146771 ) ) ;
#91200 = AXIS2_PLACEMENT_3D ( 'NONE', #151981, #3555, #69626 ) ;
#91201 = CARTESIAN_POINT ( 'NONE',  ( 5.502642741134641469, -2.243371634331346343, 0.5006679109763980673 ) ) ;
#91202 = CARTESIAN_POINT ( 'NONE',  ( 7.809133291791403586, 8.213003049952529722, -0.7216878364870257245 ) ) ;
#91204 = DIRECTION ( 'NONE',  ( 0.000000000000000000, 0.000000000000000000, -1.000000000000000000 ) ) ;
#91203 = CARTESIAN_POINT ( 'NONE',  ( 6.224601922449876312, 6.434659462379210382, 0.000000000000000000 ) ) ;
#91205 = CARTESIAN_POINT ( 'NONE',  ( 0.7621917111494004304, 1.134545731666029011, 1.991736209811171054 ) ) ;
#91206 = CARTESIAN_POINT ( 'NONE',  ( 7.465774003072942477, -6.268611901546733201, -7.465774003072967346 ) ) ;
#91207 = CARTESIAN_POINT ( 'NONE',  ( -7.449279056065764237, 7.655523418356991350, 0.7998128361456341429 ) ) ;
#91208 = CARTESIAN_POINT ( 'NONE',  ( 4.716706857919571227, -0.09384406936703558466, 1.939798966779549882 ) ) ;
#91209 = ORIENTED_EDGE ( 'NONE', *, *, #129599, .F. ) ;
#91210 = CARTESIAN_POINT ( 'NONE',  ( 7.565086526301031178, 11.76975868075249387, 1.040834085586084257E-14 ) ) ;
#91211 = EDGE_CURVE ( 'NONE', #11785, #136413, #35276, .T. ) ;
#91212 = PRESENTATION_LAYER_ASSIGNMENT (  '', '', ( #191040 ) ) ;
#91213 = EDGE_LOOP ( 'NONE', ( #196628, #3709, #83516, #9751, #190866 ) ) ;
#91214 = CARTESIAN_POINT ( 'NONE',  ( 5.888906298306328502, -1.818048641159516476, -0.5935555146628914702 ) ) ;
#91215 = CARTESIAN_POINT ( 'NONE',  ( 6.106443901014584341, -0.6257089282217034309, -1.607472872393211683 ) ) ;
#91216 = CARTESIAN_POINT ( 'NONE',  ( 5.401577436481666439, -1.966305606708594667, 0.4464985920552416720 ) ) ;
#91218 = CARTESIAN_POINT ( 'NONE',  ( -4.502716413514313842, 5.386162249589033557, -1.082531754730549967 ) ) ;
#91217 = CARTESIAN_POINT ( 'NONE',  ( -7.343712760096452463, 11.71941532008788833, -0.7998128361456291469 ) ) ;
#91219 = CARTESIAN_POINT ( 'NONE',  ( 0.000000000000000000, -0.9843749995220403282, -3.793834371823813001 ) ) ;
#91221 = CARTESIAN_POINT ( 'NONE',  ( 0.3558548230270657808, 0.6711484630133063289, 1.637870061858819559 ) ) ;
#91220 = CARTESIAN_POINT ( 'NONE',  ( 1.253981223613403806, 0.8486778832286197005, 1.910818189544212675 ) ) ;
#91222 = CARTESIAN_POINT ( 'NONE',  ( 6.346327303948391396, 0.3419391630616851474, -1.987045965717588958 ) ) ;
#91223 = MANIFOLD_SOLID_BREP ( 'Cut-Extrude2', #126141 ) ;
#91225 = CARTESIAN_POINT ( 'NONE',  ( 2.959215247630428536, 0.3357152255929369278, -2.267430770885081603 ) ) ;
#91224 = CARTESIAN_POINT ( 'NONE',  ( 5.246079093845007257, 5.085123462432798114, 0.7998128361456352531 ) ) ;
#91226 = CARTESIAN_POINT ( 'NONE',  ( 2.062088869592033635, -1.590637294955974390, -0.7065417998822677292 ) ) ;
#91227 = CARTESIAN_POINT ( 'NONE',  ( 1.250000000000037526, 8.500000000000000000, 10.85702537530423406 ) ) ;
#91228 = CARTESIAN_POINT ( 'NONE',  ( 2.530263549637286502, 1.701127810229096982, -0.3340974653274173534 ) ) ;
#91229 = CARTESIAN_POINT ( 'NONE',  ( 1.360316468749987129, 1.796875000341410900, -3.295974604355933479E-14 ) ) ;
#91230 = CARTESIAN_POINT ( 'NONE',  ( 1.644728535064543529, -0.2685211301156094632, -1.841439677390522389 ) ) ;
#91231 = CARTESIAN_POINT ( 'NONE',  ( 2.629531826656985150, 0.1086732114553476541, -2.168588674111065817 ) ) ;
#91232 = CARTESIAN_POINT ( 'NONE',  ( 3.678922940808615483, 1.700962499606586853, -1.082838980105811366 ) ) ;
#91233 = CARTESIAN_POINT ( 'NONE',  ( 3.562500000000002665, -1.451031289061261109, -1.451031289060973561 ) ) ;
#91234 = CARTESIAN_POINT ( 'NONE',  ( -0.7500000000000215383, 2.722916667349486897, 1.299038105676671107 ) ) ;
#91235 = CARTESIAN_POINT ( 'NONE',  ( 0.6570953225405625764, -1.625623130003026606, -1.033337472089399078 ) ) ;
#91236 = CARTESIAN_POINT ( 'NONE',  ( -0.6823417656250039265, 14.56770833367473195, -1.181850606188755259 ) ) ;
#91237 = CARTESIAN_POINT ( 'NONE',  ( 3.498459270752065198, -1.092227124545399164, 1.934249878339290740 ) ) ;
#91238 = ORIENTED_EDGE ( 'NONE', *, *, #32090, .F. ) ;
#91239 = CARTESIAN_POINT ( 'NONE',  ( 3.570880328030153539, 7.341005539872356600, 0.2896471194287209006 ) ) ;
#91240 = CARTESIAN_POINT ( 'NONE',  ( 1.499999999999987121, 1.045833333333352266, -0.8660254037844253849 ) ) ;
#91241 = CARTESIAN_POINT ( 'NONE',  ( 7.775764792637399836, 9.030479331953833011, -1.199719254218441611 ) ) ;
#91242 = CARTESIAN_POINT ( 'NONE',  ( -0.6823417656250246877, -0.4489583329919111243, 1.181850606188755259 ) ) ;
#91243 = CARTESIAN_POINT ( 'NONE',  ( 5.713180276867825924, 1.816287534895771216, -1.278698279616990563 ) ) ;
#91244 = CARTESIAN_POINT ( 'NONE',  ( 5.037533845850875380, 1.831247050742194515, -0.7043679133837479345 ) ) ;
#91246 = CARTESIAN_POINT ( 'NONE',  ( -4.934804725694212912, 8.701096580044490381, -0.7216878364870207285 ) ) ;
#91245 = CARTESIAN_POINT ( 'NONE',  ( 9.747949258545622442, 10.47495501116581984, 0.000000000000000000 ) ) ;
#91247 = DIRECTION ( 'NONE',  ( 0.000000000000000000, -1.000000000000000000, 0.000000000000000000 ) ) ;
#91248 = CARTESIAN_POINT ( 'NONE',  ( 5.606774309801295431, 1.718512474747270868, -1.471603694038286836 ) ) ;
#91249 = CARTESIAN_POINT ( 'NONE',  ( -5.858531774880906262, 6.967946837850073294, 1.082531754730549078 ) ) ;
#91250 = CARTESIAN_POINT ( 'NONE',  ( 2.717292478832333380, -1.793364790446878798, -1.018969015592002592 ) ) ;
#91251 = CARTESIAN_POINT ( 'NONE',  ( -5.880485940025243607, 7.883652901494672349, 1.599625672291269396 ) ) ;
#91252 = ORIENTED_EDGE ( 'NONE', *, *, #16807, .F. ) ;
#91253 = CARTESIAN_POINT ( 'NONE',  ( -1.402160292154681736E-14, 2.618750000682819490, -1.732050807568863648 ) ) ;
#91254 = CARTESIAN_POINT ( 'NONE',  ( -1.364683531249997417, 4.321875000341417028, 1.214306433183764966E-14 ) ) ;
#91255 = CARTESIAN_POINT ( 'NONE',  ( 5.360568611784803927, -1.355617963529401893, 1.289147430649554948 ) ) ;
#91256 = CARTESIAN_POINT ( 'NONE',  ( 3.146783715800211212, 0.7824046571166408670, 1.547702628640304168 ) ) ;
#91257 = CARTESIAN_POINT ( 'NONE',  ( 2.594910355399903334, -0.5442454861351472273, 1.653239653166445278 ) ) ;
#91258 = EDGE_CURVE ( 'NONE', #93052, #3985, #117328, .T. ) ;
#91259 = CARTESIAN_POINT ( 'NONE',  ( 0.8555022099123296142, 0.4403784002881392379, -2.249529875239093979 ) ) ;
#91260 = CARTESIAN_POINT ( 'NONE',  ( 1.448561363430532989, 2.204290700723564811, 0.1073905156721635390 ) ) ;
#91261 = CARTESIAN_POINT ( 'NONE',  ( 4.950766902526997804, -1.767019275552136115, -1.117201988274316049 ) ) ;
#91262 = CARTESIAN_POINT ( 'NONE',  ( 5.771417317170061345, 1.158396453637217993, 1.558476049558398913 ) ) ;
#91264 = ORIENTED_EDGE ( 'NONE', *, *, #5833, .F. ) ;
#91263 = CARTESIAN_POINT ( 'NONE',  ( 7.471411487236919058, 15.41976068137822153, 9.339997063786253051 ) ) ;
#91265 = CARTESIAN_POINT ( 'NONE',  ( 2.500000000000002220, -1.483785425626877107E-13, -2.052068128417949389 ) ) ;
#91266 = CARTESIAN_POINT ( 'NONE',  ( 0.1060925565549031974, -0.09613213100253051313, 2.014232862735332308 ) ) ;
#91267 = FILL_AREA_STYLE_COLOUR ( '', #92808 ) ;
#91268 = SURFACE_STYLE_USAGE ( .BOTH. , #42521 ) ;
#91269 = FILL_AREA_STYLE_COLOUR ( '', #183331 ) ;
#91270 = CARTESIAN_POINT ( 'NONE',  ( -9.338868881714763148, 9.789768538289042255, -0.7998128361456291469 ) ) ;
#91271 = CARTESIAN_POINT ( 'NONE',  ( 6.982612806237943559, 8.105135347821125436, -1.199719254218446718 ) ) ;
#91272 = CARTESIAN_POINT ( 'NONE',  ( -5.249999999999987566, 0.000000000000000000, 0.5999999999999969802 ) ) ;
#91274 = EDGE_CURVE ( 'NONE', #183707, #83007, #50138, .T. ) ;
#91273 = CARTESIAN_POINT ( 'NONE',  ( 4.846238042176662653, 1.821038859956089606, 0.1311717439725426648 ) ) ;
#91275 = CARTESIAN_POINT ( 'NONE',  ( 2.432911661931828284, 2.140371652790736601, 0.5367425311649312025 ) ) ;
#91276 = EDGE_LOOP ( 'NONE', ( #177257, #51126, #125280, #117349 ) ) ;
#91277 = CARTESIAN_POINT ( 'NONE',  ( -4.977251789548269301, 4.979417640660637190, 0.7216878364870257245 ) ) ;
#91278 = CARTESIAN_POINT ( 'NONE',  ( -4.516801452008150086, 5.298631777878131111, 1.199719254218452935 ) ) ;
#91279 = CARTESIAN_POINT ( 'NONE',  ( 0.000000000000000000, -2.384374999522042238, -3.793834371823813001 ) ) ;
#91280 = CARTESIAN_POINT ( 'NONE',  ( -7.542413527904030524, 7.693903958843159252, 1.040834085586084257E-14 ) ) ;
#91281 = CARTESIAN_POINT ( 'NONE',  ( 1.195576078702242473, 1.864576247583774160, -0.7769579012074608881 ) ) ;
#91282 = CARTESIAN_POINT ( 'NONE',  ( 0.7124089920921555796, 14.00000000000000711, -12.66466791154696381 ) ) ;
#91283 = CARTESIAN_POINT ( 'NONE',  ( -5.309953438407606363, 6.223975762010839574, 1.199719254218452935 ) ) ;
#91284 = CARTESIAN_POINT ( 'NONE',  ( 2.500643731865523023, 0.4022941478849762498, 1.816780921579076225 ) ) ;
#91285 = CARTESIAN_POINT ( 'NONE',  ( 10.71502147350184231, 11.39527989537399755, 0.000000000000000000 ) ) ;
#91286 = FACE_OUTER_BOUND ( 'NONE', #176695, .T. ) ;
#91287 = VERTEX_POINT ( 'NONE', #39949 ) ;
#91288 = ORIENTED_EDGE ( 'NONE', *, *, #209517, .T. ) ;
#91289 = CARTESIAN_POINT ( 'NONE',  ( -5.278201874421821316, 5.052323696447222900, 0.7998128361456341429 ) ) ;
#91290 = AXIS2_PLACEMENT_3D ( 'NONE', #174764, #105493, #72947 ) ;
#91291 = CARTESIAN_POINT ( 'NONE',  ( -7.621654909176601045, 12.04368116068139472, 0.7998128361456481317 ) ) ;
#91292 = CARTESIAN_POINT ( 'NONE',  ( 4.283705427790140519, 1.194290084605063251, 1.380960126487425166 ) ) ;
#91294 = CARTESIAN_POINT ( 'NONE',  ( -4.904330467487477918, 6.873893772473251396, -1.448588590679427801 ) ) ;
#91293 = CARTESIAN_POINT ( 'NONE',  ( -5.327428015527048366, 5.180030537728460338, -0.7998128361456362523 ) ) ;
#91295 = CARTESIAN_POINT ( 'NONE',  ( 5.959663945170571075, 7.214374732172471383, -1.219933935757764099 ) ) ;
#91296 = CARTESIAN_POINT ( 'NONE',  ( 1.123892771930210754, 0.3453300891937352568, -1.698893503174392139 ) ) ;
#91297 = CARTESIAN_POINT ( 'NONE',  ( 5.701068745948241201, -0.4431999317857804876, 1.786873912291174538 ) ) ;
#91298 = CARTESIAN_POINT ( 'NONE',  ( 4.793776464392771608, 1.707650450486393190, 1.552408976560351483 ) ) ;
#91299 = CARTESIAN_POINT ( 'NONE',  ( 5.713835393516482952, 5.630839145382857680, 0.7998128361456352531 ) ) ;
#91300 = CARTESIAN_POINT ( 'NONE',  ( 0.5091468516268854438, 1.791808316595304040, 1.017857635437851904 ) ) ;
#91301 = CARTESIAN_POINT ( 'NONE',  ( 5.378365493435281586, -0.3450152841970657858, 2.272265683862843666 ) ) ;
#91302 = CARTESIAN_POINT ( 'NONE',  ( 0.000000000000000000, 0.000000000000000000, -0.5000000000000004441 ) ) ;
#91303 = CARTESIAN_POINT ( 'NONE',  ( -5.340986169140711226, 5.195848383611072485, 0.000000000000000000 ) ) ;
#91304 = ADVANCED_FACE ( 'NONE', ( #139595 ), #184877, .T. ) ;
#91305 = CARTESIAN_POINT ( 'NONE',  ( 6.034044788248046132, 0.9204803733943857091, -1.628451883209979689 ) ) ;
#91306 = EDGE_LOOP ( 'NONE', ( #168600, #842, #211931, #177980 ) ) ;
#91308 = CARTESIAN_POINT ( 'NONE',  ( -4.634908411025374875, 6.500755460986618495, 1.599625672291263179 ) ) ;
#91307 = CARTESIAN_POINT ( 'NONE',  ( 2.970861089138316036, -1.445268511421276214, 1.252435071843561731 ) ) ;
#91309 = CARTESIAN_POINT ( 'NONE',  ( 4.319099500008596770, 2.017107695584336557, 0.8957252843501888329 ) ) ;
#91310 = CARTESIAN_POINT ( 'NONE',  ( 4.839118085652931001, -1.790413437384326789, -1.129994989630648261 ) ) ;
#91311 = CARTESIAN_POINT ( 'NONE',  ( -0.6125000000000383471, 0.7708333340161397373, -1.060881119635972647 ) ) ;
#91312 = CARTESIAN_POINT ( 'NONE',  ( -9.719212163200577237, 3.553054704878167325, 6.967211938571212571 ) ) ;
#91313 = CARTESIAN_POINT ( 'NONE',  ( -0.2110808730067144090, 0.2462152545684419269, -1.831495465910786269 ) ) ;
#91314 = CARTESIAN_POINT ( 'NONE',  ( 6.007671464186837618, 6.181573927739029806, 0.7216878364870328300 ) ) ;
#91315 = CARTESIAN_POINT ( 'NONE',  ( -5.438229012412899799, 7.437962829272074750, -1.443375672974066548 ) ) ;
#91316 = CARTESIAN_POINT ( 'NONE',  ( 1.905729856612170758, 1.919199136376721793, 1.280985070478329435 ) ) ;
#91317 = CARTESIAN_POINT ( 'NONE',  ( 3.174217076811707727, -0.9646401420641316227, -1.708233030250068785 ) ) ;
#91318 = CARTESIAN_POINT ( 'NONE',  ( -6.120580001926503755, 6.105374521861167025, -0.7998128361456361413 ) ) ;
#91319 = CARTESIAN_POINT ( 'NONE',  ( 6.403195902773025416, -1.745507933166186465, 1.098531482539546023 ) ) ;
#91320 = CARTESIAN_POINT ( 'NONE',  ( 4.555176424511575561, 4.416720038126027426, -0.7216878364870188411 ) ) ;
#91321 = CARTESIAN_POINT ( 'NONE',  ( 5.076602173674213070, 4.887400388900169368, 0.000000000000000000 ) ) ;
#91322 = ORIENTED_EDGE ( 'NONE', *, *, #210558, .F. ) ;
#91323 = CARTESIAN_POINT ( 'NONE',  ( 4.786342355033275986, -0.6839347017603314427, -1.897111394664739326 ) ) ;
#91324 = CARTESIAN_POINT ( 'NONE',  ( -9.429859533504656000, 10.96025652963230534, -1.199719254218441611 ) ) ;
#91325 = DIRECTION ( 'NONE',  ( -1.000000000000000000, 0.000000000000000000, 0.000000000000000000 ) ) ;
#91326 = CARTESIAN_POINT ( 'NONE',  ( -10.57232049882948388, 5.599334429189661400, -4.968988939937085014 ) ) ;
#91327 = CARTESIAN_POINT ( 'NONE',  ( 7.574201371528760163, 11.98831870009225931, 1.040834085586084257E-14 ) ) ;
#91328 = CARTESIAN_POINT ( 'NONE',  ( 2.008858235458183650, 0.6779177425604805407, 2.062613225174831921 ) ) ;
#91329 = CARTESIAN_POINT ( 'NONE',  ( 4.881097632946307385, 6.623252254984194565, 1.537733183400882053 ) ) ;
#91330 = FACE_OUTER_BOUND ( 'NONE', #59944, .T. ) ;
#91331 = SURFACE_SIDE_STYLE ('',( #169352 ) ) ;
#91332 = CARTESIAN_POINT ( 'NONE',  ( 4.710809438828709617, 8.349644928513606956, 0.6747337923850562635 ) ) ;
#91333 = CARTESIAN_POINT ( 'NONE',  ( 0.8958617733694884677, -0.7443198534227279950, 1.921839338364476513 ) ) ;
#91335 = CARTESIAN_POINT ( 'NONE',  ( 6.727182134110243794, 2.977085856046020051, 2.364561739503980853 ) ) ;
#91334 = CARTESIAN_POINT ( 'NONE',  ( -0.02224634325196857970, 6.946779003630102700, -2.884187630258818302 ) ) ;
#91336 = CARTESIAN_POINT ( 'NONE',  ( -1.364683531250012516, 0.5302083336747518416, 0.7879004041258379498 ) ) ;
#91337 = CARTESIAN_POINT ( 'NONE',  ( 0.000000000000000000, 15.51887838114830132, 0.000000000000000000 ) ) ;
#91338 = ORIENTED_EDGE ( 'NONE', *, *, #62182, .F. ) ;
#91339 = CARTESIAN_POINT ( 'NONE',  ( 3.158751774003202950, 0.4669426847015486493, 1.854258104404989060 ) ) ;
#91340 = CARTESIAN_POINT ( 'NONE',  ( 4.838602548666761649, 0.3042620993840873811, 1.743309385229721675 ) ) ;
#91341 = CARTESIAN_POINT ( 'NONE',  ( 5.176180785367283654, 9.260904359562321275, -0.7998128361456481317 ) ) ;
#91342 = CARTESIAN_POINT ( 'NONE',  ( -3.415764635639130020, 6.072476943965863683, 1.199719254218462483 ) ) ;
#91343 = CARTESIAN_POINT ( 'NONE',  ( 6.468375100207775397, -1.879703733780390795, -0.3681822884963186215 ) ) ;
#91344 = CARTESIAN_POINT ( 'NONE',  ( -1.500000000000013101, -0.07916666666664513852, 0.8660254037844403729 ) ) ;
#91345 = CARTESIAN_POINT ( 'NONE',  ( 1.100149375694438714, 0.8407228983892693908, -1.892171374333020406 ) ) ;
#91346 = CARTESIAN_POINT ( 'NONE',  ( 1.499999999999991118, 5.754166666666685970, 0.8660254037844524744 ) ) ;
#91347 = CARTESIAN_POINT ( 'NONE',  ( 6.491075539335432687, 1.626419376453295706, -0.9240138038444989377 ) ) ;
#91348 = CARTESIAN_POINT ( 'NONE',  ( 2.051128252772801641, -1.465761996925791122, -1.088229512710245261 ) ) ;
#91350 = CARTESIAN_POINT ( 'NONE',  ( 5.264264421420239870, 7.666326994050936428, 1.218248458220503094 ) ) ;
#91349 = CARTESIAN_POINT ( 'NONE',  ( 5.690102719724574598, -0.9953569382129350274, 1.969734210959340093 ) ) ;
#91351 = CARTESIAN_POINT ( 'NONE',  ( -1.364683531250000748, 0.2593750003414205252, 0.000000000000000000 ) ) ;
#91352 = CARTESIAN_POINT ( 'NONE',  ( 3.525881619439541037, 2.013048741316531220, -0.4491155694474731619 ) ) ;
#91354 = CARTESIAN_POINT ( 'NONE',  ( -5.689618019229208734, 9.789638122409414223, 0.7998128361456481317 ) ) ;
#91353 = CIRCLE ( 'NONE', #4839, 1.250000000000000000 ) ;
#91355 = CARTESIAN_POINT ( 'NONE',  ( 7.730120138085914583, 12.17022392774227768, 0.7998128361456462443 ) ) ;
#91356 = CARTESIAN_POINT ( 'NONE',  ( 5.301401758143367893, 6.143722458377430584, 1.199719254218462483 ) ) ;
#91357 = CARTESIAN_POINT ( 'NONE',  ( 0.5093243970649004027, 1.880507610096779025, 1.065828983023514809 ) ) ;
#91358 = CARTESIAN_POINT ( 'NONE',  ( 7.517069824134078537, 7.734612647770044092, 0.000000000000000000 ) ) ;
#91359 = CARTESIAN_POINT ( 'NONE',  ( 5.160626937512653001, -0.6942339714755951796, -1.950645400549338104 ) ) ;
#91361 = CARTESIAN_POINT ( 'NONE',  ( -1.402160292154681736E-14, 0.009375000341421267647, -1.575800808251665908 ) ) ;
#91360 = CIRCLE ( 'NONE', #115648, 0.09999999999999990841 ) ;
#91362 = CARTESIAN_POINT ( 'NONE',  ( 3.339309863714147397, -1.908069850993234340, 1.015702806061814734 ) ) ;
#91363 = CARTESIAN_POINT ( 'NONE',  ( -4.617805310829839804, 8.366410568267871994, -0.2388493967704352627 ) ) ;
#91365 = CARTESIAN_POINT ( 'NONE',  ( 2.471086628630547288, 1.751123931924388089, 0.8847596551376719631 ) ) ;
#91364 = CARTESIAN_POINT ( 'NONE',  ( 3.527994226718012438, -1.989412488823691483, 0.3473740275561196245 ) ) ;
#91366 = CARTESIAN_POINT ( 'NONE',  ( 6.720655732516641834, 7.051887106169240305, 2.771889904330120391 ) ) ;
#91369 = CARTESIAN_POINT ( 'NONE',  ( 6.968527767744109980, 7.232296605230681408, 0.7216878364870317197 ) ) ;
#91368 = CARTESIAN_POINT ( 'NONE',  ( 3.475000000000000533, -1.225000000000000311, 0.000000000000000000 ) ) ;
#91367 = CARTESIAN_POINT ( 'NONE',  ( -1.500000000000051514, 3.702083334016151639, 0.8660254037844170583 ) ) ;
#91370 = EDGE_CURVE ( 'NONE', #78339, #149147, #189382, .T. ) ;
#91371 = CARTESIAN_POINT ( 'NONE',  ( -6.282224075085783177, 8.422623735723785643, 1.599625672291269396 ) ) ;
#91372 = CARTESIAN_POINT ( 'NONE',  ( 1.007046422456716384, -0.04465021774549028655, 2.016188868504041665 ) ) ;
#91374 = CARTESIAN_POINT ( 'NONE',  ( 5.882419586753741214, -0.3201050945752722532, -2.167950725039065052 ) ) ;
#91373 = CARTESIAN_POINT ( 'NONE',  ( -5.742041750587549842, 6.657802449562273850, 1.199719254218450271 ) ) ;
#91375 = CARTESIAN_POINT ( 'NONE',  ( 5.653386866774130937, 5.697965554099072349, -0.7216878364870402685 ) ) ;
#91376 = CARTESIAN_POINT ( 'NONE',  ( 5.818603510220927255, -0.6945032022064903110, -1.782003016414166252 ) ) ;
#91377 = CARTESIAN_POINT ( 'NONE',  ( -11.95359438121989548, 12.49578100291300586, 1.059536798430472437 ) ) ;
#91378 = CARTESIAN_POINT ( 'NONE',  ( 4.975479186090852046, 6.827811688571220117, 1.443375672974062551 ) ) ;
#91380 = CARTESIAN_POINT ( 'NONE',  ( 3.620720401301917857, 0.2986476686686300175, 1.994069442355271615 ) ) ;
#91379 = CARTESIAN_POINT ( 'NONE',  ( -8.148087131688692253, 10.52918762510205042, -1.443375672974058777 ) ) ;
#91381 = CARTESIAN_POINT ( 'NONE',  ( -1.500000000000011324, 3.420833333333355597, 0.8660254037844403729 ) ) ;
#91382 = CARTESIAN_POINT ( 'NONE',  ( -1.402160292154681736E-14, 13.73437500034139624, 1.575800808251682339 ) ) ;
#91383 = CARTESIAN_POINT ( 'NONE',  ( 0.02935885042023527250, -1.056071399167260783, -1.364091372971764748 ) ) ;
#91384 = CARTESIAN_POINT ( 'NONE',  ( 6.875920180786008196, 8.050936961452347163, -1.199719254218452047 ) ) ;
#91385 = CARTESIAN_POINT ( 'NONE',  ( 7.456621297836061757, 11.64321591421002644, 0.7216878364870438212 ) ) ;
#91386 = CARTESIAN_POINT ( 'NONE',  ( 10.99943594186085782, -9.910930717204459839, -0.1113955156348795106 ) ) ;
#91387 = CARTESIAN_POINT ( 'NONE',  ( 4.551927186349598031, 1.870183863439809357, -0.04390777100237578529 ) ) ;
#91388 = ORIENTED_EDGE ( 'NONE', *, *, #173163, .F. ) ;
#91389 = CARTESIAN_POINT ( 'NONE',  ( 2.571216573722459486, 1.847313327574741315, 0.9347662400437593000 ) ) ;
#91390 = CARTESIAN_POINT ( 'NONE',  ( -7.065207446052809814, 9.336104335185325453, -1.443375672974066548 ) ) ;
#91391 = ORIENTED_EDGE ( 'NONE', *, *, #54763, .F. ) ;
#91392 = CARTESIAN_POINT ( 'NONE',  ( 5.713835393516482952, 5.630839145382857680, 0.7998128361456352531 ) ) ;
#91393 = CARTESIAN_POINT ( 'NONE',  ( -0.1351500440973339712, -0.1486198258836557429, -1.983738523497140305 ) ) ;
#91394 = CARTESIAN_POINT ( 'NONE',  ( -0.0001156980946178872989, -0.8540272384012604912, 1.597593110781750925 ) ) ;
#91395 = CARTESIAN_POINT ( 'NONE',  ( 3.892599500454941630, 6.595097612955829192, 1.082531754730549078 ) ) ;
#91396 = LINE ( 'NONE', #155308, #86901 ) ;
#91397 = ORIENTED_EDGE ( 'NONE', *, *, #52034, .F. ) ;
#91398 = EDGE_CURVE ( 'NONE', #8134, #83982, #174578, .T. ) ;
#91399 = CARTESIAN_POINT ( 'NONE',  ( 7.741342523278686549, 11.97539067722642869, 0.7216878364870438212 ) ) ;
#91401 = CARTESIAN_POINT ( 'NONE',  ( 7.618792255875527886, 10.97600916757510170, 1.199719254218460707 ) ) ;
#91400 = CARTESIAN_POINT ( 'NONE',  ( 2.189831975649577878, -1.279155337443920404, -1.487614327915102841 ) ) ;
#91402 = CARTESIAN_POINT ( 'NONE',  ( 5.501554071977204252, -1.867810700675033297, 0.4244617614653464766 ) ) ;
#91403 = CARTESIAN_POINT ( 'NONE',  ( -11.33772465723237666, 13.50868300734826377, 3.600000000000073364 ) ) ;
#91404 = CARTESIAN_POINT ( 'NONE',  ( 5.192409644353875642, 5.160158794608717514, 1.040834085586084257E-14 ) ) ;
#91405 = CARTESIAN_POINT ( 'NONE',  ( 9.642873567817520808, 12.27310513391906532, 1.599625672291279388 ) ) ;
#91407 = VERTEX_POINT ( 'NONE', #174232 ) ;
#91406 = CARTESIAN_POINT ( 'NONE',  ( 5.070386261830877928, 5.978167395966564435, -1.082531754730548412 ) ) ;
#91408 = CARTESIAN_POINT ( 'NONE',  ( -7.456621297836087514, 9.722477485607340597, 1.443375672974090751 ) ) ;
#91409 = CARTESIAN_POINT ( 'NONE',  ( 2.676834871759771417, -2.068302492614528365, -0.6285112194897370941 ) ) ;
#91410 = CARTESIAN_POINT ( 'NONE',  ( -7.024532985656169792, 9.288650798055913427, 1.443375672974064550 ) ) ;
#91411 = CARTESIAN_POINT ( 'NONE',  ( 3.390420931869152721, 6.113185632892752075, -1.199719254218452047 ) ) ;
#91412 = CARTESIAN_POINT ( 'NONE',  ( -2.442440228756222353, 6.001264033524212671, -0.7998128361456281477 ) ) ;
#91413 = CARTESIAN_POINT ( 'NONE',  ( 5.491160184941096922, 1.609068807629027820, -0.8623064814072267659 ) ) ;
#91414 = CARTESIAN_POINT ( 'NONE',  ( 8.892465212752345138, 12.91714147110841893, 7.587471063468475663 ) ) ;
#91415 = CARTESIAN_POINT ( 'NONE',  ( 0.8078137629249462215, -1.962250697097242869, 0.1890654564427676487 ) ) ;
#91416 = CARTESIAN_POINT ( 'NONE',  ( 4.025576834063953946, -0.3218090080209669024, 1.884953445776993863 ) ) ;
#91417 = ORIENTED_EDGE ( 'NONE', *, *, #52471, .F. ) ;
#91418 = CARTESIAN_POINT ( 'NONE',  ( -3.023105066167323329, 5.702484939155337607, -2.420000000000000373 ) ) ;
#91419 = CARTESIAN_POINT ( 'NONE',  ( 4.809023018811155126, -1.583041700261601958, 1.171600654023413624 ) ) ;
#91420 = ORIENTED_EDGE ( 'NONE', *, *, #178139, .F. ) ;
#91421 = CARTESIAN_POINT ( 'NONE',  ( 6.093304272135602773, -0.6500253571345508963, 1.830188593850643697 ) ) ;
#91422 = ORIENTED_EDGE ( 'NONE', *, *, #67115, .T. ) ;
#91423 = CARTESIAN_POINT ( 'NONE',  ( -6.608673532018475960, 6.674816973635147477, -0.7998128361456362523 ) ) ;
#91425 = CARTESIAN_POINT ( 'NONE',  ( -1.225000000000056044, 1.291666667349482323, -0.7072540797573317883 ) ) ;
#91424 = CARTESIAN_POINT ( 'NONE',  ( -5.204350862799341115, 7.165104988056252289, -1.599625672291271394 ) ) ;
#91426 = CARTESIAN_POINT ( 'NONE',  ( 7.146556367734764770, 9.431011410480991231, 1.443375672974063439 ) ) ;
#91428 = ORIENTED_EDGE ( 'NONE', *, *, #32207, .F. ) ;
#91427 = CARTESIAN_POINT ( 'NONE',  ( 3.387273370026026686, 0.04433669930821101945, -1.911926451916061476 ) ) ;
#91429 = CARTESIAN_POINT ( 'NONE',  ( 0.4818276840582723652, 2.058231501447155054, -0.7964225590989246761 ) ) ;
#91430 = CARTESIAN_POINT ( 'NONE',  ( 7.653681110113487840, -5.402328468025356933, 7.847520364415523808 ) ) ;
#91431 = CARTESIAN_POINT ( 'NONE',  ( 5.953776513178359764, -1.459723235216038750, -1.386512712134661207 ) ) ;
#91432 = CARTESIAN_POINT ( 'NONE',  ( 0.07278863622976063097, 7.008482404162149848, 2.000259058016622404 ) ) ;
#91434 = CARTESIAN_POINT ( 'NONE',  ( 5.577361344084559747, 1.530155114678043660, 1.313547687611632764 ) ) ;
#91433 = CARTESIAN_POINT ( 'NONE',  ( 6.375623774462673587, 1.745513195383348926, -0.5351242734627087438 ) ) ;
#91435 = CARTESIAN_POINT ( 'NONE',  ( 1.856005582152659317, -0.6995316168164237292, 1.948720873434762080 ) ) ;
#91436 = CARTESIAN_POINT ( 'NONE',  ( -5.201524489137236529, 9.220195670635433771, 0.7998128361456481317 ) ) ;
#91437 = CARTESIAN_POINT ( 'NONE',  ( -5.178050853460543834, 7.761234873892349562, -1.181743852105126669 ) ) ;
#91438 = FACE_OUTER_BOUND ( 'NONE', #128554, .T. ) ;
#91439 = CARTESIAN_POINT ( 'NONE',  ( 6.649288223980674317, -1.503899034092892162, -1.112267350887645945 ) ) ;
#91440 = CARTESIAN_POINT ( 'NONE',  ( 5.823390672269506574, 6.752709524857930745, -1.199719254218446718 ) ) ;
#91441 = CARTESIAN_POINT ( 'NONE',  ( 5.885648082108200896, 6.039213315313952002, 0.7216878364870328300 ) ) ;
#91442 = DIRECTION ( 'NONE',  ( 0.000000000000000000, 1.000000000000000000, 0.000000000000000000 ) ) ;
#91443 = CARTESIAN_POINT ( 'NONE',  ( -1.402160292154681736E-14, 12.23437500034140335, 1.575800808251682339 ) ) ;
#91445 = CARTESIAN_POINT ( 'NONE',  ( -6.794571259104023930, 7.956029886156682274, 1.199719254218452047 ) ) ;
#91444 = CARTESIAN_POINT ( 'NONE',  ( 6.825078400183554272, 2.980425674467934272, 2.309322343017068402 ) ) ;
#91446 = CARTESIAN_POINT ( 'NONE',  ( 5.045445647265833777, -1.250780835746621245, 1.201444140469201782 ) ) ;
#91447 = CLOSED_SHELL ( 'NONE', ( #188068, #77352, #142307, #19046, #89919, #32794, #145814, #119715, #14252, #122793, #117118, #208300, #111109, #207292, #88815, #77664, #44092, #44544, #69369, #88253, #71022, #155335, #135470, #139719, #76054, #102969, #113293, #74424, #201053, #32526, #192557, #147018, #85728, #21731, #160611, #56177, #174383, #177442, #114977, #13122, #184840, #137460, #117749, #22092, #170995, #211724, #39492, #2681, #124225, #212685, #15144, #212331, #133053, #2572, #47747, #203384, #154771, #165444, #80056, #82320, #22541, #123645, #97037, #128250, #63624, #173885, #117453, #180058, #73015, #123995, #88283, #48153, #151834, #136948, #111821, #91146, #21534, #181414, #28766, #10022, #121506, #14684, #125472, #38814, #54280, #197402, #67772, #105264, #79392, #56627, #94082, #83107, #144876, #114460, #132984, #122158, #163826, #75093, #19817 ) ) ;
#91448 = CARTESIAN_POINT ( 'NONE',  ( -3.567766978690493307, 7.314145241780881435, 1.040834085586084257E-14 ) ) ;
#91449 = CARTESIAN_POINT ( 'NONE',  ( 2.817306709214098870, -1.799057772339835548, -1.024303335033532658 ) ) ;
#91450 = CARTESIAN_POINT ( 'NONE',  ( 3.392305424709577188, -0.8603400307676151160, -1.934732246027433433 ) ) ;
#91451 = CARTESIAN_POINT ( 'NONE',  ( 7.949158136313996259, 8.168439335321471262, 1.040834085586084257E-14 ) ) ;
#91452 = CARTESIAN_POINT ( 'NONE',  ( 0.3423093779010028537, 2.999999999999988898, 0.3423093779009768189 ) ) ;
#91453 = CARTESIAN_POINT ( 'NONE',  ( 2.149204315396076481, 1.716066119659308331, -0.9661483248721688399 ) ) ;
#91454 = CARTESIAN_POINT ( 'NONE',  ( 5.975483201341563522, 6.103571115010600678, 0.6665044388154163224 ) ) ;
#91456 = DIRECTION ( 'NONE',  ( -0.1674078377058430267, 0.000000000000000000, 0.9858877298529756805 ) ) ;
#91455 = CARTESIAN_POINT ( 'NONE',  ( -3.474999999999998312, -1.720833333333333881, 2.006292185433951047 ) ) ;
#91457 = CARTESIAN_POINT ( 'NONE',  ( 3.574455624386526420, -2.209025962754256334, -0.6118928016028857275 ) ) ;
#91458 = CARTESIAN_POINT ( 'NONE',  ( 1.769861954154128725, 0.9373860217288846330, 1.566528536362868707 ) ) ;
#91459 = CARTESIAN_POINT ( 'NONE',  ( 3.867818961648523235, 7.734482231890414283, 1.040834085586084257E-14 ) ) ;
#91460 = CARTESIAN_POINT ( 'NONE',  ( 6.114364089638786304, 8.156510742710487705, 1.443375672974076540 ) ) ;
#91461 = CARTESIAN_POINT ( 'NONE',  ( -8.019811557683421910, 9.315200557840817908, 1.199719254218462483 ) ) ;
#91462 = EDGE_CURVE ( 'NONE', #8253, #112831, #99182, .T. ) ;
#91463 = CARTESIAN_POINT ( 'NONE',  ( 2.970950383256478755, -1.521771678934441097, 1.318087423592265717 ) ) ;
#91464 = CARTESIAN_POINT ( 'NONE',  ( 1.903102209365503894, -1.660057620245494636, 1.045011325395063251 ) ) ;
#91465 = CARTESIAN_POINT ( 'NONE',  ( -7.483210719738908168, 10.81783070874899799, 1.199719254218453823 ) ) ;
#91466 = CARTESIAN_POINT ( 'NONE',  ( -5.377780486114890124, 9.425827667109372143, 0.000000000000000000 ) ) ;
#91467 = CARTESIAN_POINT ( 'NONE',  ( 0.07536363704235479744, 6.947016338497881804, -2.739277465201896078 ) ) ;
#91469 = CARTESIAN_POINT ( 'NONE',  ( 4.838602548666761649, 0.3042620993840873811, 1.743309385229721675 ) ) ;
#91468 = CARTESIAN_POINT ( 'NONE',  ( 5.507793336809221785, -0.9391204764703815489, -1.867914344430561702 ) ) ;
#91470 = CARTESIAN_POINT ( 'NONE',  ( -7.247736482492992849, 15.00000000000182077, 10.57961706324680584 ) ) ;
#91471 = STYLED_ITEM ( 'NONE', ( #66076 ), #7315 ) ;
#91472 = CARTESIAN_POINT ( 'NONE',  ( 1.095947417326826212, -2.191629467406099430, 0.003159298377679311057 ) ) ;
#91473 = CARTESIAN_POINT ( 'NONE',  ( 5.982304607080743963, -0.2621144554034166574, -1.720346425911468469 ) ) ;
#91474 = CARTESIAN_POINT ( 'NONE',  ( 7.751511138711133064, 10.06651563329490529, -1.599625672291262513 ) ) ;
#91475 = DIRECTION ( 'NONE',  ( 0.6292706268317891372, -0.7771862570881751253, 0.000000000000000000 ) ) ;
#91476 = CARTESIAN_POINT ( 'NONE',  ( 6.223268877717999636, 2.273007049229976761, 0.3419319510214839930 ) ) ;
#91477 = CARTESIAN_POINT ( 'NONE',  ( 2.970281070238892873, 6.580799555089337893, 0.4329187822878322600 ) ) ;
#91478 = CARTESIAN_POINT ( 'NONE',  ( 5.817694146727262705, -1.364776552785733399, 1.069276891063369650 ) ) ;
#91479 = CARTESIAN_POINT ( 'NONE',  ( 6.197752310581432056, -1.568275824509495875, -1.501738253884659979 ) ) ;
#91480 = CARTESIAN_POINT ( 'NONE',  ( 2.171277156482887882, 5.684907115872006145, -0.7998128361456291469 ) ) ;
#91481 = CARTESIAN_POINT ( 'NONE',  ( -0.08258987484092288056, -1.932961894807160963, 0.8646260017347202620 ) ) ;
#91482 = CARTESIAN_POINT ( 'NONE',  ( 2.968750000000002220, 0.7852924748298364399, -1.895863743164148074 ) ) ;
#91483 = CARTESIAN_POINT ( 'NONE',  ( 0.000000000000000000, 3.466143782776612170, 0.000000000000000000 ) ) ;
#91484 = CARTESIAN_POINT ( 'NONE',  ( 4.014609399936463596, 1.362939121162042078, -1.361637018764590534 ) ) ;
#91485 = CARTESIAN_POINT ( 'NONE',  ( 1.499999999999993117, 10.63541666734946212, 0.8660254037844409281 ) ) ;
#91486 = CARTESIAN_POINT ( 'NONE',  ( 0.6807244054014843782, 1.099941690210548106, 1.929793933578232146 ) ) ;
#91487 = EDGE_LOOP ( 'NONE', ( #102868, #1073, #63778, #108205, #100446 ) ) ;
#91488 = CARTESIAN_POINT ( 'NONE',  ( -1.500000000000011324, 4.170833333333359150, 0.8660254037844403729 ) ) ;
#91489 = CARTESIAN_POINT ( 'NONE',  ( 3.985207087413062066, 6.736826471035503694, -1.199719254218452047 ) ) ;
#91490 = CARTESIAN_POINT ( 'NONE',  ( 7.305145839664861640, 7.417091655897478653, 0.7998128361456341429 ) ) ;
#91491 = CARTESIAN_POINT ( 'NONE',  ( 2.122025409673257812, -0.4832278914180427876, 2.167962204723080433 ) ) ;
#91492 = CARTESIAN_POINT ( 'NONE',  ( -9.056483424248693126, 10.62861408545402675, 1.082531754730558626 ) ) ;
#91493 = DIRECTION ( 'NONE',  ( 1.000000000000000000, -0.000000000000000000, -0.000000000000000000 ) ) ;
#91494 = CARTESIAN_POINT ( 'NONE',  ( 5.666945020832160118, 9.555260257705446847, 0.7216878364870438212 ) ) ;
#91495 = CARTESIAN_POINT ( 'NONE',  ( -8.636180661780658241, 12.05899929117736846, -1.082531754730543083 ) ) ;
#91496 = AXIS2_PLACEMENT_3D ( 'NONE', #143407, #176935, #208346 ) ;
#91497 = CARTESIAN_POINT ( 'NONE',  ( 5.695833931516881776, 9.659240330162777610, -0.7216878364870458196 ) ) ;
#91498 = CARTESIAN_POINT ( 'NONE',  ( 0.6685925339881376717, 1.356301626434471164, 1.492253803477984642 ) ) ;
#91500 = CARTESIAN_POINT ( 'NONE',  ( 6.338341894567316892, -1.106718111279564543, 1.740473967980406655 ) ) ;
#91499 = CARTESIAN_POINT ( 'NONE',  ( 8.269583629331492602, 11.73526576994040482, 1.199719254218450271 ) ) ;
#91501 = DIRECTION ( 'NONE',  ( 0.000000000000000000, -1.000000000000000000, 0.000000000000000000 ) ) ;
#91502 = CARTESIAN_POINT ( 'NONE',  ( 7.336370518326124746, 7.731722824234849689, -0.7216878364870317197 ) ) ;
#91503 = AXIS2_PLACEMENT_3D ( 'NONE', #56503, #22901, #43473 ) ;
#91504 = CARTESIAN_POINT ( 'NONE',  ( -1.201851678989727383E-14, 1.071875000341418138, 1.575800808251672791 ) ) ;
#91505 = CARTESIAN_POINT ( 'NONE',  ( 1.932500037753889455, 0.1674293521093522530, 1.761778154814014119 ) ) ;
#91506 = CARTESIAN_POINT ( 'NONE',  ( 0.2642963535325442703, 1.880433764241522088, -0.7283817610406128074 ) ) ;
#91507 = CARTESIAN_POINT ( 'NONE',  ( 5.618645907585640309, -0.03427301787072359329, 1.740288698465036976 ) ) ;
#91508 = EDGE_CURVE ( 'NONE', #31530, #213643, #195432, .T. ) ;
#91509 = CARTESIAN_POINT ( 'NONE',  ( 4.054423531099146771, -1.698574802010197837, 1.539571537138052948 ) ) ;
#91510 = CARTESIAN_POINT ( 'NONE',  ( 0.6823417656249882723, -0.4072916663252490466, 1.181850606188755259 ) ) ;
#91511 = B_SPLINE_CURVE_WITH_KNOTS ( 'NONE', 3,
 ( #165489, #53885, #116801, #100490 ),
 .UNSPECIFIED., .F., .F.,
 ( 4, 4 ),
 ( 6.034005962831002237E-05, 0.0001895969026200594165 ),
 .UNSPECIFIED. ) ;
#91512 = CARTESIAN_POINT ( 'NONE',  ( 2.554438963407625884, -1.601868926591401232, -0.9074879233003438905 ) ) ;
#91513 = CARTESIAN_POINT ( 'NONE',  ( 9.398826802771546696, 11.98838390803207865, -1.599625672291262513 ) ) ;
#91514 = DIRECTION ( 'NONE',  ( 0.000000000000000000, -1.000000000000000000, 0.000000000000000000 ) ) ;
#91515 = CARTESIAN_POINT ( 'NONE',  ( 2.907047201455060570, 1.541221212934189344, 0.9781624729086122461 ) ) ;
#91516 = CARTESIAN_POINT ( 'NONE',  ( 4.078750125433938223, -0.7691220382576718917, 1.864168106189521890 ) ) ;
#91517 = CARTESIAN_POINT ( 'NONE',  ( -10.66756793585402363, 11.33991743478486391, 0.7998128361456462443 ) ) ;
#91519 = DIRECTION ( 'NONE',  ( 0.000000000000000000, 1.000000000000000000, 0.000000000000000000 ) ) ;
#91518 = CARTESIAN_POINT ( 'NONE',  ( 1.798126127191189472, -0.7612548243747189192, 2.130717213291497547 ) ) ;
#91520 = CARTESIAN_POINT ( 'NONE',  ( 4.876057405804426814, 1.210321851207227795, 1.723226277364843462 ) ) ;
#91521 = CARTESIAN_POINT ( 'NONE',  ( 7.840529994971273453, 15.85037637632706264, 8.677903555585629647 ) ) ;
#91522 = AXIS2_PLACEMENT_3D ( 'NONE', #12030, #78101, #13090 ) ;
#91523 = CARTESIAN_POINT ( 'NONE',  ( 2.682155120989743402, -1.190029146579720587, -1.693995171316540427 ) ) ;
#91524 = CARTESIAN_POINT ( 'NONE',  ( 4.005544317833563461, 6.760553239859419250, -1.199719254218452047 ) ) ;
#91525 = CARTESIAN_POINT ( 'NONE',  ( -1.360316468750018659, 0.6927083336747492659, 0.7853790794158961308 ) ) ;
#91526 = CARTESIAN_POINT ( 'NONE',  ( 4.688201205076114597, 1.221562550966972527, 1.733079268972044895 ) ) ;
#91529 = ADVANCED_FACE ( 'NONE', ( #97233, #197894 ), #31160, .T. ) ;
#91528 = CARTESIAN_POINT ( 'NONE',  ( 1.471183419133621717, 0.1424870401847652956, -1.921283849777700947 ) ) ;
#91527 = CARTESIAN_POINT ( 'NONE',  ( -2.589244150085650009, 5.964609241834465614, 0.7216878364870317197 ) ) ;
#91530 = CARTESIAN_POINT ( 'NONE',  ( -5.842637852846353397, 5.781108681267656202, 0.7998128361456281477 ) ) ;
#91531 = CARTESIAN_POINT ( 'NONE',  ( 8.772289083241844310, 10.19309100432570148, -1.199719254218446718 ) ) ;
#91532 = CARTESIAN_POINT ( 'NONE',  ( 6.522881301506172846, 6.782652071278222117, -0.7216878364870458196 ) ) ;
#91533 = CARTESIAN_POINT ( 'NONE',  ( 4.318426605249491068, 7.201576024430431211, 1.005918518748824875 ) ) ;
#91534 = CARTESIAN_POINT ( 'NONE',  ( -4.386226389220933441, 5.076017861301227008, -1.199719254218446718 ) ) ;
#91535 = CARTESIAN_POINT ( 'NONE',  ( 5.924112389714110805, -2.104401743431310923, 0.2612745606217213856 ) ) ;
#91536 = CARTESIAN_POINT ( 'NONE',  ( 2.661270901210018636, -1.831774207203272775, -1.038945448840204122 ) ) ;
#91537 = CARTESIAN_POINT ( 'NONE',  ( -3.156015896931072540, 6.904045323053366268, 0.000000000000000000 ) ) ;
#91538 = CARTESIAN_POINT ( 'NONE',  ( 7.507464373665139412, 9.781794407407920389, 1.599625672291281386 ) ) ;
#91539 = CARTESIAN_POINT ( 'NONE',  ( 6.543805726556771951, 1.282826940501276880, 1.348393317287248205 ) ) ;
#91540 = CARTESIAN_POINT ( 'NONE',  ( 6.103141704446003679, 10.27208242182903142, 0.7998128361456462443 ) ) ;
#91541 = CARTESIAN_POINT ( 'NONE',  ( 0.000000000000000000, 0.2000000000000057288, 0.000000000000000000 ) ) ;
#91542 = CARTESIAN_POINT ( 'NONE',  ( -4.553559489343377287, 6.405848385690952718, -1.599625672291271394 ) ) ;
#91543 = CARTESIAN_POINT ( 'NONE',  ( -9.815740026613967828, 10.55404424057886636, -0.7216878364870267237 ) ) ;
#91544 = CARTESIAN_POINT ( 'NONE',  ( 0.6156802735862785259, 1.737094954450137285, 1.216079458918501333 ) ) ;
#91545 = FACE_OUTER_BOUND ( 'NONE', #78737, .T. ) ;
#91547 = CARTESIAN_POINT ( 'NONE',  ( 3.648837080137564470, -0.3802854374791163616, -1.924481129451253603 ) ) ;
#91546 = CARTESIAN_POINT ( 'NONE',  ( 0.6124999999999671818, -0.8333333333332831883, -1.060881119635969094 ) ) ;
#91548 = CARTESIAN_POINT ( 'NONE',  ( 2.325270847726228940, -0.0006328605136555342939, 2.161883445422786654 ) ) ;
#91549 = VECTOR ( 'NONE', #33311, 1000.000000000000000 ) ;
#91551 = CARTESIAN_POINT ( 'NONE',  ( -4.981332701451811396, 6.629279788159643694, -1.242877772926734625 ) ) ;
#91550 = CARTESIAN_POINT ( 'NONE',  ( -4.610654757099099221, 7.536791762327691657, 1.199719254218452935 ) ) ;
#91552 = CARTESIAN_POINT ( 'NONE',  ( -1.201851678989727383E-14, 2.321875000341416584, 1.575800808251672791 ) ) ;
#91553 = CARTESIAN_POINT ( 'NONE',  ( 3.380519863291716387, 1.572804015177066805, -0.7453022471971497698 ) ) ;
#91554 = CARTESIAN_POINT ( 'NONE',  ( 5.504247177468175600, 8.405076892812779477, 1.082531754730558626 ) ) ;
#91555 = CARTESIAN_POINT ( 'NONE',  ( -12.26626736352559455, 6.252815285820443769, 3.851661612215340647 ) ) ;
#91556 = EDGE_CURVE ( 'NONE', #112763, #176746, #143667, .T. ) ;
#91557 = EDGE_LOOP ( 'NONE', ( #121369, #52113, #8694, #39142 ) ) ;
#91558 = CARTESIAN_POINT ( 'NONE',  ( 2.231795861093866851, -1.842164517099669441, -0.8196493499348647127 ) ) ;
#91559 = CARTESIAN_POINT ( 'NONE',  ( -0.08058608058609216529, -9.900000000000005684, -10.99970480893080271 ) ) ;
#91560 = CARTESIAN_POINT ( 'NONE',  ( -3.471769853551161411, 6.208092708188416076, 1.199719254218452935 ) ) ;
#91562 = EDGE_CURVE ( 'NONE', #40528, #77834, #205753, .T. ) ;
#91561 =( BOUNDED_SURFACE ( )  B_SPLINE_SURFACE ( 3, 3, ( 
 ( #186982, #35392, #38614, #22327, #122085, #72152, #101469, #19139, #85216, #109017, #124226, #27696, #91663, #77508, #140418, #159832, #193395, #209623, #206436, #172898, #60190, #43969, #191244, #58060, #208555, #207507, #24472, #126350, #192310, #8238, #90586, #190185, #189129, #157714, #176096, #110084, #93793, #125284, #9311, #41841, #107953, #11432, #173980, #141499, #143628, #25552, #26622, #61264, #127423, #175036, #45039, #75385, #59126, #106871, #42908, #10365, #156645, #40767, #92723, #74321, #158770, #76443, #142550, #186622, #206067, #85933, #137899, #119559, #90215, #53423, #19846, #135760, #121720, #122800, #120643, #86992, #152005, #138969, #23036, #57702, #156279, #172528, #185547, #187685, #6786, #3577, #203918, #70712, #89151, #69652, #136824, #154138, #73950, #123858, #188758, #155205, #40399, #140043, #201782, #37176, #7863, #153065, #38248, #103251, #41473, #204991, #169312, #168247, #20896, #39314, #4641, #202851, #54499, #189824, #104323, #72863, #170371, #56635, #21957, #55566, #88066, #105409, #5707, #106500, #171446, #24112, #71784, #127055, #111857, #177862, #11062, #42545, #29474, #143262, #63028, #207140, #76080, #190880, #173616, #44669, #91292, #191939, #25188, #208196, #193015, #59829, #108649, #159462, #174677, #93424, #92368, #95564, #158404, #124917, #26249, #161615, #157350, #10004, #110781, #195172, #142180, #13206, #128126, #109721, #77141, #125981, #43603, #209252, #60895, #8939, #175727, #129195, #79281, #58764, #75019, #176782, #194089, #27322, #145399, #144333, #28398, #94493, #141129, #160531, #12136, #78208, #210332, #61971, #45738, #211398, #107583, #173673, #7924, #25248, #136885, #135816, #54557, #153125, #72923, #140102, #154197, #104383, #5765, #203974, #69713, #201839, #169371, #20955, #87053, #105470, #22017, #185606, #156339, #172588, #4696, #53484, #103309, #70771, #71846, #23095, #88127, #90270, #56695, #205053, #137954, #6845, #74010, #24167, #55621, #40457, #186678, #206129, #106560, #57759, #202912, #119622, #107641, #120703, #38306, #123920, #121778, #37238, #189887, #155264, #122862, #187745, #89211, #170430, #41529, #152064, #39373, #171503, #139029, #3634, #188823, #160590, #177919, #211455, #124977, #58824, #145460, #76139, #175791, #207199, #178991, #62035, #9001, #91348, #190938, #110839, #157410, #141189, #108708, #129259, #75076, #12197, #27382, #128189, #63090, #193082, #93483, #176845, #195229, #194150, #28458, #60958, #42602, #95625, #111919, #159522, #143317, #208254, #10063, #77198, #209311, #174737, #59888, #46867, #79342, #26310, #92423, #94552, #29533, #11121, #112980, #45798, #127115, #109782, #158463, #192000, #142242, #78267, #43665, #144392, #126037, #161675, #44732, #210393, #13269, #150755, #51105, #1257, #34834, #16446, #65197, #31670, #97747, #100908, #163806, #181103, #83594, #213575, #198399, #199463, #18588, #66249, #84666, #180048, #32718, #162742, #131349, #182150, #96694, #2317, #15382, #99859, #33780, #82526, #98800, #48987, #68393, #14315, #181, #196294, #166997, #130307, #80408, #212523, #50041, #117230, #197345, #81476, #146506, #67315, #165921, #134522, #200526, #52172, #47941, #116164, #149676, #64164, #132397, #147553, #17506, #114055, #115105, #133459, #183228, #164854, #118298, #148612, #30606, #56439, #155006, #153942, #23915 ),
 ( #201588, #7663, #35910, #39122, #54307, #6591, #90020, #71591, #120445, #55368, #73748, #72670, #121522, #5510, #69459, #203720, #202658, #101985, #70516, #168054, #187492, #136631, #105205, #53235, #138768, #186419, #87870, #204786, #156077, #122598, #188561, #40192, #170174, #4446, #185353, #36975, #106304, #103058, #38057, #22838, #152868, #137700, #172326, #139843, #171242, #205872, #119365, #104128, #19656, #21762, #88952, #85731, #57506, #169112, #184284, #151816, #3389, #135564, #20708, #86802, #41276, #93227, #74825, #45537, #8744, #189628, #91092, #76933, #78010, #75881, #42341, #107385, #94294, #192812, #161413, #111651, #127937, #140925, #143059, #176588, #173408, #159259, #26052, #44470, #24989, #141988, #160334, #28200, #108456, #29271, #58568, #124722, #210127, #11938, #10860, #177663, #144134, #209054, #190682, #61769, #208002, #95363, #206939, #193889, #79073, #12997, #174476, #157152, #145191, #211197, #27121, #92165, #123665, #43402, #158217, #9806, #59628, #125785, #191747, #109525, #60690, #175532, #126854, #110586, #69994, #86276, #67854, #117780, #179788, #196041, #51658, #183772, #194962, #31408, #21242, #53781, #14051, #178728, #151289, #152346, #200008, #119914, #102526, #134002, #20188, #185890, #101456, #37524, #212259, #1797, #46598, #97482, #2860, #128983, #103599, #130048, #135050, #68930, #35382, #167528, #81212, #169657, #112716, #19126, #80140, #202121, #162479, #30343, #96428, #85205, #3924, #15124, #47675, #146243, #36451, #201063, #87349, #153415, #136106, #63893, #52705, #118835, #113786, #184821, #163539, #168588, #147292, #62823, #41824, #58042, #138246, #125265, #154489, #6068, #91643, #190170, #189112, #59105, #107937, #40746, #72138, #157696, #171796, #191226, #22310, #75366, #175015, #42889, #88423, #54849, #124207, #173962, #123155, #204260, #25535, #139315, #120999, #9293, #141478, #170724, #186966, #55911, #90568, #207486, #92703, #122069, #108998, #26602, #7136, #56981, #188032, #39662, #205344, #106851, #137178, #105770, #4986, #71062, #23390, #38598, #156629, #203202, #172881, #104676, #89501, #73208, #155556, #24454, #8218, #74303, #140399, #206418, #13550, #176076, #47153, #45018, #62313, #179274, #64445, #30897, #129535, #163022, #144671, #193373, #159809, #11413, #14604, #77488, #94833, #211741, #127401, #112201, #143607, #29824, #113269, #31951, #209600, #80702, #96974, #160884, #210684, #61244, #111128, #128472, #194440, #76418, #177131, #114334, #146792, #110064, #60172, #95907, #212808, #78553, #130590, #195516, #12479, #28749, #142528, #46082, #10344, #161960, #178208, #79622, #27674, #196579, #145741, #63380, #48221, #180329, #158749, #208536, #126329, #192288, #43948, #93769, #99087, #102265, #165139, #34065, #151038, #66533, #51398, #52456, #86021, #133745, #152094, #33008, #100136, #15670, #132675, #35120, #164089, #3665, #16730, #167280, #101191, #83876, #166199, #116444, #135847, #81757, #67599, #49270, #19935, #197626, #147839, #65477, #117518, #118581, #50326, #82815, #213857, #68676, #18865, #201870, #69742, #168340, #115392, #183511, #2607, #131627, #199753, #464, #84949, #181385, #182438, #134799, #200805, #148891, #53518, #198681, #17789, #184569, #36189, #119652, #185637, #98036, #149968, #1537, #189919, #204003, #91383, #54589, #107677, #207232, #9037 ),
 ( #202945, #87085, #139057, #187775, #122894, #75111, #7954, #188853, #6877, #136918, #56726, #41564, #173706, #155294, #186709, #25281, #72955, #58856, #120736, #5799, #38338, #103339, #40489, #20988, #121808, #169402, #137986, #106594, #55652, #104414, #89243, #170463, #23126, #22048, #157443, #88159, #154227, #71876, #141223, #153155, #39407, #90300, #125012, #37269, #4730, #105501, #70805, #171533, #205084, #172621, #24197, #156370, #74046, #140136, #206162, #57790, #123950, #208286, #59918, #126074, #144425, #60993, #10096, #195267, #211490, #192035, #108744, #142275, #109815, #44767, #62069, #127146, #129291, #95660, #29568, #193119, #45831, #113016, #63127, #110875, #79376, #11154, #46902, #145495, #179025, #43698, #26345, #146545, #175825, #27417, #30643, #176880, #76170, #96727, #194187, #161711, #160626, #128224, #93515, #162776, #14354, #28492, #159557, #94583, #80444, #212563, #111952, #64202, #190969, #77231, #158497, #42635, #143350, #12227, #92458, #174770, #13303, #209345, #78300, #210427, #177954, #3426, #180083, #147589, #168092, #196332, #199498, #215, #100942, #35944, #213607, #19691, #47976, #51142, #66286, #167029, #102023, #17540, #132433, #1292, #85769, #18624, #67350, #99895, #15420, #149712, #134558, #200561, #33816, #65234, #52208, #165956, #151850, #81510, #98838, #131384, #114092, #133495, #31706, #198434, #97781, #16482, #117266, #82563, #197380, #182188, #49021, #116201, #115140, #118334, #181136, #32756, #164888, #184319, #163841, #148649, #183264, #130343, #50080, #83629, #34868, #84703, #150790, #2353, #68429, #57543, #71626, #21797, #137739, #121556, #201621, #119401, #86837, #152902, #4480, #22873, #153978, #103091, #73781, #90056, #70551, #53270, #20742, #202695, #203759, #155042, #5545, #7698, #188598, #122635, #55402, #138802, #205908, #156116, #187527, #172362, #104164, #139877, #23952, #123700, #136670, #185390, #25024, #54345, #120484, #189661, #39158, #169149, #41313, #72707, #40229, #105241, #6628, #186456, #107420, #173445, #171281, #38093, #88989, #91124, #157183, #204822, #69493, #135600, #170212, #37009, #87905, #56473, #106340, #124759, #96466, #193925, #140964, #8778, #42381, #28236, #74861, #58605, #159298, #94329, #46632, #45572, #160371, #192848, #108491, #11973, #13032, #79109, #126890, #158256, #145227, #44507, #178767, #174515, #191785, #92206, #206974, #78047, #190719, #93265, #26091, #109565, #144171, #175569, #9845, #60727, #75920, #209092, #208038, #211232, #59665, #142023, #125824, #62857, #43441, #27160, #61804, #30380, #129022, #10897, #76972, #143099, #110624, #176625, #210163, #194998, #127973, #111688, #177695, #29306, #95400, #161452, #112755, #31443, #97522, #115938, #32496, #196078, #166767, #183002, #163578, #80178, #113825, #81249, #16216, #33558, #98570, #100689, #67093, #1028, #164632, #17285, #84440, #34619, #82300, #50880, #197122, #18362, #117003, #150529, #15161, #212296, #118077, #147329, #213357, #2090, #148393, #47710, #68164, #165696, #133228, #132172, #99630, #64978, #134296, #200303, #214394, #179824, #66023, #51955, #184064, #83361, #35682, #162515, #131133, #130083, #14087, #48761, #198178, #63928, #146283, #199233, #114873, #180874, #49811, #181927, #149446, #151592, #119139, #139620, #167827, #171021, #186193, #72439, #7437, #203494, #106080 ),
 ( #19426, #136412, #38895, #85505, #89806, #168887, #22618, #104981, #87648, #103904, #120219, #205643, #3159, #71364, #53004, #23696, #201363, #69231, #135349, #55147, #56212, #54083, #20491, #185121, #138540, #88727, #57281, #155850, #172103, #36746, #121293, #154785, #102832, #137480, #4226, #6370, #86577, #37825, #204564, #122376, #152641, #73518, #70296, #202428, #188333, #39973, #187269, #123443, #189405, #101759, #169950, #21538, #153718, #5286, #58343, #111422, #210963, #12762, #124499, #90863, #160105, #143903, #159042, #190458, #94065, #175307, #156927, #11708, #77782, #206715, #8516, #108229, #126621, #209896, #128753, #174254, #45303, #61534, #43185, #92998, #157996, #25826, #26894, #10635, #173181, #9585, #62590, #29044, #42117, #74597, #192584, #127700, #76711, #95127, #193660, #109298, #59403, #24761, #141768, #107156, #44239, #207776, #110360, #91936, #177426, #125559, #142827, #161176, #78836, #144957, #41047, #140701, #208834, #75661, #191520, #60464, #176364, #27971, #182736, #129822, #130865, #112485, #14888, #131907, #46365, #34355, #47441, #49543, #197915, #180609, #196861, #213093, #18090, #178494, #164370, #146014, #116737, #79906, #30104, #162244, #148131, #149180, #147072, #113556, #96194, #165426, #115669, #84178, #100428, #198968, #212025, #214132, #33290, #13831, #15954, #97253, #181663, #63668, #64723, #17024, #99374, #179559, #166499, #195804, #31180, #66822, #83100, #82037, #150267, #756, #65760, #163307, #132965, #48499, #1835, #80983, #50612, #67894, #194726, #114618, #32234, #98305, #22357, #37566, #2898, #187010, #53825, #183810, #104720, #38641, #85242, #35420, #201104, #5032, #88469, #7180, #52744, #138287, #154529, #136150, #185930, #36491, #118878, #119955, #103646, #51698, #102568, #89544, #122111, #151330, #101498, #71107, #6108, #169698, #188076, #170768, #202167, #152388, #117820, #20231, #200047, #137225, #86316, #203245, #68971, #72178, #3966, #21286, #204302, #39705, #55958, #105814, #171840, #87392, #168628, #135090, #184864, #23433, #70034, #153459, #155595, #54889, #121043, #134039, #167568, #19168, #114121, #30672, #145522, #162805, #196363, #106899, #40794, #130373, #58089, #160660, #189155, #163873, #46929, #205389, #73251, #172925, #95686, #139358, #123194, #90612, #180113, #57027, #211521, #12256, #113047, #48003, #177987, #78333, #161740, #31737, #179053, #13331, #45863, #24502, #79405, #80474, #146573, #194218, #8263, #212592, #111984, #97810, #156671, #44799, #74347, #140451, #63157, #206462, #144455, #127181, #176910, #129322, #28525, #193149, #128255, #110904, #62096, #94616, #64230, #210458, #29600, #195299, #96755, #14382, #132465, #68464, #37042, #85804, #103126, #249, #213639, #198467, #16512, #150823, #3458, #17574, #182223, #83658, #67386, #147620, #65265, #32792, #98867, #164919, #183296, #99927, #49052, #19725, #35978, #82595, #131411, #181167, #148681, #149748, #100974, #165989, #168124, #134592, #200592, #1325, #84735, #151884, #102059, #133526, #118368, #50112, #69528, #184356, #135635, #66321, #197411, #185424, #116232, #33846, #201656, #199533, #115172, #53305, #18655, #52240, #51176, #167063, #117299, #119437, #15450, #34902, #2386, #81538, #188633, #173484, #25061, #72741, #104199, #91163, #204855, #124793, #54379, #137773, #38126, #20776, #106375 ),
 ( #86872, #40264, #55437, #23987, #186495, #57576, #121589, #138839, #189696, #74893, #41349, #139914, #157219, #155078, #203791, #170246, #21831, #8817, #87939, #105277, #7734, #187561, #122671, #123735, #141001, #56510, #207009, #154013, #171314, #152938, #39188, #172399, #4515, #58640, #5579, #90089, #156153, #6665, #22909, #89025, #190754, #70588, #73820, #120517, #42417, #71659, #136703, #202727, #205945, #107458, #169184, #27194, #92239, #79147, #177731, #146315, #30417, #112790, #125860, #61839, #161489, #158289, #78083, #10932, #29344, #174551, #126928, #145263, #13068, #93300, #14123, #43482, #109600, #195036, #211270, #144207, #162552, #62894, #210203, #175605, #46670, #60768, #80215, #191817, #178802, #63968, #212329, #159336, #9879, #129063, #96502, #12009, #77008, #130124, #28272, #75955, #196112, #108522, #59698, #142058, #143135, #193960, #110658, #209130, #128006, #26127, #208072, #95439, #192885, #44542, #176659, #94364, #160406, #45607, #111723, #163616, #135378, #18395, #179859, #47749, #81288, #67131, #113864, #97558, #65015, #85535, #31483, #117042, #132204, #84472, #167862, #149483, #198212, #133264, #151625, #150563, #199272, #17320, #147365, #50915, #51987, #118112, #165733, #197158, #184097, #83401, #3191, #213391, #16252, #131168, #15197, #183038, #48795, #49847, #114912, #148429, #34654, #31607, #180910, #99664, #32533, #33592, #98608, #35717, #164669, #82337, #66061, #101793, #115974, #181964, #100724, #69262, #19460, #1066, #166803, #2124, #68199, #134331, #200336, #189436, #203524, #153746, #55178, #38925, #119169, #36778, #4257, #70327, #136444, #154813, #71396, #20524, #205672, #7469, #202460, #185154, #152674, #120249, #121323, #72471, #137507, #139651, #106110, #40001, #187298, #56244, #123474, #73548, #105008, #89832, #21567, #57309, #155880, #41078, #54115, #102863, #156953, #186226, #37858, #107186, #171048, #86607, #173211, #204592, #172131, #22646, #138570, #103937, #24790, #90893, #8545, #88756, #169980, #74627, #122403, #23726, #6398, #188361, #87674, #201397, #53034, #168920, #5314, #142859, #161208, #61567, #176396, #127733, #95157, #108260, #42145, #29073, #141800, #175340, #190487, #210994, #77812, #58374, #140732, #174281, #44270, #206744, #25856, #9613, #124529, #91966, #45335, #192617, #12794, #158024, #209928, #28001, #193691, #75690, #144989, #111455, #177459, #26921, #78868, #207804, #59433, #125590, #208862, #191550, #43214, #109331, #60492, #143933, #110391, #159071, #93030, #126651, #10667, #94098, #76738, #160137, #11737, #54812, #171757, #186932, #105727, #104639, #124170, #170686, #137140, #38564, #41788, #37486, #22273, #172843, #141444, #190132, #207450, #88382, #103563, #154451, #120960, #40709, #107901, #122031, #72099, #187997, #23352, #169623, #21206, #203167, #6030, #138209, #73169, #204222, #153377, #173927, #140361, #55874, #87308, #71025, #39622, #89462, #205307, #155515, #58006, #24415, #90528, #7097, #189076, #25500, #206380, #139275, #8184, #56944, #91608, #74269, #157659, #123116, #4948, #75327, #106813, #156590, #119876, #9257, #185854, #96939, #125230, #128439, #143572, #29787, #179238, #160848, #209564, #144636, #162990, #95872, #210651, #28713, #158715, #78519, #63343, #129502, #177098, #208502, #195483, #94799, #14571, #10312, #27635, #142495, #191188 ),
 ( #43916, #47116, #110031, #76387, #126294, #113234, #42855, #176043, #112168, #80666, #30862, #146757, #93736, #108962, #159775, #60137, #194405, #59069, #61210, #11374, #127367, #111092, #174982, #26566, #192253, #77454, #193338, #12440, #44983, #92671, #62278, #79589, #46047, #178171, #161927, #13517, #145709, #211707, #148857, #151004, #117488, #51365, #82784, #67569, #134767, #18832, #431, #101158, #32976, #84916, #167244, #2574, #65443, #48190, #168307, #131594, #81724, #68644, #66502, #98001, #200775, #1503, #183479, #182405, #149934, #115358, #52427, #118552, #132641, #164058, #116414, #36157, #184534, #133713, #102236, #19905, #31922, #180300, #85990, #197596, #198647, #114301, #212775, #35087, #130556, #64411, #15637, #17756, #34034, #49239, #196547, #165107, #147807, #213825, #181350, #99052, #16699, #50296, #100107, #166167, #83845, #199719, #61319, #139380, #93845, #75435, #124275, #59173, #11488, #158821, #125332, #157763, #73277, #207553, #192360, #44018, #91714, #123216, #110137, #9363, #143683, #205412, #156697, #57052, #39732, #191295, #171864, #58116, #105837, #74372, #42961, #140474, #189180, #25601, #40817, #174030, #172949, #176149, #24528, #106925, #90637, #27749, #23458, #8287, #26673, #209675, #159883, #188101, #206486, #89570, #190233, #41892, #109070, #77560, #108003, #141547, #175086, #92777, #155619, #7204, #10417, #76489, #142599, #208609, #60241, #126400, #134618, #150849, #62378, #45094, #78622, #46156, #195590, #212883, #63451, #68490, #34929, #180399, #211814, #196649, #52267, #2413, #129604, #18683, #162030, #200620, #84762, #118395, #194508, #177207, #85830, #112269, #210757, #184382, #47224, #12547, #36001, #130659, #101003, #97044, #64514, #29892, #102082, #168150, #113342, #144746, #30969, #19750, #151909, #48289, #3483, #127479, #160957, #94906, #193450, #95978, #128542, #114401, #111203, #179347, #79694, #163097, #14677, #28821, #178283, #13621, #145807, #80774, #146861, #167092, #103151, #73850, #90117, #4540, #201683, #20803, #202753, #137800, #155109, #5605, #7761, #188663, #122700, #154039, #138868, #205971, #156183, #71687, #172426, #104226, #139945, #24015, #57603, #136729, #119462, #25086, #54406, #152967, #123762, #203819, #169212, #189723, #72769, #40292, #39214, #6694, #186524, #41377, #107487, #55464, #86899, #187589, #173512, #91187, #204887, #157248, #69550, #70614, #37070, #135661, #120545, #121619, #185450, #53329, #106402, #38154, #170273, #21858, #89052, #87965, #105305, #171342, #22936, #56538, #8841, #96530, #174580, #129093, #110687, #159363, #94394, #46703, #193987, #160432, #192915, #108548, #28297, #13099, #79179, #126956, #158316, #145295, #44571, #176685, #26156, #12038, #125888, #178832, #211300, #92270, #124817, #78109, #29374, #143164, #62924, #45635, #10961, #27221, #141030, #109630, #74919, #144236, #175635, #210230, #9907, #111753, #93327, #61868, #95469, #195064, #161517, #177758, #112819, #128033, #209159, #77037, #60797, #30446, #207037, #58667, #75983, #190781, #142086, #42445, #208101, #59730, #191846, #43509, #81316, #146346, #133294, #17349, #200365, #84501, #166832, #179888, #116004, #1098, #212358, #132232, #65042, #83431, #14153, #180939, #199300, #67158, #147392, #68229, #97587, #163646, #34681, #50945, #198241, #2153, #117069, #49879, #15226 ),
 ( #114939, #183067, #134361, #82367, #63999, #100750, #18428, #113894, #130150, #213419, #33623, #150591, #35748, #131198, #52014, #118140, #164695, #26, #197186, #98636, #66090, #47780, #99694, #48823, #184125, #162579, #31512, #196140, #165764, #80247, #148456, #32559, #16281, #181990, #149513, #19490, #202493, #167889, #187332, #54145, #171081, #119199, #204627, #120281, #5347, #122437, #7499, #188395, #72505, #106143, #87705, #136472, #102891, #168950, #172167, #20552, #37891, #154847, #70358, #55211, #56278, #89864, #137541, #155914, #36808, #103969, #85565, #186256, #38961, #151654, #73583, #86637, #22677, #6431, #170011, #88789, #23759, #40031, #21599, #139686, #153777, #205707, #57342, #123505, #152704, #3224, #189470, #4286, #185185, #101822, #71429, #201426, #69292, #105045, #138604, #203558, #135403, #121357, #53066, #61599, #43244, #206774, #159101, #78901, #209960, #110424, #127769, #161240, #74658, #8578, #95189, #25888, #125624, #156991, #128811, #11770, #173245, #41112, #140762, #60526, #107221, #90925, #58408, #145023, #62652, #24823, #124562, #190521, #12826, #142895, #191582, #126687, #211027, #77843, #192649, #10703, #42178, #44302, #45369, #111485, #76772, #108293, #177493, #208895, #193725, #174314, #158058, #91998, #9644, #176427, #75720, #109363, #141834, #207839, #28036, #59465, #175372, #93062, #26955, #94131, #160170, #29106, #143966, #212090, #47508, #116804, #112547, #97320, #33357, #1898, #50679, #67958, #179623, #178557, #163376, #195869, #115736, #182804, #196926, #147133, #48563, #32301, #30167, #96255, #63726, #129885, #113620, #148196, #64789, #13893, #199031, #821, #31243, #162308, #146078, #14951, #114683, #65825, #130933, #133031, #99438, #81048, #181726, #34421, #180676, #213159, #98368, #164431, #79974, #16017, #82103, #214196, #131973, #197983, #49611, #165493, #100494, #66891, #17087, #83165, #149248, #166569, #18157, #84245, #150331, #194792, #46429, #187073, #4032, #203306, #56023, #154595, #70101, #22423, #168695, #6173, #88533, #72242, #201172, #183875, #89608, #52811, #2968, #138349, #136215, #19233, #204366, #137288, #38706, #103711, #71170, #36552, #122177, #188142, #202235, #85313, #37632, #171905, #39775, #54955, #105880, #23501, #167632, #101565, #155658, #118949, #53887, #35487, #7240, #104786, #51762, #134102, #151397, #153526, #200111, #69037, #135155, #117882, #184928, #102639, #20300, #86385, #152453, #21351, #120022, #5095, #185997, #170832, #121107, #169762, #87458, #92813, #77596, #143719, #191331, #8327, #209711, #109109, #93883, #139420, #190272, #206523, #205455, #10454, #57088, #157803, #123253, #174066, #158857, #25638, #74411, #125367, #140511, #59210, #58154, #61356, #124313, #90674, #41929, #127515, #189218, #108041, #126436, #94943, #193487, #160991, #91750, #40857, #9401, #76527, #75471, #142639, #156736, #176185, #141584, #42996, #159922, #45129, #11526, #44055, #111239, #175124, #207591, #26711, #208648, #177243, #60279, #192399, #110174, #27785, #28856, #73317, #106964, #172988, #24568, #162065, #163130, #144783, #47262, #164187, #78655, #562, #79727, #81859, #15773, #212915, #14713, #31003, #50426, #210791, #196683, #178321, #148987, #112305, #62414, #194543, #180432, #181480, #179382, #145843, #128578, #197729, #147943, #116545, #66628, #16831, #29929 ) ),
 .UNSPECIFIED., .T., .F., .T. ) 
 B_SPLINE_SURFACE_WITH_KNOTS ( ( 4, 3, 4 ),
 ( 4, 1, 1, 1, 1, 1, 1, 1, 1, 1, 1, 1, 1, 1, 1, 1, 1, 1, 1, 1, 1, 1, 1, 1, 1, 1, 1, 1, 1, 1, 1, 1, 1, 1, 1, 1, 1, 1, 1, 1, 1, 1, 1, 1, 1, 1, 1, 1, 1, 1, 1, 1, 1, 1, 1, 1, 1, 1, 1, 1, 1, 1, 1, 1, 1, 1, 1, 1, 1, 1, 1, 1, 1, 1, 1, 1, 1, 1, 1, 1, 1, 1, 1, 1, 1, 1, 1, 1, 1, 1, 1, 1, 1, 1, 1, 1, 1, 1, 1, 1, 1, 1, 1, 1, 1, 1, 1, 1, 1, 1, 1, 1, 1, 1, 1, 1, 1, 1, 1, 1, 1, 1, 1, 1, 1, 1, 1, 1, 1, 1, 1, 1, 1, 1, 1, 1, 1, 1, 1, 1, 1, 1, 1, 1, 1, 1, 1, 1, 1, 1, 1, 1, 1, 1, 1, 1, 1, 1, 1, 1, 1, 1, 1, 1, 1, 1, 1, 1, 1, 1, 1, 1, 1, 1, 1, 1, 1, 1, 1, 1, 1, 1, 1, 1, 1, 1, 1, 1, 1, 1, 1, 1, 1, 1, 1, 1, 1, 1, 1, 1, 1, 1, 1, 1, 1, 1, 1, 1, 1, 1, 1, 1, 1, 1, 1, 1, 1, 1, 1, 1, 1, 1, 1, 1, 1, 1, 1, 1, 1, 1, 1, 1, 1, 1, 1, 1, 1, 1, 1, 1, 1, 1, 1, 1, 1, 1, 1, 1, 1, 1, 1, 1, 1, 1, 1, 1, 1, 1, 1, 1, 1, 1, 1, 1, 1, 1, 1, 1, 1, 1, 1, 1, 1, 1, 1, 1, 1, 1, 1, 1, 1, 1, 1, 1, 1, 1, 1, 1, 1, 1, 1, 1, 1, 1, 1, 1, 1, 1, 1, 1, 1, 1, 1, 1, 1, 1, 1, 1, 1, 1, 1, 1, 1, 1, 1, 1, 1, 1, 1, 1, 1, 1, 1, 1, 1, 1, 1, 1, 1, 1, 1, 1, 1, 1, 1, 1, 1, 1, 1, 1, 1, 1, 1, 1, 1, 1, 1, 1, 1, 1, 1, 1, 1, 1, 1, 1, 1, 1, 1, 1, 1, 1, 1, 1, 1, 1, 1, 1, 1, 1, 1, 1, 1, 1, 1, 1, 1, 1, 1, 1, 1, 1, 1, 1, 4 ),
 ( 0.000000000000000000, 0.5000000000000000000, 1.000000000000000000 ),
 ( 0.000000000000000000, 0.002600214693118923798, 0.005208871813129847643, 0.007813341859462101871, 0.01041561011214237054, 0.01302159838915000617, 0.01562452542669844589, 0.01822945805747129902, 0.02083332260852943998, 0.02343713088342555886, 0.02604210653276634729, 0.02864513693292065552, 0.03125071383394792401, 0.03385356881896259273, 0.03645895053148855841, 0.03906228851054763251, 0.04166670673482164577, 0.04427111720854654681, 0.04687446234244373178, 0.04947983976256019323, 0.05208269766733494843, 0.05468827385445936690, 0.05729129101459448647, 0.05989628262864687969, 0.06250008845252298662, 0.06510390268380349121, 0.06770888856031336001, 0.07031191025079500112, 0.07291748459129859805, 0.07552033970978830335, 0.07812571920045624507, 0.08072905536012038585, 0.08333347174482363950, 0.08593788071299547637, 0.08854122383090638759, 0.09114659965375219997, 0.09374945576594469199, 0.09635503022752239799, 0.09895804583665256116, 0.1015630356028039000, 0.1041668400134527495, 0.1067706523020897913, 0.1093756367037285043, 0.1119786565701353653, 0.1145842293264338063, 0.1171870828570002881, 0.1197924606432616973, 0.1223957954228293843, 0.1250002099740243899, 0.1276046175975352470, 0.1302079588893767237, 0.1328133332639841735, 0.1354161877457908392, 0.1380217606440506395, 0.1406247748629219918, 0.1432297629411592166, 0.1458335661004374617, 0.1484373766077259071, 0.1510423596945167368, 0.1536453778991425101, 0.1562509492307036785, 0.1588538013357113088, 0.1614591775772540871, 0.1640625111385781432, 0.1666669240170048083, 0.1692713304565471311, 0.1718746700842041231, 0.1744800431702197008, 0.1770828961840006377, 0.1796884676783837009, 0.1822914806691622869, 0.1848964672195632097, 0.1875002692887918765, 0.1901040781760970355, 0.1927090601080766463, 0.1953120768130981733, 0.1979176468793322763, 0.2005204977210985895, 0.2031258725775486607, 0.2057292050824250096, 0.2083336164487647746, 0.2109380218649763994, 0.2135413599902747928, 0.2161467319472901716, 0.2187495836553486062, 0.2213551539052408534, 0.2239581658300387468, 0.2265631510126252801, 0.2291669521530730058, 0.2317707595817034838, 0.2343757405188569010, 0.2369787558863956922, 0.2395843248466610342, 0.2421871745874512594, 0.2447925482183819501, 0.2473958798285567084, 0.2500002898434375842, 0.2526046943969075254, 0.2552080311816201097, 0.2578134021691782518, 0.2604162527337665622, 0.2630218218985046486, 0.2656248329193858781, 0.2682298168941298910, 0.2708336172670197106, 0.2734374233982336255, 0.2760424035005001331, 0.2786454176926287940, 0.2812509857062375773, 0.2838538345082703418, 0.2864592070732082663, 0.2890625379503836689, 0.2916669467743862043, 0.2942713506256608436, 0.2968746862315132518, 0.2994800564091141259, 0.3020829059924399762, 0.3046884742313171190, 0.3072914845103039694, 0.3098964674371332273, 0.3125002672036480411, 0.3151040721986592130, 0.3177090516259382103, 0.3203120648046862140, 0.3229176320309106729, 0.3255204800563645251, 0.3281258517147956355, 0.3307291820206363919, 0.3333335898142997245, 0.3359379931238887229, 0.3385413277125659537, 0.3411466972396727249, 0.3437495460039050044, 0.3463551134761772565, 0.3489581231752558743, 0.3515631052140602009, 0.3541669045353489920, 0.3567707085553323276, 0.3593756874674896018, 0.3619786997948497009, 0.3645842663929277916, 0.3671871138039469185, 0.3697924847153226668, 0.3723958146114617063, 0.3750002215352895019, 0.3776046244636719340, 0.3802079581968237365, 0.3828133272328684833, 0.3854161753401436075, 0.3880217422050354359, 0.3906247514861621029, 0.3932297327967993472, 0.3958335318339832876, 0.3984373350400814418, 0.4010423135969549691, 0.4036453252348887744, 0.4062508913640303643, 0.4088537383227308641, 0.4114591086464738368, 0.4140624382945181647, 0.4166668445089845574, 0.4192712472166146842, 0.4218745802558619973, 0.4244799489602520959, 0.4270827965726798348, 0.4296883629893904488, 0.4322913720144979099, 0.4348963527567997200, 0.4375001516709778882, 0.4401039542243071478, 0.4427089325857130886, 0.4453119436961573974, 0.4479175095155500941, 0.4505203561840259718, 0.4531257260795358843, 0.4557290556410732441, 0.4583334613066292196, 0.4609378639539425948, 0.4635411964608836533, 0.4661465649930071620, 0.4687494122726767465, 0.4713549784003855381, 0.4739579873313886638, 0.4765629676651664814, 0.4791667666174222462, 0.4817705686790782482, 0.4843755470048167200, 0.4869785577496898998, 0.4895841234185048796, 0.4921869699588339309, 0.4947923395854939010, 0.4973956692220981579, 0.5000000744991768276, 0.5026044772465965149, 0.5052078093828125116, 0.5078131779020444991, 0.5104160250110306718, 0.5130215910089035436, 0.5156246000077054914, 0.5182295800927568807, 0.5208333792441637300, 0.5234371809752277338, 0.5260421594250891397, 0.5286451699662961801, 0.5312507356436946271, 0.5338535822179446555, 0.5364589517351265879, 0.5390622816083643354, 0.5416666866573878192, 0.5442710896653298880, 0.5468744215923915242, 0.5494797902580997873, 0.5520826373584690749, 0.5546882033856646022, 0.5572912126141627009, 0.5598961926102767883, 0.5624999921219043797, 0.5651037936834493181, 0.5677087724172201755, 0.5703117829166597375, 0.5729173487617980065, 0.5755201955320329299, 0.5781255650991041772, 0.5807288953705399548, 0.5833333003519244331, 0.5859377037808047861, 0.5885410356602774895, 0.5911464046318289922, 0.5937492518856454238, 0.5963548181013198501, 0.5989578277214122615, 0.6015628077883760083, 0.6041666078212959423, 0.6067704093743923055, 0.6093753885518610192, 0.6119783991714310423, 0.6145839653434672645, 0.6171868124717531101, 0.6197921822480817466, 0.6223955130792849788, 0.6249999181534476866, 0.6276043221636865566, 0.6302076541571374202, 0.6328130235939036785, 0.6354158711632348355, 0.6380214377265494008, 0.6406244479001403924, 0.6432294281977445349, 0.6458332289130368498, 0.6484370306187589028, 0.6510420103997216490, 0.6536450213013255128, 0.6562505879594253688, 0.6588534356078361576, 0.6614588057527972520, 0.6640621373053481324, 0.6666665426327121891, 0.6692709473847417989, 0.6718742796537453543, 0.6744796497151083203, 0.6770824977620315543, 0.6796880648321572682, 0.6822910757211636534, 0.6848960564092084757, 0.6874998579679674204, 0.6901036599873985322, 0.6927086405316660311, 0.6953116518772185506, 0.6979172191805607106, 0.7005200675111846742, 0.7031254381841663958, 0.7057287706196612165, 0.7083331763606625087, 0.7109375820149322900, 0.7135409147210758363, 0.7161462855664346705, 0.7187491342530435423, 0.7213547019891674017, 0.7239577137555243125, 0.7265626949938263079, 0.7291664975571658935, 0.7317703000514055311, 0.7343752815188082650, 0.7369782934702413524, 0.7395838615780243597, 0.7421867107529701579, 0.7447920821133793279, 0.7473954155934371402, 0.7499998219085300954, 0.7526042286255122393, 0.7552075619304030596, 0.7578129337191791270, 0.7604157832075884027, 0.7630213517689198310, 0.7656243645745874904, 0.7682293465229839136, 0.7708331502520449074, 0.7734369533822141873, 0.7760419359326080624, 0.7786449486518774998, 0.7812505177233250997, 0.7838533679047272607, 0.7864587401119955690, 0.7890620747982641792, 0.7916664818479275390, 0.7942708897881238794, 0.7968742238533942368, 0.7994795967450375462, 0.8020824471973901915, 0.8046880167431663677, 0.8072910307501349747, 0.8098960135684915018, 0.8124998186244467568, 0.8151036225516941069, 0.8177086063449673370, 0.8203116199940584385, 0.8229171901884252405, 0.8255200415384508217, 0.8281254147520410447, 0.8307287508062024539, 0.8333331587509454907, 0.8359375680748931670, 0.8385409030622068549, 0.8411462772162020540, 0.8437491287946751184, 0.8463546994841673055, 0.8489577148544642515, 0.8515626987026798655, 0.8541665052467400931, 0.8567703101322480252, 0.8593752953283267937, 0.8619783100692604005, 0.8645838815458386506, 0.8671867342266933454, 0.8697921086061042306, 0.8723954461898817403, 0.8749998551902504751, 0.8776042660585271493, 0.8802076021295854868, 0.8828129777054576355, 0.8854158305722678035, 0.8880214025647872322, 0.8906244194604823194, 0.8932294044984951942, 0.8958332126919159588, 0.8984370186969063976, 0.9010420054557602976, 0.9036450214505988843, 0.9062505943687239052, 0.9088534485426573717, 0.9114588242474312985, 0.9140621635225948394, 0.9166665737391771485, 0.9192709863124074454, 0.9218743236289563825, 0.9244797007862803895, 0.9270825551036790957, 0.9296881285585824051, 0.9322911471418501295, 0.9348961335295734587, 0.9374999435335269471, 0.9401037508197458425, 0.9427087393012421046, 0.9453117567106092967, 0.9479173312323898593, 0.9505201870615167525, 0.9531255642405720430, 0.9557289053967781278, 0.9583333169903581750, 0.9609377312744702415, 0.9635410702737328137, 0.9661464495301401723, 0.9687493035862174695, 0.9713548794777306927, 0.9739579066090123804, 0.9765628826531806972, 0.9791666865793459129, 0.9817705523293528413, 0.9843754818126480011, 0.9869784094881522973, 0.9895843956701340094, 0.9921866610829068733, 0.9947911313000845634, 0.9973997837621362272, 1.000000000000000000 ),
 .UNSPECIFIED. ) 
 GEOMETRIC_REPRESENTATION_ITEM ( )  RATIONAL_B_SPLINE_SURFACE ( (
 ( 1.000000000000000222, 1.000000000000000222, 1.000000000000000000, 1.000000000000000222, 1.000000000000000000, 0.9999999999999997780, 1.000000000000000222, 1.000000000000000000, 1.000000000000000222, 1.000000000000000222, 1.000000000000000000, 0.9999999999999997780, 1.000000000000000000, 1.000000000000000222, 0.9999999999999997780, 1.000000000000000222, 0.9999999999999994449, 1.000000000000000444, 0.9999999999999996669, 1.000000000000000000, 1.000000000000000222, 1.000000000000000000, 1.000000000000000000, 0.9999999999999997780, 1.000000000000000444, 0.9999999999999996669, 1.000000000000000000, 1.000000000000000222, 0.9999999999999997780, 1.000000000000000000, 0.9999999999999997780, 0.9999999999999997780, 1.000000000000000444, 0.9999999999999994449, 1.000000000000000444, 0.9999999999999997780, 0.9999999999999997780, 0.9999999999999996669, 1.000000000000000222, 1.000000000000000000, 0.9999999999999997780, 1.000000000000000222, 0.9999999999999997780, 1.000000000000000222, 1.000000000000000000, 1.000000000000000222, 1.000000000000000000, 1.000000000000000000, 1.000000000000000444, 0.9999999999999996669, 0.9999999999999997780, 1.000000000000000000, 0.9999999999999997780, 0.9999999999999997780, 1.000000000000000000, 1.000000000000000000, 0.9999999999999997780, 1.000000000000000444, 1.000000000000000000, 0.9999999999999997780, 1.000000000000000222, 0.9999999999999996669, 1.000000000000000222, 1.000000000000000000, 0.9999999999999997780, 1.000000000000000222, 0.9999999999999997780, 1.000000000000000000, 0.9999999999999997780, 1.000000000000000222, 0.9999999999999996669, 1.000000000000000000, 1.000000000000000222, 0.9999999999999997780, 1.000000000000000222, 0.9999999999999996669, 1.000000000000000444, 1.000000000000000000, 1.000000000000000000, 1.000000000000000222, 1.000000000000000222, 1.000000000000000000, 0.9999999999999997780, 1.000000000000000222, 0.9999999999999997780, 1.000000000000000000, 1.000000000000000000, 1.000000000000000000, 0.9999999999999997780, 1.000000000000000000, 0.9999999999999997780, 1.000000000000000222, 0.9999999999999997780, 1.000000000000000000, 1.000000000000000222, 0.9999999999999997780, 1.000000000000000000, 0.9999999999999996669, 1.000000000000000444, 0.9999999999999997780, 1.000000000000000000, 1.000000000000000000, 1.000000000000000000, 0.9999999999999997780, 0.9999999999999997780, 1.000000000000000222, 1.000000000000000222, 0.9999999999999997780, 1.000000000000000000, 1.000000000000000000, 1.000000000000000222, 1.000000000000000222, 1.000000000000000000, 0.9999999999999997780, 1.000000000000000222, 1.000000000000000000, 1.000000000000000000, 0.9999999999999997780, 0.9999999999999997780, 1.000000000000000222, 1.000000000000000000, 1.000000000000000000, 1.000000000000000000, 0.9999999999999997780, 1.000000000000000222, 1.000000000000000000, 1.000000000000000000, 1.000000000000000000, 1.000000000000000444, 0.9999999999999997780, 0.9999999999999997780, 1.000000000000000000, 1.000000000000000000, 0.9999999999999997780, 1.000000000000000222, 0.9999999999999997780, 1.000000000000000222, 1.000000000000000000, 1.000000000000000222, 1.000000000000000222, 1.000000000000000000, 1.000000000000000222, 1.000000000000000000, 0.9999999999999996669, 1.000000000000000222, 0.9999999999999997780, 1.000000000000000444, 0.9999999999999997780, 1.000000000000000000, 0.9999999999999997780, 1.000000000000000222, 1.000000000000000000, 0.9999999999999997780, 1.000000000000000222, 0.9999999999999994449, 1.000000000000000000, 1.000000000000000222, 1.000000000000000222, 0.9999999999999997780, 1.000000000000000444, 0.9999999999999997780, 1.000000000000000222, 0.9999999999999997780, 1.000000000000000222, 0.9999999999999997780, 1.000000000000000000, 1.000000000000000000, 1.000000000000000222, 0.9999999999999997780, 0.9999999999999996669, 1.000000000000000444, 0.9999999999999997780, 1.000000000000000222, 1.000000000000000000, 1.000000000000000222, 0.9999999999999994449, 1.000000000000000444, 0.9999999999999997780, 1.000000000000000000, 1.000000000000000222, 1.000000000000000000, 1.000000000000000000, 0.9999999999999997780, 1.000000000000000444, 0.9999999999999997780, 1.000000000000000444, 0.9999999999999997780, 1.000000000000000000, 1.000000000000000222, 0.9999999999999996669, 1.000000000000000222, 1.000000000000000000, 1.000000000000000000, 0.9999999999999996669, 1.000000000000000222, 1.000000000000000444, 0.9999999999999997780, 1.000000000000000222, 0.9999999999999996669, 1.000000000000000444, 0.9999999999999997780, 1.000000000000000444, 0.9999999999999996669, 0.9999999999999997780, 1.000000000000000000, 0.9999999999999997780, 1.000000000000000000, 1.000000000000000000, 1.000000000000000000, 1.000000000000000000, 0.9999999999999997780, 1.000000000000000000, 0.9999999999999997780, 1.000000000000000000, 1.000000000000000000, 1.000000000000000000, 1.000000000000000000, 0.9999999999999997780, 1.000000000000000222, 0.9999999999999997780, 1.000000000000000222, 0.9999999999999997780, 1.000000000000000222, 0.9999999999999994449, 1.000000000000000444, 1.000000000000000000, 1.000000000000000222, 0.9999999999999997780, 1.000000000000000000, 0.9999999999999997780, 1.000000000000000222, 1.000000000000000000, 1.000000000000000000, 1.000000000000000222, 1.000000000000000222, 0.9999999999999996669, 1.000000000000000444, 0.9999999999999996669, 1.000000000000000444, 0.9999999999999996669, 1.000000000000000000, 1.000000000000000000, 1.000000000000000000, 0.9999999999999997780, 1.000000000000000222, 0.9999999999999997780, 1.000000000000000222, 1.000000000000000000, 0.9999999999999997780, 1.000000000000000000, 1.000000000000000222, 1.000000000000000222, 1.000000000000000000, 1.000000000000000000, 1.000000000000000000, 1.000000000000000000, 0.9999999999999997780, 1.000000000000000444, 1.000000000000000000, 0.9999999999999997780, 1.000000000000000222, 0.9999999999999996669, 1.000000000000000444, 1.000000000000000000, 1.000000000000000222, 1.000000000000000222, 0.9999999999999997780, 1.000000000000000222, 0.9999999999999997780, 1.000000000000000000, 1.000000000000000000, 0.9999999999999997780, 1.000000000000000000, 1.000000000000000000, 0.9999999999999997780, 1.000000000000000222, 1.000000000000000000, 1.000000000000000000, 1.000000000000000222, 1.000000000000000000, 1.000000000000000000, 1.000000000000000000, 1.000000000000000222, 0.9999999999999997780, 1.000000000000000222, 1.000000000000000000, 0.9999999999999997780, 1.000000000000000222, 0.9999999999999997780, 1.000000000000000222, 1.000000000000000222, 1.000000000000000000, 0.9999999999999997780, 1.000000000000000000, 1.000000000000000222, 1.000000000000000000, 1.000000000000000000, 0.9999999999999996669, 1.000000000000000444, 0.9999999999999994449, 1.000000000000000444, 0.9999999999999997780, 1.000000000000000000, 1.000000000000000000, 0.9999999999999997780, 1.000000000000000222, 0.9999999999999997780, 1.000000000000000000, 1.000000000000000444, 0.9999999999999997780, 1.000000000000000000, 0.9999999999999997780, 1.000000000000000000, 1.000000000000000000, 0.9999999999999997780, 0.9999999999999997780, 1.000000000000000000, 1.000000000000000444, 1.000000000000000000, 1.000000000000000444, 1.000000000000000000, 1.000000000000000000, 1.000000000000000000, 0.9999999999999997780, 1.000000000000000000, 1.000000000000000000, 1.000000000000000000, 1.000000000000000000, 0.9999999999999997780, 1.000000000000000222, 1.000000000000000000, 0.9999999999999997780, 1.000000000000000444, 0.9999999999999997780, 1.000000000000000222, 0.9999999999999996669, 1.000000000000000444, 1.000000000000000000, 0.9999999999999997780, 1.000000000000000000, 1.000000000000000000, 1.000000000000000000, 0.9999999999999997780, 1.000000000000000000, 1.000000000000000000, 0.9999999999999997780, 1.000000000000000444, 0.9999999999999997780, 0.9999999999999997780, 1.000000000000000000, 1.000000000000000000, 1.000000000000000222, 1.000000000000000222, 0.9999999999999997780, 1.000000000000000000, 1.000000000000000222, 1.000000000000000000, 0.9999999999999997780, 1.000000000000000222, 1.000000000000000000, 1.000000000000000000, 1.000000000000000000, 0.9999999999999997780, 1.000000000000000000, 1.000000000000000000, 1.000000000000000000, 1.000000000000000000, 0.9999999999999997780, 1.000000000000000666, 0.9999999999999996669, 0.9999999999999996669, 1.000000000000000444, 0.9999999999999996669, 1.000000000000000222, 1.000000000000000000, 1.000000000000000000, 1.000000000000000000, 1.000000000000000000, 1.000000000000000000, 0.9999999999999997780, 1.000000000000000222, 1.000000000000000222, 0.9999999999999996669, 0.9999999999999997780, 1.000000000000000000, 1.000000000000000222, 1.000000000000000222),
 ( 0.3333333333333334259, 0.3333333333333334259, 0.3333333333333333703, 0.3333333333333334259, 0.3333333333333333703, 0.3333333333333332593, 0.3333333333333334814, 0.3333333333333333703, 0.3333333333333334814, 0.3333333333333334259, 0.3333333333333333148, 0.3333333333333333148, 0.3333333333333333703, 0.3333333333333334259, 0.3333333333333332593, 0.3333333333333334814, 0.3333333333333331483, 0.3333333333333334814, 0.3333333333333333148, 0.3333333333333333148, 0.3333333333333334259, 0.3333333333333333703, 0.3333333333333333703, 0.3333333333333333148, 0.3333333333333335369, 0.3333333333333332593, 0.3333333333333333703, 0.3333333333333333703, 0.3333333333333334259, 0.3333333333333333148, 0.3333333333333333148, 0.3333333333333333148, 0.3333333333333334259, 0.3333333333333332593, 0.3333333333333334259, 0.3333333333333334259, 0.3333333333333333148, 0.3333333333333332593, 0.3333333333333333703, 0.3333333333333333703, 0.3333333333333332593, 0.3333333333333334814, 0.3333333333333333703, 0.3333333333333333703, 0.3333333333333333148, 0.3333333333333334259, 0.3333333333333333703, 0.3333333333333333703, 0.3333333333333334814, 0.3333333333333332038, 0.3333333333333334259, 0.3333333333333333703, 0.3333333333333333148, 0.3333333333333333148, 0.3333333333333333703, 0.3333333333333333703, 0.3333333333333333148, 0.3333333333333334814, 0.3333333333333333148, 0.3333333333333333703, 0.3333333333333333148, 0.3333333333333333148, 0.3333333333333334259, 0.3333333333333333703, 0.3333333333333333703, 0.3333333333333334259, 0.3333333333333333148, 0.3333333333333333148, 0.3333333333333333703, 0.3333333333333333703, 0.3333333333333332593, 0.3333333333333333703, 0.3333333333333333703, 0.3333333333333333703, 0.3333333333333333148, 0.3333333333333333148, 0.3333333333333334814, 0.3333333333333333703, 0.3333333333333334259, 0.3333333333333334259, 0.3333333333333334814, 0.3333333333333333148, 0.3333333333333333703, 0.3333333333333334259, 0.3333333333333333148, 0.3333333333333333703, 0.3333333333333333703, 0.3333333333333333703, 0.3333333333333333703, 0.3333333333333333703, 0.3333333333333333148, 0.3333333333333334814, 0.3333333333333332593, 0.3333333333333334259, 0.3333333333333333703, 0.3333333333333333703, 0.3333333333333333148, 0.3333333333333333703, 0.3333333333333334259, 0.3333333333333332593, 0.3333333333333334259, 0.3333333333333333703, 0.3333333333333333148, 0.3333333333333333148, 0.3333333333333332593, 0.3333333333333334259, 0.3333333333333333703, 0.3333333333333333703, 0.3333333333333333148, 0.3333333333333334259, 0.3333333333333333148, 0.3333333333333335369, 0.3333333333333333148, 0.3333333333333333703, 0.3333333333333333703, 0.3333333333333333703, 0.3333333333333334259, 0.3333333333333332593, 0.3333333333333333703, 0.3333333333333333703, 0.3333333333333333703, 0.3333333333333333703, 0.3333333333333333148, 0.3333333333333333703, 0.3333333333333333703, 0.3333333333333334259, 0.3333333333333333703, 0.3333333333333333703, 0.3333333333333335369, 0.3333333333333333148, 0.3333333333333333148, 0.3333333333333333703, 0.3333333333333333703, 0.3333333333333333148, 0.3333333333333334259, 0.3333333333333333148, 0.3333333333333333703, 0.3333333333333333148, 0.3333333333333334814, 0.3333333333333334259, 0.3333333333333333703, 0.3333333333333334259, 0.3333333333333334259, 0.3333333333333332593, 0.3333333333333333703, 0.3333333333333334259, 0.3333333333333334259, 0.3333333333333333148, 0.3333333333333334259, 0.3333333333333333148, 0.3333333333333334259, 0.3333333333333333703, 0.3333333333333333148, 0.3333333333333334814, 0.3333333333333332038, 0.3333333333333333703, 0.3333333333333334259, 0.3333333333333333703, 0.3333333333333333703, 0.3333333333333334814, 0.3333333333333332593, 0.3333333333333334814, 0.3333333333333332593, 0.3333333333333334259, 0.3333333333333334259, 0.3333333333333332593, 0.3333333333333334259, 0.3333333333333334259, 0.3333333333333333148, 0.3333333333333332593, 0.3333333333333334259, 0.3333333333333333148, 0.3333333333333334259, 0.3333333333333333703, 0.3333333333333334259, 0.3333333333333332038, 0.3333333333333334814, 0.3333333333333333148, 0.3333333333333333703, 0.3333333333333334259, 0.3333333333333333703, 0.3333333333333333703, 0.3333333333333334259, 0.3333333333333334259, 0.3333333333333333148, 0.3333333333333334259, 0.3333333333333333148, 0.3333333333333333703, 0.3333333333333333703, 0.3333333333333333148, 0.3333333333333335369, 0.3333333333333333148, 0.3333333333333334259, 0.3333333333333333148, 0.3333333333333334259, 0.3333333333333335369, 0.3333333333333332593, 0.3333333333333333703, 0.3333333333333333148, 0.3333333333333334259, 0.3333333333333333148, 0.3333333333333334814, 0.3333333333333332593, 0.3333333333333333703, 0.3333333333333333148, 0.3333333333333334259, 0.3333333333333333703, 0.3333333333333333148, 0.3333333333333333703, 0.3333333333333334814, 0.3333333333333333148, 0.3333333333333333703, 0.3333333333333333148, 0.3333333333333333703, 0.3333333333333333148, 0.3333333333333333703, 0.3333333333333333148, 0.3333333333333332593, 0.3333333333333334814, 0.3333333333333332593, 0.3333333333333335369, 0.3333333333333333703, 0.3333333333333333703, 0.3333333333333332038, 0.3333333333333335369, 0.3333333333333333703, 0.3333333333333334259, 0.3333333333333333148, 0.3333333333333334259, 0.3333333333333333148, 0.3333333333333334259, 0.3333333333333333703, 0.3333333333333333703, 0.3333333333333333703, 0.3333333333333334814, 0.3333333333333332038, 0.3333333333333334814, 0.3333333333333333148, 0.3333333333333334259, 0.3333333333333333148, 0.3333333333333333703, 0.3333333333333333703, 0.3333333333333333703, 0.3333333333333332593, 0.3333333333333334814, 0.3333333333333333148, 0.3333333333333333703, 0.3333333333333334259, 0.3333333333333333148, 0.3333333333333334259, 0.3333333333333333703, 0.3333333333333334814, 0.3333333333333333148, 0.3333333333333333703, 0.3333333333333334259, 0.3333333333333333703, 0.3333333333333333148, 0.3333333333333334814, 0.3333333333333333703, 0.3333333333333332593, 0.3333333333333335369, 0.3333333333333332038, 0.3333333333333335369, 0.3333333333333333148, 0.3333333333333334259, 0.3333333333333333703, 0.3333333333333333703, 0.3333333333333334259, 0.3333333333333333703, 0.3333333333333333703, 0.3333333333333333703, 0.3333333333333332593, 0.3333333333333334259, 0.3333333333333334259, 0.3333333333333333148, 0.3333333333333333703, 0.3333333333333333148, 0.3333333333333334259, 0.3333333333333334259, 0.3333333333333333148, 0.3333333333333333703, 0.3333333333333333703, 0.3333333333333333703, 0.3333333333333333703, 0.3333333333333334259, 0.3333333333333334259, 0.3333333333333333703, 0.3333333333333334259, 0.3333333333333333148, 0.3333333333333334814, 0.3333333333333334259, 0.3333333333333333148, 0.3333333333333333703, 0.3333333333333333703, 0.3333333333333334259, 0.3333333333333333703, 0.3333333333333333703, 0.3333333333333333148, 0.3333333333333335924, 0.3333333333333332038, 0.3333333333333335924, 0.3333333333333333148, 0.3333333333333333703, 0.3333333333333333148, 0.3333333333333333148, 0.3333333333333334814, 0.3333333333333332038, 0.3333333333333334814, 0.3333333333333334259, 0.3333333333333333703, 0.3333333333333334259, 0.3333333333333333148, 0.3333333333333333703, 0.3333333333333334259, 0.3333333333333333148, 0.3333333333333333148, 0.3333333333333334259, 0.3333333333333334259, 0.3333333333333333148, 0.3333333333333334814, 0.3333333333333333703, 0.3333333333333334259, 0.3333333333333333703, 0.3333333333333333148, 0.3333333333333333703, 0.3333333333333333703, 0.3333333333333333703, 0.3333333333333333703, 0.3333333333333333703, 0.3333333333333334814, 0.3333333333333333148, 0.3333333333333334259, 0.3333333333333334259, 0.3333333333333333148, 0.3333333333333334259, 0.3333333333333332038, 0.3333333333333335369, 0.3333333333333332593, 0.3333333333333333703, 0.3333333333333333703, 0.3333333333333333148, 0.3333333333333334259, 0.3333333333333333148, 0.3333333333333334259, 0.3333333333333333148, 0.3333333333333333703, 0.3333333333333334259, 0.3333333333333333703, 0.3333333333333333148, 0.3333333333333333703, 0.3333333333333333148, 0.3333333333333334259, 0.3333333333333334259, 0.3333333333333333148, 0.3333333333333333148, 0.3333333333333333703, 0.3333333333333333703, 0.3333333333333333703, 0.3333333333333333703, 0.3333333333333334259, 0.3333333333333333148, 0.3333333333333334814, 0.3333333333333332593, 0.3333333333333334259, 0.3333333333333333703, 0.3333333333333333703, 0.3333333333333333703, 0.3333333333333333148, 0.3333333333333335369, 0.3333333333333333703, 0.3333333333333332593, 0.3333333333333334814, 0.3333333333333333703, 0.3333333333333333703, 0.3333333333333333703, 0.3333333333333333703, 0.3333333333333333703, 0.3333333333333333703, 0.3333333333333333703, 0.3333333333333333703, 0.3333333333333333703, 0.3333333333333334259, 0.3333333333333332593, 0.3333333333333333148, 0.3333333333333334259, 0.3333333333333334259, 0.3333333333333334259),
 ( 0.3333333333333334259, 0.3333333333333334259, 0.3333333333333333703, 0.3333333333333334259, 0.3333333333333333703, 0.3333333333333332593, 0.3333333333333334814, 0.3333333333333333703, 0.3333333333333334814, 0.3333333333333334259, 0.3333333333333333148, 0.3333333333333333148, 0.3333333333333333703, 0.3333333333333334259, 0.3333333333333332593, 0.3333333333333334814, 0.3333333333333331483, 0.3333333333333334814, 0.3333333333333333148, 0.3333333333333333148, 0.3333333333333334259, 0.3333333333333333703, 0.3333333333333333703, 0.3333333333333333148, 0.3333333333333335369, 0.3333333333333332593, 0.3333333333333333703, 0.3333333333333333703, 0.3333333333333334259, 0.3333333333333333148, 0.3333333333333333148, 0.3333333333333333148, 0.3333333333333334259, 0.3333333333333332593, 0.3333333333333334259, 0.3333333333333334259, 0.3333333333333333148, 0.3333333333333332593, 0.3333333333333333703, 0.3333333333333333703, 0.3333333333333332593, 0.3333333333333334814, 0.3333333333333333703, 0.3333333333333333703, 0.3333333333333333148, 0.3333333333333334259, 0.3333333333333333703, 0.3333333333333333703, 0.3333333333333334814, 0.3333333333333332038, 0.3333333333333334259, 0.3333333333333333703, 0.3333333333333333148, 0.3333333333333333148, 0.3333333333333333703, 0.3333333333333333703, 0.3333333333333333148, 0.3333333333333334814, 0.3333333333333333148, 0.3333333333333333703, 0.3333333333333333148, 0.3333333333333333148, 0.3333333333333334259, 0.3333333333333333703, 0.3333333333333333703, 0.3333333333333334259, 0.3333333333333333148, 0.3333333333333333148, 0.3333333333333333703, 0.3333333333333333703, 0.3333333333333332593, 0.3333333333333333703, 0.3333333333333333703, 0.3333333333333333703, 0.3333333333333333148, 0.3333333333333333148, 0.3333333333333334814, 0.3333333333333333703, 0.3333333333333334259, 0.3333333333333334259, 0.3333333333333334814, 0.3333333333333333148, 0.3333333333333333703, 0.3333333333333334259, 0.3333333333333333148, 0.3333333333333333703, 0.3333333333333333703, 0.3333333333333333703, 0.3333333333333333703, 0.3333333333333333703, 0.3333333333333333148, 0.3333333333333334814, 0.3333333333333332593, 0.3333333333333334259, 0.3333333333333333703, 0.3333333333333333703, 0.3333333333333333148, 0.3333333333333333703, 0.3333333333333334259, 0.3333333333333332593, 0.3333333333333334259, 0.3333333333333333703, 0.3333333333333333148, 0.3333333333333333148, 0.3333333333333332593, 0.3333333333333334259, 0.3333333333333333703, 0.3333333333333333703, 0.3333333333333333148, 0.3333333333333334259, 0.3333333333333333148, 0.3333333333333335369, 0.3333333333333333148, 0.3333333333333333703, 0.3333333333333333703, 0.3333333333333333703, 0.3333333333333334259, 0.3333333333333332593, 0.3333333333333333703, 0.3333333333333333703, 0.3333333333333333703, 0.3333333333333333703, 0.3333333333333333148, 0.3333333333333333703, 0.3333333333333333703, 0.3333333333333334259, 0.3333333333333333703, 0.3333333333333333703, 0.3333333333333335369, 0.3333333333333333148, 0.3333333333333333148, 0.3333333333333333703, 0.3333333333333333703, 0.3333333333333333148, 0.3333333333333334259, 0.3333333333333333148, 0.3333333333333333703, 0.3333333333333333148, 0.3333333333333334814, 0.3333333333333334259, 0.3333333333333333703, 0.3333333333333334259, 0.3333333333333334259, 0.3333333333333332593, 0.3333333333333333703, 0.3333333333333334259, 0.3333333333333334259, 0.3333333333333333148, 0.3333333333333334259, 0.3333333333333333148, 0.3333333333333334259, 0.3333333333333333703, 0.3333333333333333148, 0.3333333333333334814, 0.3333333333333332038, 0.3333333333333333703, 0.3333333333333334259, 0.3333333333333333703, 0.3333333333333333703, 0.3333333333333334814, 0.3333333333333332593, 0.3333333333333334814, 0.3333333333333332593, 0.3333333333333334259, 0.3333333333333334259, 0.3333333333333332593, 0.3333333333333334259, 0.3333333333333334259, 0.3333333333333333148, 0.3333333333333332593, 0.3333333333333334259, 0.3333333333333333148, 0.3333333333333334259, 0.3333333333333333703, 0.3333333333333334259, 0.3333333333333332038, 0.3333333333333334814, 0.3333333333333333148, 0.3333333333333333703, 0.3333333333333334259, 0.3333333333333333703, 0.3333333333333333703, 0.3333333333333334259, 0.3333333333333334259, 0.3333333333333333148, 0.3333333333333334259, 0.3333333333333333148, 0.3333333333333333703, 0.3333333333333333703, 0.3333333333333333148, 0.3333333333333335369, 0.3333333333333333148, 0.3333333333333334259, 0.3333333333333333148, 0.3333333333333334259, 0.3333333333333335369, 0.3333333333333332593, 0.3333333333333333703, 0.3333333333333333148, 0.3333333333333334259, 0.3333333333333333148, 0.3333333333333334814, 0.3333333333333332593, 0.3333333333333333703, 0.3333333333333333148, 0.3333333333333334259, 0.3333333333333333703, 0.3333333333333333148, 0.3333333333333333703, 0.3333333333333334814, 0.3333333333333333148, 0.3333333333333333703, 0.3333333333333333148, 0.3333333333333333703, 0.3333333333333333148, 0.3333333333333333703, 0.3333333333333333148, 0.3333333333333332593, 0.3333333333333334814, 0.3333333333333332593, 0.3333333333333335369, 0.3333333333333333703, 0.3333333333333333703, 0.3333333333333332038, 0.3333333333333335369, 0.3333333333333333703, 0.3333333333333334259, 0.3333333333333333148, 0.3333333333333334259, 0.3333333333333333148, 0.3333333333333334259, 0.3333333333333333703, 0.3333333333333333703, 0.3333333333333333703, 0.3333333333333334814, 0.3333333333333332038, 0.3333333333333334814, 0.3333333333333333148, 0.3333333333333334259, 0.3333333333333333148, 0.3333333333333333703, 0.3333333333333333703, 0.3333333333333333703, 0.3333333333333332593, 0.3333333333333334814, 0.3333333333333333148, 0.3333333333333333703, 0.3333333333333334259, 0.3333333333333333148, 0.3333333333333334259, 0.3333333333333333703, 0.3333333333333334814, 0.3333333333333333148, 0.3333333333333333703, 0.3333333333333334259, 0.3333333333333333703, 0.3333333333333333148, 0.3333333333333334814, 0.3333333333333333703, 0.3333333333333332593, 0.3333333333333335369, 0.3333333333333332038, 0.3333333333333335369, 0.3333333333333333148, 0.3333333333333334259, 0.3333333333333333703, 0.3333333333333333703, 0.3333333333333334259, 0.3333333333333333703, 0.3333333333333333703, 0.3333333333333333703, 0.3333333333333332593, 0.3333333333333334259, 0.3333333333333334259, 0.3333333333333333148, 0.3333333333333333703, 0.3333333333333333148, 0.3333333333333334259, 0.3333333333333334259, 0.3333333333333333148, 0.3333333333333333703, 0.3333333333333333703, 0.3333333333333333703, 0.3333333333333333703, 0.3333333333333334259, 0.3333333333333334259, 0.3333333333333333703, 0.3333333333333334259, 0.3333333333333333148, 0.3333333333333334814, 0.3333333333333334259, 0.3333333333333333148, 0.3333333333333333703, 0.3333333333333333703, 0.3333333333333334259, 0.3333333333333333703, 0.3333333333333333703, 0.3333333333333333148, 0.3333333333333335924, 0.3333333333333332038, 0.3333333333333335924, 0.3333333333333333148, 0.3333333333333333703, 0.3333333333333333148, 0.3333333333333333148, 0.3333333333333334814, 0.3333333333333332038, 0.3333333333333334814, 0.3333333333333334259, 0.3333333333333333703, 0.3333333333333334259, 0.3333333333333333148, 0.3333333333333333703, 0.3333333333333334259, 0.3333333333333333148, 0.3333333333333333148, 0.3333333333333334259, 0.3333333333333334259, 0.3333333333333333148, 0.3333333333333334814, 0.3333333333333333703, 0.3333333333333334259, 0.3333333333333333703, 0.3333333333333333148, 0.3333333333333333703, 0.3333333333333333703, 0.3333333333333333703, 0.3333333333333333703, 0.3333333333333333703, 0.3333333333333334814, 0.3333333333333333148, 0.3333333333333334259, 0.3333333333333334259, 0.3333333333333333148, 0.3333333333333334259, 0.3333333333333332038, 0.3333333333333335369, 0.3333333333333332593, 0.3333333333333333703, 0.3333333333333333703, 0.3333333333333333148, 0.3333333333333334259, 0.3333333333333333148, 0.3333333333333334259, 0.3333333333333333148, 0.3333333333333333703, 0.3333333333333334259, 0.3333333333333333703, 0.3333333333333333148, 0.3333333333333333703, 0.3333333333333333148, 0.3333333333333334259, 0.3333333333333334259, 0.3333333333333333148, 0.3333333333333333148, 0.3333333333333333703, 0.3333333333333333703, 0.3333333333333333703, 0.3333333333333333703, 0.3333333333333334259, 0.3333333333333333148, 0.3333333333333334814, 0.3333333333333332593, 0.3333333333333334259, 0.3333333333333333703, 0.3333333333333333703, 0.3333333333333333703, 0.3333333333333333148, 0.3333333333333335369, 0.3333333333333333703, 0.3333333333333332593, 0.3333333333333334814, 0.3333333333333333703, 0.3333333333333333703, 0.3333333333333333703, 0.3333333333333333703, 0.3333333333333333703, 0.3333333333333333703, 0.3333333333333333703, 0.3333333333333333703, 0.3333333333333333703, 0.3333333333333334259, 0.3333333333333332593, 0.3333333333333333148, 0.3333333333333334259, 0.3333333333333334259, 0.3333333333333334259),
 ( 1.000000000000000222, 1.000000000000000222, 1.000000000000000000, 1.000000000000000222, 1.000000000000000000, 0.9999999999999997780, 1.000000000000000222, 1.000000000000000000, 1.000000000000000222, 1.000000000000000222, 1.000000000000000000, 0.9999999999999997780, 1.000000000000000000, 1.000000000000000222, 0.9999999999999997780, 1.000000000000000222, 0.9999999999999994449, 1.000000000000000444, 0.9999999999999996669, 1.000000000000000000, 1.000000000000000222, 1.000000000000000000, 1.000000000000000000, 0.9999999999999997780, 1.000000000000000444, 0.9999999999999996669, 1.000000000000000000, 1.000000000000000222, 0.9999999999999997780, 1.000000000000000000, 0.9999999999999997780, 0.9999999999999997780, 1.000000000000000444, 0.9999999999999994449, 1.000000000000000444, 0.9999999999999997780, 0.9999999999999997780, 0.9999999999999996669, 1.000000000000000222, 1.000000000000000000, 0.9999999999999997780, 1.000000000000000222, 0.9999999999999997780, 1.000000000000000222, 1.000000000000000000, 1.000000000000000222, 1.000000000000000000, 1.000000000000000000, 1.000000000000000444, 0.9999999999999996669, 0.9999999999999997780, 1.000000000000000000, 0.9999999999999997780, 0.9999999999999997780, 1.000000000000000000, 1.000000000000000000, 0.9999999999999997780, 1.000000000000000444, 1.000000000000000000, 0.9999999999999997780, 1.000000000000000222, 0.9999999999999996669, 1.000000000000000222, 1.000000000000000000, 0.9999999999999997780, 1.000000000000000222, 0.9999999999999997780, 1.000000000000000000, 0.9999999999999997780, 1.000000000000000222, 0.9999999999999996669, 1.000000000000000000, 1.000000000000000222, 0.9999999999999997780, 1.000000000000000222, 0.9999999999999996669, 1.000000000000000444, 1.000000000000000000, 1.000000000000000000, 1.000000000000000222, 1.000000000000000222, 1.000000000000000000, 0.9999999999999997780, 1.000000000000000222, 0.9999999999999997780, 1.000000000000000000, 1.000000000000000000, 1.000000000000000000, 0.9999999999999997780, 1.000000000000000000, 0.9999999999999997780, 1.000000000000000222, 0.9999999999999997780, 1.000000000000000000, 1.000000000000000222, 0.9999999999999997780, 1.000000000000000000, 0.9999999999999996669, 1.000000000000000444, 0.9999999999999997780, 1.000000000000000000, 1.000000000000000000, 1.000000000000000000, 0.9999999999999997780, 0.9999999999999997780, 1.000000000000000222, 1.000000000000000222, 0.9999999999999997780, 1.000000000000000000, 1.000000000000000000, 1.000000000000000222, 1.000000000000000222, 1.000000000000000000, 0.9999999999999997780, 1.000000000000000222, 1.000000000000000000, 1.000000000000000000, 0.9999999999999997780, 0.9999999999999997780, 1.000000000000000222, 1.000000000000000000, 1.000000000000000000, 1.000000000000000000, 0.9999999999999997780, 1.000000000000000222, 1.000000000000000000, 1.000000000000000000, 1.000000000000000000, 1.000000000000000444, 0.9999999999999997780, 0.9999999999999997780, 1.000000000000000000, 1.000000000000000000, 0.9999999999999997780, 1.000000000000000222, 0.9999999999999997780, 1.000000000000000222, 1.000000000000000000, 1.000000000000000222, 1.000000000000000222, 1.000000000000000000, 1.000000000000000222, 1.000000000000000000, 0.9999999999999996669, 1.000000000000000222, 0.9999999999999997780, 1.000000000000000444, 0.9999999999999997780, 1.000000000000000000, 0.9999999999999997780, 1.000000000000000222, 1.000000000000000000, 0.9999999999999997780, 1.000000000000000222, 0.9999999999999994449, 1.000000000000000000, 1.000000000000000222, 1.000000000000000222, 0.9999999999999997780, 1.000000000000000444, 0.9999999999999997780, 1.000000000000000222, 0.9999999999999997780, 1.000000000000000222, 0.9999999999999997780, 1.000000000000000000, 1.000000000000000000, 1.000000000000000222, 0.9999999999999997780, 0.9999999999999996669, 1.000000000000000444, 0.9999999999999997780, 1.000000000000000222, 1.000000000000000000, 1.000000000000000222, 0.9999999999999994449, 1.000000000000000444, 0.9999999999999997780, 1.000000000000000000, 1.000000000000000222, 1.000000000000000000, 1.000000000000000000, 0.9999999999999997780, 1.000000000000000444, 0.9999999999999997780, 1.000000000000000444, 0.9999999999999997780, 1.000000000000000000, 1.000000000000000222, 0.9999999999999996669, 1.000000000000000222, 1.000000000000000000, 1.000000000000000000, 0.9999999999999996669, 1.000000000000000222, 1.000000000000000444, 0.9999999999999997780, 1.000000000000000222, 0.9999999999999996669, 1.000000000000000444, 0.9999999999999997780, 1.000000000000000444, 0.9999999999999996669, 0.9999999999999997780, 1.000000000000000000, 0.9999999999999997780, 1.000000000000000000, 1.000000000000000000, 1.000000000000000000, 1.000000000000000000, 0.9999999999999997780, 1.000000000000000000, 0.9999999999999997780, 1.000000000000000000, 1.000000000000000000, 1.000000000000000000, 1.000000000000000000, 0.9999999999999997780, 1.000000000000000222, 0.9999999999999997780, 1.000000000000000222, 0.9999999999999997780, 1.000000000000000222, 0.9999999999999994449, 1.000000000000000444, 1.000000000000000000, 1.000000000000000222, 0.9999999999999997780, 1.000000000000000000, 0.9999999999999997780, 1.000000000000000222, 1.000000000000000000, 1.000000000000000000, 1.000000000000000222, 1.000000000000000222, 0.9999999999999996669, 1.000000000000000444, 0.9999999999999996669, 1.000000000000000444, 0.9999999999999996669, 1.000000000000000000, 1.000000000000000000, 1.000000000000000000, 0.9999999999999997780, 1.000000000000000222, 0.9999999999999997780, 1.000000000000000222, 1.000000000000000000, 0.9999999999999997780, 1.000000000000000000, 1.000000000000000222, 1.000000000000000222, 1.000000000000000000, 1.000000000000000000, 1.000000000000000000, 1.000000000000000000, 0.9999999999999997780, 1.000000000000000444, 1.000000000000000000, 0.9999999999999997780, 1.000000000000000222, 0.9999999999999996669, 1.000000000000000444, 1.000000000000000000, 1.000000000000000222, 1.000000000000000222, 0.9999999999999997780, 1.000000000000000222, 0.9999999999999997780, 1.000000000000000000, 1.000000000000000000, 0.9999999999999997780, 1.000000000000000000, 1.000000000000000000, 0.9999999999999997780, 1.000000000000000222, 1.000000000000000000, 1.000000000000000000, 1.000000000000000222, 1.000000000000000000, 1.000000000000000000, 1.000000000000000000, 1.000000000000000222, 0.9999999999999997780, 1.000000000000000222, 1.000000000000000000, 0.9999999999999997780, 1.000000000000000222, 0.9999999999999997780, 1.000000000000000222, 1.000000000000000222, 1.000000000000000000, 0.9999999999999997780, 1.000000000000000000, 1.000000000000000222, 1.000000000000000000, 1.000000000000000000, 0.9999999999999996669, 1.000000000000000444, 0.9999999999999994449, 1.000000000000000444, 0.9999999999999997780, 1.000000000000000000, 1.000000000000000000, 0.9999999999999997780, 1.000000000000000222, 0.9999999999999997780, 1.000000000000000000, 1.000000000000000444, 0.9999999999999997780, 1.000000000000000000, 0.9999999999999997780, 1.000000000000000000, 1.000000000000000000, 0.9999999999999997780, 0.9999999999999997780, 1.000000000000000000, 1.000000000000000444, 1.000000000000000000, 1.000000000000000444, 1.000000000000000000, 1.000000000000000000, 1.000000000000000000, 0.9999999999999997780, 1.000000000000000000, 1.000000000000000000, 1.000000000000000000, 1.000000000000000000, 0.9999999999999997780, 1.000000000000000222, 1.000000000000000000, 0.9999999999999997780, 1.000000000000000444, 0.9999999999999997780, 1.000000000000000222, 0.9999999999999996669, 1.000000000000000444, 1.000000000000000000, 0.9999999999999997780, 1.000000000000000000, 1.000000000000000000, 1.000000000000000000, 0.9999999999999997780, 1.000000000000000000, 1.000000000000000000, 0.9999999999999997780, 1.000000000000000444, 0.9999999999999997780, 0.9999999999999997780, 1.000000000000000000, 1.000000000000000000, 1.000000000000000222, 1.000000000000000222, 0.9999999999999997780, 1.000000000000000000, 1.000000000000000222, 1.000000000000000000, 0.9999999999999997780, 1.000000000000000222, 1.000000000000000000, 1.000000000000000000, 1.000000000000000000, 0.9999999999999997780, 1.000000000000000000, 1.000000000000000000, 1.000000000000000000, 1.000000000000000000, 0.9999999999999997780, 1.000000000000000666, 0.9999999999999996669, 0.9999999999999996669, 1.000000000000000444, 0.9999999999999996669, 1.000000000000000222, 1.000000000000000000, 1.000000000000000000, 1.000000000000000000, 1.000000000000000000, 1.000000000000000000, 0.9999999999999997780, 1.000000000000000222, 1.000000000000000222, 0.9999999999999996669, 0.9999999999999997780, 1.000000000000000000, 1.000000000000000222, 1.000000000000000222),
 ( 0.3333333333333334259, 0.3333333333333334259, 0.3333333333333333703, 0.3333333333333334259, 0.3333333333333333703, 0.3333333333333332593, 0.3333333333333334814, 0.3333333333333333703, 0.3333333333333334814, 0.3333333333333334259, 0.3333333333333333148, 0.3333333333333333148, 0.3333333333333333703, 0.3333333333333334259, 0.3333333333333332593, 0.3333333333333334814, 0.3333333333333331483, 0.3333333333333334814, 0.3333333333333333148, 0.3333333333333333148, 0.3333333333333334259, 0.3333333333333333703, 0.3333333333333333703, 0.3333333333333333148, 0.3333333333333335369, 0.3333333333333332593, 0.3333333333333333703, 0.3333333333333333703, 0.3333333333333334259, 0.3333333333333333148, 0.3333333333333333148, 0.3333333333333333148, 0.3333333333333334259, 0.3333333333333332593, 0.3333333333333334259, 0.3333333333333334259, 0.3333333333333333148, 0.3333333333333332593, 0.3333333333333333703, 0.3333333333333333703, 0.3333333333333332593, 0.3333333333333334814, 0.3333333333333333703, 0.3333333333333333703, 0.3333333333333333148, 0.3333333333333334259, 0.3333333333333333703, 0.3333333333333333703, 0.3333333333333334814, 0.3333333333333332038, 0.3333333333333334259, 0.3333333333333333703, 0.3333333333333333148, 0.3333333333333333148, 0.3333333333333333703, 0.3333333333333333703, 0.3333333333333333148, 0.3333333333333334814, 0.3333333333333333148, 0.3333333333333333703, 0.3333333333333333148, 0.3333333333333333148, 0.3333333333333334259, 0.3333333333333333703, 0.3333333333333333703, 0.3333333333333334259, 0.3333333333333333148, 0.3333333333333333148, 0.3333333333333333703, 0.3333333333333333703, 0.3333333333333332593, 0.3333333333333333703, 0.3333333333333333703, 0.3333333333333333703, 0.3333333333333333148, 0.3333333333333333148, 0.3333333333333334814, 0.3333333333333333703, 0.3333333333333334259, 0.3333333333333334259, 0.3333333333333334814, 0.3333333333333333148, 0.3333333333333333703, 0.3333333333333334259, 0.3333333333333333148, 0.3333333333333333703, 0.3333333333333333703, 0.3333333333333333703, 0.3333333333333333703, 0.3333333333333333703, 0.3333333333333333148, 0.3333333333333334814, 0.3333333333333332593, 0.3333333333333334259, 0.3333333333333333703, 0.3333333333333333703, 0.3333333333333333148, 0.3333333333333333703, 0.3333333333333334259, 0.3333333333333332593, 0.3333333333333334259, 0.3333333333333333703, 0.3333333333333333148, 0.3333333333333333148, 0.3333333333333332593, 0.3333333333333334259, 0.3333333333333333703, 0.3333333333333333703, 0.3333333333333333148, 0.3333333333333334259, 0.3333333333333333148, 0.3333333333333335369, 0.3333333333333333148, 0.3333333333333333703, 0.3333333333333333703, 0.3333333333333333703, 0.3333333333333334259, 0.3333333333333332593, 0.3333333333333333703, 0.3333333333333333703, 0.3333333333333333703, 0.3333333333333333703, 0.3333333333333333148, 0.3333333333333333703, 0.3333333333333333703, 0.3333333333333334259, 0.3333333333333333703, 0.3333333333333333703, 0.3333333333333335369, 0.3333333333333333148, 0.3333333333333333148, 0.3333333333333333703, 0.3333333333333333703, 0.3333333333333333148, 0.3333333333333334259, 0.3333333333333333148, 0.3333333333333333703, 0.3333333333333333148, 0.3333333333333334814, 0.3333333333333334259, 0.3333333333333333703, 0.3333333333333334259, 0.3333333333333334259, 0.3333333333333332593, 0.3333333333333333703, 0.3333333333333334259, 0.3333333333333334259, 0.3333333333333333148, 0.3333333333333334259, 0.3333333333333333148, 0.3333333333333334259, 0.3333333333333333703, 0.3333333333333333148, 0.3333333333333334814, 0.3333333333333332038, 0.3333333333333333703, 0.3333333333333334259, 0.3333333333333333703, 0.3333333333333333703, 0.3333333333333334814, 0.3333333333333332593, 0.3333333333333334814, 0.3333333333333332593, 0.3333333333333334259, 0.3333333333333334259, 0.3333333333333332593, 0.3333333333333334259, 0.3333333333333334259, 0.3333333333333333148, 0.3333333333333332593, 0.3333333333333334259, 0.3333333333333333148, 0.3333333333333334259, 0.3333333333333333703, 0.3333333333333334259, 0.3333333333333332038, 0.3333333333333334814, 0.3333333333333333148, 0.3333333333333333703, 0.3333333333333334259, 0.3333333333333333703, 0.3333333333333333703, 0.3333333333333334259, 0.3333333333333334259, 0.3333333333333333148, 0.3333333333333334259, 0.3333333333333333148, 0.3333333333333333703, 0.3333333333333333703, 0.3333333333333333148, 0.3333333333333335369, 0.3333333333333333148, 0.3333333333333334259, 0.3333333333333333148, 0.3333333333333334259, 0.3333333333333335369, 0.3333333333333332593, 0.3333333333333333703, 0.3333333333333333148, 0.3333333333333334259, 0.3333333333333333148, 0.3333333333333334814, 0.3333333333333332593, 0.3333333333333333703, 0.3333333333333333148, 0.3333333333333334259, 0.3333333333333333703, 0.3333333333333333148, 0.3333333333333333703, 0.3333333333333334814, 0.3333333333333333148, 0.3333333333333333703, 0.3333333333333333148, 0.3333333333333333703, 0.3333333333333333148, 0.3333333333333333703, 0.3333333333333333148, 0.3333333333333332593, 0.3333333333333334814, 0.3333333333333332593, 0.3333333333333335369, 0.3333333333333333703, 0.3333333333333333703, 0.3333333333333332038, 0.3333333333333335369, 0.3333333333333333703, 0.3333333333333334259, 0.3333333333333333148, 0.3333333333333334259, 0.3333333333333333148, 0.3333333333333334259, 0.3333333333333333703, 0.3333333333333333703, 0.3333333333333333703, 0.3333333333333334814, 0.3333333333333332038, 0.3333333333333334814, 0.3333333333333333148, 0.3333333333333334259, 0.3333333333333333148, 0.3333333333333333703, 0.3333333333333333703, 0.3333333333333333703, 0.3333333333333332593, 0.3333333333333334814, 0.3333333333333333148, 0.3333333333333333703, 0.3333333333333334259, 0.3333333333333333148, 0.3333333333333334259, 0.3333333333333333703, 0.3333333333333334814, 0.3333333333333333148, 0.3333333333333333703, 0.3333333333333334259, 0.3333333333333333703, 0.3333333333333333148, 0.3333333333333334814, 0.3333333333333333703, 0.3333333333333332593, 0.3333333333333335369, 0.3333333333333332038, 0.3333333333333335369, 0.3333333333333333148, 0.3333333333333334259, 0.3333333333333333703, 0.3333333333333333703, 0.3333333333333334259, 0.3333333333333333703, 0.3333333333333333703, 0.3333333333333333703, 0.3333333333333332593, 0.3333333333333334259, 0.3333333333333334259, 0.3333333333333333148, 0.3333333333333333703, 0.3333333333333333148, 0.3333333333333334259, 0.3333333333333334259, 0.3333333333333333148, 0.3333333333333333703, 0.3333333333333333703, 0.3333333333333333703, 0.3333333333333333703, 0.3333333333333334259, 0.3333333333333334259, 0.3333333333333333703, 0.3333333333333334259, 0.3333333333333333148, 0.3333333333333334814, 0.3333333333333334259, 0.3333333333333333148, 0.3333333333333333703, 0.3333333333333333703, 0.3333333333333334259, 0.3333333333333333703, 0.3333333333333333703, 0.3333333333333333148, 0.3333333333333335924, 0.3333333333333332038, 0.3333333333333335924, 0.3333333333333333148, 0.3333333333333333703, 0.3333333333333333148, 0.3333333333333333148, 0.3333333333333334814, 0.3333333333333332038, 0.3333333333333334814, 0.3333333333333334259, 0.3333333333333333703, 0.3333333333333334259, 0.3333333333333333148, 0.3333333333333333703, 0.3333333333333334259, 0.3333333333333333148, 0.3333333333333333148, 0.3333333333333334259, 0.3333333333333334259, 0.3333333333333333148, 0.3333333333333334814, 0.3333333333333333703, 0.3333333333333334259, 0.3333333333333333703, 0.3333333333333333148, 0.3333333333333333703, 0.3333333333333333703, 0.3333333333333333703, 0.3333333333333333703, 0.3333333333333333703, 0.3333333333333334814, 0.3333333333333333148, 0.3333333333333334259, 0.3333333333333334259, 0.3333333333333333148, 0.3333333333333334259, 0.3333333333333332038, 0.3333333333333335369, 0.3333333333333332593, 0.3333333333333333703, 0.3333333333333333703, 0.3333333333333333148, 0.3333333333333334259, 0.3333333333333333148, 0.3333333333333334259, 0.3333333333333333148, 0.3333333333333333703, 0.3333333333333334259, 0.3333333333333333703, 0.3333333333333333148, 0.3333333333333333703, 0.3333333333333333148, 0.3333333333333334259, 0.3333333333333334259, 0.3333333333333333148, 0.3333333333333333148, 0.3333333333333333703, 0.3333333333333333703, 0.3333333333333333703, 0.3333333333333333703, 0.3333333333333334259, 0.3333333333333333148, 0.3333333333333334814, 0.3333333333333332593, 0.3333333333333334259, 0.3333333333333333703, 0.3333333333333333703, 0.3333333333333333703, 0.3333333333333333148, 0.3333333333333335369, 0.3333333333333333703, 0.3333333333333332593, 0.3333333333333334814, 0.3333333333333333703, 0.3333333333333333703, 0.3333333333333333703, 0.3333333333333333703, 0.3333333333333333703, 0.3333333333333333703, 0.3333333333333333703, 0.3333333333333333703, 0.3333333333333333703, 0.3333333333333334259, 0.3333333333333332593, 0.3333333333333333148, 0.3333333333333334259, 0.3333333333333334259, 0.3333333333333334259),
 ( 0.3333333333333334259, 0.3333333333333334259, 0.3333333333333333703, 0.3333333333333334259, 0.3333333333333333703, 0.3333333333333332593, 0.3333333333333334814, 0.3333333333333333703, 0.3333333333333334814, 0.3333333333333334259, 0.3333333333333333148, 0.3333333333333333148, 0.3333333333333333703, 0.3333333333333334259, 0.3333333333333332593, 0.3333333333333334814, 0.3333333333333331483, 0.3333333333333334814, 0.3333333333333333148, 0.3333333333333333148, 0.3333333333333334259, 0.3333333333333333703, 0.3333333333333333703, 0.3333333333333333148, 0.3333333333333335369, 0.3333333333333332593, 0.3333333333333333703, 0.3333333333333333703, 0.3333333333333334259, 0.3333333333333333148, 0.3333333333333333148, 0.3333333333333333148, 0.3333333333333334259, 0.3333333333333332593, 0.3333333333333334259, 0.3333333333333334259, 0.3333333333333333148, 0.3333333333333332593, 0.3333333333333333703, 0.3333333333333333703, 0.3333333333333332593, 0.3333333333333334814, 0.3333333333333333703, 0.3333333333333333703, 0.3333333333333333148, 0.3333333333333334259, 0.3333333333333333703, 0.3333333333333333703, 0.3333333333333334814, 0.3333333333333332038, 0.3333333333333334259, 0.3333333333333333703, 0.3333333333333333148, 0.3333333333333333148, 0.3333333333333333703, 0.3333333333333333703, 0.3333333333333333148, 0.3333333333333334814, 0.3333333333333333148, 0.3333333333333333703, 0.3333333333333333148, 0.3333333333333333148, 0.3333333333333334259, 0.3333333333333333703, 0.3333333333333333703, 0.3333333333333334259, 0.3333333333333333148, 0.3333333333333333148, 0.3333333333333333703, 0.3333333333333333703, 0.3333333333333332593, 0.3333333333333333703, 0.3333333333333333703, 0.3333333333333333703, 0.3333333333333333148, 0.3333333333333333148, 0.3333333333333334814, 0.3333333333333333703, 0.3333333333333334259, 0.3333333333333334259, 0.3333333333333334814, 0.3333333333333333148, 0.3333333333333333703, 0.3333333333333334259, 0.3333333333333333148, 0.3333333333333333703, 0.3333333333333333703, 0.3333333333333333703, 0.3333333333333333703, 0.3333333333333333703, 0.3333333333333333148, 0.3333333333333334814, 0.3333333333333332593, 0.3333333333333334259, 0.3333333333333333703, 0.3333333333333333703, 0.3333333333333333148, 0.3333333333333333703, 0.3333333333333334259, 0.3333333333333332593, 0.3333333333333334259, 0.3333333333333333703, 0.3333333333333333148, 0.3333333333333333148, 0.3333333333333332593, 0.3333333333333334259, 0.3333333333333333703, 0.3333333333333333703, 0.3333333333333333148, 0.3333333333333334259, 0.3333333333333333148, 0.3333333333333335369, 0.3333333333333333148, 0.3333333333333333703, 0.3333333333333333703, 0.3333333333333333703, 0.3333333333333334259, 0.3333333333333332593, 0.3333333333333333703, 0.3333333333333333703, 0.3333333333333333703, 0.3333333333333333703, 0.3333333333333333148, 0.3333333333333333703, 0.3333333333333333703, 0.3333333333333334259, 0.3333333333333333703, 0.3333333333333333703, 0.3333333333333335369, 0.3333333333333333148, 0.3333333333333333148, 0.3333333333333333703, 0.3333333333333333703, 0.3333333333333333148, 0.3333333333333334259, 0.3333333333333333148, 0.3333333333333333703, 0.3333333333333333148, 0.3333333333333334814, 0.3333333333333334259, 0.3333333333333333703, 0.3333333333333334259, 0.3333333333333334259, 0.3333333333333332593, 0.3333333333333333703, 0.3333333333333334259, 0.3333333333333334259, 0.3333333333333333148, 0.3333333333333334259, 0.3333333333333333148, 0.3333333333333334259, 0.3333333333333333703, 0.3333333333333333148, 0.3333333333333334814, 0.3333333333333332038, 0.3333333333333333703, 0.3333333333333334259, 0.3333333333333333703, 0.3333333333333333703, 0.3333333333333334814, 0.3333333333333332593, 0.3333333333333334814, 0.3333333333333332593, 0.3333333333333334259, 0.3333333333333334259, 0.3333333333333332593, 0.3333333333333334259, 0.3333333333333334259, 0.3333333333333333148, 0.3333333333333332593, 0.3333333333333334259, 0.3333333333333333148, 0.3333333333333334259, 0.3333333333333333703, 0.3333333333333334259, 0.3333333333333332038, 0.3333333333333334814, 0.3333333333333333148, 0.3333333333333333703, 0.3333333333333334259, 0.3333333333333333703, 0.3333333333333333703, 0.3333333333333334259, 0.3333333333333334259, 0.3333333333333333148, 0.3333333333333334259, 0.3333333333333333148, 0.3333333333333333703, 0.3333333333333333703, 0.3333333333333333148, 0.3333333333333335369, 0.3333333333333333148, 0.3333333333333334259, 0.3333333333333333148, 0.3333333333333334259, 0.3333333333333335369, 0.3333333333333332593, 0.3333333333333333703, 0.3333333333333333148, 0.3333333333333334259, 0.3333333333333333148, 0.3333333333333334814, 0.3333333333333332593, 0.3333333333333333703, 0.3333333333333333148, 0.3333333333333334259, 0.3333333333333333703, 0.3333333333333333148, 0.3333333333333333703, 0.3333333333333334814, 0.3333333333333333148, 0.3333333333333333703, 0.3333333333333333148, 0.3333333333333333703, 0.3333333333333333148, 0.3333333333333333703, 0.3333333333333333148, 0.3333333333333332593, 0.3333333333333334814, 0.3333333333333332593, 0.3333333333333335369, 0.3333333333333333703, 0.3333333333333333703, 0.3333333333333332038, 0.3333333333333335369, 0.3333333333333333703, 0.3333333333333334259, 0.3333333333333333148, 0.3333333333333334259, 0.3333333333333333148, 0.3333333333333334259, 0.3333333333333333703, 0.3333333333333333703, 0.3333333333333333703, 0.3333333333333334814, 0.3333333333333332038, 0.3333333333333334814, 0.3333333333333333148, 0.3333333333333334259, 0.3333333333333333148, 0.3333333333333333703, 0.3333333333333333703, 0.3333333333333333703, 0.3333333333333332593, 0.3333333333333334814, 0.3333333333333333148, 0.3333333333333333703, 0.3333333333333334259, 0.3333333333333333148, 0.3333333333333334259, 0.3333333333333333703, 0.3333333333333334814, 0.3333333333333333148, 0.3333333333333333703, 0.3333333333333334259, 0.3333333333333333703, 0.3333333333333333148, 0.3333333333333334814, 0.3333333333333333703, 0.3333333333333332593, 0.3333333333333335369, 0.3333333333333332038, 0.3333333333333335369, 0.3333333333333333148, 0.3333333333333334259, 0.3333333333333333703, 0.3333333333333333703, 0.3333333333333334259, 0.3333333333333333703, 0.3333333333333333703, 0.3333333333333333703, 0.3333333333333332593, 0.3333333333333334259, 0.3333333333333334259, 0.3333333333333333148, 0.3333333333333333703, 0.3333333333333333148, 0.3333333333333334259, 0.3333333333333334259, 0.3333333333333333148, 0.3333333333333333703, 0.3333333333333333703, 0.3333333333333333703, 0.3333333333333333703, 0.3333333333333334259, 0.3333333333333334259, 0.3333333333333333703, 0.3333333333333334259, 0.3333333333333333148, 0.3333333333333334814, 0.3333333333333334259, 0.3333333333333333148, 0.3333333333333333703, 0.3333333333333333703, 0.3333333333333334259, 0.3333333333333333703, 0.3333333333333333703, 0.3333333333333333148, 0.3333333333333335924, 0.3333333333333332038, 0.3333333333333335924, 0.3333333333333333148, 0.3333333333333333703, 0.3333333333333333148, 0.3333333333333333148, 0.3333333333333334814, 0.3333333333333332038, 0.3333333333333334814, 0.3333333333333334259, 0.3333333333333333703, 0.3333333333333334259, 0.3333333333333333148, 0.3333333333333333703, 0.3333333333333334259, 0.3333333333333333148, 0.3333333333333333148, 0.3333333333333334259, 0.3333333333333334259, 0.3333333333333333148, 0.3333333333333334814, 0.3333333333333333703, 0.3333333333333334259, 0.3333333333333333703, 0.3333333333333333148, 0.3333333333333333703, 0.3333333333333333703, 0.3333333333333333703, 0.3333333333333333703, 0.3333333333333333703, 0.3333333333333334814, 0.3333333333333333148, 0.3333333333333334259, 0.3333333333333334259, 0.3333333333333333148, 0.3333333333333334259, 0.3333333333333332038, 0.3333333333333335369, 0.3333333333333332593, 0.3333333333333333703, 0.3333333333333333703, 0.3333333333333333148, 0.3333333333333334259, 0.3333333333333333148, 0.3333333333333334259, 0.3333333333333333148, 0.3333333333333333703, 0.3333333333333334259, 0.3333333333333333703, 0.3333333333333333148, 0.3333333333333333703, 0.3333333333333333148, 0.3333333333333334259, 0.3333333333333334259, 0.3333333333333333148, 0.3333333333333333148, 0.3333333333333333703, 0.3333333333333333703, 0.3333333333333333703, 0.3333333333333333703, 0.3333333333333334259, 0.3333333333333333148, 0.3333333333333334814, 0.3333333333333332593, 0.3333333333333334259, 0.3333333333333333703, 0.3333333333333333703, 0.3333333333333333703, 0.3333333333333333148, 0.3333333333333335369, 0.3333333333333333703, 0.3333333333333332593, 0.3333333333333334814, 0.3333333333333333703, 0.3333333333333333703, 0.3333333333333333703, 0.3333333333333333703, 0.3333333333333333703, 0.3333333333333333703, 0.3333333333333333703, 0.3333333333333333703, 0.3333333333333333703, 0.3333333333333334259, 0.3333333333333332593, 0.3333333333333333148, 0.3333333333333334259, 0.3333333333333334259, 0.3333333333333334259),
 ( 1.000000000000000222, 1.000000000000000222, 1.000000000000000000, 1.000000000000000222, 1.000000000000000000, 0.9999999999999997780, 1.000000000000000222, 1.000000000000000000, 1.000000000000000222, 1.000000000000000222, 1.000000000000000000, 0.9999999999999997780, 1.000000000000000000, 1.000000000000000222, 0.9999999999999997780, 1.000000000000000222, 0.9999999999999994449, 1.000000000000000444, 0.9999999999999996669, 1.000000000000000000, 1.000000000000000222, 1.000000000000000000, 1.000000000000000000, 0.9999999999999997780, 1.000000000000000444, 0.9999999999999996669, 1.000000000000000000, 1.000000000000000222, 0.9999999999999997780, 1.000000000000000000, 0.9999999999999997780, 0.9999999999999997780, 1.000000000000000444, 0.9999999999999994449, 1.000000000000000444, 0.9999999999999997780, 0.9999999999999997780, 0.9999999999999996669, 1.000000000000000222, 1.000000000000000000, 0.9999999999999997780, 1.000000000000000222, 0.9999999999999997780, 1.000000000000000222, 1.000000000000000000, 1.000000000000000222, 1.000000000000000000, 1.000000000000000000, 1.000000000000000444, 0.9999999999999996669, 0.9999999999999997780, 1.000000000000000000, 0.9999999999999997780, 0.9999999999999997780, 1.000000000000000000, 1.000000000000000000, 0.9999999999999997780, 1.000000000000000444, 1.000000000000000000, 0.9999999999999997780, 1.000000000000000222, 0.9999999999999996669, 1.000000000000000222, 1.000000000000000000, 0.9999999999999997780, 1.000000000000000222, 0.9999999999999997780, 1.000000000000000000, 0.9999999999999997780, 1.000000000000000222, 0.9999999999999996669, 1.000000000000000000, 1.000000000000000222, 0.9999999999999997780, 1.000000000000000222, 0.9999999999999996669, 1.000000000000000444, 1.000000000000000000, 1.000000000000000000, 1.000000000000000222, 1.000000000000000222, 1.000000000000000000, 0.9999999999999997780, 1.000000000000000222, 0.9999999999999997780, 1.000000000000000000, 1.000000000000000000, 1.000000000000000000, 0.9999999999999997780, 1.000000000000000000, 0.9999999999999997780, 1.000000000000000222, 0.9999999999999997780, 1.000000000000000000, 1.000000000000000222, 0.9999999999999997780, 1.000000000000000000, 0.9999999999999996669, 1.000000000000000444, 0.9999999999999997780, 1.000000000000000000, 1.000000000000000000, 1.000000000000000000, 0.9999999999999997780, 0.9999999999999997780, 1.000000000000000222, 1.000000000000000222, 0.9999999999999997780, 1.000000000000000000, 1.000000000000000000, 1.000000000000000222, 1.000000000000000222, 1.000000000000000000, 0.9999999999999997780, 1.000000000000000222, 1.000000000000000000, 1.000000000000000000, 0.9999999999999997780, 0.9999999999999997780, 1.000000000000000222, 1.000000000000000000, 1.000000000000000000, 1.000000000000000000, 0.9999999999999997780, 1.000000000000000222, 1.000000000000000000, 1.000000000000000000, 1.000000000000000000, 1.000000000000000444, 0.9999999999999997780, 0.9999999999999997780, 1.000000000000000000, 1.000000000000000000, 0.9999999999999997780, 1.000000000000000222, 0.9999999999999997780, 1.000000000000000222, 1.000000000000000000, 1.000000000000000222, 1.000000000000000222, 1.000000000000000000, 1.000000000000000222, 1.000000000000000000, 0.9999999999999996669, 1.000000000000000222, 0.9999999999999997780, 1.000000000000000444, 0.9999999999999997780, 1.000000000000000000, 0.9999999999999997780, 1.000000000000000222, 1.000000000000000000, 0.9999999999999997780, 1.000000000000000222, 0.9999999999999994449, 1.000000000000000000, 1.000000000000000222, 1.000000000000000222, 0.9999999999999997780, 1.000000000000000444, 0.9999999999999997780, 1.000000000000000222, 0.9999999999999997780, 1.000000000000000222, 0.9999999999999997780, 1.000000000000000000, 1.000000000000000000, 1.000000000000000222, 0.9999999999999997780, 0.9999999999999996669, 1.000000000000000444, 0.9999999999999997780, 1.000000000000000222, 1.000000000000000000, 1.000000000000000222, 0.9999999999999994449, 1.000000000000000444, 0.9999999999999997780, 1.000000000000000000, 1.000000000000000222, 1.000000000000000000, 1.000000000000000000, 0.9999999999999997780, 1.000000000000000444, 0.9999999999999997780, 1.000000000000000444, 0.9999999999999997780, 1.000000000000000000, 1.000000000000000222, 0.9999999999999996669, 1.000000000000000222, 1.000000000000000000, 1.000000000000000000, 0.9999999999999996669, 1.000000000000000222, 1.000000000000000444, 0.9999999999999997780, 1.000000000000000222, 0.9999999999999996669, 1.000000000000000444, 0.9999999999999997780, 1.000000000000000444, 0.9999999999999996669, 0.9999999999999997780, 1.000000000000000000, 0.9999999999999997780, 1.000000000000000000, 1.000000000000000000, 1.000000000000000000, 1.000000000000000000, 0.9999999999999997780, 1.000000000000000000, 0.9999999999999997780, 1.000000000000000000, 1.000000000000000000, 1.000000000000000000, 1.000000000000000000, 0.9999999999999997780, 1.000000000000000222, 0.9999999999999997780, 1.000000000000000222, 0.9999999999999997780, 1.000000000000000222, 0.9999999999999994449, 1.000000000000000444, 1.000000000000000000, 1.000000000000000222, 0.9999999999999997780, 1.000000000000000000, 0.9999999999999997780, 1.000000000000000222, 1.000000000000000000, 1.000000000000000000, 1.000000000000000222, 1.000000000000000222, 0.9999999999999996669, 1.000000000000000444, 0.9999999999999996669, 1.000000000000000444, 0.9999999999999996669, 1.000000000000000000, 1.000000000000000000, 1.000000000000000000, 0.9999999999999997780, 1.000000000000000222, 0.9999999999999997780, 1.000000000000000222, 1.000000000000000000, 0.9999999999999997780, 1.000000000000000000, 1.000000000000000222, 1.000000000000000222, 1.000000000000000000, 1.000000000000000000, 1.000000000000000000, 1.000000000000000000, 0.9999999999999997780, 1.000000000000000444, 1.000000000000000000, 0.9999999999999997780, 1.000000000000000222, 0.9999999999999996669, 1.000000000000000444, 1.000000000000000000, 1.000000000000000222, 1.000000000000000222, 0.9999999999999997780, 1.000000000000000222, 0.9999999999999997780, 1.000000000000000000, 1.000000000000000000, 0.9999999999999997780, 1.000000000000000000, 1.000000000000000000, 0.9999999999999997780, 1.000000000000000222, 1.000000000000000000, 1.000000000000000000, 1.000000000000000222, 1.000000000000000000, 1.000000000000000000, 1.000000000000000000, 1.000000000000000222, 0.9999999999999997780, 1.000000000000000222, 1.000000000000000000, 0.9999999999999997780, 1.000000000000000222, 0.9999999999999997780, 1.000000000000000222, 1.000000000000000222, 1.000000000000000000, 0.9999999999999997780, 1.000000000000000000, 1.000000000000000222, 1.000000000000000000, 1.000000000000000000, 0.9999999999999996669, 1.000000000000000444, 0.9999999999999994449, 1.000000000000000444, 0.9999999999999997780, 1.000000000000000000, 1.000000000000000000, 0.9999999999999997780, 1.000000000000000222, 0.9999999999999997780, 1.000000000000000000, 1.000000000000000444, 0.9999999999999997780, 1.000000000000000000, 0.9999999999999997780, 1.000000000000000000, 1.000000000000000000, 0.9999999999999997780, 0.9999999999999997780, 1.000000000000000000, 1.000000000000000444, 1.000000000000000000, 1.000000000000000444, 1.000000000000000000, 1.000000000000000000, 1.000000000000000000, 0.9999999999999997780, 1.000000000000000000, 1.000000000000000000, 1.000000000000000000, 1.000000000000000000, 0.9999999999999997780, 1.000000000000000222, 1.000000000000000000, 0.9999999999999997780, 1.000000000000000444, 0.9999999999999997780, 1.000000000000000222, 0.9999999999999996669, 1.000000000000000444, 1.000000000000000000, 0.9999999999999997780, 1.000000000000000000, 1.000000000000000000, 1.000000000000000000, 0.9999999999999997780, 1.000000000000000000, 1.000000000000000000, 0.9999999999999997780, 1.000000000000000444, 0.9999999999999997780, 0.9999999999999997780, 1.000000000000000000, 1.000000000000000000, 1.000000000000000222, 1.000000000000000222, 0.9999999999999997780, 1.000000000000000000, 1.000000000000000222, 1.000000000000000000, 0.9999999999999997780, 1.000000000000000222, 1.000000000000000000, 1.000000000000000000, 1.000000000000000000, 0.9999999999999997780, 1.000000000000000000, 1.000000000000000000, 1.000000000000000000, 1.000000000000000000, 0.9999999999999997780, 1.000000000000000666, 0.9999999999999996669, 0.9999999999999996669, 1.000000000000000444, 0.9999999999999996669, 1.000000000000000222, 1.000000000000000000, 1.000000000000000000, 1.000000000000000000, 1.000000000000000000, 1.000000000000000000, 0.9999999999999997780, 1.000000000000000222, 1.000000000000000222, 0.9999999999999996669, 0.9999999999999997780, 1.000000000000000000, 1.000000000000000222, 1.000000000000000222) ) ) 
 REPRESENTATION_ITEM ( '' )  SURFACE ( )  );
#91563 = CARTESIAN_POINT ( 'NONE',  ( 1.955877382181537838, 1.966306777096353153, -0.1432868284926436253 ) ) ;
#91564 = STYLED_ITEM ( 'NONE', ( #60609 ), #86101 ) ;
#91566 = CARTESIAN_POINT ( 'NONE',  ( -4.828112100242291760, 6.726159765073026264, -1.443375672974066548 ) ) ;
#91565 = CARTESIAN_POINT ( 'NONE',  ( 5.871340715825057011, -1.643613990083541143, -0.9773822251149253404 ) ) ;
#91567 = CARTESIAN_POINT ( 'NONE',  ( -4.895902867866254837, 7.765618208269001066, 1.082531754730549967 ) ) ;
#91568 = CARTESIAN_POINT ( 'NONE',  ( 6.225128807330042591, 7.291680359087043151, -1.199719254218452047 ) ) ;
#91569 = CIRCLE ( 'NONE', #119276, 0.4000000000000001887 ) ;
#91570 = CARTESIAN_POINT ( 'NONE',  ( -6.642568916052639771, 6.714361588341672515, 0.000000000000000000 ) ) ;
#91571 = CARTESIAN_POINT ( 'NONE',  ( 1.963541569377712959, -1.623395098231813494, -1.201329681988633657 ) ) ;
#91572 = DIRECTION ( 'NONE',  ( 0.000000000000000000, 0.000000000000000000, 1.000000000000000000 ) ) ;
#91573 = CARTESIAN_POINT ( 'NONE',  ( 5.227664224568670193, -2.193190438267843323, 0.7177837189984050958 ) ) ;
#91574 = DIRECTION ( 'NONE',  ( 0.000000000000000000, 0.000000000000000000, -1.000000000000000000 ) ) ;
#91575 = CARTESIAN_POINT ( 'NONE',  ( 2.465611527742004760, -0.4346729355233553416, 1.912824223707191296 ) ) ;
#91576 = CARTESIAN_POINT ( 'NONE',  ( 7.747594715205354809, 11.12627870345989756, -1.199719254218446718 ) ) ;
#91577 = CARTESIAN_POINT ( 'NONE',  ( 0.9850002542920628379, -2.016597020373378513, 0.002813405579435435122 ) ) ;
#91578 = ORIENTED_EDGE ( 'NONE', *, *, #195389, .T. ) ;
#91579 = CARTESIAN_POINT ( 'NONE',  ( 2.817688460867060485, -1.425471633543059724, -1.565750481055405263 ) ) ;
#91581 = CARTESIAN_POINT ( 'NONE',  ( -6.856673000209188906, 9.022537805042615489, 1.599625672291283607 ) ) ;
#91580 = CARTESIAN_POINT ( 'NONE',  ( -4.810445574750349174, 4.506608013497163334, 0.7998128361456341429 ) ) ;
#91582 = CARTESIAN_POINT ( 'NONE',  ( 2.343484645521694887, 1.840739972059933560, 0.04548452486473342216 ) ) ;
#91583 = ORIENTED_EDGE ( 'NONE', *, *, #26877, .F. ) ;
#91584 = CARTESIAN_POINT ( 'NONE',  ( -9.110189153378817295, 12.71597221466224603, 1.199719254218462483 ) ) ;
#91585 = CARTESIAN_POINT ( 'NONE',  ( 10.40106502431298452, 10.48805886172130997, 5.993424745873436876 ) ) ;
#91586 = CARTESIAN_POINT ( 'NONE',  ( 2.848016566918720294, -1.427295477286108394, -1.568503593382633454 ) ) ;
#91587 = CARTESIAN_POINT ( 'NONE',  ( 6.720655732516681802, 0.002698097948229584257, 1.926293798961112858 ) ) ;
#91588 = CARTESIAN_POINT ( 'NONE',  ( -0.7499999999999972244, 4.139583334016149863, -1.299038105676652899 ) ) ;
#91589 = CARTESIAN_POINT ( 'NONE',  ( 8.599949509769960088, 8.927695937686774386, 1.040834085586084257E-14 ) ) ;
#91590 = CARTESIAN_POINT ( 'NONE',  ( 8.011942431032855083, 8.311964022485323511, 0.7998128361456291469 ) ) ;
#91591 = CARTESIAN_POINT ( 'NONE',  ( 4.499328421682089463, 1.652694973434418291, 1.230784805264173221 ) ) ;
#91593 = CARTESIAN_POINT ( 'NONE',  ( 1.839159199666509981, 0.7036077657225293658, -1.701706503975081830 ) ) ;
#91592 = CARTESIAN_POINT ( 'NONE',  ( -7.015454420067433361, 10.27211502579893754, 1.199719254218453823 ) ) ;
#91594 = CARTESIAN_POINT ( 'NONE',  ( -0.6823417656250212460, 5.051041667008086655, 1.181850606188767472 ) ) ;
#91595 = CARTESIAN_POINT ( 'NONE',  ( -0.02224634325196597762, 0.2233488839939681836, -2.322587069611138144 ) ) ;
#91596 = CARTESIAN_POINT ( 'NONE',  ( -1.534012367094089946, 8.737164261768347373, 2.508166476568440828 ) ) ;
#91597 = CARTESIAN_POINT ( 'NONE',  ( 11.07131503167114772, 13.79999999999999716, 0.8043049353970801452 ) ) ;
#91598 = EDGE_CURVE ( 'NONE', #116549, #188383, #50235, .T. ) ;
#91599 = CARTESIAN_POINT ( 'NONE',  ( 1.401302286655212948, 1.802556353783949517, -1.272968949304439379 ) ) ;
#91600 = CARTESIAN_POINT ( 'NONE',  ( 2.794484930487377561, -2.256151742081555334, -0.1692699688307132133 ) ) ;
#91601 = CARTESIAN_POINT ( 'NONE',  ( -7.348156068926747331, 11.51667314714914347, 0.7216878364870458196 ) ) ;
#91602 = CARTESIAN_POINT ( 'NONE',  ( 4.095841850722721667, 1.188128187434208893, 1.367607970084052660 ) ) ;
#91603 = B_SPLINE_CURVE_WITH_KNOTS ( 'NONE', 3,
 ( #200069, #21308, #153480, #136170, #185957, #134061 ),
 .UNSPECIFIED., .F., .F.,
 ( 4, 2, 4 ),
 ( 0.001279092382393099943, 0.001599469101539996744, 0.001919845820686893545 ),
 .UNSPECIFIED. ) ;
#91604 = CARTESIAN_POINT ( 'NONE',  ( 3.133901338358492161, 1.915903397621956383, -0.005105665024216290114 ) ) ;
#91605 = CARTESIAN_POINT ( 'NONE',  ( 4.246580143467587831, -2.047389768388275577, -0.3068500204662719666 ) ) ;
#91606 = CARTESIAN_POINT ( 'NONE',  ( 0.6823417656249899377, 3.155208333674754062, 1.181850606188765695 ) ) ;
#91607 = CARTESIAN_POINT ( 'NONE',  ( 2.342595614570395668, 0.4301288016448929774, 1.923825502367804141 ) ) ;
#91608 = CARTESIAN_POINT ( 'NONE',  ( 0.6922523098862876090, -1.911435030786556855, -0.2391616053641909545 ) ) ;
#91609 = CARTESIAN_POINT ( 'NONE',  ( 3.994877460428855276, 1.580554378303768992, -1.000287695324620252 ) ) ;
#91610 = CARTESIAN_POINT ( 'NONE',  ( 1.840857126529979126, 2.283052885565831858, 0.3356036407394235033 ) ) ;
#91611 = CARTESIAN_POINT ( 'NONE',  ( 3.930005801358939621, 1.032382326871328804, 1.548228005463901491 ) ) ;
#91612 = CARTESIAN_POINT ( 'NONE',  ( -0.6823417656249969321, 4.717708333674755394, -1.181850606188749264 ) ) ;
#91613 = AXIS2_PLACEMENT_3D ( 'NONE', #83139, #178532, #79947 ) ;
#91614 = CARTESIAN_POINT ( 'NONE',  ( -4.786191920824102830, 5.542644314838231168, 1.199719254218462483 ) ) ;
#91615 = CARTESIAN_POINT ( 'NONE',  ( 4.964256800898067645, 8.943383367689749619, 0.7998128361456462443 ) ) ;
#91616 = CARTESIAN_POINT ( 'NONE',  ( 0.7500000000000006661, 8.947916667349467446, -1.299038105676657340 ) ) ;
#91617 = CARTESIAN_POINT ( 'NONE',  ( 1.137491875146545039, -1.903277616399126293, 0.9019996372539202945 ) ) ;
#91619 = CARTESIAN_POINT ( 'NONE',  ( 5.055755612212820438, 4.906101081808937892, 0.2771076874560872705 ) ) ;
#91618 = CARTESIAN_POINT ( 'NONE',  ( -1.201851678989727383E-14, 4.134375000341417028, 1.575800808251672791 ) ) ;
#91620 = CARTESIAN_POINT ( 'NONE',  ( -1.843739406749240750, 8.920000000000001705, -0.7749999999999996891 ) ) ;
#91621 = CARTESIAN_POINT ( 'NONE',  ( 2.584367824843319283, 1.138156186954141003, 1.789115803205274080 ) ) ;
#91622 = CARTESIAN_POINT ( 'NONE',  ( -0.1579319072057436268, -1.246015270063109748, -1.590120154594099278 ) ) ;
#91623 = CARTESIAN_POINT ( 'NONE',  ( -1.364683531250014514, 0.2802083336747505649, 0.7879004041258379498 ) ) ;
#91624 = CARTESIAN_POINT ( 'NONE',  ( -5.450014563013544588, 5.460697866378308341, 0.7216878364870317197 ) ) ;
#91625 = CARTESIAN_POINT ( 'NONE',  ( 5.497994985541524215, 6.373081223675282736, -1.199719254218445830 ) ) ;
#91626 = CARTESIAN_POINT ( 'NONE',  ( 1.054251131370760319, 2.159144779032458050, -0.1049546803274861440 ) ) ;
#91629 = CARTESIAN_POINT ( 'NONE',  ( 5.192409644353875642, 5.160158794608717514, 1.040834085586084257E-14 ) ) ;
#91628 = CARTESIAN_POINT ( 'NONE',  ( 6.925078400183577010, 7.053014648177382995, 2.453806744102948745 ) ) ;
#91627 = CARTESIAN_POINT ( 'NONE',  ( 5.143339171537801846, 7.093924681584509173, 1.599625672291269396 ) ) ;
#91630 = CARTESIAN_POINT ( 'NONE',  ( -0.2104748580754409459, 6.947232144882289795, -2.698723162346649662 ) ) ;
#91631 = CARTESIAN_POINT ( 'NONE',  ( 6.104703911763087909, 1.883310800321544409, 0.7212973825745233603 ) ) ;
#91633 = CARTESIAN_POINT ( 'NONE',  ( -6.170369307550858551, 8.292126506933035657, 1.443375672974058777 ) ) ;
#91632 = CARTESIAN_POINT ( 'NONE',  ( -8.188761592974040937, 11.53701037756964887, -1.082531754730543971 ) ) ;
#91634 = FACE_BOUND ( 'NONE', #192858, .T. ) ;
#91636 = CARTESIAN_POINT ( 'NONE',  ( 0.6823417656249969321, 10.27604166700806587, -1.181850606188757036 ) ) ;
#91635 = CARTESIAN_POINT ( 'NONE',  ( 0.8665589547518313118, 1.117614298721156585, 1.967126077831014896 ) ) ;
#91637 = CARTESIAN_POINT ( 'NONE',  ( -10.48453286206953727, 11.12637651536962125, 0.7998128361456462443 ) ) ;
#91639 = CARTESIAN_POINT ( 'NONE',  ( 6.292592244351721043, 1.492246071875057423, -1.356311808412967723 ) ) ;
#91638 = CARTESIAN_POINT ( 'NONE',  ( -5.761852095683518193, 6.784877535461274256, 1.082531754730546636 ) ) ;
#91640 = CARTESIAN_POINT ( 'NONE',  ( 1.364683531249988757, 0.4468750003414206917, 0.000000000000000000 ) ) ;
#91641 = CARTESIAN_POINT ( 'NONE',  ( 0.1178541238725807350, -5.389012432655391649, 10.99948089704805199 ) ) ;
#91642 = DIRECTION ( 'NONE',  ( -5.551115123125765446E-17, 0.000000000000000000, 1.000000000000000000 ) ) ;
#91643 = CARTESIAN_POINT ( 'NONE',  ( 3.334305206967770552, 1.683047542859770429, 0.3767605245002195180 ) ) ;
#91644 = CARTESIAN_POINT ( 'NONE',  ( 3.410758162289653672, 6.136912401716668519, -1.199719254218453823 ) ) ;
#91645 = CARTESIAN_POINT ( 'NONE',  ( 7.015418140428412386, 7.149352350113456822, 0.7998128361456331437 ) ) ;
#91646 = CARTESIAN_POINT ( 'NONE',  ( 0.7547153349467434769, -1.490676808382383145, -0.9535711479493594878 ) ) ;
#91647 =( BOUNDED_CURVE ( )  B_SPLINE_CURVE ( 2, ( #97989, #198635, #164048, #50283, #182390, #133700, #34020, #106546, #201827 ),
 .UNSPECIFIED., .F., .T. ) 
 B_SPLINE_CURVE_WITH_KNOTS ( ( 3, 2, 2, 2, 3 ),
 ( 0.8839285714285713969, 0.8869047619047618625, 0.8928571428571429047, 0.8988095238095238360, 0.9017857142857143016 ),
 .UNSPECIFIED. ) 
 CURVE ( )  GEOMETRIC_REPRESENTATION_ITEM ( )  RATIONAL_B_SPLINE_CURVE ( ( 0.9330127018922194093, 0.9330127018922194093, 1.000000000000000000, 0.8660254037844387076, 1.000000000000000000, 0.8660254037844387076, 1.000000000000000000, 0.9330127018922194093, 0.9330127018922194093 ) ) 
 REPRESENTATION_ITEM ( '' )  );
#91648 = CARTESIAN_POINT ( 'NONE',  ( 1.418609115998151982, -0.7265329536030593616, -1.877579518606347531 ) ) ;
#91649 = SURFACE_STYLE_USAGE ( .BOTH. , #8224 ) ;
#91650 = CARTESIAN_POINT ( 'NONE',  ( 4.366400497975233996, 1.037236317483503312, 1.947806255051434121 ) ) ;
#91651 = ORIENTED_EDGE ( 'NONE', *, *, #29662, .F. ) ;
#91652 = CARTESIAN_POINT ( 'NONE',  ( 6.914295152845067349, 11.01050207838719075, 1.040834085586084257E-14 ) ) ;
#91654 = CARTESIAN_POINT ( 'NONE',  ( 2.917592388753763366, -1.356314522985989424, -1.492243612603139757 ) ) ;
#91653 = CARTESIAN_POINT ( 'NONE',  ( 4.635462950926918957, -0.1032030737609032217, 2.118083805499561656 ) ) ;
#91656 = ORIENTED_EDGE ( 'NONE', *, *, #163618, .T. ) ;
#91655 = CARTESIAN_POINT ( 'NONE',  ( 3.568453337068989928, 0.6571482028082703541, 1.688366419454911727 ) ) ;
#91657 = CARTESIAN_POINT ( 'NONE',  ( 3.725458348705031231, 7.568394850123006279, -1.734723475976807094E-15 ) ) ;
#91658 = ORIENTED_EDGE ( 'NONE', *, *, #115804, .F. ) ;
#91659 = EDGE_CURVE ( 'NONE', #144349, #72818, #990, .T. ) ;
#91660 = CARTESIAN_POINT ( 'NONE',  ( 0.6373110600932235803, -1.319858442276698129, -1.325903642019378381 ) ) ;
#91661 = CARTESIAN_POINT ( 'NONE',  ( 2.842405760359353106, 6.467890487061221272, -0.7998128361456291469 ) ) ;
#91662 = CIRCLE ( 'NONE', #195380, 0.09999999999999982514 ) ;
#91663 = CARTESIAN_POINT ( 'NONE',  ( 6.533835636172961259, -1.196796279342365210, -1.378804128639096849 ) ) ;
#91665 = CARTESIAN_POINT ( 'NONE',  ( 2.922943415214097396, -1.687269874283424453, 0.9073053738915691779 ) ) ;
#91664 = CARTESIAN_POINT ( 'NONE',  ( 0.000000000000000000, -6.532648833121171172, 0.000000000000000000 ) ) ;
#91666 = CARTESIAN_POINT ( 'NONE',  ( 1.177073619093309986, 3.199321498342246883, 0.7750000000000135669 ) ) ;
#91667 = CIRCLE ( 'NONE', #36256, 0.08000000000000020983 ) ;
#91668 = CARTESIAN_POINT ( 'NONE',  ( 0.6823417656249882723, 1.988541667008083991, -1.181850606188749264 ) ) ;
#91669 = CARTESIAN_POINT ( 'NONE',  ( 6.471393748265543699, 5.229711127717882491, 2.420000000000010587 ) ) ;
#91670 = ORIENTED_EDGE ( 'NONE', *, *, #136398, .T. ) ;
#91671 = CARTESIAN_POINT ( 'NONE',  ( 6.916067756746836714, 8.201738816693689316, -1.082531754730548412 ) ) ;
#91672 = CARTESIAN_POINT ( 'NONE',  ( -4.882344714696960075, 5.829061934302122161, 1.082531754730549078 ) ) ;
#91673 = CARTESIAN_POINT ( 'NONE',  ( -5.237192476628793614, 9.332084666034067055, 0.7998128361456291469 ) ) ;
#91674 = CARTESIAN_POINT ( 'NONE',  ( 3.006218798242997980, -0.8556837461295876412, 1.940463308995137526 ) ) ;
#91676 = CARTESIAN_POINT ( 'NONE',  ( -11.68462027884434917, 8.171766027648200037, -4.455682980299036089 ) ) ;
#91675 = FACE_OUTER_BOUND ( 'NONE', #132441, .T. ) ;
#91677 = CARTESIAN_POINT ( 'NONE',  ( 4.798096821016461178, -1.970857504970180862, -0.05141287852120436652 ) ) ;
#91679 = CARTESIAN_POINT ( 'NONE',  ( 0.1232915322694717181, 1.753566389086946398, 0.9887636377800024245 ) ) ;
#91678 = VECTOR ( 'NONE', #94276, 1000.000000000000000 ) ;
#91680 = VERTEX_POINT ( 'NONE', #98286 ) ;
#91681 = CARTESIAN_POINT ( 'NONE',  ( 0.3689691111537584112, -0.2640367098126532031, -2.100658933187772526 ) ) ;
#91682 = CARTESIAN_POINT ( 'NONE',  ( 1.627480586986803868, 0.1543294891723171747, -2.064685722993148342 ) ) ;
#91683 = CARTESIAN_POINT ( 'NONE',  ( 2.308448745193259821, 1.734665721750632938, 0.8731161087585439518 ) ) ;
#91684 = CARTESIAN_POINT ( 'NONE',  ( 6.703580607314123085, 6.785541894813420072, 0.000000000000000000 ) ) ;
#91685 = CARTESIAN_POINT ( 'NONE',  ( 5.027041095616958444, 9.086908054853605421, 0.000000000000000000 ) ) ;
#91687 = CARTESIAN_POINT ( 'NONE',  ( 5.900823170445728572, 7.907379670318584353, 1.599625672291267398 ) ) ;
#91686 = CARTESIAN_POINT ( 'NONE',  ( 3.626972257435066460, -1.931581639804475614, 0.8003350836045771688 ) ) ;
#91688 = CARTESIAN_POINT ( 'NONE',  ( 3.390947816749319443, 6.970206529600588397, -1.734723475976807094E-15 ) ) ;
#91690 = EDGE_LOOP ( 'NONE', ( #29574, #165754, #72708 ) ) ;
#91689 = CARTESIAN_POINT ( 'NONE',  ( 0.9612203838427415548, -1.427409828940959136, -1.115214234437786223 ) ) ;
#91691 = CARTESIAN_POINT ( 'NONE',  ( 5.918643953348324160, 1.484978324971843566, -1.632713241052483832 ) ) ;
#91692 = CARTESIAN_POINT ( 'NONE',  ( 0.003376046620571365731, -7.161464053357560644, 9.586610838029431036 ) ) ;
#91693 = CARTESIAN_POINT ( 'NONE',  ( 3.891806949550260519, 1.596497936513015192, 1.523729906679156754 ) ) ;
#91694 = CARTESIAN_POINT ( 'NONE',  ( 7.446452682403650769, 9.710614100936176385, -1.599625672291262513 ) ) ;
#91695 = CARTESIAN_POINT ( 'NONE',  ( -5.956409969451652131, 6.075908546082715134, -0.6293437877468227581 ) ) ;
#91696 = CARTESIAN_POINT ( 'NONE',  ( 2.613799471529183460, -0.5979904443059110841, 1.816458080996792068 ) ) ;
#91697 = CARTESIAN_POINT ( 'NONE',  ( 8.748035429315576650, 11.22912730566677553, -1.599625672291255185 ) ) ;
#91698 = CARTESIAN_POINT ( 'NONE',  ( 5.600075274486990828, 0.8424382930321882013, -1.891409743246947217 ) ) ;
#91699 = AXIS2_PLACEMENT_3D ( 'NONE', #143067, #28207, #130055 ) ;
#91701 = CARTESIAN_POINT ( 'NONE',  ( 2.536181837661064087, 1.019768383293401248, -1.906060392209196763 ) ) ;
#91700 = CARTESIAN_POINT ( 'NONE',  ( 1.503277409322719471, 8.660639097433820766, -2.556074651073448667 ) ) ;
#91702 = CARTESIAN_POINT ( 'NONE',  ( 5.196902890030515643, 1.791362914573800369, 1.262263373074036688 ) ) ;
#91703 = ORIENTED_EDGE ( 'NONE', *, *, #189585, .F. ) ;
#91704 = ORIENTED_EDGE ( 'NONE', *, *, #56238, .F. ) ;
#91705 = CARTESIAN_POINT ( 'NONE',  ( -9.579665964948882007, -7.473374494045003757, 5.204170427930421283E-15 ) ) ;
#91706 = CARTESIAN_POINT ( 'NONE',  ( 9.499766273075879397, -9.919999999999998153, -0.06663900456894614188 ) ) ;
#91707 = CARTESIAN_POINT ( 'NONE',  ( 4.278479993564246797, 7.149254538203735798, 1.199719254218452047 ) ) ;
#91708 = CARTESIAN_POINT ( 'NONE',  ( -8.012344526598182026E-15, 15.35937500034140513, -1.575800808251669460 ) ) ;
#91709 = CARTESIAN_POINT ( 'NONE',  ( -5.015590482412729756, 4.816220082428420923, 0.000000000000000000 ) ) ;
#91711 = CARTESIAN_POINT ( 'NONE',  ( -8.676855123066022912, 10.18571440074093282, -1.082531754730543971 ) ) ;
#91710 = VECTOR ( 'NONE', #54580, 1000.000000000000000 ) ;
#91712 = CARTESIAN_POINT ( 'NONE',  ( 5.061990249855835344, 6.999017606288844284, -1.599625672291273171 ) ) ;
#91713 = CARTESIAN_POINT ( 'NONE',  ( 5.471561611210747245, -0.3092806512635417060, 2.046926588373791933 ) ) ;
#91714 = CARTESIAN_POINT ( 'NONE',  ( 4.705647360784301014, -0.5120751438620478879, 1.857136557572524715 ) ) ;
#91715 = CARTESIAN_POINT ( 'NONE',  ( -0.05311194370935175268, -1.802413661875476913, -0.9041393574176490588 ) ) ;
#91716 = CARTESIAN_POINT ( 'NONE',  ( -10.62011439820619429, 11.28455497419572318, -0.7998128361456221525 ) ) ;
#91717 = CARTESIAN_POINT ( 'NONE',  ( 7.126746022638799971, 8.343567110280638133, 1.199719254218452047 ) ) ;
#91718 = CARTESIAN_POINT ( 'NONE',  ( 5.242998352400915607, -0.2370019515391492138, -1.955029394545240162 ) ) ;
#91719 = CARTESIAN_POINT ( 'NONE',  ( 0.1292129718690297469, -2.001788180159810970, 0.8922102942980969509 ) ) ;
#91720 = CARTESIAN_POINT ( 'NONE',  ( 5.531824841778981927, -1.161409778037244100, -1.408645805323349487 ) ) ;
#91721 = AXIS2_PLACEMENT_3D ( 'NONE', #106126, #125606, #139667 ) ;
#91722 = CARTESIAN_POINT ( 'NONE',  ( 6.888951449519509218, 7.209733910627123876, -0.7216878364870317197 ) ) ;
#91723 = CARTESIAN_POINT ( 'NONE',  ( 3.294268137996273715, 5.826768013428865522, -1.082531754730543971 ) ) ;
#91724 = CARTESIAN_POINT ( 'NONE',  ( -5.010620288702242853, 8.003418215864698482, -1.199719254218453823 ) ) ;
#91725 = CARTESIAN_POINT ( 'NONE',  ( 5.065906673361608270, 5.939254536123854677, -1.199719254218450271 ) ) ;
#91726 = EDGE_LOOP ( 'NONE', ( #169700, #6110, #208651, #94626 ) ) ;
#91728 = CARTESIAN_POINT ( 'NONE',  ( 6.416276891523604142, -2.012660772237227391, 0.05378525197091872656 ) ) ;
#91727 = CARTESIAN_POINT ( 'NONE',  ( 3.104851637799400876, -0.3563606998662186554, 1.806257425991746546 ) ) ;
#91729 = CARTESIAN_POINT ( 'NONE',  ( 0.6151802255017734256, 0.7180209600621060284, -2.183386540618210692 ) ) ;
#91730 = CARTESIAN_POINT ( 'NONE',  ( 6.280128941539553367, -1.086961472313338284, -1.632890767417946032 ) ) ;
#91731 = CARTESIAN_POINT ( 'NONE',  ( -4.869349725602420520, 8.832658446511480577, 1.040834085586084257E-14 ) ) ;
#91732 = CARTESIAN_POINT ( 'NONE',  ( -3.954497087797542942, 7.557404335831681585, -0.5023533386407119661 ) ) ;
#91733 = CARTESIAN_POINT ( 'NONE',  ( -2.123823618835070537, 5.629544655282869847, 1.040834085586084257E-14 ) ) ;
#91734 = CARTESIAN_POINT ( 'NONE',  ( 0.1861046438572169504, -1.272802160389638892, -1.633586439835111648 ) ) ;
#91735 = CARTESIAN_POINT ( 'NONE',  ( -4.472210567661380587, 6.310941310395290493, 1.599625672291270506 ) ) ;
#91737 = CARTESIAN_POINT ( 'NONE',  ( 0.7603692911175019553, -1.357789551990191246, 1.287012767582619510 ) ) ;
#91736 = CARTESIAN_POINT ( 'NONE',  ( 2.929326106026585830, -1.406127681732218360, -1.547418247020322601 ) ) ;
#91738 = CARTESIAN_POINT ( 'NONE',  ( 2.143907462275076892, -0.09611812122205246056, -2.013924455302518624 ) ) ;
#91739 = ORIENTED_EDGE ( 'NONE', *, *, #41655, .F. ) ;
#91740 = CARTESIAN_POINT ( 'NONE',  ( 1.364683531249990311, 4.696875000341417916, 1.214306433183764966E-14 ) ) ;
#91741 = CARTESIAN_POINT ( 'NONE',  ( 2.366429680491717313, 0.08383053003592833008, -1.738530308508005273 ) ) ;
#91742 = CARTESIAN_POINT ( 'NONE',  ( 5.769158057814842699, 6.689438141327490150, 1.199719254218462483 ) ) ;
#91744 = CARTESIAN_POINT ( 'NONE',  ( 1.525860493984659172, 8.693043820721578996, 2.521102513734321260 ) ) ;
#91743 = DIRECTION ( 'NONE',  ( -1.000000000000000000, 7.771561172376097755E-16, 4.440892098500627148E-16 ) ) ;
#91745 = CARTESIAN_POINT ( 'NONE',  ( 2.631144668424452604, -1.609571295485120457, 0.6205441041484575093 ) ) ;
#91746 = CARTESIAN_POINT ( 'NONE',  ( 3.017305944477025825, -2.111434807548946857, 0.5868732223921411251 ) ) ;
#91747 = CARTESIAN_POINT ( 'NONE',  ( 5.707716145626243964, -0.5396369327701348029, 2.139774205771049154 ) ) ;
#91748 = CARTESIAN_POINT ( 'NONE',  ( -10.71748749772954135, 5.309591131546671505, -6.727448623506740333 ) ) ;
#91749 = CARTESIAN_POINT ( 'NONE',  ( 2.993230899678362089, 0.2615320595270088644, 2.155169926569647565 ) ) ;
#91750 = CARTESIAN_POINT ( 'NONE',  ( 1.013953575274041619, -0.8186894766500467657, -1.631917417583013341 ) ) ;
#91751 = CARTESIAN_POINT ( 'NONE',  ( 3.679011075472499392, 1.786488794941149871, -1.136238802782759238 ) ) ;
#91752 = LINE ( 'NONE', #188146, #201722 ) ;
#91753 = VERTEX_POINT ( 'NONE', #29021 ) ;
#91755 = CARTESIAN_POINT ( 'NONE',  ( 0.6823417656249882723, 0.7385416670080829915, -1.181850606188749264 ) ) ;
#91754 = CARTESIAN_POINT ( 'NONE',  ( 3.579850016053500728, -1.128938594042153021, 1.995021623459404703 ) ) ;
#91756 = CARTESIAN_POINT ( 'NONE',  ( 0.3282377607281200538, 0.1763354503153972130, -1.225000000000030953 ) ) ;
#91757 = CARTESIAN_POINT ( 'NONE',  ( 4.054051625686104998, 4.688480637177271149, -1.199719254218446718 ) ) ;
#91758 = CARTESIAN_POINT ( 'NONE',  ( 5.531947820799793192, -2.167606221786242848, 0.4847573843902542312 ) ) ;
#91759 = CARTESIAN_POINT ( 'NONE',  ( -5.070386261830872598, 8.859275038870594088, 0.7216878364870458196 ) ) ;
#91760 = CARTESIAN_POINT ( 'NONE',  ( 2.575685996916329046, 5.948791396470269888, 0.7216878364870438212 ) ) ;
#91761 = CARTESIAN_POINT ( 'NONE',  ( -6.873620692004104527, 7.121571683533994168, 0.7216878364870317197 ) ) ;
#91762 = CARTESIAN_POINT ( 'NONE',  ( 3.268924434670684498, 6.827845917175511481, -1.734723475976807094E-15 ) ) ;
#91763 = ORIENTED_EDGE ( 'NONE', *, *, #57540, .T. ) ;
#91764 = CARTESIAN_POINT ( 'NONE',  ( 4.043592392309851569, -1.492256208629010761, 1.356298961253152413 ) ) ;
#91766 = CARTESIAN_POINT ( 'NONE',  ( 3.696185820831139779, 0.9318344738791024540, -1.840181792940546179 ) ) ;
#91765 = CARTESIAN_POINT ( 'NONE',  ( 5.666418135507635512, 8.698239360479199433, 1.199719254218462483 ) ) ;
#91767 = CARTESIAN_POINT ( 'NONE',  ( 5.969332771766739931, 10.18624834369502885, -0.7998128361456481317 ) ) ;
#91768 = CARTESIAN_POINT ( 'NONE',  ( 3.512971199272317602, 6.152197928242737923, -1.082531754730549967 ) ) ;
#91769 = CARTESIAN_POINT ( 'NONE',  ( 1.001543065824772753E-15, -2.821874999522044458, 3.793834371823811669 ) ) ;
#91770 = CARTESIAN_POINT ( 'NONE',  ( 5.964808794498537736, 0.1646014364122504459, -2.185315939793014639 ) ) ;
#91771 = CARTESIAN_POINT ( 'NONE',  ( 3.779922787921150995, 1.701948043757589124, -1.081065327119046016 ) ) ;
#91772 = CARTESIAN_POINT ( 'NONE',  ( 3.034521004542716227, -1.622529355458858236, 0.8704296449140033198 ) ) ;
#91773 = CARTESIAN_POINT ( 'NONE',  ( 5.309989718046547402, 9.346738437696316737, 0.7998128361456462443 ) ) ;
#91774 = CARTESIAN_POINT ( 'NONE',  ( 6.194357462883206544, -1.817092693925310032, -0.1759843941628037589 ) ) ;
#91775 = CARTESIAN_POINT ( 'NONE',  ( 0.08910568399025410591, -0.6041685166103001325, 2.217849651370594088 ) ) ;
#91776 = CARTESIAN_POINT ( 'NONE',  ( -6.901263884555985051, 8.010228272525461435, 1.199719254218450271 ) ) ;
#91777 = CARTESIAN_POINT ( 'NONE',  ( 0.3161853103110903729, -2.218393710063219615, 0.4432750438988151687 ) ) ;
#91778 = CARTESIAN_POINT ( 'NONE',  ( 1.928482936185798247, 1.211665229685221057, -1.722411974427066506 ) ) ;
#91779 = CARTESIAN_POINT ( 'NONE',  ( -6.394605727500880299, 7.489403432619674561, -1.199719254218452047 ) ) ;
#91780 = CARTESIAN_POINT ( 'NONE',  ( 7.727257484784855635, 11.10255193463598111, -1.199719254218446718 ) ) ;
#91781 = CARTESIAN_POINT ( 'NONE',  ( 6.495764994278797388, 8.671754808115688107, 1.443375672974063439 ) ) ;
#91782 = B_SPLINE_CURVE_WITH_KNOTS ( 'NONE', 3,
 ( #39840, #18223, #19295, #86448, #55020, #168760, #20363, #138413, #105947, #120089 ),
 .UNSPECIFIED., .F., .F.,
 ( 4, 2, 2, 2, 4 ),
 ( 0.0001032556302127828247, 0.0003933207648079593225, 0.0006833858994031357390, 0.0009734510339983121555, 0.001263516168593488680 ),
 .UNSPECIFIED. ) ;
#91785 = EDGE_CURVE ( 'NONE', #130487, #115079, #5203, .T. ) ;
#91784 = AXIS2_PLACEMENT_3D ( 'NONE', #144130, #174471, #61764 ) ;
#91783 = CARTESIAN_POINT ( 'NONE',  ( -7.660520486921249983, 8.896027641951645748, -1.199719254218446718 ) ) ;
#91786 = CARTESIAN_POINT ( 'NONE',  ( 6.100805936025112786, 10.06143132543056673, 1.040834085586084257E-14 ) ) ;
#91787 = CARTESIAN_POINT ( 'NONE',  ( 4.019508774049570299, 7.801013956325979493, 0.3192432753683968061 ) ) ;
#91788 = CARTESIAN_POINT ( 'NONE',  ( -5.786632634934295361, 5.645492917045106473, 0.7998128361456341429 ) ) ;
#91790 = CARTESIAN_POINT ( 'NONE',  ( 4.447658085050952614, -2.030299463072975819, 0.9018405843745944672 ) ) ;
#91789 = CARTESIAN_POINT ( 'NONE',  ( 2.092179824929023102, 1.308410154019133076, 1.668721082780571408 ) ) ;
#91791 = CARTESIAN_POINT ( 'NONE',  ( 0.7971425760184660536, 1.793611693402120455, 1.258865353619270433 ) ) ;
#91792 = CARTESIAN_POINT ( 'NONE',  ( 0.2060869173217265982, -0.5842117877600698783, 2.128085570573131413 ) ) ;
#91793 = CARTESIAN_POINT ( 'NONE',  ( -6.296835998904160014, 6.311006518335105397, 0.000000000000000000 ) ) ;
#91794 = CARTESIAN_POINT ( 'NONE',  ( 4.422284181769401634, 0.9229163912191931107, 1.731201473044993167 ) ) ;
#91795 = CARTESIAN_POINT ( 'NONE',  ( 8.809047120577066181, 11.30030761213851953, 1.599625672291281386 ) ) ;
#91796 = CARTESIAN_POINT ( 'NONE',  ( -5.227141986104622440, 6.445127484965264664, 1.169998774669118946 ) ) ;
#91797 = CARTESIAN_POINT ( 'NONE',  ( -3.939296163840085629, 2.811845806437647699, -0.7749999999960115460 ) ) ;
#91798 = CARTESIAN_POINT ( 'NONE',  ( 1.364683531249986537, 0.6552083336747522857, -0.7879004041258239610 ) ) ;
#91799 = CARTESIAN_POINT ( 'NONE',  ( 6.610000000000010090, 0.5825982378308904863, 2.053072689460200273 ) ) ;
#91801 = ORIENTED_EDGE ( 'NONE', *, *, #202366, .F. ) ;
#91800 = CARTESIAN_POINT ( 'NONE',  ( -4.609409038966229666, 8.321468278861834378, -0.7216878364870267237 ) ) ;
#91802 = CARTESIAN_POINT ( 'NONE',  ( 3.744478000529617656, 1.131475959888720295, -1.793321066073015224 ) ) ;
#91803 = CARTESIAN_POINT ( 'NONE',  ( -4.984557751679625781, 5.844347460828191565, 1.199719254218452935 ) ) ;
#91804 = CARTESIAN_POINT ( 'NONE',  ( 5.295850518597075229, -0.7817450549502875656, 2.015575934489414411 ) ) ;
#91805 = CARTESIAN_POINT ( 'NONE',  ( 4.388128076750056117, -0.4078595375654435751, -1.795341762384855544 ) ) ;
#91806 = CARTESIAN_POINT ( 'NONE',  ( 5.384000029850495750, -2.016708404008683786, 0.004832792792668073358 ) ) ;
#91807 = CARTESIAN_POINT ( 'NONE',  ( -5.826669560333386677, 6.051347404617407832, -0.4878656478981869826 ) ) ;
#91808 = CARTESIAN_POINT ( 'NONE',  ( -0.6823417656250003738, 1.530208333674752730, -1.181850606188749264 ) ) ;
#91809 = CARTESIAN_POINT ( 'NONE',  ( -0.09478571475088257148, -0.7418789811804274992, -1.573373712294885207 ) ) ;
#91810 = CARTESIAN_POINT ( 'NONE',  ( 6.727182134110203826, 2.985950691969770254, 2.264927069331075238 ) ) ;
#91811 = CARTESIAN_POINT ( 'NONE',  ( 4.541618270897912701, 4.400902192243413502, 1.214306433183764966E-14 ) ) ;
#91812 = CARTESIAN_POINT ( 'NONE',  ( 7.592810154713589835E-16, -4.000000000000003553, -6.200000000000000178 ) ) ;
#91813 = CARTESIAN_POINT ( 'NONE',  ( 3.696290335837215668, -2.159122111672501454, -0.1082323872379290647 ) ) ;
#91814 = COLOUR_RGB ( '', 0.40784314, 0.44705882, 0.49803922) ;
#91815 = CARTESIAN_POINT ( 'NONE',  ( 5.870470189955956819, -0.4925641237488035395, 1.954873771647095415 ) ) ;
#91816 = CARTESIAN_POINT ( 'NONE',  ( -9.124274191872645545, 9.747334100047323702, -0.7216878364870267237 ) ) ;
#91817 = CARTESIAN_POINT ( 'NONE',  ( 3.502937704049163159, 1.705309618848281472, -1.328393843302433153 ) ) ;
#91818 = CARTESIAN_POINT ( 'NONE',  ( 3.409407428336236556, -0.3879349331968630077, 1.932650128172111126 ) ) ;
#91819 = AXIS2_PLACEMENT_3D ( 'NONE', #81014, #143932, #197949 ) ;
#91820 = CARTESIAN_POINT ( 'NONE',  ( 0.09952931447375359952, -0.5783855404800625211, 2.113812074898171023 ) ) ;
#91821 = CARTESIAN_POINT ( 'NONE',  ( 0.9741375256873509025, 2.223107509294399264, -0.6184994596578182735 ) ) ;
#91822 = CARTESIAN_POINT ( 'NONE',  ( 2.214203678495901606, -0.9685002052983943122, -1.818986401426671229 ) ) ;
#91823 = CARTESIAN_POINT ( 'NONE',  ( 5.179219622276672652, 1.307079648806110050, 1.436513822289321674 ) ) ;
#91825 = ORIENTED_EDGE ( 'NONE', *, *, #156316, .F. ) ;
#91824 = CARTESIAN_POINT ( 'NONE',  ( -6.846504384776750385, 10.93141284897413890, -0.7216878364870267237 ) ) ;
#91826 = CARTESIAN_POINT ( 'NONE',  ( -5.271087860662956537, 9.371629280740593870, 0.000000000000000000 ) ) ;
#91827 = CARTESIAN_POINT ( 'NONE',  ( 11.84668729035180590, 10.09481419982586736, 1.399999999999998357 ) ) ;
#91829 = ORIENTED_EDGE ( 'NONE', *, *, #129837, .T. ) ;
#91828 = CARTESIAN_POINT ( 'NONE',  ( -6.168033539574333979, 6.160736982450306876, 0.7998128361456281477 ) ) ;
#91830 = CARTESIAN_POINT ( 'NONE',  ( -7.551528372687420720, 8.872833191965849409, 1.082531754730558626 ) ) ;
#91831 = CARTESIAN_POINT ( 'NONE',  ( 2.468050989216635127, 2.164326253657654853, -0.4298898877757306725 ) ) ;
#91832 = CARTESIAN_POINT ( 'NONE',  ( -3.285556943750000070, -3.346874999522041261, 0.000000000000000000 ) ) ;
#91833 = CARTESIAN_POINT ( 'NONE',  ( 6.104347744599991188, 1.959368324604572775, 0.09974838594294095639 ) ) ;
#91834 =( BOUNDED_CURVE ( )  B_SPLINE_CURVE ( 2, ( #195577, #94891, #162018, #163085, #144731, #30956, #66588 ),
 .UNSPECIFIED., .F., .T. ) 
 B_SPLINE_CURVE_WITH_KNOTS ( ( 3, 2, 2, 3 ),
 ( 0.2857142857142859760, 0.2916666666666668517, 0.2976190476190477274, 0.3035714285714285476 ),
 .UNSPECIFIED. ) 
 CURVE ( )  GEOMETRIC_REPRESENTATION_ITEM ( )  RATIONAL_B_SPLINE_CURVE ( ( 0.9999999999999937828, 0.8660254037844449249, 1.000000000000000000, 0.8660254037844387076, 1.000000000000000000, 0.8660254037844387076, 1.000000000000000000 ) ) 
 REPRESENTATION_ITEM ( '' )  );
#91835 = CARTESIAN_POINT ( 'NONE',  ( 6.539320575229237598, 1.252639605590206928, 2.218328189723097754 ) ) ;
#91836 = CARTESIAN_POINT ( 'NONE',  ( -1.500000000000011324, 4.910416667349486453, -0.8660254037844313801 ) ) ;
#91838 = CARTESIAN_POINT ( 'NONE',  ( 6.720655732516642722, 0.008434553976904573744, 1.726293928996263549 ) ) ;
#91837 = CARTESIAN_POINT ( 'NONE',  ( -6.161504026110072196, 7.065710439381887475, -1.087211863304170523 ) ) ;
#91839 = CARTESIAN_POINT ( 'NONE',  ( 5.929618730664214077, 0.9035273275350870215, -1.604119651413847603 ) ) ;
#91840 = VERTEX_POINT ( 'NONE', #115645 ) ;
#91841 = CARTESIAN_POINT ( 'NONE',  ( 2.184514296101589537, -2.020881322650217360, -0.4031914428916544280 ) ) ;
#91842 = CARTESIAN_POINT ( 'NONE',  ( -2.754243431018125239E-14, 0.2031250003414269978, 1.570758158831750295 ) ) ;
#91843 = UNCERTAINTY_MEASURE_WITH_UNIT (LENGTH_MEASURE( 1.000000000000000082E-05 ), #145996, 'distance_accuracy_value', 'NONE');
#91844 = CARTESIAN_POINT ( 'NONE',  ( -6.073162743917628781, 9.172774736957510555, -1.199719254218440723 ) ) ;
#91845 = CARTESIAN_POINT ( 'NONE',  ( 10.91808280586644919, -9.921948886890824326, -0.1881369732364152614 ) ) ;
#91846 = CARTESIAN_POINT ( 'NONE',  ( 6.345950370838200350, -1.386202306585911925, -1.604841549997563455 ) ) ;
#91847 = CARTESIAN_POINT ( 'NONE',  ( 8.889064146099206809, 12.82244507866851180, 7.992677692963079394 ) ) ;
#91848 = CARTESIAN_POINT ( 'NONE',  ( 5.996784015946103885, 5.890669528225568996, 1.040834085586084257E-14 ) ) ;
#91849 = CARTESIAN_POINT ( 'NONE',  ( 0.8661736431406670267, 1.015005012832224329, 1.793514120848164195 ) ) ;
#91851 = CARTESIAN_POINT ( 'NONE',  ( 4.423293856316495187, -1.136390847421838490, -1.448631019334602144 ) ) ;
#91850 = CARTESIAN_POINT ( 'NONE',  ( 0.000000000000000000, 7.999999999999992895, 5.500000000000002665 ) ) ;
#91852 = CARTESIAN_POINT ( 'NONE',  ( 8.281332899848809603, 8.555976559445431562, 0.7998128361456481317 ) ) ;
#91853 = CARTESIAN_POINT ( 'NONE',  ( -8.159939477482263115, 15.51961010445367961, 8.809817911661959045 ) ) ;
#91854 = CARTESIAN_POINT ( 'NONE',  ( -6.805266759416629618, 6.904175738932996964, 0.000000000000000000 ) ) ;
#91856 = EDGE_LOOP ( 'NONE', ( #31967, #9404, #188573, #99127 ) ) ;
#91855 = FACE_BOUND ( 'NONE', #129037, .T. ) ;
#91857 =( GEOMETRIC_REPRESENTATION_CONTEXT ( 3 ) GLOBAL_UNCERTAINTY_ASSIGNED_CONTEXT ( ( #192437 ) ) GLOBAL_UNIT_ASSIGNED_CONTEXT ( ( #50885, #134301, #202433 ) ) REPRESENTATION_CONTEXT ( 'NONE', 'WORKASPACE' ) );
#91858 = CARTESIAN_POINT ( 'NONE',  ( 4.231241840954825584, 0.1069408422738199749, 2.204416794138922331 ) ) ;
#91859 = CARTESIAN_POINT ( 'NONE',  ( 0.4390364970160881564, 0.3691015439823107092, 2.129678967336546602 ) ) ;
#91860 = CARTESIAN_POINT ( 'NONE',  ( 3.678922940808615483, 1.700962499606586853, -1.082838980105811366 ) ) ;
#91861 = CARTESIAN_POINT ( 'NONE',  ( -4.758548728716557541, 8.495464583570553785, 1.040834085586084257E-14 ) ) ;
#91862 = CARTESIAN_POINT ( 'NONE',  ( 0.3164790345465406385, -0.6463921985436006379, -1.799943259716822341 ) ) ;
#91863 = CARTESIAN_POINT ( 'NONE',  ( -0.2234322562767385167, -0.4468160588090731022, -1.973564571300358228 ) ) ;
#91864 = CARTESIAN_POINT ( 'NONE',  ( 0.08058608058606961388, -5.907420853759267843, -10.99970480893079738 ) ) ;
#91865 = LINE ( 'NONE', #157921, #833 ) ;
#91866 = CARTESIAN_POINT ( 'NONE',  ( 5.602191078447533279, -0.8559053986842228845, 1.710104642658970775 ) ) ;
#91867 = CARTESIAN_POINT ( 'NONE',  ( 0.000000000000000000, -1.500000000000001332, 1.249999999999999778 ) ) ;
#91868 = CARTESIAN_POINT ( 'NONE',  ( 0.7779422811538607707, -1.042605501850740080, 1.552959968518424771 ) ) ;
#91869 = VECTOR ( 'NONE', #165721, 1000.000000000000000 ) ;
#91870 = CARTESIAN_POINT ( 'NONE',  ( 2.553923023464285347, 1.082840749376843270, 1.700961377887353798 ) ) ;
#91872 = CARTESIAN_POINT ( 'NONE',  ( 4.178421505988277218, -1.212938584752444093, 1.721516029631239064 ) ) ;
#91871 = CARTESIAN_POINT ( 'NONE',  ( -8.850775351622791831, 9.220326086515070685, -0.7998128361456291469 ) ) ;
#91873 = CARTESIAN_POINT ( 'NONE',  ( 7.958799866421889746, 9.244020251369077457, -1.199719254218441611 ) ) ;
#91875 = CARTESIAN_POINT ( 'NONE',  ( -7.015454420067433361, 10.27211502579893754, 1.199719254218453823 ) ) ;
#91874 = CARTESIAN_POINT ( 'NONE',  ( 1.499999999999987566, 0.02500000000001806333, 0.000000000000000000 ) ) ;
#91876 = CARTESIAN_POINT ( 'NONE',  ( 11.48243876534946217, 9.799999999999982947, 3.199999999999997957 ) ) ;
#91877 = CARTESIAN_POINT ( 'NONE',  ( 3.586198609924298175, 1.125526462575956010, 1.676902781687271915 ) ) ;
#91878 = CARTESIAN_POINT ( 'NONE',  ( -0.6823417656250212460, 5.301041667008086655, 1.181850606188767472 ) ) ;
#91879 = CIRCLE ( 'NONE', #46887, 11.09999999999999964 ) ;
#91880 = CARTESIAN_POINT ( 'NONE',  ( 9.246297574839974942, 11.81043314211192019, 1.443375672974076540 ) ) ;
#91881 = CARTESIAN_POINT ( 'NONE',  ( 4.095124908492456584, 1.828510582809875107, -1.152538879107746439 ) ) ;
#91882 = CARTESIAN_POINT ( 'NONE',  ( 11.48243876534946217, 12.30000000000000071, -3.200000000000001510 ) ) ;
#91883 = CARTESIAN_POINT ( 'NONE',  ( -1.500000000000011324, 4.629166666666689522, -0.8660254037844313801 ) ) ;
#91885 = FACE_OUTER_BOUND ( 'NONE', #39699, .T. ) ;
#91884 = CARTESIAN_POINT ( 'NONE',  ( 5.529746549527311039, 7.544733289238903851, -1.599625672291281386 ) ) ;
#91886 = CARTESIAN_POINT ( 'NONE',  ( 8.934460041281305109, 10.48625347199211966, -1.082531754730543083 ) ) ;
#91888 = CARTESIAN_POINT ( 'NONE',  ( 3.331659036430331344, 7.719744385808881226, 2.450696915730453007 ) ) ;
#91887 = CARTESIAN_POINT ( 'NONE',  ( 2.137404458564879484, -0.1051889750803415707, -2.168730265314787076 ) ) ;
#91890 = CARTESIAN_POINT ( 'NONE',  ( 0.7316835000789992938, 1.813914744281470925, 0.3150931809976220133 ) ) ;
#91889 = CARTESIAN_POINT ( 'NONE',  ( -5.260200412422196159, 9.080724881227137502, -0.7216878364870207285 ) ) ;
#91891 = CARTESIAN_POINT ( 'NONE',  ( -1.402160292154681736E-14, 1.446875000341420137, -1.575800808251659024 ) ) ;
#91892 = CARTESIAN_POINT ( 'NONE',  ( 2.894263506066748093, -0.6386881658498286818, -2.096408367471907841 ) ) ;
#91893 = CARTESIAN_POINT ( 'NONE',  ( 6.512744780709700088, 6.750401516064612473, 0.09762648057792142064 ) ) ;
#91894 = CARTESIAN_POINT ( 'NONE',  ( 3.924925821460770514, 2.147445456087885063, 0.7125370657276063335 ) ) ;
#91895 = CARTESIAN_POINT ( 'NONE',  ( -5.696397096036042385, 9.797547045350714967, -0.7998128361456231517 ) ) ;
#91896 = CARTESIAN_POINT ( 'NONE',  ( -1.364683531249997417, 4.821875000341417916, 1.214306433183764966E-14 ) ) ;
#91897 = CARTESIAN_POINT ( 'NONE',  ( 6.276967689384127524, 6.888745287521969907, 0.7578909454171089966 ) ) ;
#91898 = CARTESIAN_POINT ( 'NONE',  ( 1.500000000000001332, 12.87499999999999822, 0.000000000000000000 ) ) ;
#91899 = CARTESIAN_POINT ( 'NONE',  ( 5.885648082108188461, 8.920320958217979879, 1.082531754730549967 ) ) ;
#91900 = CARTESIAN_POINT ( 'NONE',  ( 4.253014324580971284, -1.470476824294727702, -0.9843664617138027095 ) ) ;
#91901 = CARTESIAN_POINT ( 'NONE',  ( 10.07100917685271035, 10.64393221595000938, 0.7998128361456462443 ) ) ;
#91902 = CARTESIAN_POINT ( 'NONE',  ( 0.3058767667667975365, -0.5614299121656821656, 2.029657625958045664 ) ) ;
#91904 = CARTESIAN_POINT ( 'NONE',  ( -1.500000000000001332, 1.150000000000019007, 0.000000000000000000 ) ) ;
#91903 = CARTESIAN_POINT ( 'NONE',  ( -1.364683531250014514, 10.58854166700806765, -0.7879004041258335089 ) ) ;
#91905 = CARTESIAN_POINT ( 'NONE',  ( 1.469134468336911192, 1.735519167469494084, 0.9312130504785380847 ) ) ;
#91906 = CARTESIAN_POINT ( 'NONE',  ( -4.664887371553763096, 7.600063145858131364, -1.199719254218453823 ) ) ;
#91907 = CARTESIAN_POINT ( 'NONE',  ( 6.521112179100128969, -1.799899466697444383, 0.9092066555835758290 ) ) ;
#91908 = ORIENTED_EDGE ( 'NONE', *, *, #161956, .T. ) ;
#91909 = CARTESIAN_POINT ( 'NONE',  ( 5.639828713604826405, 9.523624565940227882, -0.7216878364870267237 ) ) ;
#91910 = EDGE_CURVE ( 'NONE', #5587, #67094, #148352, .T. ) ;
#91911 = CARTESIAN_POINT ( 'NONE',  ( 4.293723057671197552, -0.7160966649314598476, 1.728361679364013748 ) ) ;
#91912 = CARTESIAN_POINT ( 'NONE',  ( 4.311429529933403337, -1.718370896367764189, -1.154329086688666184 ) ) ;
#91913 = CARTESIAN_POINT ( 'NONE',  ( -4.356712336337761644E-14, 1.812499999999968470, 1.414508159514561436 ) ) ;
#91914 = CARTESIAN_POINT ( 'NONE',  ( -4.760321331729590710, 8.567808963744235839, 0.7216878364870267237 ) ) ;
#91915 = CARTESIAN_POINT ( 'NONE',  ( -1.500000000000001110, 10.80208333401613707, 0.8660254037844418162 ) ) ;
#91916 = CARTESIAN_POINT ( 'NONE',  ( 9.250740883225924804, 9.686952540052077509, 1.040834085586084257E-14 ) ) ;
#91917 = CARTESIAN_POINT ( 'NONE',  ( -9.130526383799315582, 12.73969898348616070, 1.199719254218462483 ) ) ;
#91918 = CARTESIAN_POINT ( 'NONE',  ( 5.481239241674765950, 9.616805891921051952, -0.7998128361456481317 ) ) ;
#91919 = CARTESIAN_POINT ( 'NONE',  ( -5.817856928050925802, 5.960123635580414359, -1.359047942450207100E-08 ) ) ;
#91920 = CARTESIAN_POINT ( 'NONE',  ( 1.364683531249988535, 5.467708333674750953, -0.7879004041258300672 ) ) ;
#91921 = EDGE_CURVE ( 'NONE', #61933, #210405, #99352, .T. ) ;
#91922 = CARTESIAN_POINT ( 'NONE',  ( 4.035565188342554954, 1.848088059160474694, -0.6588067414724924076 ) ) ;
#91923 = CARTESIAN_POINT ( 'NONE',  ( 1.774767310740912984, -2.001205085354029301, 0.2439901982170673556 ) ) ;
#91924 = DIRECTION ( 'NONE',  ( 8.659560562354987092E-17, 0.7071067811865432429, -0.7071067811865517916 ) ) ;
#91925 = CARTESIAN_POINT ( 'NONE',  ( -4.944471571578556102, 4.870897709704155254, -0.2071306710573853627 ) ) ;
#91926 = CARTESIAN_POINT ( 'NONE',  ( 1.053721402318724021, 1.868689351376726204, -0.08586956420430363890 ) ) ;
#91927 = CARTESIAN_POINT ( 'NONE',  ( 0.6823417656249917140, 4.342708333674755394, 1.181850606188765695 ) ) ;
#91928 = CARTESIAN_POINT ( 'NONE',  ( 2.760023647720879492, 0.7205980239477025595, -1.880007780590841282 ) ) ;
#91930 = CARTESIAN_POINT ( 'NONE',  ( 3.321969493568678988, 0.9498371968033242352, -1.892263307760349900 ) ) ;
#91929 = CARTESIAN_POINT ( 'NONE',  ( -5.070386261830872598, 8.859275038870594088, 0.7216878364870458196 ) ) ;
#91931 = CARTESIAN_POINT ( 'NONE',  ( 0.7499999999999920064, 5.014583334016150751, 1.299038105676669330 ) ) ;
#91932 = CARTESIAN_POINT ( 'NONE',  ( 4.387213907293201487, 0.09840592021137170575, 2.068135374880715638 ) ) ;
#91933 = CARTESIAN_POINT ( 'NONE',  ( 4.543917759235442944, 5.330267469643351852, 1.199719254218452935 ) ) ;
#91935 = CARTESIAN_POINT ( 'NONE',  ( 11.86239285000045918, 13.79999999999998295, 1.812080536912751283 ) ) ;
#91934 = CARTESIAN_POINT ( 'NONE',  ( 0.4332924875789189167, -1.481350984940564830, -1.475676199967065338 ) ) ;
#91937 = ORIENTED_EDGE ( 'NONE', *, *, #193834, .F. ) ;
#91936 = CARTESIAN_POINT ( 'NONE',  ( 5.034128509002383289, 0.9373949799435166153, -1.566401400633938179 ) ) ;
#91938 = CARTESIAN_POINT ( 'NONE',  ( 7.618792255875527886, 10.97600916757510170, 1.199719254218460707 ) ) ;
#91939 = CARTESIAN_POINT ( 'NONE',  ( 3.289951133708762576, 7.658661826346122581, -2.499999999999995115 ) ) ;
#91940 = CARTESIAN_POINT ( 'NONE',  ( -10.49071307728992153, 3.038037579769635066, 7.129592439487457689 ) ) ;
#91941 = CARTESIAN_POINT ( 'NONE',  ( 1.364683531250000748, 11.81770833367472839, -0.7879004041258355073 ) ) ;
#91942 = CARTESIAN_POINT ( 'NONE',  ( 6.586579894266018975, -1.172543786506787145, 1.511232097859278367 ) ) ;
#91943 = CARTESIAN_POINT ( 'NONE',  ( -7.472515219426274946, 11.86968485597268064, 0.000000000000000000 ) ) ;
#91944 = CARTESIAN_POINT ( 'NONE',  ( 6.979750152936881058, 7.037463354714830643, 0.7998128361456341429 ) ) ;
#91945 = CARTESIAN_POINT ( 'NONE',  ( -11.84103413958613160, 11.11004478473142676, -1.443924719788764799 ) ) ;
#91946 = ADVANCED_FACE ( 'NONE', ( #183786 ), #200021, .T. ) ;
#91947 = CARTESIAN_POINT ( 'NONE',  ( -2.081668171172168513E-14, 5.868705557303649734, 4.125226524755077229 ) ) ;
#91948 = CARTESIAN_POINT ( 'NONE',  ( 5.359550796103802028, 5.147230771742885125, -0.7998128361456231517 ) ) ;
#91949 = EDGE_LOOP ( 'NONE', ( #175323, #179358, #74871, #110229 ) ) ;
#91950 = CARTESIAN_POINT ( 'NONE',  ( -6.261886844665283114, 8.398896966899865646, 1.599625672291269396 ) ) ;
#91951 = CARTESIAN_POINT ( 'NONE',  ( 5.483999976877721672, -2.016598147233912730, 0.002826481282774962345 ) ) ;
#91952 = FACE_OUTER_BOUND ( 'NONE', #69195, .T. ) ;
#91953 =( GEOMETRIC_REPRESENTATION_CONTEXT ( 3 ) GLOBAL_UNCERTAINTY_ASSIGNED_CONTEXT ( ( #176767 ) ) GLOBAL_UNIT_ASSIGNED_CONTEXT ( ( #107834, #25435, #26505 ) ) REPRESENTATION_CONTEXT ( 'NONE', 'WORKASPACE' ) );
#91954 = CARTESIAN_POINT ( 'NONE',  ( 3.146123468421266001, 6.442327133617253843, 0.5169845646841256803 ) ) ;
#91955 = CARTESIAN_POINT ( 'NONE',  ( -6.435690514315323796, 6.800136771869164320, 0.4354173353855045336 ) ) ;
#91956 = CARTESIAN_POINT ( 'NONE',  ( -6.087247782855839340, 6.204136622861004646, 0.000000000000000000 ) ) ;
#91957 = CIRCLE ( 'NONE', #130060, 0.8300000000000008482 ) ;
#91958 = CARTESIAN_POINT ( 'NONE',  ( 3.011882680530176604, 6.665613560593854459, 0.7998128361456341429 ) ) ;
#91959 = CARTESIAN_POINT ( 'NONE',  ( 2.465619613223976270, -0.4363654233677862759, 1.920310867443141278 ) ) ;
#91960 = EDGE_CURVE ( 'NONE', #206340, #174590, #185905, .T. ) ;
#91961 = CARTESIAN_POINT ( 'NONE',  ( 3.620720401301917857, 0.2986476686686300175, 1.994069442355271615 ) ) ;
#91962 = CARTESIAN_POINT ( 'NONE',  ( -6.482770005628665011, 10.71498210654212002, 0.7998128361456481317 ) ) ;
#91963 = CARTESIAN_POINT ( 'NONE',  ( 6.727182134110195832, 2.427649464305783322, 2.470530574517680655 ) ) ;
#91964 = CARTESIAN_POINT ( 'NONE',  ( 4.207102436150745639, -0.3756362130699179014, 2.158856393654845274 ) ) ;
#91965 = DIRECTION ( 'NONE',  ( 1.509903313490213211E-14, 0.000000000000000000, -1.000000000000000000 ) ) ;
#91966 = CARTESIAN_POINT ( 'NONE',  ( 2.186434445367648749, -1.888794084208703206, -0.3779312967549207092 ) ) ;
#91967 = CARTESIAN_POINT ( 'NONE',  ( -7.483210719738908168, 10.81783070874899799, 1.199719254218453823 ) ) ;
#91968 = EDGE_CURVE ( 'NONE', #171094, #70036, #202899, .T. ) ;
#91969 = CARTESIAN_POINT ( 'NONE',  ( 1.773601632590606955E-15, -3.437048488108780906E-15, -0.2598076211376265099 ) ) ;
#91970 = CARTESIAN_POINT ( 'NONE',  ( 0.1329588055935214119, 5.724880713053031478, -2.439996743105294907 ) ) ;
#91971 = CARTESIAN_POINT ( 'NONE',  ( 7.283754839039659146, 9.520799950344851936, -1.599625672291262513 ) ) ;
#91972 = CARTESIAN_POINT ( 'NONE',  ( 3.988069740714122791, 7.804498464141805592, 0.7998128361456321445 ) ) ;
#91973 = CARTESIAN_POINT ( 'NONE',  ( -1.225000000000028066, 1.229166666666677843, -0.7072540797573078075 ) ) ;
#91974 = CARTESIAN_POINT ( 'NONE',  ( 6.265276383290871109, 7.442482214328385304, -1.082531754730548412 ) ) ;
#91975 = ORIENTED_EDGE ( 'NONE', *, *, #141380, .T. ) ;
#91977 = CARTESIAN_POINT ( 'NONE',  ( 3.281892451336921201, 1.963554472591656053, -0.4431533499722385416 ) ) ;
#91976 = CARTESIAN_POINT ( 'NONE',  ( 6.427308110136687347, -1.208249125052461181, -1.389453836245766016 ) ) ;
#91978 = CARTESIAN_POINT ( 'NONE',  ( 4.622621100999918298, 0.5092349069827777353, -2.241135911243127055 ) ) ;
#91980 = CARTESIAN_POINT ( 'NONE',  ( 2.676407432925419272, 1.219717815897247259, -1.405545362062944559 ) ) ;
#91979 = CARTESIAN_POINT ( 'NONE',  ( -0.02900071798684483726, 7.629137130509101361, -2.773797386654376584 ) ) ;
#91981 = CARTESIAN_POINT ( 'NONE',  ( -1.642778471875000035, -1.217708332855376607, -2.845375778867859751 ) ) ;
#91982 = DIRECTION ( 'NONE',  ( 0.000000000000000000, 0.000000000000000000, -1.000000000000000000 ) ) ;
#91983 = CARTESIAN_POINT ( 'NONE',  ( 6.521744167503259249, -0.4122283346772101509, 1.874327247564554266 ) ) ;
#91984 = CARTESIAN_POINT ( 'NONE',  ( -7.588813295347149435, 9.876701482703580837, -1.599625672291263179 ) ) ;
#91985 = CARTESIAN_POINT ( 'NONE',  ( -3.689227196694341515, 7.318199139536432973, -0.7216878364870458196 ) ) ;
#91986 = CARTESIAN_POINT ( 'NONE',  ( 5.583562150179168349, -0.9389753047652232842, 1.868084059271076347 ) ) ;
#91987 = CARTESIAN_POINT ( 'NONE',  ( 6.399085315970131305, 8.488685506763726352, -1.443375672974057666 ) ) ;
#91988 = ORIENTED_EDGE ( 'NONE', *, *, #72060, .F. ) ;
#91989 = CARTESIAN_POINT ( 'NONE',  ( 0.000000000000000000, 3.466143782776612170, 0.000000000000000000 ) ) ;
#91990 = DIRECTION ( 'NONE',  ( -0.8660254037844397068, 0.4999999999999978906, 0.000000000000000000 ) ) ;
#91991 = CARTESIAN_POINT ( 'NONE',  ( 6.094358798449852621, -1.717309950877196956, -0.1615796057152525667 ) ) ;
#91992 = CARTESIAN_POINT ( 'NONE',  ( -6.033542053281340856, 6.997886136038390603, -1.199719254218446718 ) ) ;
#91993 = CARTESIAN_POINT ( 'NONE',  ( 1.494300775288709415, -1.721104260995092838, 0.2117000974225565491 ) ) ;
#91994 =( NAMED_UNIT ( * ) PLANE_ANGLE_UNIT ( ) SI_UNIT ( $, .RADIAN. ) );
#91995 = DIRECTION ( 'NONE',  ( -0.7592566023652995710, 0.6507913734559650498, 0.000000000000000000 ) ) ;
#91996 = CARTESIAN_POINT ( 'NONE',  ( -0.6170404364503407901, -1.000000000000000888, 1.902435570468869797 ) ) ;
#91997 = CARTESIAN_POINT ( 'NONE',  ( 5.805598453987085072, -1.706804643700374102, -1.341652511797826186 ) ) ;
#91998 = CARTESIAN_POINT ( 'NONE',  ( 4.160648861918358143, -1.351394993475165673, 1.227733137840483879 ) ) ;
#91999 = CARTESIAN_POINT ( 'NONE',  ( 2.254674508890702089, -0.5182927192734412269, -1.892014123021222627 ) ) ;
#92000 = PLANE ( 'NONE',  #127094 ) ;
#92001 = DIRECTION ( 'NONE',  ( 0.8003905296791061774, 0.000000000000000000, -0.5994789404140897782 ) ) ;
#92002 = CARTESIAN_POINT ( 'NONE',  ( 6.903072767652295383, 11.20533532890304684, 1.040834085586084257E-14 ) ) ;
#92003 = CARTESIAN_POINT ( 'NONE',  ( 3.123802294713691641, -0.4116375371931815796, 2.079978743196985391 ) ) ;
#92004 = CARTESIAN_POINT ( 'NONE',  ( -2.304522924643024773, 5.632434478818063361, 0.7216878364870317197 ) ) ;
#92005 = FILL_AREA_STYLE ('',( #159111 ) ) ;
#92006 = AXIS2_PLACEMENT_3D ( 'NONE', #1081, #199287, #202478 ) ;
#92007 = VECTOR ( 'NONE', #204012, 1000.000000000000000 ) ;
#92008 = CARTESIAN_POINT ( 'NONE',  ( -5.402149754905330781, 6.322992007072439691, -1.066970298751448443 ) ) ;
#92009 = CARTESIAN_POINT ( 'NONE',  ( 0.5849358142855852760, 1.980036476162419845, 0.6043757699017647811 ) ) ;
#92011 = CARTESIAN_POINT ( 'NONE',  ( 0.7500000000000006661, 14.69791666734946567, -1.299038105676657340 ) ) ;
#92010 = CARTESIAN_POINT ( 'NONE',  ( -10.46082884891970366, 3.933599711960402256, 5.880821593625136678 ) ) ;
#92013 = ORIENTED_EDGE ( 'NONE', *, *, #113537, .F. ) ;
#92012 = CARTESIAN_POINT ( 'NONE',  ( 3.510577332121900707, -2.218788133798971884, -0.1078075537720973032 ) ) ;
#92014 = CARTESIAN_POINT ( 'NONE',  ( 1.020660257703887908, -2.075033540828072454, 0.9893533861183384515 ) ) ;
#92016 = CARTESIAN_POINT ( 'NONE',  ( 6.930530977065029852, -1.274000060550171787, 1.622871787371343855 ) ) ;
#92015 = CARTESIAN_POINT ( 'NONE',  ( 10.05978679165993483, 11.79913468076720306, 1.082531754730548412 ) ) ;
#92018 = CARTESIAN_POINT ( 'NONE',  ( 3.475000000000000533, -0.5250000000000011324, 0.000000000000000000 ) ) ;
#92017 = CARTESIAN_POINT ( 'NONE',  ( 3.878514461961128479, 6.682628084666728085, -1.199719254218448494 ) ) ;
#92019 = CARTESIAN_POINT ( 'NONE',  ( -1.833030277982346634, 2.531131934864056632, -2.499999999999998668 ) ) ;
#92020 = DIRECTION ( 'NONE',  ( 0.000000000000000000, -1.000000000000000000, 0.000000000000000000 ) ) ;
#92022 = CARTESIAN_POINT ( 'NONE',  ( -1.607015867998808023, -0.9165151389911689872, 1.199999999999999734 ) ) ;
#92021 = PRESENTATION_LAYER_ASSIGNMENT (  '', '', ( #123175 ) ) ;
#92023 = CARTESIAN_POINT ( 'NONE',  ( -0.2106725631050307412, 6.947230693896488951, -2.598707507344534040 ) ) ;
#92024 = CARTESIAN_POINT ( 'NONE',  ( 2.977275877015468364, 1.638319938685417476, -0.5394319952881917457 ) ) ;
#92025 = CARTESIAN_POINT ( 'NONE',  ( 2.237517880698642880, 0.5331670712399002587, -1.944730990508992008 ) ) ;
#92026 = CARTESIAN_POINT ( 'NONE',  ( 2.479437202158024878, -2.292751561675594907, -0.1657748548101884711 ) ) ;
#92027 = CARTESIAN_POINT ( 'NONE',  ( 3.040562418613635742, 2.244949603584453612, 0.2802003048723368805 ) ) ;
#92028 = CARTESIAN_POINT ( 'NONE',  ( 4.793641967770590817, 1.559994068796449529, 1.415095702743226047 ) ) ;
#92029 = CARTESIAN_POINT ( 'NONE',  ( -5.465345320084574965, 9.390336950158399532, 0.000000000000000000 ) ) ;
#92030 = CARTESIAN_POINT ( 'NONE',  ( 3.708038350156193541, -0.7148330724025107052, -1.619118029916452262 ) ) ;
#92032 = CARTESIAN_POINT ( 'NONE',  ( 0.05906008026819106055, -2.050595067678960604, -1.024705011274627431 ) ) ;
#92031 = CARTESIAN_POINT ( 'NONE',  ( 4.055297343818933697, 5.824542549245813383, 1.443375672974058777 ) ) ;
#92033 = CARTESIAN_POINT ( 'NONE',  ( 5.788959344212086577, 1.397023377451442228, 1.199316859253784839 ) ) ;
#92035 = EDGE_CURVE ( 'NONE', #36555, #182678, #52720, .T. ) ;
#92034 = CARTESIAN_POINT ( 'NONE',  ( -2.761056838677368397, 6.372983411765559048, 0.7998128361456341429 ) ) ;
#92036 = CARTESIAN_POINT ( 'NONE',  ( 3.972175818679561043, 7.578029521860726092, -0.7216878364870197293 ) ) ;
#92037 = CARTESIAN_POINT ( 'NONE',  ( -0.7500000000000215383, 3.941666666666690411, 1.299038105676671107 ) ) ;
#92038 = CARTESIAN_POINT ( 'NONE',  ( 5.156268285673103691, -1.588865937562380148, 1.509524371192130676 ) ) ;
#92039 = CARTESIAN_POINT ( 'NONE',  ( -2.462777459176719308, 6.024990802348131780, -0.7998128361456281477 ) ) ;
#92040 = CARTESIAN_POINT ( 'NONE',  ( 0.05568659246542585761, 15.51846069310708387, 11.99987079111352983 ) ) ;
#92041 = CARTESIAN_POINT ( 'NONE',  ( 5.424307079040114665, 1.017280057988108499, 1.803113764695261523 ) ) ;
#92042 = CARTESIAN_POINT ( 'NONE',  ( 0.1984543448181053105, 1.387095780679182377, -1.463931301963219855 ) ) ;
#92043 = CARTESIAN_POINT ( 'NONE',  ( -0.6823417656250212460, 4.551041667008086655, 1.181850606188767472 ) ) ;
#92044 = CARTESIAN_POINT ( 'NONE',  ( 2.859893552614915180, 1.917175687707149967, -0.1893568897016733310 ) ) ;
#92045 = CARTESIAN_POINT ( 'NONE',  ( 1.364683531250000303, 10.00520833367473017, -0.7879004041258355073 ) ) ;
#92046 = DIRECTION ( 'NONE',  ( -8.638326563840814399E-31, 0.000000000000000000, -1.000000000000000000 ) ) ;
#92047 = CARTESIAN_POINT ( 'NONE',  ( -0.2044637419536878831, -0.1604900674421188000, -2.186121014245277383 ) ) ;
#92048 = ORIENTED_EDGE ( 'NONE', *, *, #95890, .F. ) ;
#92050 = DIRECTION ( 'NONE',  ( 0.000000000000000000, 1.000000000000000000, 0.000000000000000000 ) ) ;
#92049 = CARTESIAN_POINT ( 'NONE',  ( -5.180624094197616714, 5.216685329418210948, 0.7216878364870257245 ) ) ;
#92051 = CARTESIAN_POINT ( 'NONE',  ( 4.891794496432329886, 4.601515088792824670, -0.7998128361456211532 ) ) ;
#92052 = CARTESIAN_POINT ( 'NONE',  ( 1.464677571780234644E-15, 0.000000000000000000, -11.92000000000000171 ) ) ;
#92053 = CARTESIAN_POINT ( 'NONE',  ( -1.992711204631002198E-15, 2.999999999999989342, 1.224999999999989875 ) ) ;
#92054 = DIRECTION ( 'NONE',  ( -0.000000000000000000, -1.000000000000000000, -0.000000000000000000 ) ) ;
#92055 = DIRECTION ( 'NONE',  ( -0.7347175152297780176, 0.000000000000000000, 0.6783731810844091381 ) ) ;
#92056 = CARTESIAN_POINT ( 'NONE',  ( 0.8011316787140990714, -1.684513426579350659, 1.005393624328714264 ) ) ;
#92057 = CARTESIAN_POINT ( 'NONE',  ( -0.6823417656250212460, 1.613541667008083769, 1.181850606188755259 ) ) ;
#92058 = CARTESIAN_POINT ( 'NONE',  ( 5.881297811770386907, -0.04968318840743202180, 1.961410508136133712 ) ) ;
#92059 = CARTESIAN_POINT ( 'NONE',  ( -7.486073373039941359, 11.88550270185529278, -0.7998128361456291469 ) ) ;
#92060 = CARTESIAN_POINT ( 'NONE',  ( -4.731432421044873493, 7.503459676985569260, -1.082531754730548412 ) ) ;
#92061 = CARTESIAN_POINT ( 'NONE',  ( 6.719591497160966931, -2.098179372288328182, 0.5198544864785522579 ) ) ;
#92063 = ORIENTED_EDGE ( 'NONE', *, *, #130801, .F. ) ;
#92062 = CARTESIAN_POINT ( 'NONE',  ( -0.2106725631050202496, 0.2307243749109839093, -2.036935839376171842 ) ) ;
#92064 = CARTESIAN_POINT ( 'NONE',  ( -0.6823417656250212460, 5.551041667008087543, 1.181850606188767472 ) ) ;
#92065 = CARTESIAN_POINT ( 'NONE',  ( 0.3154175708385241750, -1.835744252435017598, 0.3582649291258357960 ) ) ;
#92066 = CARTESIAN_POINT ( 'NONE',  ( 6.714187037452940210, -1.395258515317991943, -1.029009966057025549 ) ) ;
#92068 = CARTESIAN_POINT ( 'NONE',  ( 3.052458795248469414, -1.657928338269051505, 1.433322580492613296 ) ) ;
#92067 = CARTESIAN_POINT ( 'NONE',  ( -1.360316468750023544, 0.8906250003414064587, -2.602085213965210642E-14 ) ) ;
#92069 = CARTESIAN_POINT ( 'NONE',  ( 4.630063564305310742, -1.415688044924306555, -1.822237510073132949 ) ) ;
#92070 = CARTESIAN_POINT ( 'NONE',  ( 0.2333700457068142997, -1.884473515381725361, 0.8346939899398809759 ) ) ;
#92071 = CARTESIAN_POINT ( 'NONE',  ( 1.904143259493733309, 1.439083257011425587, -1.304092337848123062 ) ) ;
#92072 = CARTESIAN_POINT ( 'NONE',  ( -5.436456408955534947, 6.405249234278626247, 1.082531754730546636 ) ) ;
#92073 = PRODUCT ( 'air flow regulation', 'air flow regulation', '', ( #151174 ) ) ;
#92074 = EDGE_CURVE ( 'NONE', #158436, #160642, #118853, .T. ) ;
#92075 = CARTESIAN_POINT ( 'NONE',  ( 5.256147377898004791, 0.8573370980917979223, -1.939729252509444279 ) ) ;
#92076 = CARTESIAN_POINT ( 'NONE',  ( 1.224999999999957012, 2.854166666666677621, 0.7072540797572558491 ) ) ;
#92077 = CARTESIAN_POINT ( 'NONE',  ( 3.129529892704606464, 0.4926417352555876872, 1.955172657653013957 ) ) ;
#92078 = CARTESIAN_POINT ( 'NONE',  ( -5.382223794500845315, 6.341977850748185652, -1.082531754730543971 ) ) ;
#92079 = CARTESIAN_POINT ( 'NONE',  ( -7.608060475923978494, 8.905100639113307182, 1.199719254218452047 ) ) ;
#92080 = CARTESIAN_POINT ( 'NONE',  ( 8.048736748007069508, 12.54194330598362406, -0.7998128361456352531 ) ) ;
#92081 = CARTESIAN_POINT ( 'NONE',  ( 1.488595654847742145, -0.2661386877833261111, -1.806066791206423439 ) ) ;
#92082 = CARTESIAN_POINT ( 'NONE',  ( -5.855142236255304944, 7.924361590421551860, -1.599625672291271394 ) ) ;
#92084 = AXIS2_PLACEMENT_3D ( 'NONE', #4737, #70812, #115399 ) ;
#92083 = CARTESIAN_POINT ( 'NONE',  ( -5.602815672633493449, 5.724646472043899870, 0.3052438699321499693 ) ) ;
#92085 = CARTESIAN_POINT ( 'NONE',  ( -4.642607672489913462, 8.343425853053251018, 0.4124909477912245825 ) ) ;
#92086 = VERTEX_POINT ( 'NONE', #134014 ) ;
#92087 = CARTESIAN_POINT ( 'NONE',  ( 5.260643881022500246, -1.494227509126961451, 1.419604852646045634 ) ) ;
#92088 = CARTESIAN_POINT ( 'NONE',  ( -5.411112705185557203, 9.327065566109540740, 0.7216878364870267237 ) ) ;
#92089 = B_SPLINE_CURVE_WITH_KNOTS ( 'NONE', 3,
 ( #15008, #147188, #78957, #160221, #145079, #211082, #48618, #13945, #212144, #63780 ),
 .UNSPECIFIED., .F., .F.,
 ( 4, 3, 3, 4 ),
 ( 0.000000000000000000, 6.251591618973194396E-05, 0.0001688574560067633145, 0.0002758324972496365921 ),
 .UNSPECIFIED. ) ;
#92090 = CARTESIAN_POINT ( 'NONE',  ( 6.658462837642789012, 9.821938173008357253, 1.082531754730549078 ) ) ;
#92091 = CARTESIAN_POINT ( 'NONE',  ( -4.223528545856940042, 4.886203710709899006, -1.199719254218446718 ) ) ;
#92092 = CARTESIAN_POINT ( 'NONE',  ( -5.002032328799064231, 4.800402236545811441, -0.7998128361456362523 ) ) ;
#92093 = CARTESIAN_POINT ( 'NONE',  ( 4.512370939326771691, -2.019285345247460839, -0.04732774261236893931 ) ) ;
#92095 = ORIENTED_EDGE ( 'NONE', *, *, #171975, .T. ) ;
#92094 = CARTESIAN_POINT ( 'NONE',  ( 6.147183147440572704, 0.2149688563512392736, 2.210895739474004529 ) ) ;
#92097 = CARTESIAN_POINT ( 'NONE',  ( 7.944714827928033962, 12.21265836598400689, 0.7216878364870438212 ) ) ;
#92096 = CARTESIAN_POINT ( 'NONE',  ( -5.191846479390389568, 5.021852078902356631, 0.7998128361456281477 ) ) ;
#92098 = CARTESIAN_POINT ( 'NONE',  ( 5.147291874682557555, 9.156924287104992288, 0.7998128361456462443 ) ) ;
#92099 = CARTESIAN_POINT ( 'NONE',  ( 4.311438335051980708, -0.3541389166773502573, 2.030069380940119572 ) ) ;
#92100 = CARTESIAN_POINT ( 'NONE',  ( 2.356092462967720458, 0.09613450340887133572, -2.014232768679749430 ) ) ;
#92101 = ORIENTED_EDGE ( 'NONE', *, *, #199274, .T. ) ;
#92102 = LINE ( 'NONE', #138710, #142181 ) ;
#92103 = CARTESIAN_POINT ( 'NONE',  ( 3.194917754314666514, 6.879154480009089134, 0.7998128361456321445 ) ) ;
#92105 = ORIENTED_EDGE ( 'NONE', *, *, #123715, .F. ) ;
#92104 = CARTESIAN_POINT ( 'NONE',  ( -11.48788097203293823, 9.769569456023079468, 3.469500700354829714 ) ) ;
#92106 = CARTESIAN_POINT ( 'NONE',  ( 5.647444738788365726, 7.344714329438926548, -1.230740020431456028 ) ) ;
#92107 = CARTESIAN_POINT ( 'NONE',  ( 2.583361055862750000, 1.319027862724517552, -1.524809160041600498 ) ) ;
#92108 = CARTESIAN_POINT ( 'NONE',  ( 2.097363409947244683, -1.840767647902554982, 0.04455809990146220728 ) ) ;
#92109 = CARTESIAN_POINT ( 'NONE',  ( 0.7335963760657808752, 0.1754145531542888048, 2.301085101356622697 ) ) ;
#92110 = CARTESIAN_POINT ( 'NONE',  ( 4.923546060418115822, 5.773167154356443120, -1.199719254218452047 ) ) ;
#92111 = CARTESIAN_POINT ( 'NONE',  ( 4.007220386668823409, 1.851715269821294640, 1.114988852100415651 ) ) ;
#92112 = CARTESIAN_POINT ( 'NONE',  ( 7.560643217915098191, 11.97250085420964716, -0.7998128361456291469 ) ) ;
#92113 = CARTESIAN_POINT ( 'NONE',  ( -5.065942953000576843, 9.062017211809330064, -0.7998128361456231517 ) ) ;
#92114 = EDGE_CURVE ( 'NONE', #188684, #150164, #29428, .T. ) ;
#92115 = CARTESIAN_POINT ( 'NONE',  ( 3.040662745855776006, 2.183360198754655812, -0.7182390863737651010 ) ) ;
#92116 = ORIENTED_EDGE ( 'NONE', *, *, #115314, .F. ) ;
#92117 = AXIS2_PLACEMENT_3D ( 'NONE', #149684, #38067, #198407 ) ;
#92118 = DIRECTION ( 'NONE',  ( 1.276756478318932585E-15, -1.000000000000000000, 1.665334536937738262E-16 ) ) ;
#92119 = CARTESIAN_POINT ( 'NONE',  ( 1.569004590881704075, 0.1408476687595125731, -1.865417194689425795 ) ) ;
#92120 = CARTESIAN_POINT ( 'NONE',  ( 5.119980909927547508, -1.054019455064346689, -1.665871061098343819 ) ) ;
#92121 = VECTOR ( 'NONE', #154313, 1000.000000000000114 ) ;
#92123 = CARTESIAN_POINT ( 'NONE',  ( 7.578644679914694926, 11.78557652663510424, 0.7216878364870438212 ) ) ;
#92122 = CARTESIAN_POINT ( 'NONE',  ( -1.364683531250012516, 4.988541667008084879, -0.7879004041258300672 ) ) ;
#92125 = CARTESIAN_POINT ( 'NONE',  ( 0.2939702064862387276, 1.638257335637434364, 1.478849500172851217 ) ) ;
#92124 = CARTESIAN_POINT ( 'NONE',  ( -5.982172092127739482, 8.002286745614243912, -1.599625672291263179 ) ) ;
#92126 = CARTESIAN_POINT ( 'NONE',  ( -2.679285714285713826, 0.4970443252110354759, -0.09999999999999592548 ) ) ;
#92127 = CARTESIAN_POINT ( 'NONE',  ( 6.003563092752934871, 5.898578451166879510, 0.7998128361456341429 ) ) ;
#92128 = CARTESIAN_POINT ( 'NONE',  ( -6.749261541504576911, 6.768559974710451677, 1.040834085586084257E-14 ) ) ;
#92129 = CARTESIAN_POINT ( 'NONE',  ( 4.803572714498323570, -0.5265354887679043472, 1.899778226852407936 ) ) ;
#92130 = CARTESIAN_POINT ( 'NONE',  ( 5.180430901434020186, -1.285682204016626029, 1.916193241175147666 ) ) ;
#92131 = CARTESIAN_POINT ( 'NONE',  ( 6.021894344906984387, 1.833355594513026876, -0.3188260975769128813 ) ) ;
#92132 = CARTESIAN_POINT ( 'NONE',  ( 2.659094170149599368, 1.659314987522000795, -1.224949181800268017 ) ) ;
#92133 = CARTESIAN_POINT ( 'NONE',  ( 6.236387472606139681, 8.298871356172400127, -1.443375672974057666 ) ) ;
#92134 = CARTESIAN_POINT ( 'NONE',  ( 8.154303043976348420, 8.478051404252736845, 0.7998128361456281477 ) ) ;
#92135 = CARTESIAN_POINT ( 'NONE',  ( 7.307481607641395094, 8.588111966078864512, -1.082531754730537976 ) ) ;
#92136 = CARTESIAN_POINT ( 'NONE',  ( -0.6823417656250003738, 1.530208333674752730, -1.181850606188749264 ) ) ;
#92137 = CARTESIAN_POINT ( 'NONE',  ( -4.705920246013195474, 14.55298554035344694, 10.99996989179731877 ) ) ;
#92138 = CARTESIAN_POINT ( 'NONE',  ( 5.300874872818828187, 8.167809204055208383, 1.082531754730558626 ) ) ;
#92139 = CARTESIAN_POINT ( 'NONE',  ( 5.354042097475935513, -0.7863316197885154013, 2.023950393233854061 ) ) ;
#92140 = DIRECTION ( 'NONE',  ( 0.000000000000000000, 0.000000000000000000, 1.000000000000000000 ) ) ;
#92141 =( REPRESENTATION_RELATIONSHIP ('NONE','NONE', #84563, #137092 ) REPRESENTATION_RELATIONSHIP_WITH_TRANSFORMATION ( #125155 )SHAPE_REPRESENTATION_RELATIONSHIP( ) );
#92143 = CARTESIAN_POINT ( 'NONE',  ( 4.194743914777058436, 1.481411246205705412, 1.093257649623424754 ) ) ;
#92142 = CARTESIAN_POINT ( 'NONE',  ( -2.318081078256692518, 5.648252324700675508, 1.040834085586084257E-14 ) ) ;
#92145 = CARTESIAN_POINT ( 'NONE',  ( 6.620655732516649294, 2.985444497229528427, 2.280274006979409407 ) ) ;
#92144 = CARTESIAN_POINT ( 'NONE',  ( 1.364683531249988535, 5.405208333674750953, -0.7879004041258300672 ) ) ;
#92146 = CARTESIAN_POINT ( 'NONE',  ( 6.233935805145816467, 2.167428969419796125, 0.3234103439683775894 ) ) ;
#92147 = CARTESIAN_POINT ( 'NONE',  ( 1.224999999999984768, 0.1875000006827803878, -5.377642775528101993E-14 ) ) ;
#92148 = CARTESIAN_POINT ( 'NONE',  ( 0.8786447689848001508, -1.256089115395578659, 1.881495417452299312 ) ) ;
#92149 = EDGE_CURVE ( 'NONE', #207276, #8852, #68944, .T. ) ;
#92150 = CARTESIAN_POINT ( 'NONE',  ( -4.023696502211203452, 7.783621949832661535, -0.4819376843918365960 ) ) ;
#92151 = DIRECTION ( 'NONE',  ( -0.000000000000000000, -1.000000000000000000, -0.000000000000000000 ) ) ;
#92152 = CARTESIAN_POINT ( 'NONE',  ( 6.592372495380235620, 6.775069446727209233, 0.2122460957004346782 ) ) ;
#92153 = CARTESIAN_POINT ( 'NONE',  ( -3.946832114909637479, 7.618738210787614484, 0.7216878364870338292 ) ) ;
#92154 = CARTESIAN_POINT ( 'NONE',  ( 0.5395309102857149819, -1.815710607404594334, 0.6001554849531522962 ) ) ;
#92155 = CARTESIAN_POINT ( 'NONE',  ( 1.305125929463516909, -0.4348595813401417987, 1.715451362885108466 ) ) ;
#92156 = CARTESIAN_POINT ( 'NONE',  ( 5.707686766122681554, 1.525977179164988540, 1.313104676043591601 ) ) ;
#92157 = CARTESIAN_POINT ( 'NONE',  ( 5.198661835836162481, 8.152523677529138979, 1.199719254218462483 ) ) ;
#92158 = CARTESIAN_POINT ( 'NONE',  ( 4.208114709606614490, -2.100488694582537619, 0.1524824656061254391 ) ) ;
#92159 = CARTESIAN_POINT ( 'NONE',  ( 2.812013442917372430, 1.061847183940438422, -1.594151112820214822 ) ) ;
#92160 = CARTESIAN_POINT ( 'NONE',  ( 4.549612403093820312, 8.500000000000243361, -0.2314049244472246580 ) ) ;
#92162 = EDGE_CURVE ( 'NONE', #177822, #161745, #109054, .T. ) ;
#92161 = CARTESIAN_POINT ( 'NONE',  ( 4.791434771068385778, -1.801603960925775016, 0.7962418042333998525 ) ) ;
#92163 = CARTESIAN_POINT ( 'NONE',  ( 5.642833896779382741, 1.947644361699039983, 0.5348221497712030148 ) ) ;
#92164 = CARTESIAN_POINT ( 'NONE',  ( 3.151090109352538082, -1.528452604574185525, -1.078222621661927061 ) ) ;
#92167 = ORIENTED_EDGE ( 'NONE', *, *, #145312, .T. ) ;
#92166 = CARTESIAN_POINT ( 'NONE',  ( 1.599720133015330337, 1.321132142916726204, 1.382909031182079307 ) ) ;
#92165 = CARTESIAN_POINT ( 'NONE',  ( 4.793404903408416295, 1.281069664470562142, 1.155212482600373125 ) ) ;
#92169 = CARTESIAN_POINT ( 'NONE',  ( 4.690757960648231695, 5.535267711253469614, 1.082531754730560403 ) ) ;
#92168 = CARTESIAN_POINT ( 'NONE',  ( 2.297764732281985633, 1.706874461811638044, 1.398895601573101111 ) ) ;
#92170 = MECHANICAL_DESIGN_GEOMETRIC_PRESENTATION_REPRESENTATION (  '', ( #188910 ), #36763 ) ;
#92171 = CARTESIAN_POINT ( 'NONE',  ( -1.364683531250000748, 2.321875000341422357, 1.214306433183764966E-14 ) ) ;
#92172 = CARTESIAN_POINT ( 'NONE',  ( 6.408651779211167465, 0.6141799454031526828, 1.863335524608072502 ) ) ;
#92173 = CARTESIAN_POINT ( 'NONE',  ( 8.046927864910717432, 9.346836249606042202, 1.199719254218462483 ) ) ;
#92174 = FACE_OUTER_BOUND ( 'NONE', #187669, .T. ) ;
#92175 = CARTESIAN_POINT ( 'NONE',  ( -3.511198596259295535, 6.271927390929313617, -1.000000000000001776 ) ) ;
#92176 = CARTESIAN_POINT ( 'NONE',  ( -0.4500000000000163869, 3.950000000000009059, -1.561251128379126385E-14 ) ) ;
#92177 = CARTESIAN_POINT ( 'NONE',  ( 7.317172109023883486, -6.705807696135622997, 7.317172109023855953 ) ) ;
#92178 = VERTEX_POINT ( 'NONE', #71079 ) ;
#92179 = CARTESIAN_POINT ( 'NONE',  ( 1.803268859043684058, -1.750145871244257467, 1.105767233283899920 ) ) ;
#92180 = CARTESIAN_POINT ( 'NONE',  ( -1.500000000000011324, 3.170833333333354265, 0.8660254037844403729 ) ) ;
#92181 = CARTESIAN_POINT ( 'NONE',  ( 5.636439174979242850, 7.598931675607687453, -1.599625672291262513 ) ) ;
#92182 = CARTESIAN_POINT ( 'NONE',  ( -6.201965203247477909, 9.323044272842313518, 1.199719254218452047 ) ) ;
#92183 = CARTESIAN_POINT ( 'NONE',  ( 4.472210567661338843, 6.310941310395290493, 1.599625672291261402 ) ) ;
#92184 = CARTESIAN_POINT ( 'NONE',  ( 6.639320575229281651, -0.0007625845807879281287, 2.103388539994067497 ) ) ;
#92185 = DIRECTION ( 'NONE',  ( -1.276756478318932585E-15, 1.000000000000000000, -1.665334536937738262E-16 ) ) ;
#92186 = CARTESIAN_POINT ( 'NONE',  ( -1.364683531250012516, 2.488541667008088876, -0.7879004041258289570 ) ) ;
#92187 = ORIENTED_EDGE ( 'NONE', *, *, #131977, .T. ) ;
#92188 =( GEOMETRIC_REPRESENTATION_CONTEXT ( 3 ) GLOBAL_UNCERTAINTY_ASSIGNED_CONTEXT ( ( #122528 ) ) GLOBAL_UNIT_ASSIGNED_CONTEXT ( ( #55190, #121337, #21578 ) ) REPRESENTATION_CONTEXT ( 'NONE', 'WORKASPACE' ) );
#92189 = EDGE_CURVE ( 'NONE', #17090, #93714, #57803, .T. ) ;
#92191 = CARTESIAN_POINT ( 'NONE',  ( 10.08690309888728187, 10.87040115823107911, -0.7216878364870257245 ) ) ;
#92190 = CARTESIAN_POINT ( 'NONE',  ( 0.09999999999999592548, -9.999999999999994671, 9.579478065113978147 ) ) ;
#92192 = CARTESIAN_POINT ( 'NONE',  ( 5.097029748277864591, 1.038832625704217527, -1.727738606215820205 ) ) ;
#92193 = CARTESIAN_POINT ( 'NONE',  ( 4.926915384452605018, -1.639780065798799757, 0.9903009516807855794 ) ) ;
#92194 = FACE_OUTER_BOUND ( 'NONE', #68205, .T. ) ;
#92195 = CARTESIAN_POINT ( 'NONE',  ( 2.191216702865448784, 1.696344223602393786, 1.387594652289561470 ) ) ;
#92196 = CARTESIAN_POINT ( 'NONE',  ( -3.741687207691642314, 6.348756928073427730, 1.082531754730560403 ) ) ;
#92197 = CARTESIAN_POINT ( 'NONE',  ( 1.499999999999989120, 2.035416667349480679, 0.8660254037844524744 ) ) ;
#92198 = CARTESIAN_POINT ( 'NONE',  ( 5.308844932141564499, -0.4931833774270472648, -1.951727149811402828 ) ) ;
#92199 = CARTESIAN_POINT ( 'NONE',  ( 1.634869402278725348, 1.785593253932623803, 0.6852637533772618639 ) ) ;
#92200 = CARTESIAN_POINT ( 'NONE',  ( -4.771579997005698459, 7.654261532226910525, -1.199719254218452047 ) ) ;
#92202 = CARTESIAN_POINT ( 'NONE',  ( 0.4390776481996219727, -1.704952938511293814, -1.076296438737800454 ) ) ;
#92201 = CARTESIAN_POINT ( 'NONE',  ( -3.145128448690323264, 4.692402494937224056, -1.443375672974059665 ) ) ;
#92203 = CARTESIAN_POINT ( 'NONE',  ( -0.6823417656250003738, 10.21354166700806587, 1.181850606188754593 ) ) ;
#92205 = CARTESIAN_POINT ( 'NONE',  ( -4.457598643843001973, 8.422558527783969851, 0.000000000000000000 ) ) ;
#92204 = CARTESIAN_POINT ( 'NONE',  ( 3.755486520148888729, 2.074727465276064997, -0.2578676962887976321 ) ) ;
#92207 = ORIENTED_EDGE ( 'NONE', *, *, #33178, .T. ) ;
#92206 = CARTESIAN_POINT ( 'NONE',  ( 2.010387792931751516, 1.280683741330263858, -1.155484876777863379 ) ) ;
#92208 = CARTESIAN_POINT ( 'NONE',  ( 5.986088515633498197, 6.942523675449257858, -1.199719254218446718 ) ) ;
#92209 = CARTESIAN_POINT ( 'NONE',  ( 0.02680830797223074380, 7.629137130509076492, -2.410890733638766825 ) ) ;
#92210 = CARTESIAN_POINT ( 'NONE',  ( 10.56511880488638333, 13.75886523581518439, -3.405056808716383276 ) ) ;
#92211 = CARTESIAN_POINT ( 'NONE',  ( -5.761852096127856981, 5.824508321678349532, 0.000000000000000000 ) ) ;
#92212 = CARTESIAN_POINT ( 'NONE',  ( 5.087333953625774008, 6.958308917361963886, 1.599625672291267398 ) ) ;
#92213 = CARTESIAN_POINT ( 'NONE',  ( 0.000000000000000000, -3.600000000000005862, 0.000000000000000000 ) ) ;
#92214 = VERTEX_POINT ( 'NONE', #151304 ) ;
#92215 = CARTESIAN_POINT ( 'NONE',  ( 2.912559398657811549, -0.5280806737378342941, -1.732764662445994919 ) ) ;
#92216 = ORIENTED_EDGE ( 'NONE', *, *, #183234, .T. ) ;
#92217 = CARTESIAN_POINT ( 'NONE',  ( 4.379447312414087357, 5.068108938359919158, -1.199719254218452047 ) ) ;
#92218 = CARTESIAN_POINT ( 'NONE',  ( 3.888156192069020634, 7.758209000714329839, 1.040834085586084257E-14 ) ) ;
#92219 = CARTESIAN_POINT ( 'NONE',  ( 3.914574264990647201, -0.5719694332564858597, -1.718857104472475861 ) ) ;
#92220 = CARTESIAN_POINT ( 'NONE',  ( -4.816538118508267630, 5.092449105792602460, -0.9495590845017554127 ) ) ;
#92221 = CARTESIAN_POINT ( 'NONE',  ( 5.790052644182137165, 6.039355072771209088, 0.5314338945540015846 ) ) ;
#92222 = ORIENTED_EDGE ( 'NONE', *, *, #41993, .F. ) ;
#92223 = CARTESIAN_POINT ( 'NONE',  ( 3.719077791506773423, -1.640430839875358204, -0.8789487387581331745 ) ) ;
#92224 = CARTESIAN_POINT ( 'NONE',  ( 1.722145930190256191, 1.895023070986867619, 0.2790570245742740041 ) ) ;
#92225 = CARTESIAN_POINT ( 'NONE',  ( 0.5514207423844892375, 0.5776932562693118944, -1.731835939664846613 ) ) ;
#92226 = CARTESIAN_POINT ( 'NONE',  ( 4.688369027973070757, 8.258219454933637849, 0.5882785783308928096 ) ) ;
#92227 = SPHERICAL_SURFACE ( 'NONE', #112618, 0.08000000000000000167 ) ;
#92228 = CARTESIAN_POINT ( 'NONE',  ( 4.909045613421183063, 8.010784895652180992, 0.9812996480243344477 ) ) ;
#92229 = CARTESIAN_POINT ( 'NONE',  ( -11.55950211276791428, 9.719999999999982876, 3.221476510067112109 ) ) ;
#92230 = CARTESIAN_POINT ( 'NONE',  ( -11.48243876534946217, 9.719999999999982876, 3.199999999999997957 ) ) ;
#92231 = CARTESIAN_POINT ( 'NONE',  ( 0.000000000000000000, 0.2000000000000057288, 0.000000000000000000 ) ) ;
#92232 = CARTESIAN_POINT ( 'NONE',  ( 5.829642864196151741, 9.745074408296771296, 0.7216878364870438212 ) ) ;
#92233 = CARTESIAN_POINT ( 'NONE',  ( 5.242998352400915607, -0.2370019515391492138, -1.955029394545240162 ) ) ;
#92234 = ADVANCED_FACE ( 'NONE', ( #186984 ), #132938, .F. ) ;
#92235 = CARTESIAN_POINT ( 'NONE',  ( -5.253948220495577637, 6.088359997788290734, 1.199719254218450271 ) ) ;
#92236 = CARTESIAN_POINT ( 'NONE',  ( 11.78331023100045627, 9.719999999999998863, -1.800000000000001155 ) ) ;
#92237 = CARTESIAN_POINT ( 'NONE',  ( 6.474583112218436298, -0.1034247314782872212, -2.189140632845664403 ) ) ;
#92238 = CARTESIAN_POINT ( 'NONE',  ( 6.934105498385400246, 10.17720795050327354, -1.199719254218441611 ) ) ;
#92239 = CARTESIAN_POINT ( 'NONE',  ( 5.930678043039342207, 1.856691256794128053, 0.5132231078649931444 ) ) ;
#92240 = CARTESIAN_POINT ( 'NONE',  ( -5.850506979496850057, 6.784345216623154151, -1.199719254218446718 ) ) ;
#92241 = EDGE_CURVE ( 'NONE', #118348, #49028, #188443, .T. ) ;
#92242 = CARTESIAN_POINT ( 'NONE',  ( 1.096400207583309028, -0.4391605778215034173, -1.771851442210800709 ) ) ;
#92243 = CARTESIAN_POINT ( 'NONE',  ( 1.700138637298425737, -0.7412910010123252569, 2.078789392164873906 ) ) ;
#92244 = CARTESIAN_POINT ( 'NONE',  ( 1.499999999999993117, 10.35416666666666430, 0.8660254037844408170 ) ) ;
#92245 = CARTESIAN_POINT ( 'NONE',  ( 1.406358598101828283, -1.903450966454448334, -0.1843715739238485363 ) ) ;
#92246 = ORIENTED_EDGE ( 'NONE', *, *, #37148, .T. ) ;
#92247 = CARTESIAN_POINT ( 'NONE',  ( 6.983263157960363010, -0.003310164959547181717, 1.953544951557646403 ) ) ;
#92248 = CARTESIAN_POINT ( 'NONE',  ( 2.806119653986011819, 1.404935138194723265, -1.341025529631818980 ) ) ;
#92249 = VECTOR ( 'NONE', #194192, 1000.000000000000000 ) ;
#92250 = VERTEX_POINT ( 'NONE', #89519 ) ;
#92251 = CARTESIAN_POINT ( 'NONE',  ( 0.7903884775103054983, -1.915307795730588181, 0.6297756287277083143 ) ) ;
#92253 = CARTESIAN_POINT ( 'NONE',  ( 6.614093472281312280, 1.855988364702824800, -0.1360997465041282051 ) ) ;
#92252 = CARTESIAN_POINT ( 'NONE',  ( -4.294900800479008574, 8.232744377192641849, 0.000000000000000000 ) ) ;
#92254 = CARTESIAN_POINT ( 'NONE',  ( 5.086243903782109221, 5.962981304947771122, -1.199719254218452047 ) ) ;
#92255 = CARTESIAN_POINT ( 'NONE',  ( -1.016884229002468915E-14, -9.671843677217918156, -9.585733692702609332 ) ) ;
#92256 = CARTESIAN_POINT ( 'NONE',  ( 4.048135823549415591, 3.984990093095080788, -0.7783338591275772433 ) ) ;
#92257 = CARTESIAN_POINT ( 'NONE',  ( -4.391951695823077984, 7.211361847513815704, 1.199719254218464037 ) ) ;
#92258 = CARTESIAN_POINT ( 'NONE',  ( -4.599959256786493533, 8.588645909551377855, 0.000000000000000000 ) ) ;
#92259 = CARTESIAN_POINT ( 'NONE',  ( 2.560326853991791829, -1.509077608345666066, 1.589458984681046516 ) ) ;
#92260 = CARTESIAN_POINT ( 'NONE',  ( 4.365362273920250225, 5.155639410070820716, 1.082531754730560403 ) ) ;
#92261 = CARTESIAN_POINT ( 'NONE',  ( 8.174640274396848483, 8.501778173076651512, 0.7998128361456291469 ) ) ;
#92263 =( BOUNDED_CURVE ( )  B_SPLINE_CURVE ( 2, ( #169719, #5052, #71128, #54912, #187029, #38663, #135112 ),
 .UNSPECIFIED., .F., .T. ) 
 B_SPLINE_CURVE_WITH_KNOTS ( ( 3, 2, 2, 3 ),
 ( 0.4250000000000004885, 0.4333333333333335147, 0.4416666666666664853, 0.4499999999999995115 ),
 .UNSPECIFIED. ) 
 CURVE ( )  GEOMETRIC_REPRESENTATION_ITEM ( )  RATIONAL_B_SPLINE_CURVE ( ( 0.9999999999999920064, 0.8660254037844467012, 1.000000000000000000, 0.8660254037844387076, 1.000000000000000000, 0.8660254037844467012, 0.9999999999999920064 ) ) 
 REPRESENTATION_ITEM ( '' )  );
#92262 = CARTESIAN_POINT ( 'NONE',  ( 0.000000000000000000, 5.999999999999998224, 0.000000000000000000 ) ) ;
#92264 = CARTESIAN_POINT ( 'NONE',  ( 2.631258204695927194, -1.703542010001803275, 0.6570300758180421807 ) ) ;
#92265 = FACE_OUTER_BOUND ( 'NONE', #138024, .T. ) ;
#92266 = CARTESIAN_POINT ( 'NONE',  ( -3.684065054611367351, 5.321161868511784299, -1.599625672291256295 ) ) ;
#92267 = CARTESIAN_POINT ( 'NONE',  ( -5.780704523637806069, 7.347994962087573079, -1.310296981949153006 ) ) ;
#92268 = FACE_OUTER_BOUND ( 'NONE', #84069, .T. ) ;
#92269 = CARTESIAN_POINT ( 'NONE',  ( 8.646349277213076334, 11.11049346154719508, 1.599625672291281386 ) ) ;
#92270 = CARTESIAN_POINT ( 'NONE',  ( 1.137189532436083672, -1.741952243817600721, 0.8230948124841385161 ) ) ;
#92271 = CARTESIAN_POINT ( 'NONE',  ( 5.295737746731337126, -1.384591195607473235, -1.390005841682784959 ) ) ;
#92272 = CARTESIAN_POINT ( 'NONE',  ( -1.500000000000001110, 15.27083333333333570, 0.8660254037844419273 ) ) ;
#92273 = CARTESIAN_POINT ( 'NONE',  ( -6.340409392685171674, 10.54889472477470846, 0.7998128361456481317 ) ) ;
#92274 = CARTESIAN_POINT ( 'NONE',  ( 3.960953433486789521, 7.772862772376584850, -0.7998128361456221525 ) ) ;
#92275 = CARTESIAN_POINT ( 'NONE',  ( 5.214472588068230330, 2.024700573814151028, 0.8392323156421463981 ) ) ;
#92276 = AXIS2_PLACEMENT_3D ( 'NONE', #26760, #7290, #190318 ) ;
#92277 = VECTOR ( 'NONE', #156944, 1000.000000000000000 ) ;
#92278 = CARTESIAN_POINT ( 'NONE',  ( 4.062132091735995765, 3.841501649887839598, -0.4581612399152183990 ) ) ;
#92279 = CARTESIAN_POINT ( 'NONE',  ( 5.700075226665620498, 0.8442301939139056355, -1.890501578402821847 ) ) ;
#92281 = CARTESIAN_POINT ( 'NONE',  ( -1.201851678989727383E-14, 3.259375000341420581, -1.575800808251660134 ) ) ;
#92280 = CARTESIAN_POINT ( 'NONE',  ( 1.347439764754987941E-16, 1.551257596039481879, 2.000000000000000000 ) ) ;
#92282 = ORIENTED_EDGE ( 'NONE', *, *, #155989, .T. ) ;
#92283 = CARTESIAN_POINT ( 'NONE',  ( 5.537770794106480210, -1.814135573521371780, 1.411581493584870728 ) ) ;
#92284 = CARTESIAN_POINT ( 'NONE',  ( 6.534666852106798096, 7.686494751288491578, -1.082531754730543083 ) ) ;
#92286 = DIRECTION ( 'NONE',  ( 0.6507913734559658270, 0.7592566023652989049, 0.000000000000000000 ) ) ;
#92285 = CARTESIAN_POINT ( 'NONE',  ( 4.407809338218622308, 8.156544971314787063, 0.000000000000000000 ) ) ;
#92287 = CARTESIAN_POINT ( 'NONE',  ( 0.6391472400242370622, -1.963128197947199727, 1.183262795983427207 ) ) ;
#92288 = CARTESIAN_POINT ( 'NONE',  ( -7.786489011996894583, -5.767087321558959978, -7.770158002575229261 ) ) ;
#92289 = CARTESIAN_POINT ( 'NONE',  ( -5.101610940492132151, 9.173906207207963348, -0.7998128361456362523 ) ) ;
#92290 = CARTESIAN_POINT ( 'NONE',  ( 5.208904604407663008, -0.2832176519766657630, 1.921071368630644649 ) ) ;
#92291 = ORIENTED_EDGE ( 'NONE', *, *, #213238, .T. ) ;
#92292 = CARTESIAN_POINT ( 'NONE',  ( 10.18181017373857600, 10.98112607889092907, 0.7216878364870438212 ) ) ;
#92293 = ORIENTED_EDGE ( 'NONE', *, *, #156185, .F. ) ;
#92294 = CARTESIAN_POINT ( 'NONE',  ( 5.062724140118719518, 0.5608846916410530348, 1.828269531156314853 ) ) ;
#92295 = CARTESIAN_POINT ( 'NONE',  ( 6.422847680425099348, 1.611446996373969265, 0.6153535913232581755 ) ) ;
#92296 = CARTESIAN_POINT ( 'NONE',  ( 5.366422816783521732, -1.968444216653497003, -0.4370823996120917765 ) ) ;
#92298 = CARTESIAN_POINT ( 'NONE',  ( -3.363831509966363598, 5.978201624052440266, -1.082531754730548412 ) ) ;
#92297 = CARTESIAN_POINT ( 'NONE',  ( -8.992082194361570302, 11.51384853155376220, 1.599625672291269396 ) ) ;
#92299 = CARTESIAN_POINT ( 'NONE',  ( -3.285556943750000070, -2.296874999522042327, 0.000000000000000000 ) ) ;
#92301 = CARTESIAN_POINT ( 'NONE',  ( 0.2503970875498504056, -1.425519035090598852, 1.048718885610238294 ) ) ;
#92300 = CARTESIAN_POINT ( 'NONE',  ( 1.974669457019386787, -0.1036536715517746843, -2.088194013563466012 ) ) ;
#92302 = CARTESIAN_POINT ( 'NONE',  ( 6.276017556857773627, 1.753032240926259311, -0.9962986157117934560 ) ) ;
#92304 = CARTESIAN_POINT ( 'NONE',  ( 3.082263327019618249, -2.258438545724365643, -0.3914850642001906356 ) ) ;
#92303 = CARTESIAN_POINT ( 'NONE',  ( 4.224247379109608680, 7.085983154673295203, -1.199719254218452047 ) ) ;
#92305 = CARTESIAN_POINT ( 'NONE',  ( 1.780815255366276162, 1.198741944763829004, 1.261882163386177869 ) ) ;
#92306 = CARTESIAN_POINT ( 'NONE',  ( 3.217144136595586179, 1.669276650691432495, -1.307696563879121365 ) ) ;
#92307 = CARTESIAN_POINT ( 'NONE',  ( -4.902626719552124257, 4.881029176893854959, -0.5815614086314065956 ) ) ;
#92308 = CARTESIAN_POINT ( 'NONE',  ( 1.967715241700284556, 1.438441333088829266, 0.9676545092154006378 ) ) ;
#92309 = CARTESIAN_POINT ( 'NONE',  ( 1.360316468749964480, 2.046875000341397133, -4.857225732735059864E-14 ) ) ;
#92310 = CARTESIAN_POINT ( 'NONE',  ( 6.350795928397162449, -1.845624747684541989, -0.8128223418941012968 ) ) ;
#92311 = CARTESIAN_POINT ( 'NONE',  ( 1.662329954472214322, -0.6657413170317361129, -1.738099805993092106 ) ) ;
#92312 = CARTESIAN_POINT ( 'NONE',  ( 2.981114689849233113, 2.043561189653697152, 0.7337040362941152916 ) ) ;
#92313 = CARTESIAN_POINT ( 'NONE',  ( 3.643767777461913493, 2.000731686840724333, -0.2516315899964287617 ) ) ;
#92315 = COLOUR_RGB ( '', 0.40784314, 0.44705882, 0.49803922) ;
#92314 = CARTESIAN_POINT ( 'NONE',  ( 5.312500000000002665, 1.451031289061327501, 1.451031289060900065 ) ) ;
#92316 =( BOUNDED_SURFACE ( )  B_SPLINE_SURFACE ( 1, 2, ( 
 ( #142595, #143676, #77553, #91708, #92771, #211807, #46150, #178277, #157759, #13616, #124270, #208604, #190228, #107998, #9356, #75430, #207549, #60235, #182498, #115454, #101258, #50388, #196644, #35181, #64508, #181444, #17855, #150030, #116509, #195584, #179342, #83940, #48283, #1600, #131688, #130652, #81821, #99151, #165202, #65542, #16794, #197690, #51460, #98098, #114396, #34129, #67660, #180392, #133805, #32015, #146855, #97039, #164149, #80766, #212875, #33073, #167341, #15735, #132738, #117582, #147903, #213920, #49336, #63445, #47219, #82877, #148955, #525, #113335, #85013, #66594, #198741, #100199, #166265, #183575, #199816, #18927, #30964, #151103, #129597, #163091, #14672, #119714, #4787, #105560, #69801, #168402, #155351, #201927, #169463, #200869, #52513, #37328, #122952, #73017, #2667, #204061, #185696, #87145, #152158, #19998, #102328, #3728, #106655, #86082, #55713, #6936, #138047, #22108, #90365, #68740, #120796, #135909, #38399, #21048, #88220, #186773, #184632, #53581, #24259, #71937, #154290, #118647, #5865, #188912, #103402, #39464, #89302, #36248, #104479, #134862, #153217, #121866, #54647, #40551, #187837, #70865, #172682, #136980, #170525, #171593, #139114, #23187, #203007, #205142, #56784, #141286, #176942, #9100, #193181, #92521, #28557, #174831, #91443, #209407, #158560, #208352, #93580, #156432, #107743, #10158, #44830, #26410, #173767, #175889, #157504, #144484, #94646, #76234, #74108, #127213, #58919, #124010, #59983, #125078, #142343, #110936, #75176, #25344, #160690, #207295, #108808, #140201, #206223, #191034, #62126, #12283, #8017, #143413, #42701, #126136, #192098, #43764, #41629, #109877, #45892, #27480, #61054, #78364, #77301, #159625, #29631, #57849, #11219, #210491, #128287, #194249, #112013, #178014, #189977, #14415, #117330, #164949, #115201, #145553, #32821, #67414, #64260, #132494, #182252, #79436, #65291, #161770, #162837, #278, #147651, #133555, #82623, #80504, #199564, #96787, #213667, #50139, #33876, #148708, #13362, #211552, #116261, #146601, #99954, #212619, #198494, #31769, #166019, #114150, #30704, #66350, #97839, #131438, #98896, #95717, #46960, #163904, #17605, #15480, #130405, #180143, #197442, #49083, #81565, #181194, #16542, #83689, #196393, #48036, #149777, #1353, #51208, #183328, #63185, #179082, #129350, #195329, #113078, #184385, #152970, #72772, #19753, #104229, #89055, #85834, #53332, #36004, #34934, #18684, #103154, #102085, #168154, #84766, #56540, #151912, #201687, #150852, #2416, #69554, #155112, #105307, #101006, #21860, #3485, #119465, #135664, #52272, #134620, #185453, #138871, #200623, #87968, #39216, #170275, #54408, #122702, #167095, #4544, #118399, #70617, #37075, #120548, #136731, #68493, #169215, #20806, #154042, #186526, #86903, #38156, #6696, #202755, #71690, #121622, #5607, #137803, #203822, #55466, #187591, #171345, #204889 ),
 ( #22939, #205973, #123765, #60800, #41379, #126958, #107489, #91189, #190784, #142089, #9910, #92272, #73852, #175638, #57605, #25089, #158319, #58670, #192918, #143166, #124819, #208104, #75985, #59732, #125890, #209161, #189726, #191849, #43511, #173515, #42447, #157250, #109632, #108551, #8843, #174582, #27224, #93329, #159365, #10965, #26158, #44574, #188665, #77039, #40295, #74921, #106406, #141033, #207040, #172429, #24017, #90119, #156186, #7763, #139947, #153674, #41003, #22575, #3111, #205600, #123398, #39927, #36700, #104935, #189362, #170976, #5242, #57238, #69182, #139573, #135303, #201316, #88681, #138497, #188287, #87604, #167782, #19378, #71318, #55103, #119094, #121252, #4180, #20446, #106036, #21493, #172058, #137431, #6323, #85458, #203449, #151544, #154740, #52956, #185074, #102785, #23652, #168843, #72397, #86528, #204519, #187223, #152594, #70251, #136364, #202384, #54034, #120171, #56166, #38851, #186148, #122330, #37782, #89760, #155809, #7393, #103856, #169906, #73472, #94028, #110321, #44200, #43149, #90820, #76676, #74556, #91898, #108188, #142790, #29004, #176327, #42075, #24718, #25787, #190417, #27934, #140657, #207739, #78800, #173136, #161139, #160066, #144924, #194691, #11670, #12727, #77744, #143865, #107113, #156883, #109262, #8470, #60426, #209858, #208796, #141731, #177390, #62556, #206671, #126586, #59364, #191481, #174214, #61496, #157954, #9546, #210930, #75622, #128720, #125520, #175270, #10599, #127663, #193625, #192547, #124458, #45267, #26855, #92960, #111388, #159006, #58303, #95091, #32196, #99338, #49510, #181625, #197880, #84138, #113519, #16982, #83061, #14855, #98272, #179528, #149137, #164330, #213059, #15920, #719, #196826, #30070, #82003, #13797, #31147, #47407, #148091, #182695, #115630, #195768, #178461, #97221, #129787, #33254, #79871, #147037, #18052, #112448, #100390, #165387, #150226, #134001, #66783, #166460, #132923, #198928, #46333, #96160, #48468, #162212, #214096, #50574, #65723, #80945, #116696, #1796, #145981, #131871, #64689, #130834, #163274, #34314, #114583, #180574, #67853, #211992, #63633, #36450, #152345, #103598, #186965, #203201, #71061, #2859, #72137, #135049, #86275, #137177, #185889, #155555, #105769, #37523, #38597, #54848, #120998, #104675, #23389, #52704, #170723, #22309, #168587, #169656, #118834, #88422, #21241, #3923, #87348, #154488, #6067, #138245, #204259, #119913, #89500, #7135, #153414, #4985, #151288, #55910, #102525, #184820, #122068, #53780, #188031, #39661, #171795, #73207, #200007, #51657, #117779, #35381, #183771, #101455, #167527, #68929, #19125, #85204, #201062, #20187, #69993, #136105, #202120, #189111, #106850, #190169, #192287, #59104, #12478, #126328, #41823, #10343, #92702, #207485, #24453, #107936, #75365, #43947, #142527, #76417, #110063, #173961, #9292, #74302, #156628, #90567, #140398, #28748, #8217 ) ),
 .UNSPECIFIED., .F., .F., .T. ) 
 B_SPLINE_SURFACE_WITH_KNOTS ( ( 2, 2 ),
 ( 3, 2, 2, 2, 2, 2, 2, 2, 2, 2, 2, 2, 2, 2, 2, 2, 2, 2, 2, 2, 2, 2, 2, 2, 2, 2, 2, 2, 2, 2, 2, 2, 2, 2, 2, 2, 2, 2, 2, 2, 2, 2, 2, 2, 2, 2, 2, 2, 2, 2, 2, 2, 2, 2, 2, 2, 2, 2, 2, 2, 2, 2, 2, 2, 2, 2, 2, 2, 2, 2, 2, 2, 2, 2, 2, 2, 2, 2, 2, 2, 2, 2, 2, 2, 2, 2, 2, 2, 2, 2, 2, 2, 2, 2, 2, 2, 2, 2, 2, 2, 2, 2, 2, 2, 2, 2, 2, 2, 2, 2, 2, 2, 2, 2, 2, 2, 2, 2, 2, 2, 2, 2, 2, 2, 2, 2, 2, 2, 2, 2, 2, 2, 2, 2, 2, 2, 2, 2, 2, 2, 2, 2, 2, 2, 2, 2, 2, 2, 2, 2, 2, 2, 2, 2, 2, 2, 2, 2, 2, 2, 2, 2, 2, 2, 2, 2, 2, 2, 3 ),
 ( 0.000000000000000000, 1.000000000000000000 ),
 ( 0.000000000000000000, 0.005952380952380952051, 0.01190476190476190410, 0.01785714285714285615, 0.02380952380952380820, 0.02976190476190476025, 0.03571428571428571230, 0.04166666666666666435, 0.04761904761904761640, 0.05357142857142856845, 0.05952380952380952051, 0.06547619047619047949, 0.07142857142857142461, 0.07738095238095238360, 0.08333333333333332871, 0.08928571428571428770, 0.09523809523809523281, 0.1011904761904761918, 0.1071428571428571369, 0.1130952380952380959, 0.1190476190476190410, 0.1250000000000000000, 0.1309523809523809590, 0.1369047619047619180, 0.1428571428571428492, 0.1488095238095238082, 0.1547619047619047672, 0.1607142857142857262, 0.1666666666666666574, 0.1726190476190476164, 0.1785714285714285754, 0.1845238095238095344, 0.1904761904761904656, 0.1964285714285714246, 0.2023809523809523836, 0.2083333333333333426, 0.2142857142857142738, 0.2202380952380952328, 0.2261904761904761918, 0.2321428571428571508, 0.2380952380952380820, 0.2440476190476190410, 0.2500000000000000000, 0.2559523809523809312, 0.2619047619047619180, 0.2678571428571428492, 0.2738095238095238360, 0.2797619047619047672, 0.2857142857142856984, 0.2916666666666666852, 0.2976190476190476164, 0.3035714285714285476, 0.3095238095238095344, 0.3154761904761904656, 0.3214285714285714524, 0.3273809523809523836, 0.3333333333333333148, 0.3392857142857143016, 0.3452380952380952328, 0.3511904761904761640, 0.3571428571428571508, 0.3630952380952380820, 0.3690476190476190688, 0.3750000000000000000, 0.3809523809523809312, 0.3869047619047619180, 0.3928571428571428492, 0.3988095238095238360, 0.4047619047619047672, 0.4107142857142856984, 0.4166666666666666852, 0.4226190476190476164, 0.4285714285714285476, 0.4345238095238095344, 0.4404761904761904656, 0.4464285714285714524, 0.4523809523809523836, 0.4583333333333333148, 0.4642857142857143016, 0.4702380952380952328, 0.4761904761904761640, 0.4821428571428571508, 0.4880952380952380820, 0.4940476190476190688, 0.5000000000000000000, 0.5059523809523809312, 0.5119047619047618625, 0.5178571428571429047, 0.5238095238095238360, 0.5297619047619047672, 0.5357142857142856984, 0.5416666666666666297, 0.5476190476190476719, 0.5535714285714286031, 0.5595238095238095344, 0.5654761904761904656, 0.5714285714285713969, 0.5773809523809523281, 0.5833333333333333703, 0.5892857142857143016, 0.5952380952380952328, 0.6011904761904761640, 0.6071428571428570953, 0.6130952380952381375, 0.6190476190476190688, 0.6250000000000000000, 0.6309523809523809312, 0.6369047619047618625, 0.6428571428571429047, 0.6488095238095238360, 0.6547619047619047672, 0.6607142857142856984, 0.6666666666666666297, 0.6726190476190476719, 0.6785714285714286031, 0.6845238095238095344, 0.6904761904761904656, 0.6964285714285713969, 0.7023809523809523281, 0.7083333333333333703, 0.7142857142857143016, 0.7202380952380952328, 0.7261904761904761640, 0.7321428571428570953, 0.7380952380952381375, 0.7440476190476190688, 0.7500000000000000000, 0.7559523809523809312, 0.7619047619047618625, 0.7678571428571429047, 0.7738095238095238360, 0.7797619047619047672, 0.7857142857142856984, 0.7916666666666666297, 0.7976190476190476719, 0.8035714285714286031, 0.8095238095238095344, 0.8154761904761904656, 0.8214285714285713969, 0.8273809523809523281, 0.8333333333333333703, 0.8392857142857143016, 0.8452380952380952328, 0.8511904761904761640, 0.8571428571428570953, 0.8630952380952381375, 0.8690476190476190688, 0.8750000000000000000, 0.8809523809523809312, 0.8869047619047618625, 0.8928571428571429047, 0.8988095238095238360, 0.9047619047619047672, 0.9107142857142856984, 0.9166666666666666297, 0.9226190476190476719, 0.9285714285714286031, 0.9345238095238095344, 0.9404761904761904656, 0.9464285714285713969, 0.9523809523809523281, 0.9583333333333333703, 0.9642857142857143016, 0.9702380952380952328, 0.9761904761904761640, 0.9821428571428570953, 0.9880952380952381375, 0.9940476190476190688, 1.000000000000000000 ),
 .UNSPECIFIED. ) 
 GEOMETRIC_REPRESENTATION_ITEM ( )  RATIONAL_B_SPLINE_SURFACE ( (
 ( 1.000000000000000000, 0.8660254037844387076, 1.000000000000000000, 0.8660254037844387076, 1.000000000000000000, 0.8660254037844387076, 1.000000000000000000, 0.8660254037844387076, 1.000000000000000000, 0.8660254037844387076, 1.000000000000000000, 0.8660254037844387076, 1.000000000000000000, 0.8660254037844387076, 1.000000000000000000, 0.8660254037844387076, 1.000000000000000000, 0.8660254037844387076, 1.000000000000000000, 0.8660254037844387076, 1.000000000000000000, 0.8660254037844387076, 1.000000000000000000, 0.8660254037844387076, 1.000000000000000000, 0.8660254037844387076, 1.000000000000000000, 0.8660254037844387076, 1.000000000000000000, 0.8660254037844387076, 1.000000000000000000, 0.8660254037844387076, 1.000000000000000000, 0.8660254037844387076, 1.000000000000000000, 0.8660254037844387076, 1.000000000000000000, 0.8660254037844387076, 1.000000000000000000, 0.8660254037844387076, 1.000000000000000000, 0.8660254037844387076, 1.000000000000000000, 0.8660254037844387076, 1.000000000000000000, 0.8660254037844387076, 1.000000000000000000, 0.8660254037844387076, 1.000000000000000000, 0.8660254037844387076, 1.000000000000000000, 0.8660254037844387076, 1.000000000000000000, 0.8660254037844387076, 1.000000000000000000, 0.8660254037844387076, 1.000000000000000000, 0.8660254037844387076, 1.000000000000000000, 0.8660254037844387076, 1.000000000000000000, 0.8660254037844387076, 1.000000000000000000, 0.8660254037844387076, 1.000000000000000000, 0.8660254037844387076, 1.000000000000000000, 0.8660254037844387076, 1.000000000000000000, 0.8660254037844387076, 1.000000000000000000, 0.8660254037844387076, 1.000000000000000000, 0.8660254037844387076, 1.000000000000000000, 0.8660254037844387076, 1.000000000000000000, 0.8660254037844387076, 1.000000000000000000, 0.8660254037844387076, 1.000000000000000000, 0.8660254037844387076, 1.000000000000000000, 0.8660254037844387076, 1.000000000000000000, 0.8660254037844387076, 1.000000000000000000, 0.8660254037844387076, 1.000000000000000000, 0.8660254037844387076, 1.000000000000000000, 0.8660254037844387076, 1.000000000000000000, 0.8660254037844387076, 1.000000000000000000, 0.8660254037844387076, 1.000000000000000000, 0.8660254037844387076, 1.000000000000000000, 0.8660254037844387076, 1.000000000000000000, 0.8660254037844387076, 1.000000000000000000, 0.8660254037844387076, 1.000000000000000000, 0.8660254037844387076, 1.000000000000000000, 0.8660254037844387076, 1.000000000000000000, 0.8660254037844387076, 1.000000000000000000, 0.8660254037844387076, 1.000000000000000000, 0.8660254037844387076, 1.000000000000000000, 0.8660254037844387076, 1.000000000000000000, 0.8660254037844387076, 1.000000000000000000, 0.8660254037844387076, 1.000000000000000000, 0.8660254037844387076, 1.000000000000000000, 0.8660254037844387076, 1.000000000000000000, 0.8660254037844387076, 1.000000000000000000, 0.8660254037844387076, 1.000000000000000000, 0.8660254037844387076, 1.000000000000000000, 0.8660254037844387076, 1.000000000000000000, 0.8660254037844387076, 1.000000000000000000, 0.8660254037844387076, 1.000000000000000000, 0.8660254037844387076, 1.000000000000000000, 0.8660254037844387076, 1.000000000000000000, 0.8660254037844387076, 1.000000000000000000, 0.8660254037844387076, 1.000000000000000000, 0.8660254037844387076, 1.000000000000000000, 0.8660254037844387076, 1.000000000000000000, 0.8660254037844387076, 1.000000000000000000, 0.8660254037844387076, 1.000000000000000000, 0.8660254037844387076, 1.000000000000000000, 0.8660254037844387076, 1.000000000000000000, 0.8660254037844387076, 1.000000000000000000, 0.8660254037844387076, 1.000000000000000000, 0.8660254037844387076, 1.000000000000000000, 0.8660254037844387076, 1.000000000000000000, 0.8660254037844387076, 1.000000000000000000, 0.8660254037844387076, 1.000000000000000000, 0.8660254037844387076, 1.000000000000000000, 0.8660254037844387076, 1.000000000000000000, 0.8660254037844387076, 1.000000000000000000, 0.8660254037844387076, 1.000000000000000000, 0.8660254037844387076, 1.000000000000000000, 0.8660254037844387076, 1.000000000000000000, 0.8660254037844387076, 1.000000000000000000, 0.8660254037844387076, 1.000000000000000000, 0.8660254037844387076, 1.000000000000000000, 0.8660254037844387076, 1.000000000000000000, 0.8660254037844387076, 1.000000000000000000, 0.8660254037844387076, 1.000000000000000000, 0.8660254037844387076, 1.000000000000000000, 0.8660254037844387076, 1.000000000000000000, 0.8660254037844387076, 1.000000000000000000, 0.8660254037844387076, 1.000000000000000000, 0.8660254037844387076, 1.000000000000000000, 0.8660254037844387076, 1.000000000000000000, 0.8660254037844387076, 1.000000000000000000, 0.8660254037844387076, 1.000000000000000000, 0.8660254037844387076, 1.000000000000000000, 0.8660254037844387076, 1.000000000000000000, 0.8660254037844387076, 1.000000000000000000, 0.8660254037844387076, 1.000000000000000000, 0.8660254037844387076, 1.000000000000000000, 0.8660254037844387076, 1.000000000000000000, 0.8660254037844387076, 1.000000000000000000, 0.8660254037844387076, 1.000000000000000000, 0.8660254037844387076, 1.000000000000000000, 0.8660254037844387076, 1.000000000000000000, 0.8660254037844387076, 1.000000000000000000, 0.8660254037844387076, 1.000000000000000000, 0.8660254037844387076, 1.000000000000000000, 0.8660254037844387076, 1.000000000000000000, 0.8660254037844387076, 1.000000000000000000, 0.8660254037844387076, 1.000000000000000000, 0.8660254037844387076, 1.000000000000000000, 0.8660254037844387076, 1.000000000000000000, 0.8660254037844387076, 1.000000000000000000, 0.8660254037844387076, 1.000000000000000000, 0.8660254037844387076, 1.000000000000000000, 0.8660254037844387076, 1.000000000000000000, 0.8660254037844387076, 1.000000000000000000, 0.8660254037844387076, 1.000000000000000000, 0.8660254037844387076, 1.000000000000000000, 0.8660254037844387076, 1.000000000000000000, 0.8660254037844387076, 1.000000000000000000, 0.8660254037844387076, 1.000000000000000000, 0.8660254037844387076, 1.000000000000000000, 0.8660254037844387076, 1.000000000000000000, 0.8660254037844387076, 1.000000000000000000, 0.8660254037844387076, 1.000000000000000000, 0.8660254037844387076, 1.000000000000000000, 0.8660254037844387076, 1.000000000000000000, 0.8660254037844387076, 1.000000000000000000, 0.8660254037844387076, 1.000000000000000000, 0.8660254037844387076, 1.000000000000000000, 0.8660254037844387076, 1.000000000000000000, 0.8660254037844387076, 1.000000000000000000, 0.8660254037844387076, 1.000000000000000000, 0.8660254037844387076, 1.000000000000000000, 0.8660254037844387076, 1.000000000000000000, 0.8660254037844387076, 1.000000000000000000, 0.8660254037844387076, 1.000000000000000000, 0.8660254037844387076, 1.000000000000000000, 0.8660254037844387076, 1.000000000000000000, 0.8660254037844387076, 1.000000000000000000, 0.8660254037844387076, 1.000000000000000000, 0.8660254037844387076, 1.000000000000000000, 0.8660254037844387076, 1.000000000000000000, 0.8660254037844387076, 1.000000000000000000, 0.8660254037844387076, 1.000000000000000000, 0.8660254037844387076, 1.000000000000000000, 0.8660254037844387076, 1.000000000000000000, 0.8660254037844387076, 1.000000000000000000, 0.8660254037844387076, 1.000000000000000000, 0.8660254037844387076, 1.000000000000000000, 0.8660254037844387076, 1.000000000000000000, 0.8660254037844387076, 1.000000000000000000, 0.8660254037844387076, 1.000000000000000000, 0.8660254037844387076, 1.000000000000000000, 0.8660254037844387076, 1.000000000000000000, 0.8660254037844387076, 1.000000000000000000, 0.8660254037844387076, 1.000000000000000000),
 ( 1.000000000000000000, 0.8660254037844387076, 1.000000000000000000, 0.8660254037844387076, 1.000000000000000000, 0.8660254037844387076, 1.000000000000000000, 0.8660254037844387076, 1.000000000000000000, 0.8660254037844387076, 1.000000000000000000, 0.8660254037844387076, 1.000000000000000000, 0.8660254037844387076, 1.000000000000000000, 0.8660254037844387076, 1.000000000000000000, 0.8660254037844387076, 1.000000000000000000, 0.8660254037844387076, 1.000000000000000000, 0.8660254037844387076, 1.000000000000000000, 0.8660254037844387076, 1.000000000000000000, 0.8660254037844387076, 1.000000000000000000, 0.8660254037844387076, 1.000000000000000000, 0.8660254037844387076, 1.000000000000000000, 0.8660254037844387076, 1.000000000000000000, 0.8660254037844387076, 1.000000000000000000, 0.8660254037844387076, 1.000000000000000000, 0.8660254037844387076, 1.000000000000000000, 0.8660254037844387076, 1.000000000000000000, 0.8660254037844387076, 1.000000000000000000, 0.8660254037844387076, 1.000000000000000000, 0.8660254037844387076, 1.000000000000000000, 0.8660254037844387076, 1.000000000000000000, 0.8660254037844387076, 1.000000000000000000, 0.8660254037844387076, 1.000000000000000000, 0.8660254037844387076, 1.000000000000000000, 0.8660254037844387076, 1.000000000000000000, 0.8660254037844387076, 1.000000000000000000, 0.8660254037844387076, 1.000000000000000000, 0.8660254037844387076, 1.000000000000000000, 0.8660254037844387076, 1.000000000000000000, 0.8660254037844387076, 1.000000000000000000, 0.8660254037844387076, 1.000000000000000000, 0.8660254037844387076, 1.000000000000000000, 0.8660254037844387076, 1.000000000000000000, 0.8660254037844387076, 1.000000000000000000, 0.8660254037844387076, 1.000000000000000000, 0.8660254037844387076, 1.000000000000000000, 0.8660254037844387076, 1.000000000000000000, 0.8660254037844387076, 1.000000000000000000, 0.8660254037844387076, 1.000000000000000000, 0.8660254037844387076, 1.000000000000000000, 0.8660254037844387076, 1.000000000000000000, 0.8660254037844387076, 1.000000000000000000, 0.8660254037844387076, 1.000000000000000000, 0.8660254037844387076, 1.000000000000000000, 0.8660254037844387076, 1.000000000000000000, 0.8660254037844387076, 1.000000000000000000, 0.8660254037844387076, 1.000000000000000000, 0.8660254037844387076, 1.000000000000000000, 0.8660254037844387076, 1.000000000000000000, 0.8660254037844387076, 1.000000000000000000, 0.8660254037844387076, 1.000000000000000000, 0.8660254037844387076, 1.000000000000000000, 0.8660254037844387076, 1.000000000000000000, 0.8660254037844387076, 1.000000000000000000, 0.8660254037844387076, 1.000000000000000000, 0.8660254037844387076, 1.000000000000000000, 0.8660254037844387076, 1.000000000000000000, 0.8660254037844387076, 1.000000000000000000, 0.8660254037844387076, 1.000000000000000000, 0.8660254037844387076, 1.000000000000000000, 0.8660254037844387076, 1.000000000000000000, 0.8660254037844387076, 1.000000000000000000, 0.8660254037844387076, 1.000000000000000000, 0.8660254037844387076, 1.000000000000000000, 0.8660254037844387076, 1.000000000000000000, 0.8660254037844387076, 1.000000000000000000, 0.8660254037844387076, 1.000000000000000000, 0.8660254037844387076, 1.000000000000000000, 0.8660254037844387076, 1.000000000000000000, 0.8660254037844387076, 1.000000000000000000, 0.8660254037844387076, 1.000000000000000000, 0.8660254037844387076, 1.000000000000000000, 0.8660254037844387076, 1.000000000000000000, 0.8660254037844387076, 1.000000000000000000, 0.8660254037844387076, 1.000000000000000000, 0.8660254037844387076, 1.000000000000000000, 0.8660254037844387076, 1.000000000000000000, 0.8660254037844387076, 1.000000000000000000, 0.8660254037844387076, 1.000000000000000000, 0.8660254037844387076, 1.000000000000000000, 0.8660254037844387076, 1.000000000000000000, 0.8660254037844387076, 1.000000000000000000, 0.8660254037844387076, 1.000000000000000000, 0.8660254037844387076, 1.000000000000000000, 0.8660254037844387076, 1.000000000000000000, 0.8660254037844387076, 1.000000000000000000, 0.8660254037844387076, 1.000000000000000000, 0.8660254037844387076, 1.000000000000000000, 0.8660254037844387076, 1.000000000000000000, 0.8660254037844387076, 1.000000000000000000, 0.8660254037844387076, 1.000000000000000000, 0.8660254037844387076, 1.000000000000000000, 0.8660254037844387076, 1.000000000000000000, 0.8660254037844387076, 1.000000000000000000, 0.8660254037844387076, 1.000000000000000000, 0.8660254037844387076, 1.000000000000000000, 0.8660254037844387076, 1.000000000000000000, 0.8660254037844387076, 1.000000000000000000, 0.8660254037844387076, 1.000000000000000000, 0.8660254037844387076, 1.000000000000000000, 0.8660254037844387076, 1.000000000000000000, 0.8660254037844387076, 1.000000000000000000, 0.8660254037844387076, 1.000000000000000000, 0.8660254037844387076, 1.000000000000000000, 0.8660254037844387076, 1.000000000000000000, 0.8660254037844387076, 1.000000000000000000, 0.8660254037844387076, 1.000000000000000000, 0.8660254037844387076, 1.000000000000000000, 0.8660254037844387076, 1.000000000000000000, 0.8660254037844387076, 1.000000000000000000, 0.8660254037844387076, 1.000000000000000000, 0.8660254037844387076, 1.000000000000000000, 0.8660254037844387076, 1.000000000000000000, 0.8660254037844387076, 1.000000000000000000, 0.8660254037844387076, 1.000000000000000000, 0.8660254037844387076, 1.000000000000000000, 0.8660254037844387076, 1.000000000000000000, 0.8660254037844387076, 1.000000000000000000, 0.8660254037844387076, 1.000000000000000000, 0.8660254037844387076, 1.000000000000000000, 0.8660254037844387076, 1.000000000000000000, 0.8660254037844387076, 1.000000000000000000, 0.8660254037844387076, 1.000000000000000000, 0.8660254037844387076, 1.000000000000000000, 0.8660254037844387076, 1.000000000000000000, 0.8660254037844387076, 1.000000000000000000, 0.8660254037844387076, 1.000000000000000000, 0.8660254037844387076, 1.000000000000000000, 0.8660254037844387076, 1.000000000000000000, 0.8660254037844387076, 1.000000000000000000, 0.8660254037844387076, 1.000000000000000000, 0.8660254037844387076, 1.000000000000000000, 0.8660254037844387076, 1.000000000000000000, 0.8660254037844387076, 1.000000000000000000, 0.8660254037844387076, 1.000000000000000000, 0.8660254037844387076, 1.000000000000000000, 0.8660254037844387076, 1.000000000000000000, 0.8660254037844387076, 1.000000000000000000, 0.8660254037844387076, 1.000000000000000000, 0.8660254037844387076, 1.000000000000000000, 0.8660254037844387076, 1.000000000000000000, 0.8660254037844387076, 1.000000000000000000, 0.8660254037844387076, 1.000000000000000000, 0.8660254037844387076, 1.000000000000000000, 0.8660254037844387076, 1.000000000000000000, 0.8660254037844387076, 1.000000000000000000, 0.8660254037844387076, 1.000000000000000000, 0.8660254037844387076, 1.000000000000000000, 0.8660254037844387076, 1.000000000000000000, 0.8660254037844387076, 1.000000000000000000, 0.8660254037844387076, 1.000000000000000000, 0.8660254037844387076, 1.000000000000000000, 0.8660254037844387076, 1.000000000000000000, 0.8660254037844387076, 1.000000000000000000, 0.8660254037844387076, 1.000000000000000000, 0.8660254037844387076, 1.000000000000000000, 0.8660254037844387076, 1.000000000000000000, 0.8660254037844387076, 1.000000000000000000, 0.8660254037844387076, 1.000000000000000000, 0.8660254037844387076, 1.000000000000000000, 0.8660254037844387076, 1.000000000000000000, 0.8660254037844387076, 1.000000000000000000, 0.8660254037844387076, 1.000000000000000000, 0.8660254037844387076, 1.000000000000000000, 0.8660254037844387076, 1.000000000000000000) ) ) 
 REPRESENTATION_ITEM ( '' )  SURFACE ( )  );
#92317 = CARTESIAN_POINT ( 'NONE',  ( 1.499999999999987121, 1.327083334016149641, -0.8660254037844253849 ) ) ;
#92318 = CARTESIAN_POINT ( 'NONE',  ( 6.481085492957645577, -0.09751705652460275486, -1.924153034975156995 ) ) ;
#92319 = CARTESIAN_POINT ( 'NONE',  ( -1.364683531250014514, 14.58854166700806232, -0.7879004041258335089 ) ) ;
#92320 = CARTESIAN_POINT ( 'NONE',  ( 3.129344976949835822, 2.009775620968552445, 0.9465212012665072949 ) ) ;
#92321 = ORIENTED_EDGE ( 'NONE', *, *, #93834, .T. ) ;
#92322 = CARTESIAN_POINT ( 'NONE',  ( -1.500000000000013101, 0.1708333333333560411, 0.8660254037844403729 ) ) ;
#92323 = CARTESIAN_POINT ( 'NONE',  ( 7.721532178182734185, 8.967207948423393304, 1.199719254218462483 ) ) ;
#92324 = CARTESIAN_POINT ( 'NONE',  ( 0.6823417656249864960, -0.8239583329919114574, -1.181850606188749264 ) ) ;
#92325 = CARTESIAN_POINT ( 'NONE',  ( 6.486594595706023370, -1.368296875179885852, 1.750867008312809059 ) ) ;
#92327 = CARTESIAN_POINT ( 'NONE',  ( 4.809014631063706524, -1.576880339463518022, 1.167019128429528374 ) ) ;
#92326 = CIRCLE ( 'NONE', #202962, 0.07999999999999998779 ) ;
#92329 = CARTESIAN_POINT ( 'NONE',  ( -4.582292731738899505, 8.289832587096611860, 0.7216878364870458196 ) ) ;
#92328 = CARTESIAN_POINT ( 'NONE',  ( 9.897088948295943212, 11.60932053017587506, 1.082531754730548412 ) ) ;
#92330 = CARTESIAN_POINT ( 'NONE',  ( -11.41042268598796561, 3.467171072964049028, 3.707471073020331076 ) ) ;
#92331 = CARTESIAN_POINT ( 'NONE',  ( 5.993528260394247020, 1.707464403934123798, 1.484360591965392828 ) ) ;
#92332 = CARTESIAN_POINT ( 'NONE',  ( 2.471201797017197777, 1.841352583063287529, 0.9297268146766042296 ) ) ;
#92333 = CARTESIAN_POINT ( 'NONE',  ( -7.230575994789712801, 7.330093503543126054, 0.7998128361456341429 ) ) ;
#92334 = ORIENTED_EDGE ( 'NONE', *, *, #105381, .F. ) ;
#92335 = CARTESIAN_POINT ( 'NONE',  ( -1.402160292154681736E-14, 2.368750000682818602, -1.732050807568863648 ) ) ;
#92336 = CARTESIAN_POINT ( 'NONE',  ( 4.112460492241882370, 1.324567223757302292, -1.321038939096484066 ) ) ;
#92337 = CARTESIAN_POINT ( 'NONE',  ( 2.584235440824592001, -0.5423091454765850417, 1.647252552357024280 ) ) ;
#92338 = CARTESIAN_POINT ( 'NONE',  ( -0.1112335732281382050, -0.5161050057324081397, -2.242239947022279356 ) ) ;
#92339 = CARTESIAN_POINT ( 'NONE',  ( 0.6927435329204565395, -2.190372518412486702, -0.2681103625320201411 ) ) ;
#92340 = CARTESIAN_POINT ( 'NONE',  ( 6.210880146794990786, -0.2354563166601444379, 1.927560789186753665 ) ) ;
#92341 =( GEOMETRIC_REPRESENTATION_CONTEXT ( 3 ) GLOBAL_UNCERTAINTY_ASSIGNED_CONTEXT ( ( #167980 ) ) GLOBAL_UNIT_ASSIGNED_CONTEXT ( ( #193242, #192157, #10216 ) ) REPRESENTATION_CONTEXT ( 'NONE', 'WORKASPACE' ) );
#92342 = CARTESIAN_POINT ( 'NONE',  ( 7.862692832760656891, 15.31533744430288024, 9.008167824251760436 ) ) ;
#92343 =( NAMED_UNIT ( * ) PLANE_ANGLE_UNIT ( ) SI_UNIT ( $, .RADIAN. ) );
#92344 = CARTESIAN_POINT ( 'NONE',  ( 0.1236729436712938751, 0.3474707636354073537, 1.986100063511665237 ) ) ;
#92345 = CARTESIAN_POINT ( 'NONE',  ( 0.1938080739139167730, 1.976361990896974508, -0.7691651810952588875 ) ) ;
#92346 = PRESENTATION_STYLE_ASSIGNMENT (( #91268 ) ) ;
#92347 = DIRECTION ( 'NONE',  ( 0.000000000000000000, 0.000000000000000000, -1.000000000000000000 ) ) ;
#92348 = CARTESIAN_POINT ( 'NONE',  ( -9.840520565420403543, 10.37502883594562597, 1.040834085586084257E-14 ) ) ;
#92349 = CARTESIAN_POINT ( 'NONE',  ( 7.820355676984174664, 8.018169799436671852, -0.7998128361456281477 ) ) ;
#92350 = CARTESIAN_POINT ( 'NONE',  ( 0.000000000000000000, 12.31951671548121219, 0.000000000000000000 ) ) ;
#92351 = CARTESIAN_POINT ( 'NONE',  ( 4.881388680972560401, 1.702354803207173584, -0.6601141376258444771 ) ) ;
#92352 = CARTESIAN_POINT ( 'NONE',  ( 1.993488836774780060, 1.919990754028239488, -1.087721427556323617 ) ) ;
#92353 = EDGE_LOOP ( 'NONE', ( #52904, #10530, #54621, #70997, #107533, #15126 ) ) ;
#92354 = CARTESIAN_POINT ( 'NONE',  ( -3.757017964318317471, 6.436919154129725484, 1.082531754730549967 ) ) ;
#92355 = CARTESIAN_POINT ( 'NONE',  ( 3.285556943750000070, -2.821874999522043570, 0.000000000000000000 ) ) ;
#92356 = CARTESIAN_POINT ( 'NONE',  ( -8.158255747121117452, 10.54105100977322174, 1.599625672291295375 ) ) ;
#92357 = CARTESIAN_POINT ( 'NONE',  ( 1.002220075199202309, -0.9041908160717628817, 1.806139134770538002 ) ) ;
#92359 = EDGE_CURVE ( 'NONE', #32719, #111607, #123170, .T. ) ;
#92358 = CARTESIAN_POINT ( 'NONE',  ( -1.286956418854606543, 4.047654341997520611, 0.4592741676706140197 ) ) ;
#92360 = ORIENTED_EDGE ( 'NONE', *, *, #38367, .T. ) ;
#92361 = CARTESIAN_POINT ( 'NONE',  ( -5.795184315198522285, 5.725746220678519904, -0.7998128361456362523 ) ) ;
#92362 = CARTESIAN_POINT ( 'NONE',  ( 3.010441868158566958, 0.6223964701937385602, 1.753942229013090159 ) ) ;
#92363 = CARTESIAN_POINT ( 'NONE',  ( 10.16199982864259788, 11.81442020729326536, 1.199719254218452047 ) ) ;
#92364 = CARTESIAN_POINT ( 'NONE',  ( 5.397554552016217144, 7.390509292142662723, 1.443375672974065660 ) ) ;
#92365 = EDGE_LOOP ( 'NONE', ( #44520, #171909, #207534, #161527 ) ) ;
#92366 = ORIENTED_EDGE ( 'NONE', *, *, #116999, .T. ) ;
#92367 = CARTESIAN_POINT ( 'NONE',  ( -7.458957065812611198, 11.85386701009007204, 0.7998128361456481317 ) ) ;
#92368 = CARTESIAN_POINT ( 'NONE',  ( 4.107882937833263526, -1.820653182827164596, 0.1363937739093170898 ) ) ;
#92369 = CARTESIAN_POINT ( 'NONE',  ( -4.248501033035892327, 6.049946853332221153, -1.599625672291271394 ) ) ;
#92370 = CARTESIAN_POINT ( 'NONE',  ( 6.606300428615679898, 6.765996464729716386, -0.04887194053871009303 ) ) ;
#92371 = CARTESIAN_POINT ( 'NONE',  ( 0.9481301099739076754, 1.159027798429014045, 1.289721149823976676 ) ) ;
#92372 = CARTESIAN_POINT ( 'NONE',  ( 5.525302006934727395, -1.171079710934025186, -1.420692760577553226 ) ) ;
#92373 = CARTESIAN_POINT ( 'NONE',  ( 3.985262446249608903, -0.2245550567474114134, -2.296750103337093396 ) ) ;
#92374 = CARTESIAN_POINT ( 'NONE',  ( 5.551137550152489553, 5.441024994791534120, 0.7998128361456352531 ) ) ;
#92375 = CARTESIAN_POINT ( 'NONE',  ( 0.7728169288007546989, -1.939476032597256872, -0.6969182633713083552 ) ) ;
#92376 = CARTESIAN_POINT ( 'NONE',  ( 6.307567778855705853, 8.381915046796901692, -1.599625672291262513 ) ) ;
#92377 = CARTESIAN_POINT ( 'NONE',  ( 2.507286712376335824, -1.920573583173491139, 0.2874136252781610001 ) ) ;
#92378 = EDGE_CURVE ( 'NONE', #72572, #50089, #156646, .T. ) ;
#92379 = EDGE_CURVE ( 'NONE', #201806, #128654, #22530, .T. ) ;
#92380 = CARTESIAN_POINT ( 'NONE',  ( 5.448667688119189556, 1.537605954158068666, 1.708491323253034100 ) ) ;
#92381 = CARTESIAN_POINT ( 'NONE',  ( 0.7500000000000006661, 11.44791666734946212, -1.299038105676657340 ) ) ;
#92382 = CARTESIAN_POINT ( 'NONE',  ( -2.830620210203090181, 6.524417021870718258, 0.000000000000000000 ) ) ;
#92383 = CARTESIAN_POINT ( 'NONE',  ( 5.190257414508706368, -1.856628772771324210, -0.2281712211116558864 ) ) ;
#92384 = EDGE_LOOP ( 'NONE', ( #125709, #147228, #174692, #133791 ) ) ;
#92386 = CARTESIAN_POINT ( 'NONE',  ( -4.125423880308188629, 8.035021303660014880, -0.7998128361456481317 ) ) ;
#92385 = CARTESIAN_POINT ( 'NONE',  ( 2.214975196874233720, 1.533708969217022933, -1.142120075431733994 ) ) ;
#92387 = CARTESIAN_POINT ( 'NONE',  ( 3.422699507934781060, 1.400174360247144589, -1.705827624971032686 ) ) ;
#92388 = CARTESIAN_POINT ( 'NONE',  ( -1.552391752028397856E-14, 0.1250000006828045906, 1.414508159514549446 ) ) ;
#92389 = CARTESIAN_POINT ( 'NONE',  ( 6.883263157960373135, 2.058310207169287143, 2.252834201749584153 ) ) ;
#92390 = CARTESIAN_POINT ( 'NONE',  ( 4.055297343818923039, 7.745280977848496562, 0.7216878364870257245 ) ) ;
#92391 = CARTESIAN_POINT ( 'NONE',  ( -6.902509602688830626, 7.225551755991315162, -0.7216878364870338292 ) ) ;
#92392 = CARTESIAN_POINT ( 'NONE',  ( 2.204549329899041510, -2.307029201398633322, 0.05716382847485364238 ) ) ;
#92393 = CARTESIAN_POINT ( 'NONE',  ( 2.611707774152134842, 0.5260268489151798121, -1.889944157703125072 ) ) ;
#92394 = CARTESIAN_POINT ( 'NONE',  ( 6.174688434915334589, 1.389358497796209013, -1.524562697504736164 ) ) ;
#92395 = CARTESIAN_POINT ( 'NONE',  ( 3.497640442645619796, 6.064035702186436616, -1.082531754730543083 ) ) ;
#92396 = CARTESIAN_POINT ( 'NONE',  ( 3.907435596788138010, -1.928258004016227378, 0.5899861904685861358 ) ) ;
#92397 = CARTESIAN_POINT ( 'NONE',  ( 5.551137550152489553, 5.441024994791534120, 0.7998128361456352531 ) ) ;
#92398 = EDGE_LOOP ( 'NONE', ( #195041, #12599, #37537, #190804 ) ) ;
#92399 = CARTESIAN_POINT ( 'NONE',  ( 4.487517715496184501, -0.5331711073110931842, 1.944729879240604253 ) ) ;
#92400 = CARTESIAN_POINT ( 'NONE',  ( -9.297140650669053485, 11.86975006391249643, 1.599625672291281386 ) ) ;
#92401 = CARTESIAN_POINT ( 'NONE',  ( -11.14501278000869355, 7.223412960316487386, -3.546411330735405265 ) ) ;
#92402 = CARTESIAN_POINT ( 'NONE',  ( 2.535011535630975477, 5.901337858304024131, 0.7216878364870438212 ) ) ;
#92404 = VECTOR ( 'NONE', #173295, 1000.000000000000000 ) ;
#92403 = CARTESIAN_POINT ( 'NONE',  ( 2.536178501573463695, 1.332599179293973091, 1.713937585783622541 ) ) ;
#92405 = CARTESIAN_POINT ( 'NONE',  ( 5.879395890181562834, 6.888325289080478697, -1.199719254218452047 ) ) ;
#92406 = CARTESIAN_POINT ( 'NONE',  ( -0.1021852871539799257, 7.117056311352818909, -3.989408415137027042 ) ) ;
#92407 = CARTESIAN_POINT ( 'NONE',  ( 2.231529376059933956, -1.218349341866202362, -1.419469154777988518 ) ) ;
#92408 = CARTESIAN_POINT ( 'NONE',  ( 6.485629946217342123, 1.485420011660616657, 1.570608065930901187 ) ) ;
#92410 = CARTESIAN_POINT ( 'NONE',  ( 3.468329555040600365, 6.306621445965236106, 1.127812995945943086 ) ) ;
#92409 = CARTESIAN_POINT ( 'NONE',  ( 0.07775346131144458828, -0.005211914751935413023, -2.288974916015192651 ) ) ;
#92411 = CARTESIAN_POINT ( 'NONE',  ( -1.402160292154681736E-14, 0.5718750003414239114, 1.575800808251672791 ) ) ;
#92412 = DIRECTION ( 'NONE',  ( -1.000000000000000000, 1.224646799147352714E-16, 0.000000000000000000 ) ) ;
#92413 = CARTESIAN_POINT ( 'NONE',  ( 3.281800106729782840, 1.865104756965057620, -0.4213900744019505318 ) ) ;
#92414 = CARTESIAN_POINT ( 'NONE',  ( 4.416719503454580753, 1.618597840523916753, 0.7163212975811702465 ) ) ;
#92415 = CARTESIAN_POINT ( 'NONE',  ( 1.418461073652961257, -0.6892283116659430053, -1.783923526276688154 ) ) ;
#92416 = CARTESIAN_POINT ( 'NONE',  ( -4.925689880466507908, 4.641059703499347044, -0.7998128361456221525 ) ) ;
#92418 = CARTESIAN_POINT ( 'NONE',  ( -0.2353475280464593089, -0.1482846297235005661, -1.883952934485186415 ) ) ;
#92417 = DIRECTION ( 'NONE',  ( 0.7592566023653004592, -0.6507913734559639396, -0.000000000000000000 ) ) ;
#92419 = CARTESIAN_POINT ( 'NONE',  ( -1.500000000000001332, -0.3499999999999753308, 0.000000000000000000 ) ) ;
#92420 = CARTESIAN_POINT ( 'NONE',  ( 1.258353326579707776, -2.070544811992577561, -0.001879966208345739808 ) ) ;
#92421 = CARTESIAN_POINT ( 'NONE',  ( -0.7500000000000215383, 5.441666666666685082, 1.299038105676671107 ) ) ;
#92422 = CARTESIAN_POINT ( 'NONE',  ( 6.649288223980674317, -1.503899034092892162, -1.112267350887645945 ) ) ;
#92423 = CARTESIAN_POINT ( 'NONE',  ( 1.471042373949003501, 0.1361147407585860392, -1.820667060309004937 ) ) ;
#92425 = CARTESIAN_POINT ( 'NONE',  ( 4.600487305768355739, 8.366733224642864286, -0.1591645125929436189 ) ) ;
#92424 = CARTESIAN_POINT ( 'NONE',  ( 5.303435803989668074, 1.802500012205746183, 1.273053691228965389 ) ) ;
#92426 = CARTESIAN_POINT ( 'NONE',  ( -1.402160292154681736E-14, -0.4281249996585808071, 1.575800808251672791 ) ) ;
#92427 = CARTESIAN_POINT ( 'NONE',  ( 3.508308746731583216, 2.062851380131548229, 0.002797760368935045105 ) ) ;
#92428 = CARTESIAN_POINT ( 'NONE',  ( -8.213542131780492639, 8.476887330032372603, 1.040834085586084257E-14 ) ) ;
#92429 = CARTESIAN_POINT ( 'NONE',  ( 9.738834413317897898, 10.25639499182604730, 0.000000000000000000 ) ) ;
#92430 = CARTESIAN_POINT ( 'NONE',  ( 1.446621748570332322, 3.374878948858031080, -0.4012476001784985313 ) ) ;
#92431 = CARTESIAN_POINT ( 'NONE',  ( 0.7905619602705875604, -2.145198653374354336, -0.2653712149464776959 ) ) ;
#92432 = CARTESIAN_POINT ( 'NONE',  ( 5.494797395288433250, 9.632623737803665875, 0.000000000000000000 ) ) ;
#92433 = VECTOR ( 'NONE', #97315, 1000.000000000000000 ) ;
#92434 = ORIENTED_EDGE ( 'NONE', *, *, #13181, .T. ) ;
#92435 = CARTESIAN_POINT ( 'NONE',  ( 5.916483165358986440, 0.8355632440216669288, 1.894440869009452300 ) ) ;
#92436 = CARTESIAN_POINT ( 'NONE',  ( 1.364683531249986537, 0.4260416670080872659, 0.7879004041258500513 ) ) ;
#92437 = CARTESIAN_POINT ( 'NONE',  ( 3.058072297120766780, 2.151488047868503894, -0.2085137855245971505 ) ) ;
#92438 = CARTESIAN_POINT ( 'NONE',  ( -4.879429750001362365, 8.060225557361109239, -0.9362273787268098335 ) ) ;
#92440 = CARTESIAN_POINT ( 'NONE',  ( 2.172246964874047670, -0.9220853831424129510, -1.731647142839589648 ) ) ;
#92439 = CARTESIAN_POINT ( 'NONE',  ( 2.983074145627107931, -1.866958838928289399, -0.7709177042417614256 ) ) ;
#92441 = CARTESIAN_POINT ( 'NONE',  ( 6.720655732516649827, 0.5759399164693942419, 2.126764875236677454 ) ) ;
#92442 = ORIENTED_EDGE ( 'NONE', *, *, #8236, .F. ) ;
#92443 = ADVANCED_FACE ( 'NONE', ( #23406 ), #92724, .F. ) ;
#92446 = CARTESIAN_POINT ( 'NONE',  ( 7.293923454472087897, 8.572294120714675003, 1.082531754730558626 ) ) ;
#92445 = CARTESIAN_POINT ( 'NONE',  ( -1.737500000000000266, -1.458333333333332371, -3.009438278150923907 ) ) ;
#92444 = CARTESIAN_POINT ( 'NONE',  ( 11.01135777277262306, 0.000000000000000000, -1.400000000000001910 ) ) ;
#92447 = CARTESIAN_POINT ( 'NONE',  ( -7.306918443122272677, 7.489436036589583345, 0.7998128361456341429 ) ) ;
#92448 = CARTESIAN_POINT ( 'NONE',  ( 1.376185782568883020, -2.007256511855738612, -0.1928315418098166534 ) ) ;
#92450 = CARTESIAN_POINT ( 'NONE',  ( 6.550331612656306035, -1.695486744446069727, 1.388264742925699569 ) ) ;
#92449 = CARTESIAN_POINT ( 'NONE',  ( -4.822949958159302497, 6.649860922651058992, -1.599625672291256295 ) ) ;
#92451 = DIRECTION ( 'NONE',  ( -0.008295560218254071499, -1.694007603815957969E-16, -0.9999655912483517151 ) ) ;
#92452 = CARTESIAN_POINT ( 'NONE',  ( 5.396708386617175890, -1.867154475869851504, -0.4128305108781898936 ) ) ;
#92453 = CARTESIAN_POINT ( 'NONE',  ( -4.499752021454321849, 4.967787669261691796, -0.8784368744512593974 ) ) ;
#92454 = CARTESIAN_POINT ( 'NONE',  ( 5.626270559546814098, 7.587068290936515247, 1.443375672974062551 ) ) ;
#92456 = CARTESIAN_POINT ( 'NONE',  ( 2.970327539257538341, -1.987051465770898417, -0.3419137282784574516 ) ) ;
#92455 = CARTESIAN_POINT ( 'NONE',  ( -8.256552360598034213, 11.61609960646427986, 1.082531754730549967 ) ) ;
#92457 = CARTESIAN_POINT ( 'NONE',  ( -0.6823417656250039265, 13.38020833367473195, -1.181850606188755259 ) ) ;
#92458 = CARTESIAN_POINT ( 'NONE',  ( 4.840679758638335883, 0.2971110944181546976, 1.698800604571904849 ) ) ;
#92459 = CARTESIAN_POINT ( 'NONE',  ( 6.119526231721748033, 8.232809585132461194, 1.599625672291269396 ) ) ;
#92460 = CARTESIAN_POINT ( 'NONE',  ( 2.737856954955798727, 5.281584649835344258, 1.199719254218452047 ) ) ;
#92461 = CARTESIAN_POINT ( 'NONE',  ( -11.33772467203841394, 11.00732847981850426, -3.600000000000000977 ) ) ;
#92462 = CARTESIAN_POINT ( 'NONE',  ( 4.411305886619627081, -0.3218996851035611506, 1.842484647571709822 ) ) ;
#92463 = ADVANCED_FACE ( 'NONE', ( #204276 ), #10601, .T. ) ;
#92464 = CARTESIAN_POINT ( 'NONE',  ( 0.000000000000000000, 4.400000000000001243, 0.000000000000000000 ) ) ;
#92465 = CIRCLE ( 'NONE', #113374, 12.00000000000000178 ) ;
#92466 = CARTESIAN_POINT ( 'NONE',  ( 0.7958623839904412911, -1.461433461687311253, -1.466603172318406090 ) ) ;
#92467 = CYLINDRICAL_SURFACE ( 'NONE', #22368, 2.025000000000006573 ) ;
#92468 = ORIENTED_EDGE ( 'NONE', *, *, #29848, .F. ) ;
#92469 = CARTESIAN_POINT ( 'NONE',  ( 3.217027588192558074, 6.975225629525113824, -1.734723475976807094E-15 ) ) ;
#92470 = CARTESIAN_POINT ( 'NONE',  ( -0.01795374796791787686, -2.016030408028956167, -0.04665595434990427171 ) ) ;
#92471 = CARTESIAN_POINT ( 'NONE',  ( -0.05289022600267567070, -1.656485410061825592, 0.7338673832079073422 ) ) ;
#92472 = CARTESIAN_POINT ( 'NONE',  ( 4.529832720297257254, 8.298905583739861314, 0.000000000000000000 ) ) ;
#92473 = CARTESIAN_POINT ( 'NONE',  ( 11.15287142971249246, 9.124439414695240558, 4.432553360691933619 ) ) ;
#92474 = ORIENTED_EDGE ( 'NONE', *, *, #38562, .F. ) ;
#92476 = CARTESIAN_POINT ( 'NONE',  ( 6.968000882419564945, 10.21675256520979858, 1.199719254218460707 ) ) ;
#92475 = CARTESIAN_POINT ( 'NONE',  ( 0.5374593765826127800, 1.831924746014142791, -0.7026076897959919743 ) ) ;
#92477 = CARTESIAN_POINT ( 'NONE',  ( 5.026915340915774522, -1.640707562863060520, 0.9885212758144015233 ) ) ;
#92478 = CARTESIAN_POINT ( 'NONE',  ( 0.000000000000000000, -3.042800438942089514, 0.000000000000000000 ) ) ;
#92479 = CARTESIAN_POINT ( 'NONE',  ( -10.43434622977936854, 1.529612873802629780, 5.577395135400619708 ) ) ;
#92481 = ORIENTED_EDGE ( 'NONE', *, *, #168793, .F. ) ;
#92480 = CARTESIAN_POINT ( 'NONE',  ( 3.036663219780971978, 6.486598156479028709, -0.7216878364870267237 ) ) ;
#92482 = EDGE_CURVE ( 'NONE', #96549, #95577, #22845, .T. ) ;
#92483 = CARTESIAN_POINT ( 'NONE',  ( -7.212574532790092974, 10.39812547402169862, -1.082531754730543971 ) ) ;
#92484 = AXIS2_PLACEMENT_3D ( 'NONE', #191603, #90944, #157011 ) ;
#92485 = CARTESIAN_POINT ( 'NONE',  ( 2.202237438260604030, -2.161223104231101644, 0.05255616829508147347 ) ) ;
#92486 = CARTESIAN_POINT ( 'NONE',  ( -3.851398154733808088, 6.650992392901508232, -1.199719254218450271 ) ) ;
#92487 = CARTESIAN_POINT ( 'NONE',  ( 7.688882512725796481, 8.142986817701137525, 0.000000000000000000 ) ) ;
#92488 = CARTESIAN_POINT ( 'NONE',  ( -2.252626078164912560, 5.779814191167667481, 0.7998128361456341429 ) ) ;
#92489 = EDGE_CURVE ( 'NONE', #79317, #213798, #190690, .T. ) ;
#92490 = CARTESIAN_POINT ( 'NONE',  ( 4.489149150750438189, 1.630474666268775685, -0.8212668906743822994 ) ) ;
#92491 = CARTESIAN_POINT ( 'NONE',  ( 11.22826844164464433, 7.784147190670918093, 5.449213193111969389 ) ) ;
#92492 = CARTESIAN_POINT ( 'NONE',  ( 1.036326318785439016, 1.941456103877332140, 0.3412654001589945918 ) ) ;
#92493 = VERTEX_POINT ( 'NONE', #43411 ) ;
#92494 = LINE ( 'NONE', #158533, #63174 ) ;
#92495 = CARTESIAN_POINT ( 'NONE',  ( 3.912524032909367566, 0.7067130192578415793, 1.838586846604377323 ) ) ;
#92496 = ORIENTED_EDGE ( 'NONE', *, *, #14937, .F. ) ;
#92497 = CARTESIAN_POINT ( 'NONE',  ( 5.636261916347573120, 0.3829244189050336478, 1.903776902374450630 ) ) ;
#92498 = EDGE_LOOP ( 'NONE', ( #44515, #13204, #173750 ) ) ;
#92499 = CARTESIAN_POINT ( 'NONE',  ( -6.286140498591554326, 7.362860665558790707, 1.199719254218452047 ) ) ;
#92501 = CARTESIAN_POINT ( 'NONE',  ( 6.152600690169603759, 2.097733681304454034, 0.3095894981632040244 ) ) ;
#92500 = CARTESIAN_POINT ( 'NONE',  ( -5.646044625448194410, 5.551749915969804938, 0.000000000000000000 ) ) ;
#92502 = CARTESIAN_POINT ( 'NONE',  ( 7.824464048418096951, 8.301165276008827476, -0.7216878364870317197 ) ) ;
#92504 = ORIENTED_EDGE ( 'NONE', *, *, #101474, .T. ) ;
#92503 = CARTESIAN_POINT ( 'NONE',  ( 4.406835678522929456, -0.4222698756407486931, -1.864907683101609370 ) ) ;
#92505 = B_SPLINE_CURVE_WITH_KNOTS ( 'NONE', 3,
 ( #196276, #91597, #114034, #207441, #9246, #157649 ),
 .UNSPECIFIED., .F., .F.,
 ( 4, 2, 4 ),
 ( 0.0006258038130483377197, 0.0009388807108837884767, 0.001251957608719239234 ),
 .UNSPECIFIED. ) ;
#92506 = CARTESIAN_POINT ( 'NONE',  ( -6.748402506350539731, 15.51952511195976214, -9.932705294953846575 ) ) ;
#92507 = CARTESIAN_POINT ( 'NONE',  ( 2.891631901464575272, 6.595597328342462262, 0.000000000000000000 ) ) ;
#92508 = CARTESIAN_POINT ( 'NONE',  ( 9.406792723036451420, 4.446947629225756593, -7.380298948578194462 ) ) ;
#92509 = CARTESIAN_POINT ( 'NONE',  ( 4.652993947568984545, 0.3464272572618365964, 1.982917695270119518 ) ) ;
#92510 = DIRECTION ( 'NONE',  ( 1.000000000000000000, -0.000000000000000000, 1.224646799147353207E-16 ) ) ;
#92511 = CARTESIAN_POINT ( 'NONE',  ( 5.760330229460346452, 0.7440287100829169331, 1.667389206893993725 ) ) ;
#92512 = CARTESIAN_POINT ( 'NONE',  ( 1.645070734656968625, -0.3017366986639742343, -2.048123538821472245 ) ) ;
#92513 = CARTESIAN_POINT ( 'NONE',  ( -5.442708600882160574, 8.437244903416123876, -1.199719254218446718 ) ) ;
#92514 = CARTESIAN_POINT ( 'NONE',  ( -5.355672060655169098, 7.601107163255693244, -1.239215230201977436 ) ) ;
#92515 = DIRECTION ( 'NONE',  ( 0.000000000000000000, 0.000000000000000000, -1.000000000000000000 ) ) ;
#92516 = CARTESIAN_POINT ( 'NONE',  ( 1.001543065824772753E-15, -2.821874999522044458, 3.793834371823810780 ) ) ;
#92517 = CARTESIAN_POINT ( 'NONE',  ( 4.299907273828439180, 8.168308919441841454, 1.040834085586084257E-14 ) ) ;
#92518 = DIRECTION ( 'NONE',  ( 0.000000000000000000, 0.000000000000000000, 1.000000000000000000 ) ) ;
#92519 = CARTESIAN_POINT ( 'NONE',  ( 4.963693636378940788, 5.923969009597785274, -1.082531754730548412 ) ) ;
#92520 = CARTESIAN_POINT ( 'NONE',  ( -15.75000000000000000, 12.30000000000000071, -1.800000000000001155 ) ) ;
#92521 = CARTESIAN_POINT ( 'NONE',  ( 1.364683531249997417, 12.29687500034139980, 2.602085213965210642E-15 ) ) ;
#92522 = CARTESIAN_POINT ( 'NONE',  ( -5.135841261478327979, 4.886236314679810455, 0.7998128361456341429 ) ) ;
#92524 = CARTESIAN_POINT ( 'NONE',  ( -5.875479466675803231, 7.948088359245467416, -1.599625672291271394 ) ) ;
#92523 = CARTESIAN_POINT ( 'NONE',  ( 6.766604819867117371, -7.256397064628601790, -6.766604819867143128 ) ) ;
#92525 = CARTESIAN_POINT ( 'NONE',  ( 4.359819935191601381, -0.006009022472676025205, -1.734343005118470726 ) ) ;
#92526 = CARTESIAN_POINT ( 'NONE',  ( -3.554208825076827782, 7.298327395898266623, 0.7998128361456341429 ) ) ;
#92527 = CARTESIAN_POINT ( 'NONE',  ( 2.887621454190898884, -1.933326653459125355, 0.7409182656877840722 ) ) ;
#92528 = CARTESIAN_POINT ( 'NONE',  ( 3.023186137256496764, -1.865899319694108272, 1.000581237753160879 ) ) ;
#92529 = CARTESIAN_POINT ( 'NONE',  ( 6.968000882419564945, 10.21675256520979858, 1.199719254218460707 ) ) ;
#92530 = CARTESIAN_POINT ( 'NONE',  ( 0.08500055850266946544, -9.912493587006867557, 10.99967158169071446 ) ) ;
#92531 = CARTESIAN_POINT ( 'NONE',  ( 1.744903480705553012, -0.2836847097360816194, -1.948756091721944861 ) ) ;
#92532 = CARTESIAN_POINT ( 'NONE',  ( 5.834672162164848075, 6.194663582219344988, 0.9174233710642684114 ) ) ;
#92533 = CARTESIAN_POINT ( 'NONE',  ( 3.063779527008311021, 5.557864633942907417, 1.082531754730546636 ) ) ;
#92535 = CARTESIAN_POINT ( 'NONE',  ( -0.07025823700084612988, -1.875094440630159065, 0.3749275819610526916 ) ) ;
#92534 = CARTESIAN_POINT ( 'NONE',  ( -1.737499999999997824, -2.391666666666667052, 3.009438278150925683 ) ) ;
#92536 = CARTESIAN_POINT ( 'NONE',  ( 3.785359544849807190, 1.659571404495253866, 1.581462771572618609 ) ) ;
#92537 = CARTESIAN_POINT ( 'NONE',  ( 0.4690313652776016418, 0.1822212253758948297, -1.816563760317004395 ) ) ;
#92538 = CARTESIAN_POINT ( 'NONE',  ( 4.681308178468477799, 8.683552984847038303, 0.000000000000000000 ) ) ;
#92539 = CARTESIAN_POINT ( 'NONE',  ( 7.443063143778065438, 7.785921210603627962, -0.7216878364870257245 ) ) ;
#92540 = CARTESIAN_POINT ( 'NONE',  ( -9.155833807930273238, 9.576227618873799585, -0.7998128361456291469 ) ) ;
#92541 = CARTESIAN_POINT ( 'NONE',  ( 2.197523118450269486, 1.838911438263282738, -0.8198142501213819822 ) ) ;
#92542 = CARTESIAN_POINT ( 'NONE',  ( 2.535929169054650156, 1.202975682259961765, 1.549578550289295586 ) ) ;
#92543 = CARTESIAN_POINT ( 'NONE',  ( -9.104463846776669200, 10.58062822844965645, -1.199719254218441611 ) ) ;
#92544 = VECTOR ( 'NONE', #158110, 1000.000000000000000 ) ;
#92545 = CARTESIAN_POINT ( 'NONE',  ( -6.307567778855718288, 8.381915046796901692, -1.599625672291263179 ) ) ;
#92546 = CARTESIAN_POINT ( 'NONE',  ( 0.07536363704233395300, 5.720741966631408104, -2.738263776839637398 ) ) ;
#92548 = CARTESIAN_POINT ( 'NONE',  ( 3.695971326421595204, -1.767833007231565334, -0.08711813594433276409 ) ) ;
#92547 = CARTESIAN_POINT ( 'NONE',  ( 5.455056007322736100, 0.4086298902603173744, -2.050129383449701415 ) ) ;
#92549 = CARTESIAN_POINT ( 'NONE',  ( -3.796053574492201044, 16.00000000000182254, 12.24940615670304211 ) ) ;
#92550 = CARTESIAN_POINT ( 'NONE',  ( 6.544901331262317434, -1.836973039681317088, -1.370978055005685370 ) ) ;
#92551 = CARTESIAN_POINT ( 'NONE',  ( 5.402228116617870946, 1.314032936993884793, -1.141193381800218232 ) ) ;
#92552 = CARTESIAN_POINT ( 'NONE',  ( 9.250740883225924804, 9.686952540052077509, 1.040834085586084257E-14 ) ) ;
#92553 = CARTESIAN_POINT ( 'NONE',  ( 5.766309430914762224, 2.125181855325126712, -0.8765443895848085143 ) ) ;
#92554 = DIRECTION ( 'NONE',  ( 0.000000000000000000, 0.000000000000000000, -1.000000000000000000 ) ) ;
#92555 = CARTESIAN_POINT ( 'NONE',  ( 6.116466030266402676, 0.5002120791919911769, -1.660072079997718442 ) ) ;
#92556 = CARTESIAN_POINT ( 'NONE',  ( 5.846172790272405884, -0.9815748167120906809, 1.936718618010783377 ) ) ;
#92557 = CARTESIAN_POINT ( 'NONE',  ( 3.277320446201373638, 4.846626492033466072, 1.599625672291267398 ) ) ;
#92558 = CARTESIAN_POINT ( 'NONE',  ( 0.5150563930837145366, 0.1624822992478615336, 2.111197286521369065 ) ) ;
#92559 = CARTESIAN_POINT ( 'NONE',  ( 6.437500000220395258, 1.451031294483499545, -1.451031289061371021 ) ) ;
#92560 = CARTESIAN_POINT ( 'NONE',  ( -0.7499999999999972244, 5.389583334016151639, -1.299038105676652899 ) ) ;
#92561 = CARTESIAN_POINT ( 'NONE',  ( 4.489231697071988769, 1.720940496173857470, -0.8657641181536148700 ) ) ;
#92562 = CARTESIAN_POINT ( 'NONE',  ( 0.7500000000000006661, 11.36458333401613174, 1.299038105676657340 ) ) ;
#92563 = CARTESIAN_POINT ( 'NONE',  ( 0.1709645942036420174, 0.8561845417300646410, 2.049862257243968422 ) ) ;
#92564 = ORIENTED_EDGE ( 'NONE', *, *, #83416, .T. ) ;
#92565 = CARTESIAN_POINT ( 'NONE',  ( -1.499999999999997780, 4.650000000000022560, 1.214306433183764966E-14 ) ) ;
#92566 = CARTESIAN_POINT ( 'NONE',  ( 3.876741858503734761, 6.610283703974623393, 1.199719254218462483 ) ) ;
#92567 = CARTESIAN_POINT ( 'NONE',  ( 5.849453209292126310, 8.911780279894442103, 1.199719254218462483 ) ) ;
#92568 = CARTESIAN_POINT ( 'NONE',  ( 2.702056655550812980, 1.572631313784816687, 1.569006521454456848 ) ) ;
#92569 = SURFACE_SIDE_STYLE ('',( #108854 ) ) ;
#92570 = CARTESIAN_POINT ( 'NONE',  ( 6.317736394288131052, 9.354147645769410602, 1.082531754730558626 ) ) ;
#92571 = CARTESIAN_POINT ( 'NONE',  ( -8.744645890690007306, 12.18554205823825498, 1.082531754730558626 ) ) ;
#92572 = CARTESIAN_POINT ( 'NONE',  ( 7.363486825997814123, 7.763358516518489516, 0.000000000000000000 ) ) ;
#92573 = AXIS2_PLACEMENT_3D ( 'NONE', #160121, #11722, #144972 ) ;
#92574 = CARTESIAN_POINT ( 'NONE',  ( 0.2642963535325442703, 1.880433764241522088, -0.7283817610406128074 ) ) ;
#92576 = CARTESIAN_POINT ( 'NONE',  ( 5.705554990011762584, -1.623920158085298437, -1.271698733341574350 ) ) ;
#92575 = CARTESIAN_POINT ( 'NONE',  ( 9.402743226277308963, 10.92862083786708816, -1.199719254218446718 ) ) ;
#92577 = DIRECTION ( 'NONE',  ( 0.000000000000000000, -0.000000000000000000, 1.000000000000000000 ) ) ;
#92578 = CARTESIAN_POINT ( 'NONE',  ( -4.464712657601869417, 4.103252943490596216, 0.7998128361456341429 ) ) ;
#92579 = CARTESIAN_POINT ( 'NONE',  ( 5.844973620822823790, 9.833236634353070826, 0.7216878364870317197 ) ) ;
#92580 = CARTESIAN_POINT ( 'NONE',  ( 3.023105066167310895, 5.702484939155337607, -2.499999999999995115 ) ) ;
#92581 = CARTESIAN_POINT ( 'NONE',  ( 1.364683531249986537, 1.113541667008082658, 0.7879004041258500513 ) ) ;
#92582 = CARTESIAN_POINT ( 'NONE',  ( 0.6668358675281795822, 0.1816249057532189626, -1.760414781625377234 ) ) ;
#92583 = CARTESIAN_POINT ( 'NONE',  ( 0.1236729436712938751, 0.3474707636354073537, 1.986100063511665237 ) ) ;
#92584 = CARTESIAN_POINT ( 'NONE',  ( 6.163578228761874556, 0.9028020746227163329, 1.487850569839582970 ) ) ;
#92585 = CARTESIAN_POINT ( 'NONE',  ( 3.439304851068147428, -1.736875716534720615, -1.496195766483783274 ) ) ;
#92586 = CARTESIAN_POINT ( 'NONE',  ( 1.364683531249988757, 0.1343750003414204142, 0.000000000000000000 ) ) ;
#92587 = CARTESIAN_POINT ( 'NONE',  ( 1.956743257466783570, 0.3155556147324266036, -1.813728304320901596 ) ) ;
#92588 = CARTESIAN_POINT ( 'NONE',  ( 8.238550898598388628, 12.76339314834017102, 0.7998128361456462443 ) ) ;
#92589 = CARTESIAN_POINT ( 'NONE',  ( -10.47657863273387058, 4.460721775326359939, 5.863621068794715896 ) ) ;
#92590 = CARTESIAN_POINT ( 'NONE',  ( 2.994927033977520470, 1.566606242385214731, -0.9370212210159312161 ) ) ;
#92591 = CARTESIAN_POINT ( 'NONE',  ( 3.445935549842124690, -1.779626424299302956, -0.9480406757386842242 ) ) ;
#92592 = CARTESIAN_POINT ( 'NONE',  ( -9.854078719034067291, 10.39084668182823634, 0.7998128361456462443 ) ) ;
#92593 = CARTESIAN_POINT ( 'NONE',  ( 0.000000000000000000, -0.2000000000000057288, 0.000000000000000000 ) ) ;
#92594 = CARTESIAN_POINT ( 'NONE',  ( 5.913134528375765697, 1.855721070963678443, 0.9956851948400150532 ) ) ;
#92595 = CARTESIAN_POINT ( 'NONE',  ( 10.03397232106342862, 14.16760128048179723, 7.472996930959428852 ) ) ;
#92596 = CARTESIAN_POINT ( 'NONE',  ( 2.348173244826061268, -0.8873571809006628452, 1.870714752860686447 ) ) ;
#92597 = CARTESIAN_POINT ( 'NONE',  ( 5.379888026524302980, 5.170957540566797128, -0.7998128361456211532 ) ) ;
#92598 = CARTESIAN_POINT ( 'NONE',  ( -4.957638175832625493E-14, 0.8593750003414141192, -1.570758158831808249 ) ) ;
#92599 = CARTESIAN_POINT ( 'NONE',  ( 4.951869195850400196, -1.499954228463634243, -1.499123153458590707 ) ) ;
#92600 = CARTESIAN_POINT ( 'NONE',  ( 0.4340449649811276012, 0.9916047912509761142, -1.651568591070247116 ) ) ;
#92601 = CARTESIAN_POINT ( 'NONE',  ( -3.644109427023046521, 7.473487774827342278, 0.000000000000000000 ) ) ;
#92602 = CARTESIAN_POINT ( 'NONE',  ( 8.259941899223605333, 10.65968485389279508, -1.599625672291268286 ) ) ;
#92603 = CARTESIAN_POINT ( 'NONE',  ( 5.275531169048895741, 7.248148678680751189, -1.443375672974078761 ) ) ;
#92604 = CARTESIAN_POINT ( 'NONE',  ( 1.001543065824772753E-15, -0.5687499990440827435, 4.012584370867899430 ) ) ;
#92605 = CARTESIAN_POINT ( 'NONE',  ( -6.240830780992103755, 6.175390754112560110, 1.040834085586084257E-14 ) ) ;
#92606 = CARTESIAN_POINT ( 'NONE',  ( -0.1750823283547575382, -0.9565501389544858180, -2.002587789130043205 ) ) ;
#92607 = CARTESIAN_POINT ( 'NONE',  ( 2.292140615954643579, -0.9012634372634602542, 1.903512165690796065 ) ) ;
#92608 = CARTESIAN_POINT ( 'NONE',  ( -6.154475385960665790, 6.144919136567696505, 0.000000000000000000 ) ) ;
#92609 = CARTESIAN_POINT ( 'NONE',  ( 7.052212457402625922, 11.37933163361175382, -0.7998128361456291469 ) ) ;
#92610 = CARTESIAN_POINT ( 'NONE',  ( 6.807467476049567701, -1.494282888040651347, -1.108890849153229441 ) ) ;
#92611 = CARTESIAN_POINT ( 'NONE',  ( 8.046927864910717432, 9.346836249606042202, 1.199719254218462483 ) ) ;
#92612 = DIRECTION ( 'NONE',  ( 0.000000000000000000, 0.000000000000000000, -1.000000000000000000 ) ) ;
#92613 = ORIENTED_EDGE ( 'NONE', *, *, #119894, .T. ) ;
#92614 = CARTESIAN_POINT ( 'NONE',  ( -3.363304624641834106, 6.081549941127532222, -1.199719254218452047 ) ) ;
#92616 = CARTESIAN_POINT ( 'NONE',  ( -8.758204044748012507, 11.24099069033793974, 1.443375672974064550 ) ) ;
#92615 = AXIS2_PLACEMENT_3D ( 'NONE', #61689, #193808, #100586 ) ;
#92617 = CARTESIAN_POINT ( 'NONE',  ( 0.4223351350958382544, -2.109807164369668087, 0.2139620856976830743 ) ) ;
#92618 = DIRECTION ( 'NONE',  ( -5.578564026256490882E-16, -1.000000000000000000, -9.066213480720158442E-32 ) ) ;
#92620 = CARTESIAN_POINT ( 'NONE',  ( 3.789464544343919883, -1.813617537123424661, 0.7486148740368094856 ) ) ;
#92619 = CARTESIAN_POINT ( 'NONE',  ( -1.225000000000007416, -0.5000000000000004441, -1.734723475976807094E-15 ) ) ;
#92621 = CARTESIAN_POINT ( 'NONE',  ( 1.463986924769441478, 2.129665692569195024, -0.3698555562515608020 ) ) ;
#92623 = CARTESIAN_POINT ( 'NONE',  ( -5.958637689794747949, 6.108898536480521280, 0.7553493914738591553 ) ) ;
#92622 = CARTESIAN_POINT ( 'NONE',  ( -3.461074353238556167, 7.259946855412102273, 0.000000000000000000 ) ) ;
#92624 = CARTESIAN_POINT ( 'NONE',  ( -1.364683531250000748, 1.259375000341421469, 0.000000000000000000 ) ) ;
#92625 = CARTESIAN_POINT ( 'NONE',  ( 2.624636096055412704, -1.623921194558699765, 0.6262662122848341451 ) ) ;
#92626 = CARTESIAN_POINT ( 'NONE',  ( 5.341549334104184865, 8.215262742221458581, 1.082531754730558626 ) ) ;
#92627 = CARTESIAN_POINT ( 'NONE',  ( -12.36958382383909871, 9.653479897959526213, -1.396270995789667513 ) ) ;
#92629 = ADVANCED_FACE ( 'NONE', ( #155013 ), #39717, .T. ) ;
#92628 = CIRCLE ( 'NONE', #64903, 11.92000000000000171 ) ;
#92630 = CARTESIAN_POINT ( 'NONE',  ( 2.583361055862750000, 1.319027862724517552, -1.524809160041600498 ) ) ;
#92631 = CARTESIAN_POINT ( 'NONE',  ( 6.825078400183551608, 4.689370880799383912, 2.706890346843467299 ) ) ;
#92632 = CARTESIAN_POINT ( 'NONE',  ( -5.320648938720212051, 5.172121614787156929, 0.000000000000000000 ) ) ;
#92633 = CARTESIAN_POINT ( 'NONE',  ( 1.850399468497238242, 0.6164509289473228959, 1.872685729773468255 ) ) ;
#92635 = CARTESIAN_POINT ( 'NONE',  ( -6.943184063974186415, 7.273005294157565359, -0.7216878364870338292 ) ) ;
#92634 = CARTESIAN_POINT ( 'NONE',  ( 6.099862406061942188, 1.323743610676546334, 1.380425988546908567 ) ) ;
#92636 = CARTESIAN_POINT ( 'NONE',  ( -4.597623488365601752, 8.377994813152914944, 0.7216878364870267237 ) ) ;
#92637 = CARTESIAN_POINT ( 'NONE',  ( 4.538947565524982686, 8.517465603079630299, 0.000000000000000000 ) ) ;
#92638 = CARTESIAN_POINT ( 'NONE',  ( -5.818384198920079520, 6.817144982608731141, 1.199719254218452935 ) ) ;
#92639 = CARTESIAN_POINT ( 'NONE',  ( 0.6276103948988649428, -0.2939658443398012744, 1.998026100167526575 ) ) ;
#92640 = CARTESIAN_POINT ( 'NONE',  ( 5.965930945686983122, 2.274828880937030728, -0.3866611637039600313 ) ) ;
#92641 = CARTESIAN_POINT ( 'NONE',  ( 5.617619635959271385, 0.3843197845415853853, -1.923678648292715732 ) ) ;
#92642 = ADVANCED_FACE ( 'NONE', ( #173415 ), #68772, .F. ) ;
#92643 = CARTESIAN_POINT ( 'NONE',  ( 3.291801117278610800, -1.314073873198824627, -1.456807609480186061 ) ) ;
#92644 = CARTESIAN_POINT ( 'NONE',  ( 8.235688245297327015, 11.69572115523387268, -1.199719254218446718 ) ) ;
#92645 = CARTESIAN_POINT ( 'NONE',  ( 1.160779977835691312, 1.203355533934968635, 1.617816888933524710 ) ) ;
#92646 = ORIENTED_EDGE ( 'NONE', *, *, #203174, .F. ) ;
#92647 = CARTESIAN_POINT ( 'NONE',  ( 0.7259617406208430657, 0.8522569803141609723, -1.938411259892757421 ) ) ;
#92649 = CARTESIAN_POINT ( 'NONE',  ( -5.181187258716735577, 9.196468901811520880, 0.7998128361456481317 ) ) ;
#92648 = CARTESIAN_POINT ( 'NONE',  ( -3.867100128395853709, 5.534702787927018974, -1.599625672291256295 ) ) ;
#92650 = CARTESIAN_POINT ( 'NONE',  ( 1.657894046870052485, -1.302874822933766774, 1.301145727299134025 ) ) ;
#92651 = ORIENTED_EDGE ( 'NONE', *, *, #39389, .F. ) ;
#92652 = CARTESIAN_POINT ( 'NONE',  ( 11.52487297331679095, 8.447199575603240973, 3.365429268895913761 ) ) ;
#92653 = CARTESIAN_POINT ( 'NONE',  ( 3.463236921083117981, -1.731491641549892435, 1.224000437801611163 ) ) ;
#92654 = CARTESIAN_POINT ( 'NONE',  ( -1.201851678989727383E-14, 4.868750000682822154, -1.732050807568863648 ) ) ;
#92655 = CARTESIAN_POINT ( 'NONE',  ( 6.401421083946654100, 10.62007503124645957, -0.7998128361456291469 ) ) ;
#92656 = CARTESIAN_POINT ( 'NONE',  ( 5.352436782344940802, 9.466536356036257871, 0.000000000000000000 ) ) ;
#92657 = CARTESIAN_POINT ( 'NONE',  ( 4.815729912100211507, -2.021797975182148654, 0.3980178507551126454 ) ) ;
#92659 = CARTESIAN_POINT ( 'NONE',  ( 1.610644152589552958, -0.2245515952020246675, 1.827417025815617935 ) ) ;
#92658 = CARTESIAN_POINT ( 'NONE',  ( -8.362681821530818738, 8.650883634741092010, -0.7998128361456291469 ) ) ;
#92660 = CARTESIAN_POINT ( 'NONE',  ( 1.364683531249990311, 4.634375000341417916, 1.214306433183764966E-14 ) ) ;
#92661 = FACE_OUTER_BOUND ( 'NONE', #67358, .T. ) ;
#92662 = CARTESIAN_POINT ( 'NONE',  ( -11.89197369110779867, 13.80000000000000249, 0.8056055387119849254 ) ) ;
#92663 = CARTESIAN_POINT ( 'NONE',  ( 1.207977004800918852, -0.5332226995428279714, 2.141375170867452660 ) ) ;
#92664 = CARTESIAN_POINT ( 'NONE',  ( 2.161739655719534081, 0.3883039046224411317, -2.228698702525088393 ) ) ;
#92665 = CARTESIAN_POINT ( 'NONE',  ( -8.893785580884703279, 10.43879993486270585, 1.082531754730558626 ) ) ;
#92666 = CARTESIAN_POINT ( 'NONE',  ( 2.496125854487367235, -0.9279945471987390837, 1.555666070890851627 ) ) ;
#92667 = CARTESIAN_POINT ( 'NONE',  ( 2.887788952342277948, -1.913322710806207194, 0.09880452340514658816 ) ) ;
#92668 = CARTESIAN_POINT ( 'NONE',  ( 3.684089399883890614, -1.230936008959164996, -1.664559344884769088 ) ) ;
#92669 = CARTESIAN_POINT ( 'NONE',  ( 1.364683531249988757, 2.446875000341415696, 1.214306433183764966E-14 ) ) ;
#92670 = CARTESIAN_POINT ( 'NONE',  ( 2.834795904189919558, 0.2398841137210059038, 1.956746676604983248 ) ) ;
#92671 = CARTESIAN_POINT ( 'NONE',  ( 6.234985708453399944, 0.1916802727454213762, 1.916943350541326030 ) ) ;
#92672 = CARTESIAN_POINT ( 'NONE',  ( 4.170664822833985319, -1.745344833062393075, -0.6735866001992969476 ) ) ;
#92674 = CARTESIAN_POINT ( 'NONE',  ( 4.598366155629488361, 8.485928551783258555, 0.1149073004905968448 ) ) ;
#92673 = CARTESIAN_POINT ( 'NONE',  ( 2.086955060466778811, -2.263696646927360501, -0.4477047476570076290 ) ) ;
#92675 = CARTESIAN_POINT ( 'NONE',  ( 3.349909636924102596, -0.7564274094383013347, 1.700591413421480125 ) ) ;
#92676 = CARTESIAN_POINT ( 'NONE',  ( -1.001543065824772872E-14, 4.321875000341417916, 1.575800808251672791 ) ) ;
#92677 = CARTESIAN_POINT ( 'NONE',  ( -5.122283107864663343, 4.870418468797203637, 0.000000000000000000 ) ) ;
#92678 = CARTESIAN_POINT ( 'NONE',  ( 5.774883364416965037, 8.824782127540085952, -1.199719254218440723 ) ) ;
#92679 = CARTESIAN_POINT ( 'NONE',  ( 11.07790593930098311, 9.799999999999998934, 0.6999999999999992895 ) ) ;
#92680 = CARTESIAN_POINT ( 'NONE',  ( 0.5046868689226053917, -0.7117215327378585421, -1.982300686916990573 ) ) ;
#92681 = CARTESIAN_POINT ( 'NONE',  ( -0.6823417656250212460, 4.113541667008085767, 1.181850606188767472 ) ) ;
#92682 = CARTESIAN_POINT ( 'NONE',  ( 6.485629946217342123, 1.485420011660616879, 1.570608065930901187 ) ) ;
#92683 = CARTESIAN_POINT ( 'NONE',  ( 0.1233147457768641181, 1.759488896278412540, 0.9916404401272023161 ) ) ;
#92684 = CARTESIAN_POINT ( 'NONE',  ( -1.402160292154681736E-14, -0.5531249996585814177, -1.575800808251665908 ) ) ;
#92685 = CARTESIAN_POINT ( 'NONE',  ( -3.633221978782283923, 7.182583375313884133, -0.7216878364870267237 ) ) ;
#92686 = ADVANCED_FACE ( 'NONE', ( #92174 ), #75763, .T. ) ;
#92689 = CARTESIAN_POINT ( 'NONE',  ( 4.392478581147586603, 4.226905887534702977, -0.7216878364870188411 ) ) ;
#92688 = CARTESIAN_POINT ( 'NONE',  ( 6.925078400183547700, 0.5992389604297322370, 1.809181922849491198 ) ) ;
#92687 = CARTESIAN_POINT ( 'NONE',  ( 5.040599249230596435, 9.102725900736217568, 0.7998128361456341429 ) ) ;
#92690 = CARTESIAN_POINT ( 'NONE',  ( -3.871735385154307263, 6.674719161725423788, -1.199719254218450271 ) ) ;
#92691 = CARTESIAN_POINT ( 'NONE',  ( 4.540250091716044878, 0.7762272601403925609, 1.861345588084816871 ) ) ;
#92693 = CARTESIAN_POINT ( 'NONE',  ( -6.983858524370814003, 9.241197259889665006, 1.443375672974064550 ) ) ;
#92692 = CARTESIAN_POINT ( 'NONE',  ( -8.758204044748012507, 11.24099069033793974, 1.443375672974064550 ) ) ;
#92694 = SURFACE_STYLE_USAGE ( .BOTH. , #141469 ) ;
#92696 = CARTESIAN_POINT ( 'NONE',  ( 1.364683531249997417, 11.23437500034139802, 2.602085213965210642E-15 ) ) ;
#92695 = CARTESIAN_POINT ( 'NONE',  ( 5.998930166150279852, 1.769978137569449883, -1.240765152474863520 ) ) ;
#92697 = CARTESIAN_POINT ( 'NONE',  ( -11.01453822196416077, 5.351648037286913073, 4.768917646641087416 ) ) ;
#92699 = CARTESIAN_POINT ( 'NONE',  ( 6.204703874486805049, 1.882480396761162744, 0.7231267579426368108 ) ) ;
#92698 = CARTESIAN_POINT ( 'NONE',  ( -6.521108698048779573, 8.631046119188804155, -1.443375672974058777 ) ) ;
#92700 = CARTESIAN_POINT ( 'NONE',  ( -1.364683531250014514, 1.301041667008083325, -0.7879004041258289570 ) ) ;
#92701 = CARTESIAN_POINT ( 'NONE',  ( 0.4382560683119198774, -5.200000000000008171, 10.99126615174921007 ) ) ;
#92702 = CARTESIAN_POINT ( 'NONE',  ( 0.7500000000000006661, 8.833333333333332149, 1.299038105676657340 ) ) ;
#92703 = CARTESIAN_POINT ( 'NONE',  ( 2.806937704738516448, 1.457146550840708210, 0.9226662414157487113 ) ) ;
#92704 = CARTESIAN_POINT ( 'NONE',  ( 6.156284269057003655, 9.340026192945279249, -1.199719254218452047 ) ) ;
#92705 = CARTESIAN_POINT ( 'NONE',  ( 5.529746549527311039, 7.544733289238903851, -1.599625672291281386 ) ) ;
#92706 = CARTESIAN_POINT ( 'NONE',  ( 1.364683531249988757, -0.5531249996585801965, 0.000000000000000000 ) ) ;
#92707 = CARTESIAN_POINT ( 'NONE',  ( 0.8425835904034431056, -1.521979116790536768, 0.9028166612478020214 ) ) ;
#92708 = CARTESIAN_POINT ( 'NONE',  ( 2.420566579892877268, -0.7724838186086988578, -1.859170112617714699 ) ) ;
#92709 = CARTESIAN_POINT ( 'NONE',  ( 2.345197385039651472, 5.679888015947478941, -0.7216878364870267237 ) ) ;
#92710 = CARTESIAN_POINT ( 'NONE',  ( 4.665167916288286420, -1.969490514480085164, -0.9956290437203789701 ) ) ;
#92711 = AXIS2_PLACEMENT_3D ( 'NONE', #137791, #201674, #55456 ) ;
#92712 = CARTESIAN_POINT ( 'NONE',  ( 4.873980352634836422, -2.130485078384927178, 0.4170503277054308788 ) ) ;
#92713 = ORIENTED_EDGE ( 'NONE', *, *, #44262, .T. ) ;
#92714 = CARTESIAN_POINT ( 'NONE',  ( 2.898410978271408922, 6.603506251283770112, -0.7998128361456362523 ) ) ;
#92715 = CARTESIAN_POINT ( 'NONE',  ( 7.226132685959389512, 11.37431253368722750, -0.7216878364870267237 ) ) ;
#92717 = CARTESIAN_POINT ( 'NONE',  ( 2.372672929649359386, -0.3474902101525711995, -1.986097784353996643 ) ) ;
#92716 = CARTESIAN_POINT ( 'NONE',  ( 2.772263606761758759, 2.110060413066455975, -0.2101530891244970389 ) ) ;
#92719 = ORIENTED_EDGE ( 'NONE', *, *, #185325, .F. ) ;
#92718 = CARTESIAN_POINT ( 'NONE',  ( 3.515680188161012687, -0.5209108127710823100, 1.735096886039680930 ) ) ;
#92720 = CARTESIAN_POINT ( 'NONE',  ( 6.170896192875352959, 7.228408975556602556, 1.199719254218453823 ) ) ;
#92721 = ORIENTED_EDGE ( 'NONE', *, *, #160495, .F. ) ;
#92722 = CARTESIAN_POINT ( 'NONE',  ( 0.8306673739700667358, 0.1335802410974036292, 1.865940672528036304 ) ) ;
#92723 = CARTESIAN_POINT ( 'NONE',  ( 5.725187622324654946, -0.04035785615889506128, 1.825416780793003069 ) ) ;
#92725 = CARTESIAN_POINT ( 'NONE',  ( 1.551812156574260637, 0.9880582627100834570, 1.641127140810652252 ) ) ;
#92724 = PLANE ( 'NONE',  #112453 ) ;
#92727 = CIRCLE ( 'NONE', #123875, 8.500000000000000000 ) ;
#92726 = CIRCLE ( 'NONE', #26963, 8.049999999999993605 ) ;
#92728 = CARTESIAN_POINT ( 'NONE',  ( 0.6823417656249899377, 1.905208333674752952, 1.181850606188755259 ) ) ;
#92729 = DIRECTION ( 'NONE',  ( 0.000000000000000000, 1.000000000000000000, 0.000000000000000000 ) ) ;
#92730 = ADVANCED_FACE ( 'NONE', ( #93236 ), #145199, .T. ) ;
#92731 = CARTESIAN_POINT ( 'NONE',  ( 6.048345925472166762, 10.07050432311064903, 0.7216878364870317197 ) ) ;
#92732 = CARTESIAN_POINT ( 'NONE',  ( -5.966997003790232235, 7.094489604910957148, -1.082531754730549967 ) ) ;
#92733 = CARTESIAN_POINT ( 'NONE',  ( -7.923814432544069142, 8.209148024248356990, 0.000000000000000000 ) ) ;
#92734 = CARTESIAN_POINT ( 'NONE',  ( 3.146849984228027974, 2.069795010335002239, 0.4607391970517027979 ) ) ;
#92736 = CARTESIAN_POINT ( 'NONE',  ( -10.45142907045522129, 5.144535043903895932, -5.216774619840575333 ) ) ;
#92735 = CARTESIAN_POINT ( 'NONE',  ( -1.500000000000016209, 5.670833333333358262, 0.8660254037844375974 ) ) ;
#92737 = CARTESIAN_POINT ( 'NONE',  ( 4.973880039175529788, 1.132619354422999436, 1.613344424267410204 ) ) ;
#92738 = CARTESIAN_POINT ( 'NONE',  ( 6.117437049485344502, 1.593764408019750389, 1.056661447057717362 ) ) ;
#92739 = VERTEX_POINT ( 'NONE', #46605 ) ;
#92740 = CARTESIAN_POINT ( 'NONE',  ( -0.0001774970986804374768, -2.075397304607224047, 0.4179963677126071753 ) ) ;
#92742 = ADVANCED_FACE ( 'NONE', ( #213328 ), #9346, .T. ) ;
#92741 = FACE_OUTER_BOUND ( 'NONE', #187431, .T. ) ;
#92743 = CARTESIAN_POINT ( 'NONE',  ( 2.066927875543830950, 1.535623996113824496, -1.388825173883188713 ) ) ;
#92744 = CARTESIAN_POINT ( 'NONE',  ( 2.712754350931959380, -0.1900897480172674958, 1.932619341894822540 ) ) ;
#92745 = VERTEX_POINT ( 'NONE', #29279 ) ;
#92746 = CARTESIAN_POINT ( 'NONE',  ( 4.193214648376505593, 8.114110533073061404, 0.000000000000000000 ) ) ;
#92747 = CARTESIAN_POINT ( 'NONE',  ( 7.049313524462606395, 7.188896964819984525, 0.000000000000000000 ) ) ;
#92749 = CARTESIAN_POINT ( 'NONE',  ( 6.114890974963323345, 7.092793211334054604, 1.199719254218462483 ) ) ;
#92748 = CARTESIAN_POINT ( 'NONE',  ( 3.468770583794348550, 0.05092928562340763576, -2.090184462658881248 ) ) ;
#92750 = CARTESIAN_POINT ( 'NONE',  ( 3.838366886000300404, 6.531826229425389485, -1.082531754730548412 ) ) ;
#92752 = ORIENTED_EDGE ( 'NONE', *, *, #29804, .T. ) ;
#92751 = CARTESIAN_POINT ( 'NONE',  ( 0.8206315121990900296, 1.372318096965993384, -1.182507040619881877 ) ) ;
#92753 = CARTESIAN_POINT ( 'NONE',  ( 5.233140740401229785, 0.1595256157847015632, 2.201181388321731713 ) ) ;
#92754 = DIRECTION ( 'NONE',  ( 0.7592566023653005702, -0.6507913734559639396, 0.000000000000000000 ) ) ;
#92755 = CARTESIAN_POINT ( 'NONE',  ( 3.364504783244476993, 0.9904720576699842516, 1.972067388187691339 ) ) ;
#92756 = CARTESIAN_POINT ( 'NONE',  ( 8.782984583554449998, 9.141236857102018831, 1.040834085586084257E-14 ) ) ;
#92757 = CARTESIAN_POINT ( 'NONE',  ( -3.231779075379147770, 6.036511184309971689, 2.420000000000000373 ) ) ;
#92758 = CARTESIAN_POINT ( 'NONE',  ( 1.980978873585538480, -1.748965405663160944, -0.7736543689686598002 ) ) ;
#92759 = CIRCLE ( 'NONE', #213763, 11.95586206894156689 ) ;
#92760 = CARTESIAN_POINT ( 'NONE',  ( 8.585337585951586803, 11.03931315507545108, -1.599625672291255185 ) ) ;
#92761 = CARTESIAN_POINT ( 'NONE',  ( 5.002425025097493538, 2.064580399062130311, 0.1557331365308264881 ) ) ;
#92763 = CARTESIAN_POINT ( 'NONE',  ( 3.221700144506876917, -2.083771231579465866, 0.5749860669421112958 ) ) ;
#92762 = CARTESIAN_POINT ( 'NONE',  ( 0.000000000000000000, 0.06547992991065912372, 0.000000000000000000 ) ) ;
#92764 = CARTESIAN_POINT ( 'NONE',  ( 4.652002595327206613, 0.8389548150543740812, 2.024815518666116088 ) ) ;
#92765 = ORIENTED_EDGE ( 'NONE', *, *, #85587, .F. ) ;
#92766 = CARTESIAN_POINT ( 'NONE',  ( -0.1296875068448159751, 0.001480089298542403009, -1.826395826379861864 ) ) ;
#92767 = AXIS2_PLACEMENT_3D ( 'NONE', #44000, #93825, #89551 ) ;
#92768 = CARTESIAN_POINT ( 'NONE',  ( 0.9311234436981512541, -1.853130369558481538, -3.475000000000000977 ) ) ;
#92769 = DIRECTION ( 'NONE',  ( 1.000000000000000000, 0.000000000000000000, 0.000000000000000000 ) ) ;
#92770 = CARTESIAN_POINT ( 'NONE',  ( 5.273195401072370281, 5.116759154198018855, -0.7998128361456481317 ) ) ;
#92771 = CARTESIAN_POINT ( 'NONE',  ( 0.6823417656249969321, 15.33854166700806410, -1.181850606188757036 ) ) ;
#92772 = DIRECTION ( 'NONE',  ( -1.000000000000000000, 0.000000000000000000, 0.000000000000000000 ) ) ;
#92773 = EDGE_CURVE ( 'NONE', #181560, #203057, #98634, .T. ) ;
#92774 = CARTESIAN_POINT ( 'NONE',  ( -7.361714222540411967, 11.53249099303175385, 0.000000000000000000 ) ) ;
#92775 = CARTESIAN_POINT ( 'NONE',  ( 5.550083779947807550, 7.568460058062819407, -1.599625672291283607 ) ) ;
#92776 = CARTESIAN_POINT ( 'NONE',  ( 5.893440691016273547, -1.874049447596724427, 0.8799615681738190975 ) ) ;
#92777 = CARTESIAN_POINT ( 'NONE',  ( 3.984924265943972532, -0.1901312170250069600, -1.917098255223735004 ) ) ;
#92778 = CARTESIAN_POINT ( 'NONE',  ( 0.2984541275833849094, 1.388471424577278235, -1.462460896543740674 ) ) ;
#92779 = CARTESIAN_POINT ( 'NONE',  ( 4.150767584078112193, 7.994312614733129152, 0.7998128361456321445 ) ) ;
#92780 = DIRECTION ( 'NONE',  ( -1.000000000000000000, 0.000000000000000000, 0.000000000000000000 ) ) ;
#92781 = CARTESIAN_POINT ( 'NONE',  ( 5.032068834786890044, 1.130672129898707245, 1.612349476345806831 ) ) ;
#92782 = CARTESIAN_POINT ( 'NONE',  ( 0.3401085955914601722, 2.185883683461706362, 0.1570275565265024931 ) ) ;
#92783 = CARTESIAN_POINT ( 'NONE',  ( 5.145057536039753465, -1.563975785779356587, 0.9416349707431560523 ) ) ;
#92784 = CARTESIAN_POINT ( 'NONE',  ( 7.838022202476093270, 8.316983122409855156, 0.7216878364870267237 ) ) ;
#92785 = CARTESIAN_POINT ( 'NONE',  ( 3.131570294632282092, 5.636953862837537521, -1.082531754730543971 ) ) ;
#92786 = CARTESIAN_POINT ( 'NONE',  ( -6.791708605802965870, 6.888357893050385705, -0.7998128361456362523 ) ) ;
#92787 = CARTESIAN_POINT ( 'NONE',  ( 4.044074958626150185, 7.940114228364351767, 0.7998128361456271485 ) ) ;
#92788 = ORIENTED_EDGE ( 'NONE', *, *, #30754, .T. ) ;
#92790 = CARTESIAN_POINT ( 'NONE',  ( 5.853776559028295523, -1.461190594579380608, -1.385140169207878413 ) ) ;
#92789 = CARTESIAN_POINT ( 'NONE',  ( 2.331387312403776946, 0.8663521307504215008, -1.624669977836174839 ) ) ;
#92791 = CARTESIAN_POINT ( 'NONE',  ( 1.212782571277282395, -1.812964642495185963, -1.412582873482233659 ) ) ;
#92792 = CARTESIAN_POINT ( 'NONE',  ( 5.102378460580520247, 1.956245014681293970, 0.1482201060269832671 ) ) ;
#92793 = CARTESIAN_POINT ( 'NONE',  ( -6.501298352952815662, 7.543601818988450169, -1.199719254218446718 ) ) ;
#92794 = CARTESIAN_POINT ( 'NONE',  ( -6.796206128891405740, -7.030236945366977075, 6.776587425048123059 ) ) ;
#92795 = CARTESIAN_POINT ( 'NONE',  ( -4.471491734408701291, 4.111161866431900513, 1.214306433183764966E-14 ) ) ;
#92796 = CARTESIAN_POINT ( 'NONE',  ( 0.8189040078958352842, -1.500748464528355974, 1.426492703164506937 ) ) ;
#92797 = CARTESIAN_POINT ( 'NONE',  ( -5.418418667316934112, 6.350518529071726981, -1.199719254218453823 ) ) ;
#92799 = CARTESIAN_POINT ( 'NONE',  ( 6.614108672291515667, -0.8387186360741160085, -1.558468296174354784 ) ) ;
#92798 = CARTESIAN_POINT ( 'NONE',  ( 1.839510613029649466, 0.7972044211956804682, -1.932997742640076400 ) ) ;
#92800 = CARTESIAN_POINT ( 'NONE',  ( 0.3584499564876124644, 8.158857887133999398, -1.968348077346313341 ) ) ;
#92801 = CARTESIAN_POINT ( 'NONE',  ( -15.75000000000000000, 13.39999999999998259, 3.599999999999999201 ) ) ;
#92802 = CARTESIAN_POINT ( 'NONE',  ( 1.733560280482333571, 1.721479560191770730, 0.2551580012965410371 ) ) ;
#92803 =( GEOMETRIC_REPRESENTATION_CONTEXT ( 3 ) GLOBAL_UNCERTAINTY_ASSIGNED_CONTEXT ( ( #99231 ) ) GLOBAL_UNIT_ASSIGNED_CONTEXT ( ( #194148, #40723, #145458 ) ) REPRESENTATION_CONTEXT ( 'NONE', 'WORKASPACE' ) );
#92804 = CARTESIAN_POINT ( 'NONE',  ( 4.364835388595708743, 7.179726155748598515, 1.199719254218462483 ) ) ;
#92806 = CARTESIAN_POINT ( 'NONE',  ( 1.543281805264333117, 8.695372333414642441, 2.508924166024208979 ) ) ;
#92805 = CARTESIAN_POINT ( 'NONE',  ( -11.41381675112453387, 13.40000000000000036, -3.704697986577184299 ) ) ;
#92807 = CARTESIAN_POINT ( 'NONE',  ( 2.349869733406087402, 1.724505987646451688, 0.04327962033413671611 ) ) ;
#92808 = COLOUR_RGB ( '', 0.31764706, 0.68627451, 0.89019608) ;
#92809 = CARTESIAN_POINT ( 'NONE',  ( 2.525153347276567484, -2.043736813514348771, 0.7916865192442237298 ) ) ;
#92810 = CARTESIAN_POINT ( 'NONE',  ( 5.074942902252104204, -2.077123540546990110, -0.7459609299403434646 ) ) ;
#92811 = CARTESIAN_POINT ( 'NONE',  ( -10.19200560444942560, 4.477620260464512114, -5.707107691925500603 ) ) ;
#92812 = CARTESIAN_POINT ( 'NONE',  ( 2.184662588793543136, 1.252765144364040850, -1.772974741507940211 ) ) ;
#92813 = CARTESIAN_POINT ( 'NONE',  ( 1.629252094361890890, -1.719607636260962025, 0.6136192449261099746 ) ) ;
#92814 = CARTESIAN_POINT ( 'NONE',  ( 3.503210936237437068, -0.1516218309994079028, 2.111938774394610974 ) ) ;
#92815 = CARTESIAN_POINT ( 'NONE',  ( 1.220146605508150803E-14, 9.718750000682797818, -1.499999999999998446 ) ) ;
#92816 = ORIENTED_EDGE ( 'NONE', *, *, #34246, .T. ) ;
#92818 = CARTESIAN_POINT ( 'NONE',  ( -1.364683531250014514, 1.801041667008085767, -0.7879004041258289570 ) ) ;
#92817 = CARTESIAN_POINT ( 'NONE',  ( 3.913864042289341150, -1.178888685321772156, -1.965896434285055117 ) ) ;
#92819 = CARTESIAN_POINT ( 'NONE',  ( -1.326716514427061987E-15, 2.999999999999988454, -1.225000000000003864 ) ) ;
#92820 = CARTESIAN_POINT ( 'NONE',  ( 5.379888026524302980, 5.170957540566797128, -0.7998128361456211532 ) ) ;
#92821 = CARTESIAN_POINT ( 'NONE',  ( 6.305373609846285810, 1.934184411435871498, -1.092212275460135773 ) ) ;
#92822 = CARTESIAN_POINT ( 'NONE',  ( -6.561783159334141580, 7.718130443053708767, -1.082531754730544860 ) ) ;
#92823 = CARTESIAN_POINT ( 'NONE',  ( 3.063779527008304360, 6.518233848244248563, 0.7216878364870317197 ) ) ;
#92824 = CARTESIAN_POINT ( 'NONE',  ( -6.277061933002790362, 8.346324893301817482, 1.443375672974078761 ) ) ;
#92825 =( BOUNDED_SURFACE ( )  B_SPLINE_SURFACE ( 3, 2, ( 
 ( #81040, #128803, #193717 ),
 ( #194785, #176419, #13886 ),
 ( #32293, #64782, #28026 ),
 ( #162301, #97309, #211020 ),
 ( #46421, #143958, #62644 ),
 ( #213152, #127761, #94124 ),
 ( #212082, #142886, #160162 ),
 ( #98359, #130923, #164424 ) ),
 .UNSPECIFIED., .F., .F., .T. ) 
 B_SPLINE_SURFACE_WITH_KNOTS ( ( 4, 2, 2, 4 ),
 ( 3, 3 ),
 ( 0.000000000000000000, 0.0004924884914732687849, 0.0007387327372099031231, 0.0009849769829465375697 ),
 ( 0.000000000000000000, 1.000000000000000000 ),
 .UNSPECIFIED. ) 
 GEOMETRIC_REPRESENTATION_ITEM ( )  RATIONAL_B_SPLINE_SURFACE ( (
 ( 1.000000000000000000, 0.7045118851637608426, 1.000000000000000000),
 ( 1.000000000000000000, 0.7593505504064975709, 1.000000000000000000),
 ( 1.000000000000000000, 0.8104906253032382324, 1.000000000000000000),
 ( 1.000000000000000000, 0.8722646935501497945, 1.000000000000000000),
 ( 1.000000000000000000, 0.8905178607896807597, 1.000000000000000000),
 ( 1.000000000000000000, 0.9170530604351546655, 1.000000000000000000),
 ( 1.000000000000000000, 0.9248184710078904969, 1.000000000000000000),
 ( 1.000000000000000000, 0.9238795325112871826, 1.000000000000000000) ) ) 
 REPRESENTATION_ITEM ( '' )  SURFACE ( )  );
#92826 = CARTESIAN_POINT ( 'NONE',  ( 3.390947817193682656, 6.009837315817661008, -1.082531754730549967 ) ) ;
#92827 = EDGE_LOOP ( 'NONE', ( #146830, #197033, #190471, #130600 ) ) ;
#92828 = CARTESIAN_POINT ( 'NONE',  ( 4.201796189063250253, 1.844709454618495670, 0.8146275914719460776 ) ) ;
#92830 = CARTESIAN_POINT ( 'NONE',  ( 2.518489969072700507, 0.8780072382167501965, 1.866465334303254897 ) ) ;
#92829 = CARTESIAN_POINT ( 'NONE',  ( 4.950698647284403009, 8.927565521807144577, 1.040834085586084257E-14 ) ) ;
#92831 = CARTESIAN_POINT ( 'NONE',  ( -15.75000000000000000, 10.19999999999999929, -3.600000000000000977 ) ) ;
#92832 = CARTESIAN_POINT ( 'NONE',  ( 3.540087506499646874, 7.144202834309300698, -0.7216878364870338292 ) ) ;
#92833 = CARTESIAN_POINT ( 'NONE',  ( 3.285556943750000514, -2.413541666188708579, 1.896917185911906500 ) ) ;
#92834 = CARTESIAN_POINT ( 'NONE',  ( -1.201851678989727383E-14, 5.196875000341422357, -1.575800808251660134 ) ) ;
#92835 = CARTESIAN_POINT ( 'NONE',  ( 6.246043798300164873, 0.6838514278588082584, 2.082077653496945402 ) ) ;
#92836 = CARTESIAN_POINT ( 'NONE',  ( 3.938125092175647879, -1.678004675797317713, -1.117833462672225497 ) ) ;
#92837 = CARTESIAN_POINT ( 'NONE',  ( 2.348939331405873077, 0.4892633877765646400, -1.774999737812533063 ) ) ;
#92838 = CARTESIAN_POINT ( 'NONE',  ( 7.806797523370503811, 8.002351953554066810, 1.040834085586084257E-14 ) ) ;
#92839 =( NAMED_UNIT ( * ) SI_UNIT ( $, .STERADIAN. ) SOLID_ANGLE_UNIT ( ) );
#92840 = CARTESIAN_POINT ( 'NONE',  ( 6.387720234973090605, 1.261301916940280154, 1.320039730931761524 ) ) ;
#92841 = CARTESIAN_POINT ( 'NONE',  ( -0.1335965759122420549, -0.1551069838626080166, -2.263292908747056131 ) ) ;
#92842 = CARTESIAN_POINT ( 'NONE',  ( -7.250913225210214641, 7.353820272367037170, 0.7998128361456341429 ) ) ;
#92844 = CARTESIAN_POINT ( 'NONE',  ( -6.330731382938325602, 6.350551133041632212, 0.7998128361456281477 ) ) ;
#92843 = CARTESIAN_POINT ( 'NONE',  ( 5.823173511171203742, -0.06224829877122214916, 2.261828766561886361 ) ) ;
#92845 = CARTESIAN_POINT ( 'NONE',  ( 2.192140752285096639, -0.8994906754480420652, 1.904460908831892008 ) ) ;
#92846 = CARTESIAN_POINT ( 'NONE',  ( -6.934069218746458318, 7.054445274817795486, -0.7998128361456362523 ) ) ;
#92847 = CARTESIAN_POINT ( 'NONE',  ( 7.889955328148847258, 11.29236608522730911, -1.199719254218446718 ) ) ;
#92848 = CARTESIAN_POINT ( 'NONE',  ( 6.902509602688803980, 9.146290184594002781, -1.443375672974064550 ) ) ;
#92849 = CARTESIAN_POINT ( 'NONE',  ( -7.877450944739929461, 9.149113176073413456, 1.199719254218462483 ) ) ;
#92850 = CARTESIAN_POINT ( 'NONE',  ( 1.499999999999959588, 7.064371086078063300, -10.89416074946470836 ) ) ;
#92851 = CARTESIAN_POINT ( 'NONE',  ( 8.229436053370683624, 8.703356271795033905, 0.7216878364870458196 ) ) ;
#92852 = CARTESIAN_POINT ( 'NONE',  ( 4.149696378627680815, 7.633013953984455036, -0.8115063166676712569 ) ) ;
#92853 = CARTESIAN_POINT ( 'NONE',  ( -5.623934791570306402, 5.455678766453782913, 0.7998128361456341429 ) ) ;
#92854 = CARTESIAN_POINT ( 'NONE',  ( 3.076664410187186505, 1.002321471918452556, 1.982530577833590879 ) ) ;
#92855 = CARTESIAN_POINT ( 'NONE',  ( 0.01274299142895937362, -0.9473294304004549193, -1.991142614049784099 ) ) ;
#92856 = CARTESIAN_POINT ( 'NONE',  ( -6.459533842268148973, 6.500820668926428958, 0.000000000000000000 ) ) ;
#92857 = CARTESIAN_POINT ( 'NONE',  ( 4.476163270806094552, 8.373940915915776273, 0.7998128361456462443 ) ) ;
#92858 = CARTESIAN_POINT ( 'NONE',  ( 4.017981030900905637, 1.947309607215493621, -0.2378496960543720617 ) ) ;
#92859 = CARTESIAN_POINT ( 'NONE',  ( 9.589694723567584234, 10.08239868711733855, -0.7998128361456281477 ) ) ;
#92860 = CARTESIAN_POINT ( 'NONE',  ( -5.552553451737586521, 6.223206628393089801, 0.9334509375357492589 ) ) ;
#92861 = DIRECTION ( 'NONE',  ( -0.6507913734559641616, -0.7592566023653004592, 0.000000000000000000 ) ) ;
#92862 = CARTESIAN_POINT ( 'NONE',  ( -0.6823417656250212460, 0.8010416670080899859, 1.181850606188755259 ) ) ;
#92863 = CARTESIAN_POINT ( 'NONE',  ( -4.421367491832313590, 6.251624388594711590, 1.443375672974065660 ) ) ;
#92865 = VERTEX_POINT ( 'NONE', #11945 ) ;
#92864 = CARTESIAN_POINT ( 'NONE',  ( -7.063434843039784639, 7.343021526408956667, 1.040834085586084257E-14 ) ) ;
#92867 = CARTESIAN_POINT ( 'NONE',  ( 3.937823072884456099, -2.028283017459261650, 0.6187693826033290323 ) ) ;
#92866 = AXIS2_PLACEMENT_3D ( 'NONE', #43237, #24815, #205697 ) ;
#92868 = CARTESIAN_POINT ( 'NONE',  ( -5.418418667316934112, 6.350518529071726981, -1.199719254218453823 ) ) ;
#92869 = CARTESIAN_POINT ( 'NONE',  ( 4.241217004700631676, -1.882188537963986219, 1.063020064016991117 ) ) ;
#92870 = CARTESIAN_POINT ( 'NONE',  ( 3.790429961727882713, 1.553415782126759792, -0.9881970032953185656 ) ) ;
#92871 = CARTESIAN_POINT ( 'NONE',  ( -5.012544637203120601, 6.604931577287184830, 1.238112577840282169 ) ) ;
#92872 = CARTESIAN_POINT ( 'NONE',  ( 1.364683531249986537, 0.7177083336747527298, -0.7879004041258239610 ) ) ;
#92873 = CARTESIAN_POINT ( 'NONE',  ( 5.911982399937937949, 1.163873415549965262, -1.294066288734674997 ) ) ;
#92874 = CARTESIAN_POINT ( 'NONE',  ( 6.827182134110207024, 2.985003573113382824, 2.264833014350222662 ) ) ;
#92875 = CARTESIAN_POINT ( 'NONE',  ( 2.412988153552339643, 5.758977245878946327, 0.7216878364870438212 ) ) ;
#92876 = FILL_AREA_STYLE_COLOUR ( '', #32257 ) ;
#92877 = EDGE_CURVE ( 'NONE', #185672, #92893, #163936, .T. ) ;
#92878 = CARTESIAN_POINT ( 'NONE',  ( 2.905317003618158367, 1.825515667692039878, 1.157497049167732550 ) ) ;
#92879 = CARTESIAN_POINT ( 'NONE',  ( 5.888046020683160187, -0.05228737891407529703, 2.015604419750731680 ) ) ;
#92880 = CARTESIAN_POINT ( 'NONE',  ( -7.158341917891067219, 11.29522330427417565, 0.000000000000000000 ) ) ;
#92881 = STYLED_ITEM ( 'NONE', ( #203569 ), #203429 ) ;
#92882 = CARTESIAN_POINT ( 'NONE',  ( 2.044033295145482043, 0.8276103948961744949, -1.997198329219296742 ) ) ;
#92883 = CARTESIAN_POINT ( 'NONE',  ( 3.251204012874517879, -1.609649185575717123, -1.137836448096725794 ) ) ;
#92884 = CARTESIAN_POINT ( 'NONE',  ( -3.147653791585729444, 8.920000000000001705, -2.419999999999998597 ) ) ;
#92885 = CARTESIAN_POINT ( 'NONE',  ( 0.9390046912478089425, 2.274041295854188238, 0.3912414073941206105 ) ) ;
#92886 = CARTESIAN_POINT ( 'NONE',  ( 4.247558953154553230, 1.941557341479711152, -0.05109960196620494388 ) ) ;
#92889 = EDGE_LOOP ( 'NONE', ( #127570, #17141 ) ) ;
#92888 = CARTESIAN_POINT ( 'NONE',  ( -1.257539916218628262, 3.158837156058347695, 0.7750000000000100142 ) ) ;
#92887 = CARTESIAN_POINT ( 'NONE',  ( -9.449669878600625239, 10.12696240122997082, -0.7216878364870267237 ) ) ;
#92890 = CARTESIAN_POINT ( 'NONE',  ( -6.818824913030298696, 6.919993584815607335, 0.7998128361456341429 ) ) ;
#92891 = CARTESIAN_POINT ( 'NONE',  ( -0.02244404828157658613, -0.004869073801674199918, -2.189079685368473527 ) ) ;
#92893 = VERTEX_POINT ( 'NONE', #210703 ) ;
#92892 = CARTESIAN_POINT ( 'NONE',  ( -5.978219388983010418, 5.939287140093762574, -0.7998128361456362523 ) ) ;
#92894 = CARTESIAN_POINT ( 'NONE',  ( -8.012505595552038784, 8.450270737673262644, 0.7216878364870578100 ) ) ;
#92895 = CARTESIAN_POINT ( 'NONE',  ( 2.397764582540245382, 1.705505620506567510, 1.400368488499253994 ) ) ;
#92896 = CARTESIAN_POINT ( 'NONE',  ( -1.642778471874998480, -3.988541666188710089, 2.845375778867863303 ) ) ;
#92897 = CARTESIAN_POINT ( 'NONE',  ( 6.262552437187629550, -0.7028992384056665932, -1.831702256219314151 ) ) ;
#92898 = CARTESIAN_POINT ( 'NONE',  ( -1.201851678989727383E-14, 5.259375000341421469, -1.575800808251660134 ) ) ;
#92899 = CARTESIAN_POINT ( 'NONE',  ( 0.7499999999999920064, 4.514583334016150751, 1.299038105676669330 ) ) ;
#92900 = CARTESIAN_POINT ( 'NONE',  ( 5.971451247601332391, 6.106144735068791185, -0.6754856502540294017 ) ) ;
#92902 = LINE ( 'NONE', #206614, #68439 ) ;
#92901 = CARTESIAN_POINT ( 'NONE',  ( 0.1749903794560749015, 6.948553613792602057, -2.550375946188668586 ) ) ;
#92903 = CARTESIAN_POINT ( 'NONE',  ( 5.419803763747102821, 1.093575605593154920, -1.481025086994464113 ) ) ;
#92904 = EDGE_LOOP ( 'NONE', ( #40239, #89661, #162516, #87359, #203533 ) ) ;
#92905 = CARTESIAN_POINT ( 'NONE',  ( -1.225000000000056044, 2.541666667349471886, -0.7072540797572937077 ) ) ;
#92906 = CARTESIAN_POINT ( 'NONE',  ( -6.612626235163205024, 8.737816579155630592, -1.599625672291263179 ) ) ;
#92907 = CARTESIAN_POINT ( 'NONE',  ( 10.91864124492992616, -9.978085788838701120, -0.1530507449821316146 ) ) ;
#92908 = CARTESIAN_POINT ( 'NONE',  ( 6.047156637250688860, 0.2094617991648151656, 2.110256208591613003 ) ) ;
#92909 = CARTESIAN_POINT ( 'NONE',  ( 11.95103256899996502, 6.645237973884175808, 0.4970601757468578463 ) ) ;
#92910 = CARTESIAN_POINT ( 'NONE',  ( 3.649115900372475796, 7.409052317076538330, 1.040834085586084257E-14 ) ) ;
#92911 = CARTESIAN_POINT ( 'NONE',  ( 0.4091470207043126917, 1.792883176943863122, 1.016159331636699470 ) ) ;
#92914 = CARTESIAN_POINT ( 'NONE',  ( 5.038538826285253514, -1.576363729006284187, 0.9512496309353533075 ) ) ;
#92913 = CARTESIAN_POINT ( 'NONE',  ( 1.978732740145513480, 1.735006779315110492, 0.6737207639663128633 ) ) ;
#92912 = CARTESIAN_POINT ( 'NONE',  ( -10.28373532799257539, 4.806408141292263458, 6.104877701959067871 ) ) ;
#92915 = CARTESIAN_POINT ( 'NONE',  ( 6.096362627639171805, 10.26417349888772179, -0.7998128361456291469 ) ) ;
#92916 = CARTESIAN_POINT ( 'NONE',  ( -7.829692872007384175, 15.51984681892806073, 9.104471052007852450 ) ) ;
#92917 =( BOUNDED_CURVE ( )  B_SPLINE_CURVE ( 2, ( #87887, #155025, #5527, #137719, #203739, #6609, #72690 ),
 .UNSPECIFIED., .F., .T. ) 
 B_SPLINE_CURVE_WITH_KNOTS ( ( 3, 2, 2, 3 ),
 ( 0.4141369526679988811, 0.4166666666666666852, 0.4226190476190476164, 0.4251487616177153650 ),
 .UNSPECIFIED. ) 
 CURVE ( )  GEOMETRIC_REPRESENTATION_ITEM ( )  RATIONAL_B_SPLINE_CURVE ( ( 0.9345202395942611151, 0.9430618748659218564, 1.000000000000000000, 0.8660254037844387076, 1.000000000000000000, 0.9430618748659225226, 0.9345202395942613371 ) ) 
 REPRESENTATION_ITEM ( '' )  );
#92918 = CARTESIAN_POINT ( 'NONE',  ( -4.782994330570982555, 8.802186828966616972, 0.000000000000000000 ) ) ;
#92920 = ORIENTED_EDGE ( 'NONE', *, *, #71027, .T. ) ;
#92919 = CARTESIAN_POINT ( 'NONE',  ( -6.688963559358025890, -6.732807188596383163, -6.903494779225468392 ) ) ;
#92921 = CARTESIAN_POINT ( 'NONE',  ( 4.582781371344160526, -2.140174514510746029, -0.5380331057033281850 ) ) ;
#92922 = CARTESIAN_POINT ( 'NONE',  ( 6.468092748254181679, 1.154776641680499205, 1.945382213218769252 ) ) ;
#92923 = CARTESIAN_POINT ( 'NONE',  ( -4.595850885352567694, 8.305650432979225783, 1.040834085586084257E-14 ) ) ;
#92924 = CARTESIAN_POINT ( 'NONE',  ( 6.240474538790502734, 1.035194401182498281, -1.486496517754380742 ) ) ;
#92925 = CARTESIAN_POINT ( 'NONE',  ( 6.157445398352582977, 1.830988975552667153, -0.5633538272611648967 ) ) ;
#92926 = VECTOR ( 'NONE', #1269, 1000.000000000000000 ) ;
#92927 = FACE_OUTER_BOUND ( 'NONE', #188464, .T. ) ;
#92928 = CARTESIAN_POINT ( 'NONE',  ( 0.07536363704233400851, 2.864322694550157422, -2.632457840217193645 ) ) ;
#92929 = CARTESIAN_POINT ( 'NONE',  ( 6.147114339676178041, 0.1922309238813116050, 1.902605946959089689 ) ) ;
#92930 = DIRECTION ( 'NONE',  ( 1.000000000000000000, -7.771561172376097755E-16, -4.440892098500627148E-16 ) ) ;
#92931 = CARTESIAN_POINT ( 'NONE',  ( 1.270139834521961886, -1.189467451172643964, 1.443775233441677130 ) ) ;
#92932 = CARTESIAN_POINT ( 'NONE',  ( 1.903530124611974017, -1.954778955200174861, 0.4946342604733033887 ) ) ;
#92934 = CARTESIAN_POINT ( 'NONE',  ( 4.002637171539184635, -0.6605693356034693098, -1.999858192447926397 ) ) ;
#92933 = CARTESIAN_POINT ( 'NONE',  ( -9.398826802771548472, 11.98838390803207865, -1.599625672291263179 ) ) ;
#92935 = CARTESIAN_POINT ( 'NONE',  ( 8.446893396513862839, 9.813462703143045474, -1.199719254218445830 ) ) ;
#92937 = CARTESIAN_POINT ( 'NONE',  ( -7.167456763118792651, 11.51378332361394818, 0.000000000000000000 ) ) ;
#92936 = CARTESIAN_POINT ( 'NONE',  ( -1.402160292154681736E-14, -0.5374999999999753308, 1.732050807568877637 ) ) ;
#92938 = CYLINDRICAL_SURFACE ( 'NONE', #72023, 1.500000000000000222 ) ;
#92939 = CARTESIAN_POINT ( 'NONE',  ( 2.707290811070970804, 1.730213373471348737, -1.041854834777849126 ) ) ;
#92940 = CARTESIAN_POINT ( 'NONE',  ( -1.201851678989727383E-14, 3.821875000341423689, 1.575800808251672791 ) ) ;
#92941 = CARTESIAN_POINT ( 'NONE',  ( 4.196412238629597447, 4.854568018944682706, -1.199719254218452047 ) ) ;
#92942 = CARTESIAN_POINT ( 'NONE',  ( 3.972077263441410100, 1.197190051160206936, 1.799587594625361220 ) ) ;
#92943 = CARTESIAN_POINT ( 'NONE',  ( -1.737499999999997824, -1.647916665710749573, 3.009438278150925683 ) ) ;
#92944 = CARTESIAN_POINT ( 'NONE',  ( -1.201851678989727383E-14, 5.087500000000019007, -1.732050807568863648 ) ) ;
#92946 = DIRECTION ( 'NONE',  ( -5.578564026256490882E-16, -1.000000000000000000, -9.066213480720158442E-32 ) ) ;
#92945 = CARTESIAN_POINT ( 'NONE',  ( 7.075376061485196821, 9.347967719856493218, 1.599625672291268286 ) ) ;
#92947 = CARTESIAN_POINT ( 'NONE',  ( 8.066738210006679566, 10.43428054980638997, 1.443375672974076540 ) ) ;
#92949 = CARTESIAN_POINT ( 'NONE',  ( 9.397879144821100539, 13.53129603721547980, -7.462055881301290050 ) ) ;
#92948 = CARTESIAN_POINT ( 'NONE',  ( 2.154941862968827504, -0.5775488349282401623, -2.092905974620140164 ) ) ;
#92951 = CARTESIAN_POINT ( 'NONE',  ( 0.6965153189463432204, 1.505040478001760107, 1.060415605250275339 ) ) ;
#92950 = CARTESIAN_POINT ( 'NONE',  ( -6.236387472606145010, 9.259240570473746601, -1.082531754730538864 ) ) ;
#92952 = CARTESIAN_POINT ( 'NONE',  ( -1.364683531250012516, 1.780208333674757615, 0.7879004041258379498 ) ) ;
#92953 = CARTESIAN_POINT ( 'NONE',  ( 2.454835928891830221, -1.908367152989149718, -1.077367144120815023 ) ) ;
#92954 = CARTESIAN_POINT ( 'NONE',  ( 6.983263157960386991, 6.036006179461032239, 2.548702536770989457 ) ) ;
#92955 = CARTESIAN_POINT ( 'NONE',  ( 4.030342351814687696, 1.213150246598847293, -1.909612865279747052 ) ) ;
#92956 = CARTESIAN_POINT ( 'NONE',  ( -5.859094939400033120, 9.987361195942037639, -0.7998128361456231517 ) ) ;
#92958 = CIRCLE ( 'NONE', #131190, 11.54340198673881979 ) ;
#92957 = CARTESIAN_POINT ( 'NONE',  ( -0.6823417656249969321, 5.280208333674756283, -1.181850606188749264 ) ) ;
#92959 = CARTESIAN_POINT ( 'NONE',  ( 5.794989345469916842, 7.230977472937116346, 1.182549002416101835 ) ) ;
#92960 = CARTESIAN_POINT ( 'NONE',  ( -0.7500000000000179856, 11.79166666666666607, 1.299038105676658228 ) ) ;
#92961 = CARTESIAN_POINT ( 'NONE',  ( 6.888951449519509218, 7.209733910627123876, -0.7216878364870317197 ) ) ;
#92962 = CARTESIAN_POINT ( 'NONE',  ( 4.499107683057060214, 1.420662411309661088, 1.055048638519467286 ) ) ;
#92963 = CARTESIAN_POINT ( 'NONE',  ( 7.587759525142423911, 12.00413654597487501, 0.7998128361456462443 ) ) ;
#92964 = CARTESIAN_POINT ( 'NONE',  ( 0.7277292075377658209, -1.999665741513008799, 0.6608504825312794262 ) ) ;
#92966 = CARTESIAN_POINT ( 'NONE',  ( -1.500000000000013101, 1.129166666666688634, -0.8660254037844313801 ) ) ;
#92965 = CARTESIAN_POINT ( 'NONE',  ( -1.364683531250014514, 10.83854166700806942, -0.7879004041258335089 ) ) ;
#92967 = AXIS2_PLACEMENT_3D ( 'NONE', #137687, #69443, #200513 ) ;
#92968 = CARTESIAN_POINT ( 'NONE',  ( -3.949167883330528372, 7.829389307186077396, 1.214306433183764966E-14 ) ) ;
#92969 = CARTESIAN_POINT ( 'NONE',  ( 6.275017575846199236, 1.753023089329442064, -0.9963169848806670004 ) ) ;
#92970 = VERTEX_POINT ( 'NONE', #109015 ) ;
#92971 = CARTESIAN_POINT ( 'NONE',  ( 7.619319141200070256, 8.951922421897323900, 1.082531754730558626 ) ) ;
#92972 = CARTESIAN_POINT ( 'NONE',  ( 10.08456733046637765, 10.65975006183261087, 0.000000000000000000 ) ) ;
#92973 = CARTESIAN_POINT ( 'NONE',  ( 3.309304339999539657, -0.3661640501408692794, 1.834289908569000538 ) ) ;
#92974 = CARTESIAN_POINT ( 'NONE',  ( 4.680570891794395116, 1.277791010243028991, -1.628752506732597638 ) ) ;
#92975 = CARTESIAN_POINT ( 'NONE',  ( -6.333067150914850174, 8.481940657524365434, 1.443375672974064550 ) ) ;
#92976 = CARTESIAN_POINT ( 'NONE',  ( -2.493954129951868826, 3.487142912321097299, 11.73313169142968881 ) ) ;
#92977 = CARTESIAN_POINT ( 'NONE',  ( 8.483651433849084711, 10.92067931095586886, 1.599625672291281386 ) ) ;
#92978 = CARTESIAN_POINT ( 'NONE',  ( -8.292783513053063160, 12.82666453187061073, 0.7998128361456481317 ) ) ;
#92979 = CARTESIAN_POINT ( 'NONE',  ( 7.679767667498067496, 7.924426798361372093, 0.000000000000000000 ) ) ;
#92980 = EDGE_CURVE ( 'NONE', #146105, #129260, #153565, .T. ) ;
#92981 = CARTESIAN_POINT ( 'NONE',  ( 5.090963066000425030, 4.916608305390635536, -0.1510418726307351800 ) ) ;
#92982 = CARTESIAN_POINT ( 'NONE',  ( -1.364683531250014514, -1.219791666325248602, 0.7879004041258379498 ) ) ;
#92983 = CARTESIAN_POINT ( 'NONE',  ( 3.789464544343919883, -1.813617537123424661, 0.7486148740368094856 ) ) ;
#92984 = CARTESIAN_POINT ( 'NONE',  ( 0.7376574009502724349, -1.897405874265755354, -0.6818954202830116440 ) ) ;
#92985 = CARTESIAN_POINT ( 'NONE',  ( -2.986538976760251263, 6.706322249520737522, -0.7998128361456481317 ) ) ;
#92986 = CARTESIAN_POINT ( 'NONE',  ( 4.127082626822145883, 7.435606486324357611, -0.7117951089531282527 ) ) ;
#92987 = CARTESIAN_POINT ( 'NONE',  ( 0.4560483712790652233, 0.7097975879313439540, 1.730851494400275747 ) ) ;
#92988 = CARTESIAN_POINT ( 'NONE',  ( -1.201851678989727383E-14, 3.446875000341421469, -1.575800808251660134 ) ) ;
#92989 = CARTESIAN_POINT ( 'NONE',  ( 3.006110871101048687, -0.8120814715368419590, 1.842311383860009588 ) ) ;
#92991 = CARTESIAN_POINT ( 'NONE',  ( 3.040728130433269616, -1.601530262690466389, 1.384902248896832333 ) ) ;
#92990 = CARTESIAN_POINT ( 'NONE',  ( -7.239690840017442675, 7.548653522882887934, 0.7216878364870317197 ) ) ;
#92993 = EDGE_CURVE ( 'NONE', #127447, #73877, #76071, .T. ) ;
#92992 = DIRECTION ( 'NONE',  ( 0.000000000000000000, 1.000000000000000000, 0.000000000000000000 ) ) ;
#92994 = CARTESIAN_POINT ( 'NONE',  ( 5.090316257491098284, 1.067296284200716983, -1.773933887923849984 ) ) ;
#92995 = CARTESIAN_POINT ( 'NONE',  ( 6.587282531393223728, 8.778525268082516320, 1.599625672291268286 ) ) ;
#92997 = CARTESIAN_POINT ( 'NONE',  ( 3.216308754939877446, 4.775446185561722956, -1.599625672291262513 ) ) ;
#92996 = CARTESIAN_POINT ( 'NONE',  ( 0.2047783418026409563, 1.821168281471240435, 1.026754182986739927 ) ) ;
#92999 = ORIENTED_EDGE ( 'NONE', *, *, #20907, .T. ) ;
#92998 = CARTESIAN_POINT ( 'NONE',  ( 5.456004705108882469, 1.823398332572896186, -0.09148835057352226741 ) ) ;
#93000 = CARTESIAN_POINT ( 'NONE',  ( 7.995557903757111617, 10.35123685918189729, 1.599625672291281386 ) ) ;
#93001 = CARTESIAN_POINT ( 'NONE',  ( 2.060660350336875002, 8.500464906087991324, -2.499999999999994671 ) ) ;
#93002 = CARTESIAN_POINT ( 'NONE',  ( 11.73212044392280262, 8.686627382477217552, -4.360314433000339385 ) ) ;
#93003 = CARTESIAN_POINT ( 'NONE',  ( -11.73082749631449140, 4.534045925630191931, 5.066687987500840151 ) ) ;
#93004 = CARTESIAN_POINT ( 'NONE',  ( 1.364683531250000748, 12.31770833367473195, -0.7879004041258355073 ) ) ;
#93005 = CARTESIAN_POINT ( 'NONE',  ( 6.569012486276131213, -1.474873517498687558, 1.216900358440069052 ) ) ;
#93006 = CARTESIAN_POINT ( 'NONE',  ( -8.402302512167102222, 10.82577223566020841, -1.599625672291263179 ) ) ;
#93007 = AXIS2_PLACEMENT_3D ( 'NONE', #129632, #26703, #11519 ) ;
#93008 = CARTESIAN_POINT ( 'NONE',  ( 6.844168616800228477, 6.879284895888727824, -0.7998128361456281477 ) ) ;
#93009 = CARTESIAN_POINT ( 'NONE',  ( 0.6801582343749970061, 2.505208333674749266, 1.178068619123801675 ) ) ;
#93010 = CARTESIAN_POINT ( 'NONE',  ( 3.185802909086937973, 6.660594460669327255, 0.7216878364870317197 ) ) ;
#93011 = CARTESIAN_POINT ( 'NONE',  ( -3.794760873454035899, 7.353399519509664195, 0.6126618612011502929 ) ) ;
#93012 = CARTESIAN_POINT ( 'NONE',  ( 5.183294799126148433, 4.941598775268944976, 1.040834085586084257E-14 ) ) ;
#93013 = VERTEX_POINT ( 'NONE', #61262 ) ;
#93014 = CARTESIAN_POINT ( 'NONE',  ( -6.180537922983287302, 8.303989891604203422, -1.599625672291271394 ) ) ;
#93015 = CARTESIAN_POINT ( 'NONE',  ( -0.02299388927990211537, 2.886218872804919400, -2.399728103386359557 ) ) ;
#93017 = CARTESIAN_POINT ( 'NONE',  ( 5.182959862174088883, 9.268813282503625572, 0.7998128361456331437 ) ) ;
#93016 = CARTESIAN_POINT ( 'NONE',  ( 0.2514851628624798496, -9.242341987627179734, -9.497468999145715074 ) ) ;
#93018 = LINE ( 'NONE', #58364, #46876 ) ;
#93019 = AXIS2_PLACEMENT_3D ( 'NONE', #159611, #176929, #11208 ) ;
#93020 = CARTESIAN_POINT ( 'NONE',  ( -6.502161524297833672, 6.757477167027320597, -0.005777863564433716181 ) ) ;
#93021 = EDGE_CURVE ( 'NONE', #149924, #174590, #63997, .T. ) ;
#93022 = CARTESIAN_POINT ( 'NONE',  ( -5.585596099150182958, 8.499983968108443477, -1.082531754730544860 ) ) ;
#93023 = CARTESIAN_POINT ( 'NONE',  ( 4.009460741339333723, 5.700790169694431420, -1.599625672291256295 ) ) ;
#93024 = CARTESIAN_POINT ( 'NONE',  ( 2.008593398387849671, 0.6130636034600014383, 1.871695086544410636 ) ) ;
#93025 = CARTESIAN_POINT ( 'NONE',  ( 3.321888824615967906, 0.9040932542298124597, -1.802426844439278142 ) ) ;
#93026 = CARTESIAN_POINT ( 'NONE',  ( -7.670162217029145246, 9.971608557999250166, 1.599625672291295375 ) ) ;
#93027 = CARTESIAN_POINT ( 'NONE',  ( 6.827182134110223011, 1.235230467647760788, 2.302354205009625954 ) ) ;
#93028 = CARTESIAN_POINT ( 'NONE',  ( 3.468858241077877214, 0.05382521638562161315, -2.190950023606648145 ) ) ;
#93029 = FACE_OUTER_BOUND ( 'NONE', #113595, .T. ) ;
#93030 = CARTESIAN_POINT ( 'NONE',  ( 1.746969779936607292, -1.628684531152933657, 1.028491977540356705 ) ) ;
#93031 = CARTESIAN_POINT ( 'NONE',  ( -7.458957065812611198, 11.85386701009007204, 0.7998128361456481317 ) ) ;
#93032 = SURFACE_STYLE_FILL_AREA ( #110393 ) ;
#93033 = CARTESIAN_POINT ( 'NONE',  ( 0.2329586101569528500, 5.725166970077667727, -2.439795138137319963 ) ) ;
#93034 = CARTESIAN_POINT ( 'NONE',  ( 7.609150525767641504, 9.900428251527500834, -1.599625672291262513 ) ) ;
#93035 = CARTESIAN_POINT ( 'NONE',  ( 3.974511587100456822, 7.788680618259193444, 1.040834085586084257E-14 ) ) ;
#93036 = CARTESIAN_POINT ( 'NONE',  ( -1.225000000000019407, 1.250000000000028866, -1.734723475976807094E-14 ) ) ;
#93037 = CARTESIAN_POINT ( 'NONE',  ( 6.238160076063542725, 6.450477308261824305, -0.7216878364870458196 ) ) ;
#93038 = ORIENTED_EDGE ( 'NONE', *, *, #186024, .T. ) ;
#93040 = CARTESIAN_POINT ( 'NONE',  ( 2.719391910328097683, 1.701792079550172421, 1.075097526896612088 ) ) ;
#93039 = CARTESIAN_POINT ( 'NONE',  ( 6.585540641348407220, -0.7802508550805786758, 1.666130356082275998 ) ) ;
#93041 = CARTESIAN_POINT ( 'NONE',  ( 4.200743080572525656, -1.581147070632774598, -1.668312408496865684 ) ) ;
#93043 = CARTESIAN_POINT ( 'NONE',  ( 1.920531177235841103, -1.320465346956477992, 1.311572250416197960 ) ) ;
#93042 = CARTESIAN_POINT ( 'NONE',  ( -0.1288028175206907822, 6.946859453142047336, -2.869069570226709498 ) ) ;
#93044 = CARTESIAN_POINT ( 'NONE',  ( -3.285556943750000070, -0.8093749995220431703, 0.000000000000000000 ) ) ;
#93045 = CARTESIAN_POINT ( 'NONE',  ( 0.4000000000000045186, 2.999999999999988898, 0.4999999999999674705 ) ) ;
#93046 = CARTESIAN_POINT ( 'NONE',  ( 6.275647926998929371, 0.3200337115364471074, -1.885262484646982095 ) ) ;
#93047 = CARTESIAN_POINT ( 'NONE',  ( -7.157815033010924921, 10.43820240756634199, 1.199719254218453823 ) ) ;
#93048 = CARTESIAN_POINT ( 'NONE',  ( -6.617788377246204945, 6.893376992974917350, -0.7216878364870338292 ) ) ;
#93050 = CARTESIAN_POINT ( 'NONE',  ( 4.082764389539480732, -0.1829629792115642917, -1.861669828791753467 ) ) ;
#93049 = CARTESIAN_POINT ( 'NONE',  ( 4.915614241032515430, -1.119620181645267776, -1.765504464341709934 ) ) ;
#93051 = CARTESIAN_POINT ( 'NONE',  ( 5.016153647376196290, 8.796003655340152605, 0.7216878364870438212 ) ) ;
#93052 = VERTEX_POINT ( 'NONE', #3433 ) ;
#93053 = AXIS2_PLACEMENT_3D ( 'NONE', #196238, #113994, #82468 ) ;
#93054 = CARTESIAN_POINT ( 'NONE',  ( -1.492390896412726597, 7.408229809043063163, 4.235510822232345873 ) ) ;
#93055 = DIRECTION ( 'NONE',  ( 0.000000000000000000, 1.000000000000000000, 0.000000000000000000 ) ) ;
#93056 = CARTESIAN_POINT ( 'NONE',  ( 5.637229722410256549, -1.556708995667484441, 0.7431856355405024317 ) ) ;
#93057 = CARTESIAN_POINT ( 'NONE',  ( -7.088215381846223906, 7.164006121775713609, 0.7998128361456341429 ) ) ;
#93058 = CARTESIAN_POINT ( 'NONE',  ( 1.968989728591052479, -1.700769290752032870, -0.3374826141460812168 ) ) ;
#93059 = CARTESIAN_POINT ( 'NONE',  ( 6.484567079770447329, -6.583980363594976737, 7.100579091573052004 ) ) ;
#93060 = DIRECTION ( 'NONE',  ( -0.7592566023653016805, -0.6507913734559627184, -7.055894209357776889E-15 ) ) ;
#93061 = CARTESIAN_POINT ( 'NONE',  ( 6.420782495146515778, -1.541274310347956922, 1.529322475779694601 ) ) ;
#93062 = CARTESIAN_POINT ( 'NONE',  ( 3.984828715814022981, -0.1808549858164226476, -1.816707794649790708 ) ) ;
#93063 = CARTESIAN_POINT ( 'NONE',  ( 2.588659458060487584, 1.901619664775334728, 0.4814403318105645591 ) ) ;
#93064 = DIRECTION ( 'NONE',  ( -0.9980366791917738567, 0.000000000000000000, 0.06263215618080149316 ) ) ;
#93065 = CARTESIAN_POINT ( 'NONE',  ( 8.426556166093362776, 9.789735934319136135, -1.199719254218446718 ) ) ;
#93066 = CARTESIAN_POINT ( 'NONE',  ( 2.385534290476189145, 0.1013982516714604792, -2.118174289320504666 ) ) ;
#93067 = CARTESIAN_POINT ( 'NONE',  ( -2.928197990871687306, 5.399686175116803710, 1.082531754730560403 ) ) ;
#93068 = AXIS2_PLACEMENT_3D ( 'NONE', #172851, #107908, #40716 ) ;
#93069 = CARTESIAN_POINT ( 'NONE',  ( 1.734723475976807094E-15, -3.469446951953614189E-15, -0.2879360613984097150 ) ) ;
#93070 = CARTESIAN_POINT ( 'NONE',  ( -4.512490679940424521, 7.037946173918820492, -1.151410311177623935 ) ) ;
#93071 = CARTESIAN_POINT ( 'NONE',  ( 0.6903901511902330590, 1.067356595782501749, -1.773781848916009096 ) ) ;
#93073 = CARTESIAN_POINT ( 'NONE',  ( 0.7500000000000006661, 13.36458333401613352, 1.299038105676657340 ) ) ;
#93072 = CARTESIAN_POINT ( 'NONE',  ( -10.65376315971086640, 4.226338639847933898, 5.523257262081396668 ) ) ;
#93075 = ORIENTED_EDGE ( 'NONE', *, *, #4848, .T. ) ;
#93074 = CARTESIAN_POINT ( 'NONE',  ( 3.440272213978716742, -1.324219266349660806, -1.783276862766651760 ) ) ;
#93076 = CARTESIAN_POINT ( 'NONE',  ( 0.7745980011552360267, 2.023606461939434720, -1.090472508649400263 ) ) ;
#93078 = CARTESIAN_POINT ( 'NONE',  ( 6.807491137956053429, -1.653082740107037152, -1.233284719700310506 ) ) ;
#93077 = CARTESIAN_POINT ( 'NONE',  ( 2.659370686574860976, 6.254349567645977714, -0.7998128361456291469 ) ) ;
#93080 = CARTESIAN_POINT ( 'NONE',  ( -3.475000000000000533, -2.129166666666665542, -2.006292185433948827 ) ) ;
#93079 = CARTESIAN_POINT ( 'NONE',  ( 3.854260808034858155, 7.718664386007802136, -0.7998128361456362523 ) ) ;
#93081 = CARTESIAN_POINT ( 'NONE',  ( 0.1331565106231329398, 0.7299000548664087429, -2.029785554894456556 ) ) ;
#93082 = CARTESIAN_POINT ( 'NONE',  ( 5.636236351835953506, 0.3653394402399374741, 1.804471444190151930 ) ) ;
#93083 = CARTESIAN_POINT ( 'NONE',  ( -3.602337597214539753E-15, 12.59375000068279782, 1.500000000000001554 ) ) ;
#93084 = CARTESIAN_POINT ( 'NONE',  ( -0.1104750535120234134, 0.7027814200676918421, -2.185477693842474256 ) ) ;
#93085 = CARTESIAN_POINT ( 'NONE',  ( 2.467434050970338077, 1.692020480068063826, -0.3335236308374764369 ) ) ;
#93086 = CARTESIAN_POINT ( 'NONE',  ( 1.182827746461931229, 1.645757370610765102, -1.164989914844760444 ) ) ;
#93087 =( BOUNDED_CURVE ( )  B_SPLINE_CURVE ( 2, ( #52835, #199057, #36576, #101587, #102662, #134126, #33380, #150354, #67983 ),
 .UNSPECIFIED., .F., .T. ) 
 B_SPLINE_CURVE_WITH_KNOTS ( ( 3, 2, 2, 2, 3 ),
 ( 0.3839285714285713969, 0.3869047619047619180, 0.3928571428571428492, 0.3988095238095238360, 0.4017857142857143016 ),
 .UNSPECIFIED. ) 
 CURVE ( )  GEOMETRIC_REPRESENTATION_ITEM ( )  RATIONAL_B_SPLINE_CURVE ( ( 0.9330127018922194093, 0.9330127018922187432, 1.000000000000000000, 0.8660254037844387076, 1.000000000000000000, 0.8660254037844387076, 1.000000000000000000, 0.9330127018922194093, 0.9330127018922194093 ) ) 
 REPRESENTATION_ITEM ( '' )  );
#93088 = CARTESIAN_POINT ( 'NONE',  ( 2.760663040853128525, 2.181856774409622890, -0.7236605881647265592 ) ) ;
#93089 = CARTESIAN_POINT ( 'NONE',  ( 1.827766392559232012, -2.130618655838847353, 0.7612957800654009954 ) ) ;
#93090 = CARTESIAN_POINT ( 'NONE',  ( 4.863951442137788739, 2.083289488599335826, -0.3080729427491457062 ) ) ;
#93091 = CARTESIAN_POINT ( 'NONE',  ( -7.607533591043815768, 8.048079742405473525, 0.000000000000000000 ) ) ;
#93092 = CARTESIAN_POINT ( 'NONE',  ( 3.479546766767865673, 1.120508650343427171, 1.369845563140754230 ) ) ;
#93094 = CARTESIAN_POINT ( 'NONE',  ( 6.462434034201492317, -2.093801447487374734, -0.9336288876484639676 ) ) ;
#93093 = CARTESIAN_POINT ( 'NONE',  ( 4.001064729364292916, 6.721640380016713934, -1.082531754730548412 ) ) ;
#93095 = CARTESIAN_POINT ( 'NONE',  ( 4.452959842461719830, 0.4008590389125502029, -1.796806262838637647 ) ) ;
#93096 = CARTESIAN_POINT ( 'NONE',  ( -6.098470168048611306, 6.009303372345148553, 1.040834085586084257E-14 ) ) ;
#93097 = CARTESIAN_POINT ( 'NONE',  ( 4.297571505407542958, 7.957657823043374989, -0.7216878364870197293 ) ) ;
#93098 = CARTESIAN_POINT ( 'NONE',  ( -0.7500000000000215383, 3.441666666666689967, 1.299038105676671107 ) ) ;
#93099 = CARTESIAN_POINT ( 'NONE',  ( 4.418054252288761141, 1.349281245414082342, -1.726737887558588591 ) ) ;
#93100 = CARTESIAN_POINT ( 'NONE',  ( -5.274285450916075035, 6.112086766612214284, 1.199719254218450271 ) ) ;
#93101 = DIRECTION ( 'NONE',  ( 0.000000000000000000, 0.000000000000000000, -1.000000000000000000 ) ) ;
#93102 = CARTESIAN_POINT ( 'NONE',  ( 4.598136200040512378, 0.8882050449813773119, -1.870312673664726644 ) ) ;
#93103 = CARTESIAN_POINT ( 'NONE',  ( 0.4797043241997685503, -0.7212876333932433104, 1.883314553594167107 ) ) ;
#93104 = CARTESIAN_POINT ( 'NONE',  ( 1.364683531249990311, 4.384375000341417028, 1.214306433183764966E-14 ) ) ;
#93105 = CARTESIAN_POINT ( 'NONE',  ( 3.686086919817387564, -0.9488725894866935073, 1.676545010912360745 ) ) ;
#93106 = CARTESIAN_POINT ( 'NONE',  ( 1.364683531249996529, 9.463541667008062319, 0.7879004041258405033 ) ) ;
#93107 = CARTESIAN_POINT ( 'NONE',  ( -4.622967192579922724, 4.495809267539077503, 1.214306433183764966E-14 ) ) ;
#93108 = CARTESIAN_POINT ( 'NONE',  ( 6.345950370838200350, -1.386202306585911925, -1.604841549997563455 ) ) ;
#93109 = VERTEX_POINT ( 'NONE', #70558 ) ;
#93111 = DIRECTION ( 'NONE',  ( 1.039099362110107450E-15, 1.000000000000000000, -4.583713267641621330E-32 ) ) ;
#93110 = CARTESIAN_POINT ( 'NONE',  ( 0.000000000000000000, 15.44694763437329676, -11.95586206896577153 ) ) ;
#93112 = CARTESIAN_POINT ( 'NONE',  ( 4.029797971759831121, 5.724516938518342535, -1.599625672291255185 ) ) ;
#93113 = CARTESIAN_POINT ( 'NONE',  ( -1.084637062511546901, 3.117628807292010862, -1.105835307554786429 ) ) ;
#93114 = CARTESIAN_POINT ( 'NONE',  ( -0.08053691275167716712, 15.51846456562902965, 11.99972973886013961 ) ) ;
#93115 = AXIS2_PLACEMENT_3D ( 'NONE', #2095, #19429, #67097 ) ;
#93116 = DIRECTION ( 'NONE',  ( 8.673617379884087537E-15, -1.000000000000000000, 0.000000000000000000 ) ) ;
#93117 = FACE_OUTER_BOUND ( 'NONE', #38973, .T. ) ;
#93118 = CARTESIAN_POINT ( 'NONE',  ( 1.609737659951641309, 0.5726723138891122167, -1.876404140693301636 ) ) ;
#93119 = CARTESIAN_POINT ( 'NONE',  ( -0.6823417656250212460, 0.8635416670080899859, 1.181850606188755259 ) ) ;
#93121 = EDGE_CURVE ( 'NONE', #79124, #79300, #185034, .T. ) ;
#93120 =( GEOMETRIC_REPRESENTATION_CONTEXT ( 3 ) GLOBAL_UNCERTAINTY_ASSIGNED_CONTEXT ( ( #180772 ) ) GLOBAL_UNIT_ASSIGNED_CONTEXT ( ( #67595, #68671, #37264 ) ) REPRESENTATION_CONTEXT ( 'NONE', 'WORKASPACE' ) );
#93122 = CARTESIAN_POINT ( 'NONE',  ( 0.000000000000000000, 0.7999999999999951594, 11.69999999999999041 ) ) ;
#93123 = CARTESIAN_POINT ( 'NONE',  ( 5.072687121480487171, 1.354251660176824856, -1.419695456575476689 ) ) ;
#93124 = CARTESIAN_POINT ( 'NONE',  ( -10.13488352141530768, 11.78278451552804817, 1.199719254218462483 ) ) ;
#93125 = CARTESIAN_POINT ( 'NONE',  ( -4.704316113817535339, 8.432193199521691440, 0.7216878364870458196 ) ) ;
#93126 = CARTESIAN_POINT ( 'NONE',  ( 0.1458946441583548470, -1.751458424797154523, -1.431810583859528974 ) ) ;
#93128 = VERTEX_POINT ( 'NONE', #67355 ) ;
#93127 = CARTESIAN_POINT ( 'NONE',  ( -0.2868663046952891760, -5.229832900979432431, -10.99643026930490919 ) ) ;
#93129 = CARTESIAN_POINT ( 'NONE',  ( 0.6823417656249899377, 4.926041667008086655, -1.181850606188754593 ) ) ;
#93130 = CARTESIAN_POINT ( 'NONE',  ( 0.4033012769992084245, -0.5052730135347226481, 1.800932346938296069 ) ) ;
#93131 = CARTESIAN_POINT ( 'NONE',  ( 6.749374558768074017, -1.701276501228730309, -0.3333242692393871831 ) ) ;
#93133 = CARTESIAN_POINT ( 'NONE',  ( 2.613028500285840661, -0.2118117899099076218, 2.181281865515646068 ) ) ;
#93132 = CARTESIAN_POINT ( 'NONE',  ( -0.6801582343750299797, 0.9322916670080338974, 1.178068619123803451 ) ) ;
#93134 = CARTESIAN_POINT ( 'NONE',  ( 4.805897800482852311, -0.6205396350037055697, 2.222522205952178975 ) ) ;
#93135 = CARTESIAN_POINT ( 'NONE',  ( 5.694623797941932963, -0.4965738858758206309, -1.999944147208564171 ) ) ;
#93136 = CARTESIAN_POINT ( 'NONE',  ( 1.763517528630250686, 0.9983118466501934574, 1.665567687315899992 ) ) ;
#93137 = CARTESIAN_POINT ( 'NONE',  ( -7.185458225118419584, 7.485382138834033583, 1.040834085586084257E-14 ) ) ;
#93138 = EDGE_CURVE ( 'NONE', #100761, #86666, #69500, .T. ) ;
#93139 = CARTESIAN_POINT ( 'NONE',  ( 5.584829485406742400, 5.817820313668822685, -0.7485926948523046187 ) ) ;
#93140 = CARTESIAN_POINT ( 'NONE',  ( 4.939744792934912532, -2.012803497507458683, 0.6676120485993168874 ) ) ;
#93141 = CARTESIAN_POINT ( 'NONE',  ( 2.250625165576759290, 1.976955744075848065, -0.3961026872240576702 ) ) ;
#93142 = CARTESIAN_POINT ( 'NONE',  ( -5.436456408955534947, 6.405249234278626247, 1.082531754730546636 ) ) ;
#93143 = CARTESIAN_POINT ( 'NONE',  ( 5.350674426004140116, 0.6359874849255696683, 2.113150234885258438 ) ) ;
#93144 = CARTESIAN_POINT ( 'NONE',  ( -6.526270840131767059, 8.707344961610770540, -1.599625672291271394 ) ) ;
#93145 = CARTESIAN_POINT ( 'NONE',  ( 10.57266086055835075, 11.22919251360659310, 0.000000000000000000 ) ) ;
#93146 = CARTESIAN_POINT ( 'NONE',  ( 0.2756506080626683342, 1.048234779247591453, 1.494575289200591239 ) ) ;
#93147 = CARTESIAN_POINT ( 'NONE',  ( -4.938913097128142304, 8.984092056616635347, -0.7998128361456362523 ) ) ;
#93149 = CARTESIAN_POINT ( 'NONE',  ( -4.444040490229336449, 8.406740681901359480, 0.7998128361456350310 ) ) ;
#93148 = CARTESIAN_POINT ( 'NONE',  ( -5.386518286579200954, 7.671588192869585043, 1.336358942847740927 ) ) ;
#93150 = CARTESIAN_POINT ( 'NONE',  ( 1.524175555628257905, 8.756493634679708649, -2.487619788734836135 ) ) ;
#93151 = VERTEX_POINT ( 'NONE', #33821 ) ;
#93152 = CARTESIAN_POINT ( 'NONE',  ( 5.366112562010656895, 1.013659120426290361, 1.794278544449072088 ) ) ;
#93153 = CARTESIAN_POINT ( 'NONE',  ( -0.6801582343750091075, 2.848958333674732391, -1.178068619123848526 ) ) ;
#93154 = CARTESIAN_POINT ( 'NONE',  ( 0.3080734816350748084, -8.169755926620672071, 9.495223711095322372 ) ) ;
#93155 = CARTESIAN_POINT ( 'NONE',  ( -2.767835915484202047, 6.380892334706859792, -0.7998128361456281477 ) ) ;
#93156 = CARTESIAN_POINT ( 'NONE',  ( -6.138157188980746248, 5.995865266587975917, 0.1610769774899509232 ) ) ;
#93157 = CARTESIAN_POINT ( 'NONE',  ( 4.477216424163804831, -1.805109318760585779, -0.9060198856494814379 ) ) ;
#93159 = ORIENTED_EDGE ( 'NONE', *, *, #78317, .T. ) ;
#93158 = CARTESIAN_POINT ( 'NONE',  ( 0.7499999999999885647, 0.4833333333333564297, 1.299038105676657340 ) ) ;
#93161 = CARTESIAN_POINT ( 'NONE',  ( 9.897088948295946764, 10.64895131587453569, 0.7216878364870438212 ) ) ;
#93160 = CARTESIAN_POINT ( 'NONE',  ( -4.899292406491858820, 6.809203455697518947, -1.599625672291271394 ) ) ;
#93162 = CARTESIAN_POINT ( 'NONE',  ( 6.662942426112080874, 9.860851032851066122, 1.199719254218460707 ) ) ;
#93163 = CARTESIAN_POINT ( 'NONE',  ( 4.118082307656718122, -1.057753326809774963, -1.768578378466668877 ) ) ;
#93164 = CARTESIAN_POINT ( 'NONE',  ( 2.320935597664942396, 0.9480396085976349196, -1.779626998253575509 ) ) ;
#93165 = ORIENTED_EDGE ( 'NONE', *, *, #74123, .T. ) ;
#93166 = CARTESIAN_POINT ( 'NONE',  ( -1.734723475976807094E-15, 2.999999999999988898, -6.938893903907228378E-15 ) ) ;
#93167 = CARTESIAN_POINT ( 'NONE',  ( 3.520313441042647540, 7.258782781191745137, 0.7998128361456321445 ) ) ;
#93168 = B_SPLINE_CURVE_WITH_KNOTS ( 'NONE', 3,
 ( #31098, #148038, #192495, #210881, #110268, #13747, #179474, #96105, #161085, #196775 ),
 .UNSPECIFIED., .F., .F.,
 ( 4, 2, 2, 2, 4 ),
 ( 0.000000000000000000, 0.0006317681591994424740, 0.001263536318398884731, 0.001895304477598327422, 0.002527072636797769896 ),
 .UNSPECIFIED. ) ;
#93170 = ORIENTED_EDGE ( 'NONE', *, *, #176689, .T. ) ;
#93169 = CARTESIAN_POINT ( 'NONE',  ( -0.006913841192827608478, 8.234242197375163386, -1.999988128101763074 ) ) ;
#93171 = B_SPLINE_CURVE_WITH_KNOTS ( 'NONE', 3,
 ( #182870, #18224, #53952, #101629, #186065, #103777, #201236, #150393, #51826, #68025, #52877, #119013, #123315, #126501, #40918, #174131, #107024, #205517, #176247, #60341, #189279, #41995, #157870, #105948, #27849, #25704, #93947, #173049, #158922, #76593, #44118, #140575, #57149, #206588 ),
 .UNSPECIFIED., .F., .F.,
 ( 4, 2, 2, 2, 2, 2, 2, 2, 2, 2, 2, 2, 2, 2, 2, 2, 4 ),
 ( 1.734723475976807094E-18, 0.001499835624873080290, 0.002999671249746158844, 0.004499506874619237616, 0.005999342499492315954, 0.007499178124365395159, 0.008999013749238471763, 0.009748931561675010932, 0.01049884937411154663, 0.01199868499898462497, 0.01349852062385770504, 0.01499835624873078165, 0.01649819187360385825, 0.01799802749847694006, 0.02099769874822308285, 0.02249753437309615772, 0.02399736999796922565 ),
 .UNSPECIFIED. ) ;
#93172 = CARTESIAN_POINT ( 'NONE',  ( 3.093124880496417983, 1.122326866504215426, -1.674630914042275709 ) ) ;
#93173 = CARTESIAN_POINT ( 'NONE',  ( 2.519273208346615167, -1.059988974693906183, -1.505194322970206722 ) ) ;
#93174 = ADVANCED_FACE ( 'NONE', ( #118342 ), #212718, .F. ) ;
#93175 = CARTESIAN_POINT ( 'NONE',  ( 0.5226545517994193313, -1.239659060731788998, -1.946298918093934960 ) ) ;
#93176 = CARTESIAN_POINT ( 'NONE',  ( 4.199993725183334803, 8.122019456014369254, -0.7998128361456362523 ) ) ;
#93177 = CARTESIAN_POINT ( 'NONE',  ( 2.776834730583700228, -2.067601613962879448, -0.6303956341740593050 ) ) ;
#93178 = CARTESIAN_POINT ( 'NONE',  ( 8.748035429315576650, 11.22912730566677553, -1.599625672291255185 ) ) ;
#93179 = CARTESIAN_POINT ( 'NONE',  ( -5.605406444246153974, 8.627059054007450101, -1.199719254218440723 ) ) ;
#93180 = CARTESIAN_POINT ( 'NONE',  ( 2.741952636841408442, -2.198962954702073702, -0.6686182857488265352 ) ) ;
#93181 = ORIENTED_EDGE ( 'NONE', *, *, #151057, .T. ) ;
#93182 = LINE ( 'NONE', #106260, #7673 ) ;
#93183 = CARTESIAN_POINT ( 'NONE',  ( 1.410794581852807150, 1.648159533202856686, 0.8848386531258023435 ) ) ;
#93184 = ORIENTED_EDGE ( 'NONE', *, *, #138625, .F. ) ;
#93185 = CARTESIAN_POINT ( 'NONE',  ( 5.981319044003478247, 1.821754654810204599, -0.7540403668018207384 ) ) ;
#93188 = ADVANCED_FACE ( 'NONE', ( #84708 ), #137746, .F. ) ;
#93187 = CARTESIAN_POINT ( 'NONE',  ( 9.720832950873944611, 10.44331931888218001, -0.7216878364870257245 ) ) ;
#93186 = CARTESIAN_POINT ( 'NONE',  ( -1.364683531250012516, 3.488541667008085767, -0.7879004041258300672 ) ) ;
#93190 = CARTESIAN_POINT ( 'NONE',  ( 1.032169062358662348, -1.402649970393770484, -1.703791656331831605 ) ) ;
#93189 = CARTESIAN_POINT ( 'NONE',  ( -6.261168011412601153, 6.199117522936475666, 1.040834085586084257E-14 ) ) ;
#93191 = CARTESIAN_POINT ( 'NONE',  ( 3.006787879153326681, 6.373552747333731006, -0.4818892653130519843 ) ) ;
#93192 = CARTESIAN_POINT ( 'NONE',  ( 6.193377243344257543, 6.120028293523423812, -0.7998128361456281477 ) ) ;
#93193 = CARTESIAN_POINT ( 'NONE',  ( -6.098470168048611306, 6.009303372345148553, 1.040834085586084257E-14 ) ) ;
#93194 = CARTESIAN_POINT ( 'NONE',  ( 0.3275200278799066389, 3.116672424413486908, 0.4674645318177238495 ) ) ;
#93195 = CARTESIAN_POINT ( 'NONE',  ( 5.506699291815658093, 1.493407355681115378, -1.287129089984188290 ) ) ;
#93196 = CARTESIAN_POINT ( 'NONE',  ( -0.1929003719821283658, -0.4722129235960635940, -2.074948700427194481 ) ) ;
#93197 = CARTESIAN_POINT ( 'NONE',  ( 4.020403473283917783, -1.184823721361260018, -1.980193191683382148 ) ) ;
#93198 = CARTESIAN_POINT ( 'NONE',  ( 3.045816552677531597, 1.455321998776702319, 1.461834479831431555 ) ) ;
#93199 = CARTESIAN_POINT ( 'NONE',  ( 7.144783764721768904, 7.437928601704619780, 1.040834085586084257E-14 ) ) ;
#93200 = CARTESIAN_POINT ( 'NONE',  ( 5.367048706163317640, 7.354919138647580290, -1.599625672291281386 ) ) ;
#93201 = CARTESIAN_POINT ( 'NONE',  ( 4.224247379109608680, 7.085983154673295203, -1.199719254218452047 ) ) ;
#93202 = CARTESIAN_POINT ( 'NONE',  ( 1.364683531249986537, 1.967708333674750731, -0.7879004041258239610 ) ) ;
#93203 = CARTESIAN_POINT ( 'NONE',  ( 4.472210567661338843, 6.310941310395290493, 1.599625672291261402 ) ) ;
#93204 = CARTESIAN_POINT ( 'NONE',  ( 6.033015167956792268, 8.061603667414825480, -1.443375672974057666 ) ) ;
#93205 = CARTESIAN_POINT ( 'NONE',  ( 5.670445308384678640, -0.9712495897680500923, -1.941886722523916253 ) ) ;
#93206 = CARTESIAN_POINT ( 'NONE',  ( -9.579665964948885559, -7.473374494045003757, -0.07999999999998980149 ) ) ;
#93208 = CARTESIAN_POINT ( 'NONE',  ( 3.808014051635350672, 1.299385917162833692, -1.304790556973287163 ) ) ;
#93207 = CARTESIAN_POINT ( 'NONE',  ( -3.578989364327652467, 6.158942777482099729, 1.082531754730560403 ) ) ;
#93209 = CARTESIAN_POINT ( 'NONE',  ( 6.620655732516647518, 0.007553340620044743381, 1.826407896915738238 ) ) ;
#93210 = CARTESIAN_POINT ( 'NONE',  ( 5.161759341795384870, 1.079763445194487970, 1.907048802792680631 ) ) ;
#93211 = CARTESIAN_POINT ( 'NONE',  ( 0.3282377607281107834, 0.1361645503674392965, 1.224999999999955014 ) ) ;
#93212 = CARTESIAN_POINT ( 'NONE',  ( 0.7028506612886147309, -0.7633063118723592000, -2.129901512202157399 ) ) ;
#93213 = CARTESIAN_POINT ( 'NONE',  ( -4.371234765837696656, 7.372762773471292164, -1.195546268109607846 ) ) ;
#93214 = CARTESIAN_POINT ( 'NONE',  ( -1.423205080756925867, 7.980384757729337863, -10.65537363484301636 ) ) ;
#93215 = CARTESIAN_POINT ( 'NONE',  ( 5.141188686642438554, 7.897460914975725998, 1.230089993873971999 ) ) ;
#93216 = AXIS2_PLACEMENT_3D ( 'NONE', #155491, #205284, #90504 ) ;
#93217 = CARTESIAN_POINT ( 'NONE',  ( -4.299344108864961989, 6.109263775132799168, -1.443375672974066548 ) ) ;
#93218 = CARTESIAN_POINT ( 'NONE',  ( -7.636191794455552184, -6.027819618361864862, -7.636191794455517545 ) ) ;
#93219 = CARTESIAN_POINT ( 'NONE',  ( 0.3207183204587023551, -0.09351970983179427876, 1.767511165302604326 ) ) ;
#93220 = CARTESIAN_POINT ( 'NONE',  ( 5.531894615797754433, -1.963542475010676469, 0.4432068886008522779 ) ) ;
#93221 = CARTESIAN_POINT ( 'NONE',  ( 4.014754730066903754, 1.490810813664491974, -1.487730979428596223 ) ) ;
#93222 = CARTESIAN_POINT ( 'NONE',  ( 3.761272268043499345, 1.802513535502557218, -0.6487917036162252904 ) ) ;
#93223 = CARTESIAN_POINT ( 'NONE',  ( 3.195971524519376494, 4.751719416737803847, -1.599625672291262513 ) ) ;
#93224 = CARTESIAN_POINT ( 'NONE',  ( 4.844182406995376944, -0.9301426015250592316, 1.736093160643120914 ) ) ;
#93225 = CARTESIAN_POINT ( 'NONE',  ( 5.502215278945715937, -0.9042992897083046433, 1.806084391566422198 ) ) ;
#93226 = CARTESIAN_POINT ( 'NONE',  ( 2.236979667955760309, -1.672073921526989748, 0.8388852543278202401 ) ) ;
#93229 = ORIENTED_EDGE ( 'NONE', *, *, #6621, .F. ) ;
#93228 = CARTESIAN_POINT ( 'NONE',  ( 1.740342883905017013, 1.098329146349947827, -1.565357986077076990 ) ) ;
#93227 = CARTESIAN_POINT ( 'NONE',  ( 5.672382752830540831, -1.089361703149527072, 1.337344134918318606 ) ) ;
#93231 = CARTESIAN_POINT ( 'NONE',  ( 4.419594888374914099, 5.218910793601261311, -1.082531754730548412 ) ) ;
#93230 = CARTESIAN_POINT ( 'NONE',  ( 2.438337523484556790, 1.039148161723329578, -1.946916322307743474 ) ) ;
#93232 = CARTESIAN_POINT ( 'NONE',  ( -0.6823417656250003738, 2.030208333674753174, -1.181850606188749264 ) ) ;
#93233 = CARTESIAN_POINT ( 'NONE',  ( 6.391066755906244623, 0.1909826923555627554, 1.952524381009380861 ) ) ;
#93235 = AXIS2_PLACEMENT_3D ( 'NONE', #174503, #110613, #43429 ) ;
#93234 = CARTESIAN_POINT ( 'NONE',  ( 6.414979237560321401, 10.63589287712906462, 1.040834085586084257E-14 ) ) ;
#93236 = FACE_OUTER_BOUND ( 'NONE', #115149, .T. ) ;
#93237 = CARTESIAN_POINT ( 'NONE',  ( 10.58872653680447584, -6.465328379374285284, 9.269928574751062911E-15 ) ) ;
#93238 = FACE_OUTER_BOUND ( 'NONE', #58078, .T. ) ;
#93239 = CARTESIAN_POINT ( 'NONE',  ( -10.10516068267232548, -6.085430761754775375, 0.4362825330288350734 ) ) ;
#93240 = CARTESIAN_POINT ( 'NONE',  ( 2.523957353938070192, 2.030885678308389952, -0.4015143504868187718 ) ) ;
#93241 = CARTESIAN_POINT ( 'NONE',  ( 0.7499999999999902300, 3.233333333333352044, 1.299038105676669330 ) ) ;
#93242 = CARTESIAN_POINT ( 'NONE',  ( 4.449046963578762615, 8.342305224150557308, -0.7998128361456231517 ) ) ;
#93243 = CARTESIAN_POINT ( 'NONE',  ( -7.739006755302186846, 7.923262724141010516, 0.7998128361456462443 ) ) ;
#93244 = CARTESIAN_POINT ( 'NONE',  ( 3.390420931869152721, 6.113185632892752075, -1.199719254218452047 ) ) ;
#93245 = CARTESIAN_POINT ( 'NONE',  ( -0.1106727585415967219, -0.002281114264979232885, -2.003378291782103471 ) ) ;
#93246 = SURFACE_STYLE_USAGE ( .BOTH. , #210144 ) ;
#93247 = CARTESIAN_POINT ( 'NONE',  ( 0.6823417656249899377, 3.176041667008085323, -1.181850606188754593 ) ) ;
#93249 = CARTESIAN_POINT ( 'NONE',  ( 4.681643115420508039, 4.356338477612361260, 0.7998128361456341429 ) ) ;
#93248 = LINE ( 'NONE', #143081, #23811 ) ;
#93250 = CARTESIAN_POINT ( 'NONE',  ( 5.272814466252145671, -2.006652483137221665, 0.1948127969565379425 ) ) ;
#93251 = CARTESIAN_POINT ( 'NONE',  ( 4.311684426593565433, -1.183387839401760511, -1.506387502079686191 ) ) ;
#93252 = CARTESIAN_POINT ( 'NONE',  ( 0.000000000000000000, 0.000000000000000000, 0.000000000000000000 ) ) ;
#93253 = CARTESIAN_POINT ( 'NONE',  ( 2.947022816757137065, -1.793111998972513277, -1.259777465452505796 ) ) ;
#93254 = CARTESIAN_POINT ( 'NONE',  ( 0.1333692844072559280, 0.001398348041498076455, -2.053671342968105051 ) ) ;
#93255 = CARTESIAN_POINT ( 'NONE',  ( 1.499999999999987121, 0.5770833340161539704, -0.8660254037844253849 ) ) ;
#93256 = CARTESIAN_POINT ( 'NONE',  ( 5.502202757749218520, -0.9014697883563610459, 1.800137906301606305 ) ) ;
#93257 = CARTESIAN_POINT ( 'NONE',  ( 1.775505761281343631, 0.3235837346332003372, -1.884644527778083001 ) ) ;
#93258 = CARTESIAN_POINT ( 'NONE',  ( -6.018930129462987999, 9.109503353427070849, 1.199719254218452047 ) ) ;
#93260 = CARTESIAN_POINT ( 'NONE',  ( 6.556269899348222907, -1.302956475595556496, 1.669668561148303976 ) ) ;
#93259 = CARTESIAN_POINT ( 'NONE',  ( -4.446711195602264688, 4.290177271065136466, -0.7216878364870207285 ) ) ;
#93262 = ADVANCED_FACE ( 'NONE', ( #136677 ), #185397, .F. ) ;
#93261 = CARTESIAN_POINT ( 'NONE',  ( 0.6823417656249934904, 10.25520833367472839, 1.181850606188764807 ) ) ;
#93264 = CARTESIAN_POINT ( 'NONE',  ( -5.759181390754928742, 9.941071732514568993, 0.000000000000000000 ) ) ;
#93263 = CARTESIAN_POINT ( 'NONE',  ( 3.351197789220595080, 0.5058271172731694243, -2.028516034726547623 ) ) ;
#93266 = ORIENTED_EDGE ( 'NONE', *, *, #84325, .T. ) ;
#93265 = CARTESIAN_POINT ( 'NONE',  ( 1.940065037515970037, 1.705369652917272383, 0.2570983470618106170 ) ) ;
#93267 = CARTESIAN_POINT ( 'NONE',  ( 6.469000917296717112, -1.638331675554663747, 1.346054232038436105 ) ) ;
#93268 = CARTESIAN_POINT ( 'NONE',  ( 5.931855901178834323, 6.879252291918818152, 1.199719254218462483 ) ) ;
#93269 = DIRECTION ( 'NONE',  ( 0.000000000000000000, 0.000000000000000000, -1.000000000000000000 ) ) ;
#93270 = CARTESIAN_POINT ( 'NONE',  ( 0.3282377607281070087, 0.8236645496846426440, 1.224999999999953904 ) ) ;
#93271 = CARTESIAN_POINT ( 'NONE',  ( 7.005920419302681168, -8.176248043968630697, -6.451695228974969609 ) ) ;
#93272 = CARTESIAN_POINT ( 'NONE',  ( 5.331380718671758778, 7.243030143248949670, -1.599625672291256295 ) ) ;
#93273 = DIRECTION ( 'NONE',  ( 0.000000000000000000, 0.000000000000000000, 1.000000000000000000 ) ) ;
#93274 = CARTESIAN_POINT ( 'NONE',  ( 2.402729293200474459, -0.3110027565414590356, -1.784399550462684392 ) ) ;
#93275 = CARTESIAN_POINT ( 'NONE',  ( 2.381428537494710618, 5.930083727052461562, 0.7998128361456462443 ) ) ;
#93276 = VERTEX_POINT ( 'NONE', #21804 ) ;
#93277 = CARTESIAN_POINT ( 'NONE',  ( 6.073126464278658432, 6.050012061272033392, 0.000000000000000000 ) ) ;
#93278 = CARTESIAN_POINT ( 'NONE',  ( 3.246531836744088295, 1.767876921188500150, 0.3942315000180166562 ) ) ;
#93279 = CARTESIAN_POINT ( 'NONE',  ( 6.639320575229248789, 2.444019389566108647, 2.379739370560208567 ) ) ;
#93280 = CARTESIAN_POINT ( 'NONE',  ( -10.91804383151480806, -8.407420853759271395, 0.1905751639681790843 ) ) ;
#93281 = CARTESIAN_POINT ( 'NONE',  ( 4.103641366189806128, 7.455328040159560743, 0.6459977421944228526 ) ) ;
#93282 = VERTEX_POINT ( 'NONE', #86844 ) ;
#93283 = AXIS2_PLACEMENT_3D ( 'NONE', #95938, #80733, #62345 ) ;
#93284 = CARTESIAN_POINT ( 'NONE',  ( 3.912436197073854593, 0.6682525715841195479, 1.737132965711101873 ) ) ;
#93285 = EDGE_CURVE ( 'NONE', #152385, #121606, #2359, .T. ) ;
#93286 = CARTESIAN_POINT ( 'NONE',  ( 1.616650230726389248, 0.1894562617417178962, 1.906227014244334717 ) ) ;
#93287 = CARTESIAN_POINT ( 'NONE',  ( 0.3932109892899987580, 1.349039491128176449, 1.230163767592551638 ) ) ;
#93288 = CARTESIAN_POINT ( 'NONE',  ( -11.96217875511318240, 13.82854366578976979, 0.9561995067075053090 ) ) ;
#93289 = CARTESIAN_POINT ( 'NONE',  ( -10.72841194583914515, 4.501991598509155423, -5.277862265383093998 ) ) ;
#93290 = CARTESIAN_POINT ( 'NONE',  ( 5.279289985772466665, 7.652873027719338417, 1.222721368963412214 ) ) ;
#93291 = CARTESIAN_POINT ( 'NONE',  ( -11.43195036480940452, 9.944755037147515964, 3.649565797774462883 ) ) ;
#93292 = LINE ( 'NONE', #59689, #1461 ) ;
#93293 = CARTESIAN_POINT ( 'NONE',  ( -3.307826292054316664, 4.882216645528547616, -1.443375672974059665 ) ) ;
#93294 = CARTESIAN_POINT ( 'NONE',  ( 8.622622508611357262, 9.162073802909148412, -0.7216878364870197293 ) ) ;
#93295 = CARTESIAN_POINT ( 'NONE',  ( 6.297704708030454235, -1.423956832742166112, -1.360762174370538258 ) ) ;
#93296 = CARTESIAN_POINT ( 'NONE',  ( -3.716906668440817185, 7.488141546489591072, 0.7998128361456341429 ) ) ;
#93297 = CARTESIAN_POINT ( 'NONE',  ( -9.499668754396999759, -7.215568602690300537, -0.07933194018451479590 ) ) ;
#93298 = CARTESIAN_POINT ( 'NONE',  ( 0.5508686287750690358, -1.767239575335936230, -1.116659500934626514 ) ) ;
#93299 = CARTESIAN_POINT ( 'NONE',  ( 8.457588896826466751, 8.761608555919362828, 1.040834085586084257E-14 ) ) ;
#93300 = CARTESIAN_POINT ( 'NONE',  ( 5.631840744973369617, -1.222119163988559354, -1.489112003571291476 ) ) ;
#93301 = CARTESIAN_POINT ( 'NONE',  ( -5.042743069279040036, 7.970618449879118828, 1.199719254218464037 ) ) ;
#93302 = CARTESIAN_POINT ( 'NONE',  ( 1.571042225754931465, 0.1381101175703668971, -1.820421783975199048 ) ) ;
#93303 = CARTESIAN_POINT ( 'NONE',  ( 2.526237079854487089, -1.271617311931704686, -1.803507373242494438 ) ) ;
#93304 = CARTESIAN_POINT ( 'NONE',  ( 1.419999999999820961, 7.204077025658620848, -4.238769367544755973 ) ) ;
#93305 = CARTESIAN_POINT ( 'NONE',  ( 0.4570967503451648373, -1.639016809899789040, 0.9851245988263114262 ) ) ;
#93306 = ORIENTED_EDGE ( 'NONE', *, *, #158430, .T. ) ;
#93307 = CARTESIAN_POINT ( 'NONE',  ( 0.7132589462262963753, -1.661971685727476000, -1.056574055910926013 ) ) ;
#93308 = CARTESIAN_POINT ( 'NONE',  ( 2.085399755688497336, -0.8285669363069894100, 1.756555673176816157 ) ) ;
#93309 = ORIENTED_EDGE ( 'NONE', *, *, #100213, .T. ) ;
#93310 = CARTESIAN_POINT ( 'NONE',  ( 0.4388270972612972609, 1.158508728638860230, 1.649830871073371119 ) ) ;
#93312 = CARTESIAN_POINT ( 'NONE',  ( 6.051566885458855793, 1.408179756913958913, 1.216655509429155124 ) ) ;
#93311 = CARTESIAN_POINT ( 'NONE',  ( -4.959250327548641479, 9.007818825440551791, -0.7998128361456362523 ) ) ;
#93313 = CARTESIAN_POINT ( 'NONE',  ( 4.441177836928239309, 7.339068688795062911, 1.199719254218452047 ) ) ;
#93314 = CARTESIAN_POINT ( 'NONE',  ( -7.680942717881084292, -5.294771359305316061, -7.874499448206164764 ) ) ;
#93315 = CARTESIAN_POINT ( 'NONE',  ( -5.311043488251275591, 7.219303374425030562, -1.599625672291256295 ) ) ;
#93316 = CARTESIAN_POINT ( 'NONE',  ( -5.427006627220116286, 9.553534508390610469, -0.7998128361456362523 ) ) ;
#93317 = CARTESIAN_POINT ( 'NONE',  ( 2.296645709751913955, 1.758124065145909798, -1.308193547052277861 ) ) ;
#93318 = CARTESIAN_POINT ( 'NONE',  ( 2.724825686666657809, 6.122787701178987518, 0.000000000000000000 ) ) ;
#93319 = CARTESIAN_POINT ( 'NONE',  ( 7.309781096423290769, 8.557108029695882578, 1.199719254218452935 ) ) ;
#93320 = DIRECTION ( 'NONE',  ( 1.000000000000000000, 0.000000000000000000, -1.465138070926357285E-17 ) ) ;
#93321 = CARTESIAN_POINT ( 'NONE',  ( 2.349991895876184511, 1.825291697999480434, 0.04531359951509549705 ) ) ;
#93322 = CARTESIAN_POINT ( 'NONE',  ( -2.415323921528888196, 5.969628341758991930, 0.7998128361456341429 ) ) ;
#93323 =( GEOMETRIC_REPRESENTATION_CONTEXT ( 3 ) GLOBAL_UNCERTAINTY_ASSIGNED_CONTEXT ( ( #150387 ) ) GLOBAL_UNIT_ASSIGNED_CONTEXT ( ( #171936, #89635, #139448 ) ) REPRESENTATION_CONTEXT ( 'NONE', 'WORKASPACE' ) );
#93324 = CARTESIAN_POINT ( 'NONE',  ( -5.830795741961422252, 7.309361553235873998, -1.292907557591252088 ) ) ;
#93325 = DIRECTION ( 'NONE',  ( 0.000000000000000000, 0.000000000000000000, -1.000000000000000000 ) ) ;
#93326 = CARTESIAN_POINT ( 'NONE',  ( 8.703444544968814256, 12.24143683818393313, -1.199719254218446718 ) ) ;
#93327 = CARTESIAN_POINT ( 'NONE',  ( 0.8383531591091289981, 1.897801360490163569, 0.3304300003270659314 ) ) ;
#93328 = CARTESIAN_POINT ( 'NONE',  ( 5.313317156408340125, -1.655227327604656740, -1.052681782574490743 ) ) ;
#93329 = CARTESIAN_POINT ( 'NONE',  ( -1.500000000000015099, 14.72916666666666252, -0.8660254037844309360 ) ) ;
#93330 = CARTESIAN_POINT ( 'NONE',  ( -8.064402442030170093, 8.302891025323665630, 0.7998128361456602331 ) ) ;
#93331 = CARTESIAN_POINT ( 'NONE',  ( 5.311043488251262268, 7.219303374425030562, -1.599625672291256295 ) ) ;
#93332 = EDGE_CURVE ( 'NONE', #57355, #28244, #46696, .T. ) ;
#93333 = CARTESIAN_POINT ( 'NONE',  ( 5.548420995840112724, -1.728225626343689925, 1.347513067664840358 ) ) ;
#93334 = B_SPLINE_CURVE_WITH_KNOTS ( 'NONE', 3,
 ( #141228, #57795, #140142, #10101 ),
 .UNSPECIFIED., .F., .F.,
 ( 4, 4 ),
 ( 0.0002312911391078497833, 0.0002795137126933823967 ),
 .UNSPECIFIED. ) ;
#93335 = CARTESIAN_POINT ( 'NONE',  ( 4.792970997630896512, 5.550553237779539018, 1.199719254218464037 ) ) ;
#93336 = CARTESIAN_POINT ( 'NONE',  ( 4.205968427668831389, 0.7022645179026367757, -1.947615878368731623 ) ) ;
#93338 = CARTESIAN_POINT ( 'NONE',  ( 1.364683531249988757, 0.9468750003414211358, 0.000000000000000000 ) ) ;
#93337 = DIRECTION ( 'NONE',  ( 0.000000000000000000, 0.000000000000000000, -1.000000000000000000 ) ) ;
#93339 = VERTEX_POINT ( 'NONE', #17546 ) ;
#93340 = CARTESIAN_POINT ( 'NONE',  ( 4.588719013068318198, -0.6136123943910645195, 2.215248572529082693 ) ) ;
#93341 = CARTESIAN_POINT ( 'NONE',  ( 7.944714827928056167, 8.371181508778631652, 0.7216878364870458196 ) ) ;
#93343 = CARTESIAN_POINT ( 'NONE',  ( -1.642778471874998480, -0.4010416661887096224, 2.845375778867863303 ) ) ;
#93342 = CARTESIAN_POINT ( 'NONE',  ( 5.451787166470912993, 6.493411461371761284, -1.082531754730548412 ) ) ;
#93344 = CARTESIAN_POINT ( 'NONE',  ( 6.620655732516643965, 2.083750514537034970, 2.135603474206409835 ) ) ;
#93345 = CARTESIAN_POINT ( 'NONE',  ( -5.912237504011027767, 9.055304967058290799, 1.199719254218454489 ) ) ;
#93346 = CARTESIAN_POINT ( 'NONE',  ( 4.681548850490841573, -0.9142078566968904196, 1.713296222823880166 ) ) ;
#93347 = VERTEX_POINT ( 'NONE', #71633 ) ;
#93348 = CARTESIAN_POINT ( 'NONE',  ( 8.365017589507326434, 12.70301158782650397, -0.7216878364870338292 ) ) ;
#93349 = EDGE_LOOP ( 'NONE', ( #1832, #30946, #161495, #196620 ) ) ;
#93350 = CARTESIAN_POINT ( 'NONE',  ( 4.623256175466385010, 1.666654777633369555, 0.9376445158523971646 ) ) ;
#93351 = CARTESIAN_POINT ( 'NONE',  ( 6.317413179709785886, -0.2053877530918957195, 1.712446389806308256 ) ) ;
#93352 = CARTESIAN_POINT ( 'NONE',  ( 4.944546133779973651, -1.457238331152037825, 1.394083050251286870 ) ) ;
#93354 = CARTESIAN_POINT ( 'NONE',  ( -9.748756651352278979, 4.000007913748506283, -7.301653494139321410 ) ) ;
#93353 = CARTESIAN_POINT ( 'NONE',  ( -9.667127221743832877, 11.23706883257798772, 1.199719254218462483 ) ) ;
#93355 = CARTESIAN_POINT ( 'NONE',  ( -3.285556943750000070, -0.1093749995220438809, 0.000000000000000000 ) ) ;
#93357 = CARTESIAN_POINT ( 'NONE',  ( 0.4086181399716379281, 1.536643064871806574, 0.8779792868154213670 ) ) ;
#93356 = CARTESIAN_POINT ( 'NONE',  ( 1.289138792185164251, 1.584031432202914313, 1.364508995882382170 ) ) ;
#93358 = CARTESIAN_POINT ( 'NONE',  ( 6.293592298849589817, 1.492257802130890765, -1.356297202127904944 ) ) ;
#93359 = MANIFOLD_SOLID_BREP ( 'Fillet4', #178018 ) ;
#93361 = CARTESIAN_POINT ( 'NONE',  ( 3.433774379101984575, 1.031038968642459475, -2.047360584804863493 ) ) ;
#93360 = CARTESIAN_POINT ( 'NONE',  ( 4.492547798081839794, 6.334668079219206049, 1.599625672291262513 ) ) ;
#93362 = CARTESIAN_POINT ( 'NONE',  ( 2.554330413957212276, -1.514043700042773111, -0.8579764065595529843 ) ) ;
#93363 = AXIS2_PLACEMENT_3D ( 'NONE', #72384, #135289, #101698 ) ;
#93364 = CARTESIAN_POINT ( 'NONE',  ( 11.92051736251532823, 11.15180243792678638, -1.381800029228912763 ) ) ;
#93365 = CARTESIAN_POINT ( 'NONE',  ( 0.5613444508567478897, 1.446164810419462432, -0.9560955100236142590 ) ) ;
#93366 = CARTESIAN_POINT ( 'NONE',  ( -4.957638175832625493E-14, 1.734375000341442208, 1.570758158831756068 ) ) ;
#93367 = CARTESIAN_POINT ( 'NONE',  ( 1.328301213181204421, -1.184495032981685014, 1.435421900094263403 ) ) ;
#93368 = CARTESIAN_POINT ( 'NONE',  ( 2.401036581340802556, 0.4739146800750834165, 2.118683212603386767 ) ) ;
#93369 = CARTESIAN_POINT ( 'NONE',  ( 3.995327539805045181, -0.3399590882401174463, 1.987497567597557468 ) ) ;
#93370 = CARTESIAN_POINT ( 'NONE',  ( 4.281250000000002665, 0.7852924748302082536, 1.895863743163987980 ) ) ;
#93371 = CARTESIAN_POINT ( 'NONE',  ( 0.7499999999999885647, 1.347916667349485786, -1.299038105676652899 ) ) ;
#93372 = CARTESIAN_POINT ( 'NONE',  ( 0.4285742275551830960, 1.842496385298073580, 0.5622912056609475906 ) ) ;
#93373 = CARTESIAN_POINT ( 'NONE',  ( -1.364683531250010295, 14.63020833367473550, 0.7879004041258445001 ) ) ;
#93374 = CARTESIAN_POINT ( 'NONE',  ( 3.270003694065525046, 0.5362613544047705183, -2.155619276402853224 ) ) ;
#93375 = ORIENTED_EDGE ( 'NONE', *, *, #193499, .F. ) ;
#93376 = CARTESIAN_POINT ( 'NONE',  ( 1.224999999999974998, 2.416666667349527842, 0.7072540797572656190 ) ) ;
#93377 = CARTESIAN_POINT ( 'NONE',  ( 9.101601193475611140, 9.512956235343358102, -0.7998128361456221525 ) ) ;
#93378 = EDGE_CURVE ( 'NONE', #168625, #165933, #46857, .T. ) ;
#93379 = CARTESIAN_POINT ( 'NONE',  ( -1.402160292154681736E-14, -0.9281249996585830830, 1.575800808251672791 ) ) ;
#93380 = CARTESIAN_POINT ( 'NONE',  ( -0.09271296656673803926, -0.4979868145295326953, -2.173146351408902888 ) ) ;
#93381 = CARTESIAN_POINT ( 'NONE',  ( 4.281663391851794565, -1.878042059144067633, 0.5673916069991249422 ) ) ;
#93383 = CARTESIAN_POINT ( 'NONE',  ( -6.236387472606153892, 8.298871356172400127, -1.443375672974059665 ) ) ;
#93382 = CARTESIAN_POINT ( 'NONE',  ( 3.063252641683779753, 5.661212951017999373, 1.199719254218450271 ) ) ;
#93384 = VECTOR ( 'NONE', #156913, 1000.000000000000000 ) ;
#93385 = CARTESIAN_POINT ( 'NONE',  ( -1.393602545685228788, 4.337953148244114487, 0.1272763605452716384 ) ) ;
#93386 = CARTESIAN_POINT ( 'NONE',  ( 5.958357971250668683, 0.9089415708923481718, 2.071969630155451547 ) ) ;
#93387 = CARTESIAN_POINT ( 'NONE',  ( 2.541531169099729759, 1.886825176844410645, -0.8337591773379445792 ) ) ;
#93388 = CARTESIAN_POINT ( 'NONE',  ( -6.579784621333750749, 6.570836901177822931, 0.7998128361456341429 ) ) ;
#93389 = ORIENTED_EDGE ( 'NONE', *, *, #167734, .T. ) ;
#93390 = CARTESIAN_POINT ( 'NONE',  ( 0.7499999999999885647, 2.347916667349486453, -1.299038105676652899 ) ) ;
#93391 = CARTESIAN_POINT ( 'NONE',  ( 3.409304255485625657, -0.3681080166235695117, 1.833790788056933962 ) ) ;
#93392 = CARTESIAN_POINT ( 'NONE',  ( 2.601899516932767220, -0.1674142849007881351, 1.726012112926772701 ) ) ;
#93393 = CARTESIAN_POINT ( 'NONE',  ( 6.444889499930222421, -1.758869480593090673, -1.307235502039267860 ) ) ;
#93394 = CARTESIAN_POINT ( 'NONE',  ( 1.466163881440044836, 2.173982691173735216, -0.3780781022180225159 ) ) ;
#93395 = B_SPLINE_CURVE_WITH_KNOTS ( 'NONE', 3,
 ( #102929, #70394, #101862, #166869, #185223, #87743, #53107, #18463, #119240, #198276 ),
 .UNSPECIFIED., .F., .F.,
 ( 4, 3, 3, 4 ),
 ( 8.276099466726772067E-17, 3.125225830659262568E-05, 6.250473674881420159E-05, 0.0001070711423775351414 ),
 .UNSPECIFIED. ) ;
#93396 = CARTESIAN_POINT ( 'NONE',  ( 3.538091169922503276, 0.9737216987566952309, -1.930062384640649054 ) ) ;
#93397 = CARTESIAN_POINT ( 'NONE',  ( 5.595633723370948331, -1.942124712531563491, 0.002075263307293323100 ) ) ;
#93398 = ADVANCED_FACE ( 'NONE', ( #149717 ), #23221, .T. ) ;
#93399 = CARTESIAN_POINT ( 'NONE',  ( 7.904908961251512878, 15.38485759653958240, 9.030111759985443243 ) ) ;
#93400 = DIRECTION ( 'NONE',  ( -0.000000000000000000, -1.000000000000000000, -0.000000000000000000 ) ) ;
#93401 = CARTESIAN_POINT ( 'NONE',  ( 0.07077104593807002908, 0.8175350930016941353, 1.956879683024402183 ) ) ;
#93402 = CARTESIAN_POINT ( 'NONE',  ( -1.360316468750026875, 2.140625000341400685, -4.857225732735059864E-14 ) ) ;
#93403 = CARTESIAN_POINT ( 'NONE',  ( -11.89942855770814134, 12.30000000000000071, -0.7000000000000009548 ) ) ;
#93404 = CARTESIAN_POINT ( 'NONE',  ( -9.124801077197171040, 10.60435499727357289, -1.199719254218441611 ) ) ;
#93405 = CARTESIAN_POINT ( 'NONE',  ( 5.798083248138522272, 9.916180889470295412, 0.7998128361456462443 ) ) ;
#93406 = CARTESIAN_POINT ( 'NONE',  ( 11.96217875511317885, 12.27145633421023518, 0.9561995067075056420 ) ) ;
#93407 = CARTESIAN_POINT ( 'NONE',  ( 3.668406916800326822, -1.225078373119499187, 1.353803248016255178 ) ) ;
#93408 = CARTESIAN_POINT ( 'NONE',  ( 1.764966765715753949, -1.560254191817540992, 1.560848541443552895 ) ) ;
#93409 = ORIENTED_EDGE ( 'NONE', *, *, #16357, .T. ) ;
#93410 = CARTESIAN_POINT ( 'NONE',  ( -3.485854892044998543, 6.120562236477518070, -1.082531754730546636 ) ) ;
#93411 = CARTESIAN_POINT ( 'NONE',  ( -1.642778471874998480, -1.538541666188709245, 2.845375778867863303 ) ) ;
#93412 = CARTESIAN_POINT ( 'NONE',  ( -8.830438121202295321, 9.196599317691152464, -0.7998128361456291469 ) ) ;
#93413 = CARTESIAN_POINT ( 'NONE',  ( 0.8088602503539430444, -0.4949860548154049189, -1.958043583812353550 ) ) ;
#93414 = CARTESIAN_POINT ( 'NONE',  ( 0.7508259783030580836, 2.089789393294994468, 0.3585813216958123606 ) ) ;
#93415 = CARTESIAN_POINT ( 'NONE',  ( 0.000000000000000000, 8.600000000000017408, -0.3999999999999819811 ) ) ;
#93416 = VERTEX_POINT ( 'NONE', #75926 ) ;
#93417 = CARTESIAN_POINT ( 'NONE',  ( -4.749098946536820520, 8.762642214260091933, 0.7998128361456281477 ) ) ;
#93418 = CARTESIAN_POINT ( 'NONE',  ( 2.746734941909965588, -0.3128536233567563163, -1.834277165529672793 ) ) ;
#93419 = CARTESIAN_POINT ( 'NONE',  ( 4.216749469050096621, 4.878294787768598262, -1.199719254218452047 ) ) ;
#93420 = CARTESIAN_POINT ( 'NONE',  ( 0.3917762336288696523, 1.602822130585265015, 1.450656209987542855 ) ) ;
#93421 = CARTESIAN_POINT ( 'NONE',  ( 5.748672702226536479, 1.986101125435947301, -0.3474646712962395911 ) ) ;
#93422 = ORIENTED_EDGE ( 'NONE', *, *, #63875, .F. ) ;
#93423 = CARTESIAN_POINT ( 'NONE',  ( -9.646789991323334590, 11.21334206375407305, 1.199719254218462483 ) ) ;
#93424 = CARTESIAN_POINT ( 'NONE',  ( 4.125493313500066428, -1.746467973620144942, 0.5319596651164605339 ) ) ;
#93426 = CARTESIAN_POINT ( 'NONE',  ( -5.796555320980813164, 6.214368590181693186, -1.006237437275556257 ) ) ;
#93425 = CARTESIAN_POINT ( 'NONE',  ( -4.980641328173854632, 6.904110530993182948, 1.599625672291263179 ) ) ;
#93427 = CARTESIAN_POINT ( 'NONE',  ( 6.225987253121650689, 7.022442755726078900, -1.008712875586889712 ) ) ;
#93428 = CARTESIAN_POINT ( 'NONE',  ( 6.151720201709268920, -0.2930281871833945173, -1.994563951915592881 ) ) ;
#93429 = CARTESIAN_POINT ( 'NONE',  ( 5.841722611436679813, 1.839261846420519930, 0.08593139445873398952 ) ) ;
#93430 = CARTESIAN_POINT ( 'NONE',  ( -10.99681319029664728, -5.196788179137224795, 0.2733121965684452426 ) ) ;
#93431 = CARTESIAN_POINT ( 'NONE',  ( 4.090657727307928759, -2.282307194306469444, -0.3406017358680757390 ) ) ;
#93432 = CARTESIAN_POINT ( 'NONE',  ( 5.559725510055676168, 8.644040974110419384, 1.199719254218451159 ) ) ;
#93433 = CARTESIAN_POINT ( 'NONE',  ( 6.696550776676711614, -0.5693818166121329405, -2.085215994158528208 ) ) ;
#93434 = CARTESIAN_POINT ( 'NONE',  ( 5.133733721068893807, 9.141106441222381918, 1.040834085586084257E-14 ) ) ;
#93435 = CARTESIAN_POINT ( 'NONE',  ( 2.261185778363482779, 1.904153404235246594, -0.3810316102009890238 ) ) ;
#93436 = VECTOR ( 'NONE', #114152, 1000.000000000000000 ) ;
#93437 = CARTESIAN_POINT ( 'NONE',  ( 5.483857608503296177, 2.120574376644312586, 0.8868611222285858187 ) ) ;
#93438 = FACE_OUTER_BOUND ( 'NONE', #104424, .T. ) ;
#93439 = CARTESIAN_POINT ( 'NONE',  ( -7.761116589180078407, 8.019333873657032541, 0.000000000000000000 ) ) ;
#93440 = CARTESIAN_POINT ( 'NONE',  ( 4.416781281874038179, 1.710313510141375115, 0.7581657270378170388 ) ) ;
#93441 = VERTEX_POINT ( 'NONE', #158262 ) ;
#93445 = EDGE_CURVE ( 'NONE', #47959, #52032, #157396, .T. ) ;
#93444 = CARTESIAN_POINT ( 'NONE',  ( -5.743814354044916470, 6.730146830254374990, -1.199719254218453823 ) ) ;
#93443 = CARTESIAN_POINT ( 'NONE',  ( -1.499999999999997780, 1.931250000682817269, 0.000000000000000000 ) ) ;
#93442 = CARTESIAN_POINT ( 'NONE',  ( 2.179812656587180264, 1.874749209517186710, -0.3766967574026017229 ) ) ;
#93446 = CARTESIAN_POINT ( 'NONE',  ( 3.633602750639616019, -2.039237483250630589, 0.8441791899983088765 ) ) ;
#93447 = CARTESIAN_POINT ( 'NONE',  ( -1.752700365193352367E-14, 0.7500000006828075882, -1.414508159514589636 ) ) ;
#93448 = CARTESIAN_POINT ( 'NONE',  ( 6.983263157960335477, 6.035714437257905018, 2.641087593604172667 ) ) ;
#93449 = CARTESIAN_POINT ( 'NONE',  ( 5.194182247366868843, 8.113610817686430110, 1.082531754730548412 ) ) ;
#93450 = CARTESIAN_POINT ( 'NONE',  ( -4.787437638956920871, 8.599444655509458357, -0.7216878364870338292 ) ) ;
#93451 = CARTESIAN_POINT ( 'NONE',  ( 1.739464312186237871, -1.425129977898047740, -1.362296117697106013 ) ) ;
#93452 = EDGE_CURVE ( 'NONE', #202678, #194213, #109222, .T. ) ;
#93453 = CARTESIAN_POINT ( 'NONE',  ( 2.046342449252246620, 0.8823731130137985046, -2.132409122670553270 ) ) ;
#93454 = CARTESIAN_POINT ( 'NONE',  ( 2.840232074097197579, -1.010955899468408248, 1.681206195012739046 ) ) ;
#93455 = CARTESIAN_POINT ( 'NONE',  ( 11.52888687719656957, 11.29423125104975512, 3.331331986263658784 ) ) ;
#93456 = CARTESIAN_POINT ( 'NONE',  ( 6.702015009205530838, 0.7948373677021604022, -1.903462506645931640 ) ) ;
#93457 = CARTESIAN_POINT ( 'NONE',  ( 4.528060117284240071, 5.345453560662148718, 1.082531754730560403 ) ) ;
#93458 = CARTESIAN_POINT ( 'NONE',  ( 3.801970467005914678, -1.040791964576088358, -1.727064642965264740 ) ) ;
#93459 = CARTESIAN_POINT ( 'NONE',  ( 6.052789233858158369, 6.026285292448116948, 0.000000000000000000 ) ) ;
#93460 = EDGE_LOOP ( 'NONE', ( #4636, #90679, #140184, #200702 ) ) ;
#93461 = DIRECTION ( 'NONE',  ( -1.224646799147353454E-16, 0.000000000000000000, -1.000000000000000000 ) ) ;
#93462 = CARTESIAN_POINT ( 'NONE',  ( 9.398826802771546696, 11.98838390803207865, -1.599625672291262513 ) ) ;
#93463 = CARTESIAN_POINT ( 'NONE',  ( 1.920994505713587541, -1.537477318048833475, 1.533119463567463203 ) ) ;
#93464 = CARTESIAN_POINT ( 'NONE',  ( 11.84668730067608600, 13.39999999999998259, 1.319999999999998286 ) ) ;
#93465 = CARTESIAN_POINT ( 'NONE',  ( -6.755832238374201992, 14.48046842839597836, -9.927744211455593160 ) ) ;
#93466 = CARTESIAN_POINT ( 'NONE',  ( 1.393942678861017637, 0.9000000000000014655, -1.636894562288534472 ) ) ;
#93467 = CARTESIAN_POINT ( 'NONE',  ( 1.985418980784030119, 1.286400883397397221, 1.358229366437320618 ) ) ;
#93468 = CARTESIAN_POINT ( 'NONE',  ( 6.098930168602409552, 1.771044849343451633, -1.239067683784184970 ) ) ;
#93470 = CARTESIAN_POINT ( 'NONE',  ( 6.727182134110170075, 7.629137130509032971, 2.310944104600751281 ) ) ;
#93469 = CARTESIAN_POINT ( 'NONE',  ( 0.07775346131144719730, 4.079442786094135798, -2.843586357576178614 ) ) ;
#93471 = CARTESIAN_POINT ( 'NONE',  ( -1.402160292154681736E-14, -0.9281249996585830830, 1.575800808251672791 ) ) ;
#93472 = DIRECTION ( 'NONE',  ( 1.214306433183764966E-17, 1.000000000000000000, 5.200010849845536803E-32 ) ) ;
#93473 = CARTESIAN_POINT ( 'NONE',  ( 2.701700744156261713, 1.353761940859641966, 1.350867010771430898 ) ) ;
#93474 = MECHANICAL_DESIGN_GEOMETRIC_PRESENTATION_REPRESENTATION (  '', ( #114243 ), #72718 ) ;
#93475 = CARTESIAN_POINT ( 'NONE',  ( 4.047515533282939337, 0.5961193180711570339, -1.666553171763493602 ) ) ;
#93476 = CARTESIAN_POINT ( 'NONE',  ( 1.629408300089076889, -0.2329066467734330903, 1.897959532673603844 ) ) ;
#93477 = CARTESIAN_POINT ( 'NONE',  ( -5.901876940650454095, 5.779944607047298177, -0.7998128361456291469 ) ) ;
#93478 = CARTESIAN_POINT ( 'NONE',  ( 0.1103573706816539240, 1.834011727325855379, 0.5536052920952787559 ) ) ;
#93479 = CARTESIAN_POINT ( 'NONE',  ( -1.402160292154681736E-14, -0.4124999999999747202, -1.732050807568870754 ) ) ;
#93480 = CARTESIAN_POINT ( 'NONE',  ( 1.135311898753359472, -0.04898221611688948623, -2.069941200615910581 ) ) ;
#93481 = CARTESIAN_POINT ( 'NONE',  ( 1.364683531249986537, -1.073958332991911790, 0.7879004041258500513 ) ) ;
#93482 = CARTESIAN_POINT ( 'NONE',  ( 5.330866702616011921, 0.1386157390740362649, 1.865562100978317206 ) ) ;
#93483 = CARTESIAN_POINT ( 'NONE',  ( 1.822601884235462766, 1.703052241681313861, 0.6583118566880485911 ) ) ;
#93485 = CARTESIAN_POINT ( 'NONE',  ( 4.605417112443645600, 8.360468292628990383, 0.2083848827989076002 ) ) ;
#93484 = CARTESIAN_POINT ( 'NONE',  ( 6.024089167411393220, -1.222679950896175205, -1.837027303407394507 ) ) ;
#93486 = CARTESIAN_POINT ( 'NONE',  ( -0.6823417656250003738, -1.032291666325242607, -1.181850606188749264 ) ) ;
#93487 = CARTESIAN_POINT ( 'NONE',  ( 3.402832357982612077, 0.4983898525147857361, 2.001458950477213339 ) ) ;
#93488 = CARTESIAN_POINT ( 'NONE',  ( -5.716734326456539783, 9.821273814174633188, -0.7998128361456231517 ) ) ;
#93489 = CARTESIAN_POINT ( 'NONE',  ( -11.41381675112453387, 13.40000000000000036, -3.704697986577184299 ) ) ;
#93490 = CARTESIAN_POINT ( 'NONE',  ( 9.426996880203592610, 9.892584536526015881, -0.7998128361456281477 ) ) ;
#93491 = CARTESIAN_POINT ( 'NONE',  ( 1.435158330144293393, 3.628467426565245901, -0.4529249069356899304 ) ) ;
#93492 = CARTESIAN_POINT ( 'NONE',  ( -0.9999999999999988898, 5.868705557303652398, -4.125226524755048807 ) ) ;
#93493 = CARTESIAN_POINT ( 'NONE',  ( 5.657495238652423097, 9.822437888394988548, 0.000000000000000000 ) ) ;
#93494 = ORIENTED_EDGE ( 'NONE', *, *, #44939, .T. ) ;
#93495 = CARTESIAN_POINT ( 'NONE',  ( 5.600075274486990828, 0.8424382930321882013, -1.891409743246947217 ) ) ;
#93496 = CARTESIAN_POINT ( 'NONE',  ( 1.364683531249986537, -0.3239583329919163424, 0.7879004041258500513 ) ) ;
#93497 = CARTESIAN_POINT ( 'NONE',  ( 2.811983876933336735, -2.138515761559431461, 0.3140893029918228052 ) ) ;
#93498 = CARTESIAN_POINT ( 'NONE',  ( -4.627894000755552462, 8.353582960325299567, 0.3099817540855500653 ) ) ;
#93499 = CARTESIAN_POINT ( 'NONE',  ( 3.686198542540094714, 1.123799323442754572, 1.677924191584168501 ) ) ;
#93500 = CARTESIAN_POINT ( 'NONE',  ( 6.720655732516665815, 3.683894443391816154, 2.687682123607849416 ) ) ;
#93501 = EDGE_LOOP ( 'NONE', ( #25827, #171878, #120524, #3440 ) ) ;
#93503 = CARTESIAN_POINT ( 'NONE',  ( 6.317736394288122170, 10.31451686007074997, 0.7216878364870438212 ) ) ;
#93502 = CARTESIAN_POINT ( 'NONE',  ( 3.475000000000000533, -0.9041666666666666741, 2.006292185433948827 ) ) ;
#93504 = CARTESIAN_POINT ( 'NONE',  ( -6.474900878978163021, 9.711745571186627402, -1.199719254218452047 ) ) ;
#93505 = CARTESIAN_POINT ( 'NONE',  ( 1.885954221117658092, -2.015980662343511032, 0.05432778586660082232 ) ) ;
#93507 = CARTESIAN_POINT ( 'NONE',  ( 6.304242050522723240, 1.625252681175231029, -1.470355468214133321 ) ) ;
#93506 = CARTESIAN_POINT ( 'NONE',  ( -5.199715606040888005, 6.025088614257851027, -1.199719254218446718 ) ) ;
#93508 = CARTESIAN_POINT ( 'NONE',  ( -0.7500000000000215383, 4.722916667349482012, 1.299038105676671107 ) ) ;
#93509 = CARTESIAN_POINT ( 'NONE',  ( 4.306835718904429733, -0.4242474483713705169, -1.864571660543254739 ) ) ;
#93510 = CARTESIAN_POINT ( 'NONE',  ( -3.789667630219657912, 4.380032642466370696, 1.199719254218462483 ) ) ;
#93511 = CARTESIAN_POINT ( 'NONE',  ( 5.951666246274797345, 7.966696592119163256, 1.443375672974062551 ) ) ;
#93513 = CARTESIAN_POINT ( 'NONE',  ( 3.814077502958601595, 1.076299547611740293, -1.704950967544152984 ) ) ;
#93512 = CARTESIAN_POINT ( 'NONE',  ( -8.717529583462656717, 11.19353715217169309, 1.443375672974064550 ) ) ;
#93514 = CARTESIAN_POINT ( 'NONE',  ( -0.6823417656250003738, 13.46354166700806942, 1.181850606188754593 ) ) ;
#93515 = CARTESIAN_POINT ( 'NONE',  ( 5.121954690102882957, -0.9251313946504275965, -1.455449238992040373 ) ) ;
#93516 = CARTESIAN_POINT ( 'NONE',  ( 7.686546744304875389, 7.932335721302671949, 0.7998128361456291469 ) ) ;
#93517 = CARTESIAN_POINT ( 'NONE',  ( 3.195971524519376494, 4.751719416737803847, -1.599625672291262513 ) ) ;
#93518 = CARTESIAN_POINT ( 'NONE',  ( -6.770610912236891821, -7.154544010627095219, -6.663994888585869525 ) ) ;
#93519 = CARTESIAN_POINT ( 'NONE',  ( 4.534354090784907143, 1.834037221929617711, 0.3668691113338993226 ) ) ;
#93520 =( BOUNDED_CURVE ( )  B_SPLINE_CURVE ( 3, ( #193649, #155839, #190446, #25815 ),
 .UNSPECIFIED., .F., .T. ) 
 B_SPLINE_CURVE_WITH_KNOTS ( ( 4, 4 ),
 ( 4.148111545443665449, 4.712388980384681680 ),
 .UNSPECIFIED. ) 
 CURVE ( )  GEOMETRIC_REPRESENTATION_ITEM ( )  RATIONAL_B_SPLINE_CURVE ( ( 1.000000000000000000, 0.9736414627471525751, 0.9736414627471525751, 1.000000000000000000 ) ) 
 REPRESENTATION_ITEM ( '' )  );
#93521 = DIRECTION ( 'NONE',  ( -0.6507913734559640506, -0.7592566023653003482, 0.000000000000000000 ) ) ;
#93522 = CARTESIAN_POINT ( 'NONE',  ( 0.8661811918178536907, -2.060611401584189650, 0.1992402130865863485 ) ) ;
#93523 = CARTESIAN_POINT ( 'NONE',  ( 0.000000000000000000, 13.49999999999999822, 0.000000000000000000 ) ) ;
#93524 = VERTEX_POINT ( 'NONE', #191790 ) ;
#93525 = CARTESIAN_POINT ( 'NONE',  ( 6.322923312362423331, 1.337123347216003788, -1.222299563558794766 ) ) ;
#93526 = CARTESIAN_POINT ( 'NONE',  ( 4.203910148689107729, 7.062256385849379647, -1.199719254218448494 ) ) ;
#93527 =( NAMED_UNIT ( * ) PLANE_ANGLE_UNIT ( ) SI_UNIT ( $, .RADIAN. ) );
#93528 = CARTESIAN_POINT ( 'NONE',  ( 0.6503002719215627003, 1.784868618687754926, 0.3088405841149675091 ) ) ;
#93529 = CARTESIAN_POINT ( 'NONE',  ( 5.112833325684902341, 7.058334528089426740, -1.443375672974078761 ) ) ;
#93530 = LINE ( 'NONE', #111966, #72969 ) ;
#93531 = VERTEX_POINT ( 'NONE', #171289 ) ;
#93533 = CARTESIAN_POINT ( 'NONE',  ( 9.088043039861931405, 9.497138389460751284, 1.040834085586084257E-14 ) ) ;
#93532 = CARTESIAN_POINT ( 'NONE',  ( 1.099968687278202406, 0.7983322178258808188, -1.792280776234013828 ) ) ;
#93534 = CARTESIAN_POINT ( 'NONE',  ( 4.763251566037994600, 1.785832754541897049, -0.6935334960865118248 ) ) ;
#93535 = CARTESIAN_POINT ( 'NONE',  ( 5.178851490740248309, 5.144340948726068063, 0.7216878364870010776 ) ) ;
#93536 = CARTESIAN_POINT ( 'NONE',  ( -5.520246714036333380, 7.462180650995058784, 1.249303437716933196 ) ) ;
#93537 =( NAMED_UNIT ( * ) SI_UNIT ( $, .STERADIAN. ) SOLID_ANGLE_UNIT ( ) );
#93539 = ORIENTED_EDGE ( 'NONE', *, *, #201026, .T. ) ;
#93538 = CARTESIAN_POINT ( 'NONE',  ( 4.311129659465574804, 7.013106455143060636, -1.082531754730548412 ) ) ;
#93540 = CARTESIAN_POINT ( 'NONE',  ( -8.026063749610043985, 12.30756544127966912, -0.7216878364870267237 ) ) ;
#93541 = CARTESIAN_POINT ( 'NONE',  ( 2.237400686453533183, -1.931180590798301955, 0.9714560045831142077 ) ) ;
#93542 = CARTESIAN_POINT ( 'NONE',  ( -5.093022980588950865, 5.970890227889075419, -1.199719254218453823 ) ) ;
#93543 = CARTESIAN_POINT ( 'NONE',  ( 5.695833931516881776, 9.659240330162777610, -0.7216878364870458196 ) ) ;
#93544 = CARTESIAN_POINT ( 'NONE',  ( -0.1753031400193918454, -0.9122597987226389593, -1.912455998546586544 ) ) ;
#93545 = CARTESIAN_POINT ( 'NONE',  ( 4.735264887803245060, -1.668767028523497675, 0.7406363711058363553 ) ) ;
#93546 = CARTESIAN_POINT ( 'NONE',  ( 8.831606621645018862, 13.23576961196815205, 7.655963609598713582 ) ) ;
#93547 = CARTESIAN_POINT ( 'NONE',  ( 1.071480742727632940, 1.901078573484305201, -0.5215319001752088957 ) ) ;
#93548 = CARTESIAN_POINT ( 'NONE',  ( 4.043146078444789460, 0.09904687726844901841, 1.909973672635330910 ) ) ;
#93549 = ORIENTED_EDGE ( 'NONE', *, *, #162643, .F. ) ;
#93550 = FACE_OUTER_BOUND ( 'NONE', #106242, .T. ) ;
#93551 = CARTESIAN_POINT ( 'NONE',  ( 4.351979406267578732, -0.7558620137302939357, 1.818942442720396624 ) ) ;
#93552 = ORIENTED_EDGE ( 'NONE', *, *, #70698, .F. ) ;
#93553 = CARTESIAN_POINT ( 'NONE',  ( 6.022988683830415191, -1.827201308531730017, 0.6583088893449047241 ) ) ;
#93554 = VERTEX_POINT ( 'NONE', #88996 ) ;
#93555 = CARTESIAN_POINT ( 'NONE',  ( -6.180537922983287302, 8.303989891604203422, -1.599625672291271394 ) ) ;
#93557 = CARTESIAN_POINT ( 'NONE',  ( 5.994406619193555663, -1.133004004027007294, 1.792352430775605798 ) ) ;
#93556 = CARTESIAN_POINT ( 'NONE',  ( -5.659602779061863487, 5.567567761852417085, 0.7998128361456281477 ) ) ;
#93558 = CARTESIAN_POINT ( 'NONE',  ( 7.471952054462756010, 7.889901283060952508, 0.7216878364870267237 ) ) ;
#93560 = VERTEX_POINT ( 'NONE', #92211 ) ;
#93559 = CARTESIAN_POINT ( 'NONE',  ( 4.494721087910216184, -1.855708629272670773, -0.4612273479895279138 ) ) ;
#93561 = CARTESIAN_POINT ( 'NONE',  ( 6.983263157960366563, 2.056882910316945701, 2.252511522010155698 ) ) ;
#93562 = CARTESIAN_POINT ( 'NONE',  ( 4.913904330310220558, 4.697586238308844919, 0.000000000000000000 ) ) ;
#93563 = AXIS2_PLACEMENT_3D ( 'NONE', #19455, #181959, #149479 ) ;
#93564 = CARTESIAN_POINT ( 'NONE',  ( 9.601932014265541326, 4.115787152683093808, -7.121345992675182757 ) ) ;
#93565 = CARTESIAN_POINT ( 'NONE',  ( 5.584640334855505373, -1.275214923639787834, 1.557698558565046243 ) ) ;
#93566 = FACE_OUTER_BOUND ( 'NONE', #1193, .T. ) ;
#93567 = CARTESIAN_POINT ( 'NONE',  ( 6.568987803155795113, -1.671525225137669102, -0.7347104647430282576 ) ) ;
#93568 = CARTESIAN_POINT ( 'NONE',  ( 1.715371797147913435, -1.774658612622433296, -1.066089629202723765 ) ) ;
#93569 = CARTESIAN_POINT ( 'NONE',  ( -9.002250809794013264, 9.604973487622245898, -0.7216878364870267237 ) ) ;
#93570 =( BOUNDED_CURVE ( )  B_SPLINE_CURVE ( 2, ( #83852, #135823, #197602, #69720, #115367, #34041, #166175, #200782, #17764, #1510, #52434, #67576, #118560, #51372, #199726, #117495, #184544, #36164, #102243, #152071, #3641, #201848, #119629, #122869, #54564, #123927, #186685, #137961, #188830, #5774, #7931, #58831, #189895, #90277, #40465, #172596, #106568, #75083, #104390, #74019, #140109, #206136, #203981, #57766, #24174, #120710, #70779, #88134, #38313, #170437, #155271, #141196, #22025, #156346, #91356, #154205, #55628, #71853, #37245, #20962, #105477, #171510, #41537, #23103, #107648, #207207, #89219, #124985, #121785, #173680, #169378 ),
 .UNSPECIFIED., .F., .T. ) 
 B_SPLINE_CURVE_WITH_KNOTS ( ( 3, 2, 2, 2, 2, 2, 2, 2, 2, 2, 2, 2, 2, 2, 2, 2, 2, 2, 2, 2, 2, 2, 2, 2, 2, 2, 2, 2, 2, 2, 2, 2, 2, 2, 2, 3 ),
 ( 0.1345121972685508482, 0.1375000000000000111, 0.1416666666666666630, 0.1458333333333333426, 0.1499999999999999944, 0.1541666666666666741, 0.1583333333333333259, 0.1625000000000000056, 0.1666666666666666574, 0.1708333333333333370, 0.1749999999999999889, 0.1791666666666666685, 0.1833333333333333204, 0.1875000000000000000, 0.1916666666666666796, 0.1958333333333333315, 0.2000000000000000111, 0.2041666666666666630, 0.2083333333333333426, 0.2124999999999999944, 0.2166666666666666741, 0.2208333333333333259, 0.2250000000000000056, 0.2291666666666666574, 0.2333333333333333370, 0.2374999999999999889, 0.2416666666666666685, 0.2458333333333333204, 0.2500000000000000000, 0.2541666666666666519, 0.2583333333333333592, 0.2625000000000000111, 0.2666666666666666630, 0.2708333333333333148, 0.2750000000000000222, 0.2787508327459756741 ),
 .UNSPECIFIED. ) 
 CURVE ( )  GEOMETRIC_REPRESENTATION_ITEM ( )  RATIONAL_B_SPLINE_CURVE ( ( 0.9456386119390516320, 0.9039304805157636347, 1.000000000000000000, 0.8660254037844387076, 1.000000000000000000, 0.8660254037844387076, 1.000000000000000000, 0.8660254037844387076, 1.000000000000000000, 0.8660254037844387076, 1.000000000000000000, 0.8660254037844387076, 1.000000000000000000, 0.8660254037844387076, 1.000000000000000000, 0.8660254037844387076, 1.000000000000000000, 0.8660254037844387076, 1.000000000000000000, 0.8660254037844387076, 1.000000000000000000, 0.8660254037844387076, 1.000000000000000000, 0.8660254037844387076, 1.000000000000000000, 0.8660254037844387076, 1.000000000000000000, 0.8660254037844387076, 1.000000000000000000, 0.8660254037844387076, 1.000000000000000000, 0.8660254037844387076, 1.000000000000000000, 0.8660254037844387076, 1.000000000000000000, 0.8660254037844387076, 1.000000000000000000, 0.8660254037844387076, 1.000000000000000000, 0.8660254037844387076, 1.000000000000000000, 0.8660254037844387076, 1.000000000000000000, 0.8660254037844387076, 1.000000000000000000, 0.8660254037844387076, 1.000000000000000000, 0.8660254037844387076, 1.000000000000000000, 0.8660254037844387076, 1.000000000000000000, 0.8660254037844387076, 1.000000000000000000, 0.8660254037844387076, 1.000000000000000000, 0.8660254037844387076, 1.000000000000000000, 0.8660254037844387076, 1.000000000000000000, 0.8660254037844387076, 1.000000000000000000, 0.8660254037844387076, 1.000000000000000000, 0.8660254037844387076, 1.000000000000000000, 0.8660254037844387076, 1.000000000000000000, 0.8660254037844387076, 1.000000000000000000, 0.8793960873725932270, 0.9759274250375058468 ) ) 
 REPRESENTATION_ITEM ( '' )  );
#93571 = CARTESIAN_POINT ( 'NONE',  ( -5.295344997983027824, 7.654313019038245791, -1.225062028442117423 ) ) ;
#93572 = CARTESIAN_POINT ( 'NONE',  ( 1.224999999999953015, 1.854166666666720698, 0.7072540797572656190 ) ) ;
#93573 = CARTESIAN_POINT ( 'NONE',  ( 3.285556943750000514, -2.763541666188706891, 1.896917185911906722 ) ) ;
#93574 = CARTESIAN_POINT ( 'NONE',  ( 4.462605117192430804, 8.358123070033169455, 1.040834085586084257E-14 ) ) ;
#93575 = FACE_OUTER_BOUND ( 'NONE', #122409, .T. ) ;
#93576 = ADVANCED_FACE ( 'NONE', ( #139884 ), #109571, .F. ) ;
#93577 = CARTESIAN_POINT ( 'NONE',  ( 6.224601922449876312, 6.434659462379210382, 0.000000000000000000 ) ) ;
#93578 = AXIS2_PLACEMENT_3D ( 'NONE', #114393, #39461, #54644 ) ;
#93579 = CARTESIAN_POINT ( 'NONE',  ( 3.837121167867449945, 4.435395103055503441, 1.199719254218464037 ) ) ;
#93580 = CARTESIAN_POINT ( 'NONE',  ( -1.364683531250014514, 12.15104166700806765, -0.7879004041258335089 ) ) ;
#93581 = CARTESIAN_POINT ( 'NONE',  ( -5.461236948206312114, 5.265864615862458464, 0.7998128361456341429 ) ) ;
#93583 = CARTESIAN_POINT ( 'NONE',  ( -7.130662446144611977, 7.283804040115648526, 0.000000000000000000 ) ) ;
#93582 = CARTESIAN_POINT ( 'NONE',  ( -11.88234649872613602, 11.25660782916751579, -0.9090484974825174813 ) ) ;
#93584 = EDGE_CURVE ( 'NONE', #109578, #22427, #154139, .T. ) ;
#93585 = CARTESIAN_POINT ( 'NONE',  ( 3.586273015720359503, -0.4996269028240771237, 1.660617844614233674 ) ) ;
#93586 = CARTESIAN_POINT ( 'NONE',  ( -3.228813138348844536, 6.918699094715619502, 0.7998128361456341429 ) ) ;
#93587 = CARTESIAN_POINT ( 'NONE',  ( 1.762639944428091576, -0.7413553172891698129, -1.933158369416078770 ) ) ;
#93588 = CARTESIAN_POINT ( 'NONE',  ( 3.286815299386883549, 1.667571603535710434, -1.304429798788673267 ) ) ;
#93589 = CARTESIAN_POINT ( 'NONE',  ( 6.916630921265960019, 11.22115317478565188, 0.7998128361456462443 ) ) ;
#93590 = CARTESIAN_POINT ( 'NONE',  ( -0.6823417656249969321, 3.967708333674754950, -1.181850606188749264 ) ) ;
#93591 = CARTESIAN_POINT ( 'NONE',  ( 1.129674139269299049, 1.899472608897791348, -0.5201393403096374879 ) ) ;
#93592 = CARTESIAN_POINT ( 'NONE',  ( 5.291954866116698852, 6.573566887673666592, 1.361072633976003310 ) ) ;
#93593 = CARTESIAN_POINT ( 'NONE',  ( 5.504247177468190699, 5.523969249908757817, 0.7216878364870317197 ) ) ;
#93595 = CARTESIAN_POINT ( 'NONE',  ( 0.2637284958507991606, 0.5978344860198721022, -1.816641584731902626 ) ) ;
#93594 = CARTESIAN_POINT ( 'NONE',  ( 3.475000000000000533, -2.274999999999999467, 0.000000000000000000 ) ) ;
#93596 = CARTESIAN_POINT ( 'NONE',  ( 4.259948577007838466, 1.078808246893525391, 2.022540810160260882 ) ) ;
#93597 = CARTESIAN_POINT ( 'NONE',  ( 0.2053145577999641314, -0.4904175937916722128, 1.758528939493007259 ) ) ;
#93598 = CARTESIAN_POINT ( 'NONE',  ( 3.340010735810138520, -1.142844047782382466, -1.533173144288489276 ) ) ;
#93599 = CARTESIAN_POINT ( 'NONE',  ( 5.180097208873055692, 8.201141289397330780, -1.199719254218450271 ) ) ;
#93600 = CARTESIAN_POINT ( 'NONE',  ( 6.222829318548112276, 9.243422724072711816, -1.082531754730537976 ) ) ;
#93601 = CARTESIAN_POINT ( 'NONE',  ( -8.158255747121117452, 10.54105100977322174, 1.599625672291295375 ) ) ;
#93602 = CARTESIAN_POINT ( 'NONE',  ( 2.215092046557234795, 1.614471179978003823, -1.202476892717120105 ) ) ;
#93603 = CARTESIAN_POINT ( 'NONE',  ( 2.448037131198562921, -0.8433605282326918084, 1.771390271482737200 ) ) ;
#93604 = CARTESIAN_POINT ( 'NONE',  ( -9.982881178363895103, 10.54111621771303753, 1.040834085586084257E-14 ) ) ;
#93605 = CARTESIAN_POINT ( 'NONE',  ( -5.526920175865215334, 9.599823971818089774, 0.7998128361456481317 ) ) ;
#93606 = CARTESIAN_POINT ( 'NONE',  ( -11.33171338088452451, 6.586873243287150181, 3.814917260415342959 ) ) ;
#93608 = CARTESIAN_POINT ( 'NONE',  ( 2.975218959772182536, 1.681091501613757533, -0.5536541633112538330 ) ) ;
#93607 = CARTESIAN_POINT ( 'NONE',  ( 5.402318495819277366, 1.583515501651384438, -1.365094957383119700 ) ) ;
#93609 = CARTESIAN_POINT ( 'NONE',  ( -0.3282377607281345422, 0.1138354509981740759, 1.224999999999971667 ) ) ;
#93610 = CARTESIAN_POINT ( 'NONE',  ( 6.421853422025334268, 1.325270252340422061, -1.870170258788282247 ) ) ;
#93611 = CARTESIAN_POINT ( 'NONE',  ( 5.648340061037051107, -1.368025295233719074, 1.075653158840290891 ) ) ;
#93612 = CARTESIAN_POINT ( 'NONE',  ( 8.426556166093362776, 9.789735934319136135, -1.199719254218446718 ) ) ;
#93613 = CARTESIAN_POINT ( 'NONE',  ( -1.499999999999981126, 4.129166666666685082, -0.8660254037844499209 ) ) ;
#93614 = CARTESIAN_POINT ( 'NONE',  ( 5.870364492519208888, -0.4185229733149243292, 1.682389803524992011 ) ) ;
#93615 = COLOUR_RGB ( '', 0.66274510, 0.83137255, 0.94901961) ;
#93616 = CARTESIAN_POINT ( 'NONE',  ( 5.811019572999191141, -1.715256576162796032, 1.331060940585542030 ) ) ;
#93617 = LINE ( 'NONE', #89339, #193345 ) ;
#93618 = CARTESIAN_POINT ( 'NONE',  ( -0.02988430322643093051, -0.9920087411236072628, 1.870552836459241419 ) ) ;
#93619 = CARTESIAN_POINT ( 'NONE',  ( 4.531250000000003553, -0.7852924748302230196, -1.895863743163982429 ) ) ;
#93620 = DIRECTION ( 'NONE',  ( 1.000000000000000000, 3.451266460341926649E-31, 0.000000000000000000 ) ) ;
#93621 = CARTESIAN_POINT ( 'NONE',  ( 3.786086853528514151, -0.9505683805260138897, 1.675471031514904396 ) ) ;
#93622 = CARTESIAN_POINT ( 'NONE',  ( -6.009258394948636914E-15, 11.46875000068279604, -1.732050807568875195 ) ) ;
#93623 = CARTESIAN_POINT ( 'NONE',  ( 6.381102873985867063, -2.030373413249999093, -0.9015990085984818547 ) ) ;
#93624 = ORIENTED_EDGE ( 'NONE', *, *, #198470, .T. ) ;
#93625 = CARTESIAN_POINT ( 'NONE',  ( 0.7499999999999902300, 3.983333333333352488, 1.299038105676669330 ) ) ;
#93626 = CARTESIAN_POINT ( 'NONE',  ( 6.484877546038077867, 6.460111979999551224, 1.040834085586084257E-14 ) ) ;
#93627 = CARTESIAN_POINT ( 'NONE',  ( 2.842673000788879634, 1.232056068812878991, -1.848115600964394867 ) ) ;
#93628 = CARTESIAN_POINT ( 'NONE',  ( -5.914749137557818059, 6.074338953224275528, -0.6118981238392419142 ) ) ;
#93629 = CARTESIAN_POINT ( 'NONE',  ( 7.836249599018724865, 9.205007956019091608, -1.082531754730537976 ) ) ;
#93630 = CARTESIAN_POINT ( 'NONE',  ( -9.775065565328612038, 10.50659070241261794, -0.7216878364870267237 ) ) ;
#93631 = CARTESIAN_POINT ( 'NONE',  ( 6.753369913382843315, 8.011924666102361314, -1.082531754730548412 ) ) ;
#93632 = CARTESIAN_POINT ( 'NONE',  ( 0.4928148368598186946, -2.006445878461552645, 0.2004378712678403507 ) ) ;
#93634 = CARTESIAN_POINT ( 'NONE',  ( 5.336407798562197158, -1.148744492729685707, 1.713005319730724008 ) ) ;
#93633 = CARTESIAN_POINT ( 'NONE',  ( 7.703003830858588863, 12.13858823597705872, -0.7998128361456291469 ) ) ;
#93635 = DIRECTION ( 'NONE',  ( 0.000000000000000000, 0.000000000000000000, 1.000000000000000000 ) ) ;
#93636 = CARTESIAN_POINT ( 'NONE',  ( -15.75000000000000000, 12.30000000000000071, -1.800000000000001155 ) ) ;
#93637 = FILL_AREA_STYLE ('',( #205203 ) ) ;
#93638 = CARTESIAN_POINT ( 'NONE',  ( -0.6823417656250212460, 1.551041667008083769, 1.181850606188755259 ) ) ;
#93639 = CARTESIAN_POINT ( 'NONE',  ( 0.7547153349467434769, -1.490676808382383145, -0.9535711479493594878 ) ) ;
#93640 = CARTESIAN_POINT ( 'NONE',  ( 5.783786074351109363, 1.412321387942861328, -1.005976269456631211 ) ) ;
#93641 = CARTESIAN_POINT ( 'NONE',  ( 5.390116981161272136, -0.4305884537129686662, -1.686203596905116342 ) ) ;
#93642 = CARTESIAN_POINT ( 'NONE',  ( 2.753816761298252036, 2.281055701876167685, -0.2276813034018300430 ) ) ;
#93643 = CARTESIAN_POINT ( 'NONE',  ( -1.402160292154681736E-14, -0.5531249996585814177, -1.575800808251665908 ) ) ;
#93644 = CARTESIAN_POINT ( 'NONE',  ( 2.818100271072516261, 1.733748696238574416, 0.6199764264002775027 ) ) ;
#93645 = ADVANCED_FACE ( 'NONE', ( #155049 ), #41317, .T. ) ;
#93646 = CARTESIAN_POINT ( 'NONE',  ( 7.723341061279088038, 12.16231500480096983, -0.7998128361456291469 ) ) ;
#93647 = CARTESIAN_POINT ( 'NONE',  ( -9.858348327010764578, 3.999999999999995559, 6.855072103023518437 ) ) ;
#93648 = CARTESIAN_POINT ( 'NONE',  ( 2.485134345765506847, 1.670108983700506977, -0.7376146046164517855 ) ) ;
#93649 = CARTESIAN_POINT ( 'NONE',  ( 3.358046224211252095, 0.04667712216412447934, -2.016033814150198999 ) ) ;
#93650 = CARTESIAN_POINT ( 'NONE',  ( -2.440104460335327463, 5.790612937125752424, 1.040834085586084257E-14 ) ) ;
#93651 = CARTESIAN_POINT ( 'NONE',  ( 7.826754997383993384, 14.96923099944252478, -9.976823565866945742 ) ) ;
#93652 = CARTESIAN_POINT ( 'NONE',  ( 3.979594558520031189, 1.983667836772174509, -0.7075980189445835178 ) ) ;
#93653 = CARTESIAN_POINT ( 'NONE',  ( -7.074657228232555717, 7.148188275893099686, 1.040834085586084257E-14 ) ) ;
#93654 = CARTESIAN_POINT ( 'NONE',  ( 9.023309422432060245, 13.48888919738144665, 9.153259163867227599 ) ) ;
#93655 = CARTESIAN_POINT ( 'NONE',  ( 2.084514231050747401, 1.193861083872927109, -1.691280048542340708 ) ) ;
#93656 = CARTESIAN_POINT ( 'NONE',  ( 5.366329872910639232, 5.155139694684188534, 1.040834085586084257E-14 ) ) ;
#93657 = CARTESIAN_POINT ( 'NONE',  ( -2.353626204688216217E-14, 0.9843750003414547534, 1.570758158831764062 ) ) ;
#93659 = B_SPLINE_CURVE_WITH_KNOTS ( 'NONE', 3,
 ( #138797, #69487, #38088, #106335, #104159, #204817, #136665, #7693, #122630, #25019 ),
 .UNSPECIFIED., .F., .F.,
 ( 4, 3, 3, 4 ),
 ( 0.000000000000000000, 3.125366356300422706E-05, 6.250667109586610789E-05, 0.0001104411237298844468 ),
 .UNSPECIFIED. ) ;
#93658 = CARTESIAN_POINT ( 'NONE',  ( 4.635462950926918957, -0.1032030737609032217, 2.118083805499561656 ) ) ;
#93660 = ITEM_DEFINED_TRANSFORMATION ( 'NONE', 'NONE', #3876,  #200407 ) ;
#93661 = CARTESIAN_POINT ( 'NONE',  ( 1.383290355582541542, 1.780271273866357529, -0.7366933121468289825 ) ) ;
#93662 = EDGE_LOOP ( 'NONE', ( #125599, #189515 ) ) ;
#93663 = CARTESIAN_POINT ( 'NONE',  ( -6.005335696210345020, 5.970922831858983315, 0.7998128361456281477 ) ) ;
#93664 = CARTESIAN_POINT ( 'NONE',  ( 7.072549687823125097, 11.40305840243567381, -0.7998128361456291469 ) ) ;
#93665 = CARTESIAN_POINT ( 'NONE',  ( 6.170369307550823912, 7.331757292631694511, 1.082531754730549967 ) ) ;
#93666 = CARTESIAN_POINT ( 'NONE',  ( 1.064774733001451423, 2.800000000000024247, -1.047209855801954248 ) ) ;
#93667 = CARTESIAN_POINT ( 'NONE',  ( -5.416646063859567484, 6.278174148379618735, 1.199719254218450271 ) ) ;
#93668 = CARTESIAN_POINT ( 'NONE',  ( 6.011998765391792787, -0.7129019540204998284, 1.997330473063135381 ) ) ;
#93669 = CARTESIAN_POINT ( 'NONE',  ( 1.219907122830860446, -2.054670964268051847, 0.4612076382107341277 ) ) ;
#93670 = CARTESIAN_POINT ( 'NONE',  ( -4.793689830883590020, 7.750332681742931662, 1.199719254218452935 ) ) ;
#93671 = CARTESIAN_POINT ( 'NONE',  ( 8.158255747121103241, 10.54105100977322174, 1.599625672291281386 ) ) ;
#93672 = CARTESIAN_POINT ( 'NONE',  ( 6.297681919442434939, -1.347125180836796998, -1.284110876681610725 ) ) ;
#93673 = CARTESIAN_POINT ( 'NONE',  ( 6.425674737872927089, 9.584038729905381970, -1.199719254218440723 ) ) ;
#93674 = EDGE_CURVE ( 'NONE', #15203, #109724, #105601, .T. ) ;
#93675 = DIRECTION ( 'NONE',  ( 1.276756478318932585E-15, -1.000000000000000000, 1.665334536937738262E-16 ) ) ;
#93676 = CARTESIAN_POINT ( 'NONE',  ( -4.390861645979385663, 6.216034235099629157, -1.599625672291271394 ) ) ;
#93677 = CARTESIAN_POINT ( 'NONE',  ( -10.49364770729726359, 11.34493653470939023, 0.7216878364870438212 ) ) ;
#93678 = CARTESIAN_POINT ( 'NONE',  ( 0.5277791401020451856, -0.3051165123582540994, 2.098401203810342786 ) ) ;
#93679 = DIRECTION ( 'NONE',  ( 0.000000000000000000, 8.546850786086437571E-32, 1.000000000000000000 ) ) ;
#93681 = CARTESIAN_POINT ( 'NONE',  ( 2.611707774152134842, 0.5260268489151798121, -1.889944157703125072 ) ) ;
#93680 = CARTESIAN_POINT ( 'NONE',  ( 1.360316468749964480, 2.796875000341370043, -3.989863994746656317E-14 ) ) ;
#93682 = CARTESIAN_POINT ( 'NONE',  ( 1.165152350680317195, -1.954565670758709128, -0.9236901323337529668 ) ) ;
#93684 = CARTESIAN_POINT ( 'NONE',  ( -5.656850995454980158, 6.308143005704411443, 1.156498089891801140 ) ) ;
#93683 = CARTESIAN_POINT ( 'NONE',  ( -4.423703259808839938, 8.383013913077441259, 0.7998128361456352531 ) ) ;
#93685 = CARTESIAN_POINT ( 'NONE',  ( -0.6823417656250212460, 2.051041667008083991, 1.181850606188767472 ) ) ;
#93686 = CARTESIAN_POINT ( 'NONE',  ( 2.600625072996507470, 0.8205526226049694172, -1.527383475524378031 ) ) ;
#93687 = CARTESIAN_POINT ( 'NONE',  ( 2.923474784230184920, 0.9664119506291848349, -1.447106689822146963 ) ) ;
#93688 = CARTESIAN_POINT ( 'NONE',  ( 7.293923454472091450, 7.611924906413328529, 0.7216878364870317197 ) ) ;
#93689 = CARTESIAN_POINT ( 'NONE',  ( -11.87992086682929660, 5.100687730227392969, -4.764507118098673111 ) ) ;
#93690 = CARTESIAN_POINT ( 'NONE',  ( 2.126327167286511166, 0.3474154575464418748, -1.985796285822030161 ) ) ;
#93691 = CARTESIAN_POINT ( 'NONE',  ( 6.825078400183572036, 7.629137130509069387, 2.744348168701661095 ) ) ;
#93692 = CARTESIAN_POINT ( 'NONE',  ( -3.298376509874564988, 7.070132704820777825, 0.000000000000000000 ) ) ;
#93693 = AXIS2_PLACEMENT_3D ( 'NONE', #108588, #121657, #71725 ) ;
#93694 = CARTESIAN_POINT ( 'NONE',  ( 1.410939872204178602, 1.737622768476089430, 0.9313336078424112596 ) ) ;
#93697 = EDGE_CURVE ( 'NONE', #50054, #7711, #107210, .T. ) ;
#93696 = CARTESIAN_POINT ( 'NONE',  ( -6.319508997745553636, 6.545384383557486530, 0.7216878364870257245 ) ) ;
#93695 = CARTESIAN_POINT ( 'NONE',  ( 5.273660385517703553, 0.3669835118517566497, -1.876681294024808988 ) ) ;
#93698 = CARTESIAN_POINT ( 'NONE',  ( -5.763624699140882157, 7.817591130454727200, -1.443375672974066548 ) ) ;
#93699 = CARTESIAN_POINT ( 'NONE',  ( 4.688087255275310561, 8.691461907788344377, -0.7998128361456381397 ) ) ;
#93700 = CARTESIAN_POINT ( 'NONE',  ( -6.794571259104023930, 7.956029886156682274, 1.199719254218452047 ) ) ;
#93701 = CARTESIAN_POINT ( 'NONE',  ( 1.049479869930733944, -1.824965358647975489, 0.8655331567536515003 ) ) ;
#93702 = CARTESIAN_POINT ( 'NONE',  ( -0.3878679656440754964, 3.999999999999934275, 1.007084189318353973 ) ) ;
#93703 = ADVANCED_FACE ( 'NONE', ( #208043 ), #179530, .T. ) ;
#93704 = CARTESIAN_POINT ( 'NONE',  ( 5.719831105939597649, -2.253009325453013023, 0.4983019283236743702 ) ) ;
#93705 = CARTESIAN_POINT ( 'NONE',  ( 6.127397123722368555, 0.1457569626216181913, -1.956525209266091192 ) ) ;
#93706 = CARTESIAN_POINT ( 'NONE',  ( 3.274216958324972726, -0.9628348462043828659, -1.709115330885315087 ) ) ;
#93707 = CARTESIAN_POINT ( 'NONE',  ( 7.397945374551106568, 11.78268670361832093, -0.7998128361456291469 ) ) ;
#93708 = CARTESIAN_POINT ( 'NONE',  ( 0.3170300144729014669, 1.034162889623980286, -1.730867746391979933 ) ) ;
#93709 = VERTEX_POINT ( 'NONE', #196083 ) ;
#93710 = CARTESIAN_POINT ( 'NONE',  ( 1.481820193039787403, -0.7077492718140475647, 1.995708955693164199 ) ) ;
#93712 = CARTESIAN_POINT ( 'NONE',  ( -7.157815033010924921, 10.43820240756634199, 1.199719254218453823 ) ) ;
#93711 = CARTESIAN_POINT ( 'NONE',  ( -4.111146893441842920, 5.819424013814012753, 1.599625672291267398 ) ) ;
#93713 = CARTESIAN_POINT ( 'NONE',  ( 2.378628397106247849, 1.683441843134887428, -0.7459445200509451368 ) ) ;
#93714 = VERTEX_POINT ( 'NONE', #32501 ) ;
#93715 = CARTESIAN_POINT ( 'NONE',  ( 12.00021129026602651, 7.586573191464381694, -0.2104672827513448807 ) ) ;
#93716 = CARTESIAN_POINT ( 'NONE',  ( 2.812858766682566181, -0.6196351552101020399, -2.028021595557969015 ) ) ;
#93717 = CARTESIAN_POINT ( 'NONE',  ( -1.499999999999997780, 4.931250000682820378, 1.214306433183764966E-14 ) ) ;
#93718 = CARTESIAN_POINT ( 'NONE',  ( 7.507464373665139412, 9.781794407407920389, 1.599625672291281386 ) ) ;
#93720 = CARTESIAN_POINT ( 'NONE',  ( 6.607619761813720238, 8.802252036906432764, 1.599625672291268286 ) ) ;
#93719 = B_SPLINE_CURVE_WITH_KNOTS ( 'NONE', 3,
 ( #78051, #127977, #29310, #209096, #59669, #60731 ),
 .UNSPECIFIED., .F., .F.,
 ( 4, 2, 4 ),
 ( 0.000000000000000000, 0.0003141588434155108628, 0.0006283176868310217256 ),
 .UNSPECIFIED. ) ;
#93721 = CARTESIAN_POINT ( 'NONE',  ( 2.759116376063870391, -1.791426917979478395, -1.018529149919424892 ) ) ;
#93723 = CARTESIAN_POINT ( 'NONE',  ( 0.08126746489400815676, -0.8690269180096841239, 1.623235155968821841 ) ) ;
#93722 = CARTESIAN_POINT ( 'NONE',  ( -6.516665389662827934, 10.75452672124865217, 0.000000000000000000 ) ) ;
#93724 = CARTESIAN_POINT ( 'NONE',  ( 1.364683531249988535, 4.113541667008088432, 0.7879004041258500513 ) ) ;
#93725 = FACE_OUTER_BOUND ( 'NONE', #86124, .T. ) ;
#93726 = CARTESIAN_POINT ( 'NONE',  ( 1.297698954646254954, 4.098833406624212472, 0.4386024987755403060 ) ) ;
#93727 = CARTESIAN_POINT ( 'NONE',  ( 0.4345545588612038657, 1.130843733186673639, -1.894998796914903139 ) ) ;
#93728 = CARTESIAN_POINT ( 'NONE',  ( 2.829655204463392693, -2.111994357890615071, 0.8116228763568857918 ) ) ;
#93729 = CARTESIAN_POINT ( 'NONE',  ( -7.944714827928056167, 10.29191993738131927, 1.443375672974090751 ) ) ;
#93730 = CARTESIAN_POINT ( 'NONE',  ( 1.951130291612662715, -1.617002164660426677, 0.8169817665307582688 ) ) ;
#93731 = CARTESIAN_POINT ( 'NONE',  ( 3.538217205509861962, 0.6946294275822698649, 1.785521036047182486 ) ) ;
#93732 = CARTESIAN_POINT ( 'NONE',  ( 4.633297751427938316, 0.003287558298453730800, -2.070544812459538253 ) ) ;
#93733 = CARTESIAN_POINT ( 'NONE',  ( -1.201851678989727383E-14, 2.759375000341417916, -1.575800808251660134 ) ) ;
#93734 =( GEOMETRIC_REPRESENTATION_CONTEXT ( 3 ) GLOBAL_UNCERTAINTY_ASSIGNED_CONTEXT ( ( #185024 ) ) GLOBAL_UNIT_ASSIGNED_CONTEXT ( ( #81896, #116584, #198819 ) ) REPRESENTATION_CONTEXT ( 'NONE', 'WORKASPACE' ) );
#93735 = CARTESIAN_POINT ( 'NONE',  ( 3.203940287746226634, -1.969268756981055635, 0.09538867180547243307 ) ) ;
#93736 = CARTESIAN_POINT ( 'NONE',  ( 6.533821582689818719, -1.260454884444404122, -1.457021811732343686 ) ) ;
#93737 = CARTESIAN_POINT ( 'NONE',  ( 2.447944060942487621, 1.870205405844455049, 0.04815357881200743595 ) ) ;
#93739 = CARTESIAN_POINT ( 'NONE',  ( 4.937886321289528979, 7.980522944944189234, -1.013380012275147291 ) ) ;
#93738 = CARTESIAN_POINT ( 'NONE',  ( 2.825201024400230132, 2.173230126089547909, 0.7765846127750095640 ) ) ;
#93740 = CARTESIAN_POINT ( 'NONE',  ( 2.787383077106736273, -1.737616373609903286, 0.6669969758191662823 ) ) ;
#93741 = CARTESIAN_POINT ( 'NONE',  ( -1.201851678989727383E-14, 3.071875000341420137, 1.575800808251672791 ) ) ;
#93742 = CARTESIAN_POINT ( 'NONE',  ( 6.672339319202143848, -0.9689918024566068766, -1.820889590527257740 ) ) ;
#93743 = CARTESIAN_POINT ( 'NONE',  ( -3.978428010606240850, 6.728917548094202949, -1.199719254218452047 ) ) ;
#93744 = CARTESIAN_POINT ( 'NONE',  ( 5.587931867126699537, 9.671004278289832001, -0.7998128361456291469 ) ) ;
#93745 = CARTESIAN_POINT ( 'NONE',  ( -1.286956418854627637, 4.047654341997620975, 0.4592741676705713871 ) ) ;
#93746 = CARTESIAN_POINT ( 'NONE',  ( 0.1707221987203759173, -1.373943582462642921, 1.596272430080846405 ) ) ;
#93747 = CARTESIAN_POINT ( 'NONE',  ( 1.364683531249988535, 4.426041667008082214, 0.7879004041258500513 ) ) ;
#93748 = CARTESIAN_POINT ( 'NONE',  ( 5.958325562381369345, 0.8699925256120243366, 1.978967057501494820 ) ) ;
#93749 = CARTESIAN_POINT ( 'NONE',  ( 6.445964431295706731, -1.320945465521980555, -1.527872228271543342 ) ) ;
#93750 = CARTESIAN_POINT ( 'NONE',  ( 1.364683531249986537, -1.136458332991912235, 0.7879004041258500513 ) ) ;
#93751 = CARTESIAN_POINT ( 'NONE',  ( -5.612712406377534435, 5.650512016969639895, 0.7216878364870317197 ) ) ;
#93754 = CARTESIAN_POINT ( 'NONE',  ( 4.039966587192259873, 5.736380323189513852, 1.443375672974062551 ) ) ;
#93753 = CARTESIAN_POINT ( 'NONE',  ( 6.825078400183581806, 2.095667212029386661, 2.065897939415714646 ) ) ;
#93752 = CARTESIAN_POINT ( 'NONE',  ( 5.905458427204159477, 9.047396044116986502, 1.199719254218452047 ) ) ;
#93755 = CARTESIAN_POINT ( 'NONE',  ( 4.944546133779973651, -1.457238331152037825, 1.394083050251286870 ) ) ;
#93756 = CARTESIAN_POINT ( 'NONE',  ( -6.906989191158078079, 10.14557225873805812, -1.199719254218440723 ) ) ;
#93758 = CARTESIAN_POINT ( 'NONE',  ( -5.763624699140868834, 9.738329559057408602, -0.7216878364870338292 ) ) ;
#93757 = CARTESIAN_POINT ( 'NONE',  ( -9.815740026613960723, 11.51441345488021106, -1.082531754730539753 ) ) ;
#93759 = CARTESIAN_POINT ( 'NONE',  ( 0.000000000000000000, -0.02876672507444791305, 0.000000000000000000 ) ) ;
#93761 = CARTESIAN_POINT ( 'NONE',  ( 1.364683531250000748, 11.25520833367473372, -0.7879004041258355073 ) ) ;
#93760 = CARTESIAN_POINT ( 'NONE',  ( 6.561405286136595905, 0.3748316153167965403, -2.128808860954830795 ) ) ;
#93762 = CARTESIAN_POINT ( 'NONE',  ( 10.30923643716940141, 0.9706168436483928463, -5.952040432139411585 ) ) ;
#93763 = CARTESIAN_POINT ( 'NONE',  ( 0.000000000000000000, -3.600000000000005862, 0.000000000000000000 ) ) ;
#93765 = CARTESIAN_POINT ( 'NONE',  ( -0.03574161356561295771, -1.858227405880557015, -0.4649775414454700995 ) ) ;
#93764 = CARTESIAN_POINT ( 'NONE',  ( -5.192409643909507544, 9.001635651295671892, 0.7216878364870458196 ) ) ;
#93766 = CARTESIAN_POINT ( 'NONE',  ( -1.364683531250000748, 0.8218750003414210248, 0.000000000000000000 ) ) ;
#93767 = CARTESIAN_POINT ( 'NONE',  ( 0.3540227772641007520, -5.166863022244653436, 10.99462479582587271 ) ) ;
#93768 = FACE_OUTER_BOUND ( 'NONE', #188488, .T. ) ;
#93769 = CARTESIAN_POINT ( 'NONE',  ( 1.207153632009206223, -0.4226329412084055548, 1.672169654609439116 ) ) ;
#93770 = CARTESIAN_POINT ( 'NONE',  ( 6.535912570239620578, 9.782925877658371405, 1.199719254218452047 ) ) ;
#93771 = CARTESIAN_POINT ( 'NONE',  ( 6.852720297064418986, 6.959538199522133262, 0.7998128361456331437 ) ) ;
#93772 = CARTESIAN_POINT ( 'NONE',  ( -1.402160292154681736E-14, -0.9906249996585834161, -1.575800808251665908 ) ) ;
#93773 = CARTESIAN_POINT ( 'NONE',  ( 1.211743588231738888, -0.7890745783359112142, -1.584151303567796543 ) ) ;
#93774 = CARTESIAN_POINT ( 'NONE',  ( 9.083599731475988648, 10.66024977721925104, 1.082531754730549967 ) ) ;
#93775 = CARTESIAN_POINT ( 'NONE',  ( 1.981109662258444537, -1.841391200710382980, -0.8139001868950055396 ) ) ;
#93776 = DIRECTION ( 'NONE',  ( 0.000000000000000000, -1.000000000000000000, 0.000000000000000000 ) ) ;
#93777 = ADVANCED_FACE ( 'NONE', ( #15166 ), #84859, .T. ) ;
#93778 = CARTESIAN_POINT ( 'NONE',  ( 4.542132036680512464, 0.9468659437555368985, -1.993456357439137960 ) ) ;
#93779 = CIRCLE ( 'NONE', #187127, 0.07999999999999994615 ) ;
#93780 = CARTESIAN_POINT ( 'NONE',  ( 5.190355475387732120, 1.122157983508360157, -1.858477351540340328 ) ) ;
#93781 = VERTEX_POINT ( 'NONE', #162520 ) ;
#93782 = CARTESIAN_POINT ( 'NONE',  ( -1.500000000000015099, -0.5791666666666476226, 0.8660254037844403729 ) ) ;
#93784 = CARTESIAN_POINT ( 'NONE',  ( 7.415946836550712185, 10.63539316174243865, 1.082531754730558626 ) ) ;
#93783 = CIRCLE ( 'NONE', #145600, 11.09999999999999964 ) ;
#93786 = CARTESIAN_POINT ( 'NONE',  ( 2.442982655898734645, -1.755780842375562312, -0.9913809985205720432 ) ) ;
#93785 = CARTESIAN_POINT ( 'NONE',  ( 3.176547234745368264, 0.9552152173708803318, 1.893241096743401464 ) ) ;
#93788 = ORIENTED_EDGE ( 'NONE', *, *, #85411, .T. ) ;
#93787 = CARTESIAN_POINT ( 'NONE',  ( 3.445387325821075652, -1.671857736322950094, 0.6981543005735133534 ) ) ;
#93789 = CARTESIAN_POINT ( 'NONE',  ( 5.013482942003290255, 9.071090208970993274, -0.7998128361456481317 ) ) ;
#93790 = ORIENTED_EDGE ( 'NONE', *, *, #135040, .F. ) ;
#93791 = CARTESIAN_POINT ( 'NONE',  ( 0.7076149179639171782, -1.862046558926268913, 0.1791945732521060819 ) ) ;
#93792 = CARTESIAN_POINT ( 'NONE',  ( 5.555090253297246150, 7.504024600312024340, 1.599625672291267398 ) ) ;
#93793 = CARTESIAN_POINT ( 'NONE',  ( 6.111906964637446649, -1.811269838261083232, 0.2284818145076653595 ) ) ;
#93795 = CARTESIAN_POINT ( 'NONE',  ( 1.182675045768744271, 1.564012596108365072, -1.105954659444969401 ) ) ;
#93794 = CARTESIAN_POINT ( 'NONE',  ( -4.386226389220933441, 5.076017861301227008, -1.199719254218446718 ) ) ;
#93796 = LINE ( 'NONE', #65500, #27976 ) ;
#93797 = CARTESIAN_POINT ( 'NONE',  ( 0.6823417656249899377, 1.405208333674752508, 1.181850606188755259 ) ) ;
#93798 = DIRECTION ( 'NONE',  ( -3.330669073875479482E-16, 3.330669073875479482E-16, 1.000000000000000000 ) ) ;
#93799 = CARTESIAN_POINT ( 'NONE',  ( -9.006694118179950692, 9.402231314165087284, 1.040834085586084257E-14 ) ) ;
#93800 = CARTESIAN_POINT ( 'NONE',  ( 5.207972885698374022, -2.151664816535401314, 0.2080130470862306957 ) ) ;
#93801 = CARTESIAN_POINT ( 'NONE',  ( -5.153507786970276783, 6.145418851954329575, -1.082531754730549967 ) ) ;
#93802 = CARTESIAN_POINT ( 'NONE',  ( -6.237633190739009237, 9.434933268240943249, 1.199719254218452047 ) ) ;
#93803 = CARTESIAN_POINT ( 'NONE',  ( 2.812858766682566181, -0.6196351552101020399, -2.028021595557969015 ) ) ;
#93805 = CARTESIAN_POINT ( 'NONE',  ( -10.02511099414689077, 5.770000865873268658, 5.887978427067937837 ) ) ;
#93804 = PLANE ( 'NONE',  #93283 ) ;
#93806 = CARTESIAN_POINT ( 'NONE',  ( 4.112542095708375811, 1.396345452295008727, -1.391819494878621111 ) ) ;
#93807 = CARTESIAN_POINT ( 'NONE',  ( 6.469012471580376733, -1.473683540339595810, 1.218514635347216046 ) ) ;
#93808 = CARTESIAN_POINT ( 'NONE',  ( 5.190659055775300956, 1.601436234092843414, -1.385157061098884146 ) ) ;
#93809 = FILL_AREA_STYLE_COLOUR ( '', #121852 ) ;
#93810 = CARTESIAN_POINT ( 'NONE',  ( 0.4673438449808891004, 1.800595422158430825, 1.021790579661909781 ) ) ;
#93811 = CARTESIAN_POINT ( 'NONE',  ( 3.222533412629301708, 0.04844597582449915174, 1.941506634493498362 ) ) ;
#93812 = ORIENTED_EDGE ( 'NONE', *, *, #153420, .T. ) ;
#93813 = FACE_OUTER_BOUND ( 'NONE', #174428, .T. ) ;
#93814 = CARTESIAN_POINT ( 'NONE',  ( 7.038618024149998043, 8.240751112043669835, -1.199719254218452047 ) ) ;
#93816 = CARTESIAN_POINT ( 'NONE',  ( 6.681470773436232413, 6.689470745297396270, -0.7998128361456281477 ) ) ;
#93815 = CARTESIAN_POINT ( 'NONE',  ( 3.398458197991469643, 1.647775209707361466, -1.286576258924768235 ) ) ;
#93817 = CARTESIAN_POINT ( 'NONE',  ( 5.533136087708556694, 5.627949321847663278, 0.000000000000000000 ) ) ;
#93819 = VERTEX_POINT ( 'NONE', #111694 ) ;
#93818 = CARTESIAN_POINT ( 'NONE',  ( 0.6272531361488179469, -0.2670696439982013781, 1.791522762418327419 ) ) ;
#93820 = CARTESIAN_POINT ( 'NONE',  ( 5.215527394842717435, -0.3265260713646127022, 2.182469266582609091 ) ) ;
#93821 = CARTESIAN_POINT ( 'NONE',  ( -0.2970643657731193432, -6.863149499369280093, -10.99622371251743225 ) ) ;
#93822 = ADVANCED_FACE ( 'NONE', ( #28242 ), #176631, .T. ) ;
#93823 = CARTESIAN_POINT ( 'NONE',  ( 3.153566124713353513, -1.803153744294363703, -1.271922660818012973 ) ) ;
#93824 = CARTESIAN_POINT ( 'NONE',  ( 7.853197290813620945, 10.18514947741448573, 1.599625672291281386 ) ) ;
#93825 = DIRECTION ( 'NONE',  ( 0.000000000000000000, 0.000000000000000000, 1.000000000000000000 ) ) ;
#93826 = CARTESIAN_POINT ( 'NONE',  ( 1.312987857083922627, 1.562780923097413677, -1.101767902142808175 ) ) ;
#93827 = CARTESIAN_POINT ( 'NONE',  ( 8.235688245297327015, 11.69572115523387268, -1.199719254218446718 ) ) ;
#93828 = CARTESIAN_POINT ( 'NONE',  ( 5.705552448923417508, -1.629793913574303588, -1.276656259598766940 ) ) ;
#93830 = CARTESIAN_POINT ( 'NONE',  ( 2.835029207381420502, 0.2633842809251253358, 2.145520918749081574 ) ) ;
#93829 = DIRECTION ( 'NONE',  ( -0.000000000000000000, -1.000000000000000000, -0.000000000000000000 ) ) ;
#93831 = CARTESIAN_POINT ( 'NONE',  ( 4.511385190476093321, -2.149204750630455241, 0.4279282578087198474 ) ) ;
#93832 = EDGE_LOOP ( 'NONE', ( #66548, #113557, #37998, #109824, #19441 ) ) ;
#93833 = DIRECTION ( 'NONE',  ( -0.9999980456341537316, 0.000000000000000000, -0.001977050295958610645 ) ) ;
#93834 = EDGE_CURVE ( 'NONE', #66250, #94599, #78754, .T. ) ;
#93835 = CARTESIAN_POINT ( 'NONE',  ( 4.016103985132956744, 7.694334506561854248, -0.3640553937371555082 ) ) ;
#93836 = CARTESIAN_POINT ( 'NONE',  ( -8.121044095224613457, 15.44793984265997189, 8.785326000989064354 ) ) ;
#93837 = CARTESIAN_POINT ( 'NONE',  ( 5.422335090822693715, 5.290755458906732933, 0.000000000000000000 ) ) ;
#93838 = CARTESIAN_POINT ( 'NONE',  ( 0.000000000000000000, -2.734374999522040550, -3.793834371823813445 ) ) ;
#93839 = CARTESIAN_POINT ( 'NONE',  ( -4.516801452008150086, 5.298631777878131111, 1.199719254218452935 ) ) ;
#93840 = CARTESIAN_POINT ( 'NONE',  ( 0.08851783505585240908, -0.5350849913869708541, 1.944072358963434555 ) ) ;
#93841 = AXIS2_PLACEMENT_3D ( 'NONE', #128165, #12174, #97723 ) ;
#93842 = CARTESIAN_POINT ( 'NONE',  ( -7.700668062882065179, 10.96756792579566664, -1.082531754730543971 ) ) ;
#93843 = CARTESIAN_POINT ( 'NONE',  ( 6.249382461256315580, 6.255644057745969988, -0.7998128361456481317 ) ) ;
#93844 = CARTESIAN_POINT ( 'NONE',  ( 5.541872263726007830, 1.386227983376321582, 1.537841262885197846 ) ) ;
#93845 = CARTESIAN_POINT ( 'NONE',  ( 4.916589582839517192, 1.327171671461774061, -1.396654247447129960 ) ) ;
#93846 = CARTESIAN_POINT ( 'NONE',  ( 6.292584676692968948, 1.568786179414104032, -1.421969346915842092 ) ) ;
#93847 = CARTESIAN_POINT ( 'NONE',  ( 5.443762371086860341, 6.309809840144842141, 1.199719254218462483 ) ) ;
#93848 = CARTESIAN_POINT ( 'NONE',  ( 0.000000000000000000, 0.08000000000000020983, 2.080000000000000071 ) ) ;
#93849 = CARTESIAN_POINT ( 'NONE',  ( 5.119951519371389814, 1.948576354197928628, -0.2848888285253112218 ) ) ;
#93850 = CARTESIAN_POINT ( 'NONE',  ( 0.3928598746986839974, 1.819701785225702473, -1.220828600141062203 ) ) ;
#93851 = CARTESIAN_POINT ( 'NONE',  ( 3.791466046568803705, 1.323482414808102137, 1.257835202898072380 ) ) ;
#93852 = PRODUCT ( 'isolation 510', 'isolation 510', '', ( #69877 ) ) ;
#93853 = CARTESIAN_POINT ( 'NONE',  ( 5.668717624289557833, 8.667235424096215723, -1.082531754730548412 ) ) ;
#93854 = CARTESIAN_POINT ( 'NONE',  ( 3.999292125906905859, 5.688926785023260102, 1.443375672974062551 ) ) ;
#93855 = CARTESIAN_POINT ( 'NONE',  ( -5.986807348886189040, 9.142303119412650503, -1.199719254218452047 ) ) ;
#93856 = CARTESIAN_POINT ( 'NONE',  ( 3.542423274920540432, 7.354853930707762721, -1.734723475976807094E-15 ) ) ;
#93857 = ORIENTED_EDGE ( 'NONE', *, *, #162091, .F. ) ;
#93859 = CARTESIAN_POINT ( 'NONE',  ( 4.763936024516410406, 0.6273381447981136727, -1.913061789696899995 ) ) ;
#93858 = CARTESIAN_POINT ( 'NONE',  ( 1.329379181053941483, 0.9071106928158387817, -1.602193565413398968 ) ) ;
#93860 = CARTESIAN_POINT ( 'NONE',  ( 1.370962024642598864, -0.5571102548348834116, 2.229726662508556778 ) ) ;
#93861 = CARTESIAN_POINT ( 'NONE',  ( 5.524254240939322713, 0.9636562883742012531, 1.708648623189083393 ) ) ;
#93862 = CARTESIAN_POINT ( 'NONE',  ( -6.227272627378437342, 6.159572908229946187, -0.7998128361456291469 ) ) ;
#93863 = CARTESIAN_POINT ( 'NONE',  ( 0.2333690889706926119, 0.7157316027301027228, -2.136973218959358434 ) ) ;
#93864 = CARTESIAN_POINT ( 'NONE',  ( -4.460796234096120472, 5.163016013655583158, 1.199719254218462483 ) ) ;
#93865 = CARTESIAN_POINT ( 'NONE',  ( 0.6431357727456864515, -0.2518013131528433757, -2.054909676291870380 ) ) ;
#93866 = CARTESIAN_POINT ( 'NONE',  ( -5.971440312176176768, 5.931378217152456500, 0.000000000000000000 ) ) ;
#93868 = CARTESIAN_POINT ( 'NONE',  ( 0.07479286986305370977, 0.004866263145587856019, -1.855573292446038414 ) ) ;
#93867 = CARTESIAN_POINT ( 'NONE',  ( 1.997712292880989837, -2.090220067774691159, 0.05436529341687650757 ) ) ;
#93869 = CARTESIAN_POINT ( 'NONE',  ( 0.4999999999999779066, 3.949999999999988187, 0.3999999999999576672 ) ) ;
#93870 = EDGE_LOOP ( 'NONE', ( #99346, #83108, #181664, #10909 ) ) ;
#93871 = CARTESIAN_POINT ( 'NONE',  ( -0.2104748580754183807, 4.084054299358617079, -2.658391380015924010 ) ) ;
#93872 = CARTESIAN_POINT ( 'NONE',  ( 1.698380523978352485, 1.446983168995601199, 0.9667953101664509274 ) ) ;
#93873 = AXIS2_PLACEMENT_3D ( 'NONE', #33031, #199773, #182460 ) ;
#93874 = CARTESIAN_POINT ( 'NONE',  ( 6.148786358997489820, 7.132337826040578754, -1.199719254218446718 ) ) ;
#93876 = CARTESIAN_POINT ( 'NONE',  ( 1.576106191276486213, 8.678179183658462748, 2.499999999999318767 ) ) ;
#93875 = FACE_OUTER_BOUND ( 'NONE', #149605, .T. ) ;
#93877 = CARTESIAN_POINT ( 'NONE',  ( 3.105755298912396878, -1.722902020775359144, 0.08520973767557615819 ) ) ;
#93878 = CARTESIAN_POINT ( 'NONE',  ( 1.154151856878969928, 0.8927059368322427524, 2.001694687108931170 ) ) ;
#93879 = CARTESIAN_POINT ( 'NONE',  ( 0.07043219980315276740, -0.8200377064033654850, 1.527959277978730768 ) ) ;
#93880 = CARTESIAN_POINT ( 'NONE',  ( 4.512475528931441104, -0.9420208833846724916, -1.995868093903986118 ) ) ;
#93881 = CARTESIAN_POINT ( 'NONE',  ( -10.68988767858338917, 3.994679225574373493, -4.900161361628223133 ) ) ;
#93882 = CARTESIAN_POINT ( 'NONE',  ( 2.360437767749205218, -2.170642449777848260, 0.04973808404824981572 ) ) ;
#93883 = CARTESIAN_POINT ( 'NONE',  ( 1.506192966688112422, -0.6554880476431452774, -1.704135612709246184 ) ) ;
#93884 = CARTESIAN_POINT ( 'NONE',  ( 3.028621024253768113, 0.5188578782318100657, 2.052648472271414448 ) ) ;
#93885 = CARTESIAN_POINT ( 'NONE',  ( 6.639320575229251453, 0.008029245381881154262, 1.796863947021019481 ) ) ;
#93886 = ORIENTED_EDGE ( 'NONE', *, *, #54909, .F. ) ;
#93888 = CARTESIAN_POINT ( 'NONE',  ( -1.364683531250000748, 1.821875000341421913, 0.000000000000000000 ) ) ;
#93887 = CARTESIAN_POINT ( 'NONE',  ( 3.193229341380324549, 1.808410471145019960, 1.408695239656273301 ) ) ;
#93889 = CARTESIAN_POINT ( 'NONE',  ( 3.816783937446950770, 4.411668334231586996, 1.199719254218464037 ) ) ;
#93890 = CARTESIAN_POINT ( 'NONE',  ( 3.623053363349855172, 5.249981562040033189, 1.599625672291267398 ) ) ;
#93891 = VECTOR ( 'NONE', #22892, 1000.000000000000114 ) ;
#93892 = CARTESIAN_POINT ( 'NONE',  ( 6.076846083367460238, -1.572777764080468321, 1.568860064416939037 ) ) ;
#93893 = CARTESIAN_POINT ( 'NONE',  ( -6.616015773788831211, 7.781401826584148473, 1.082531754730549967 ) ) ;
#93894 = CARTESIAN_POINT ( 'NONE',  ( 3.551873057100274789, 7.087676300018221021, 0.7216878364870298324 ) ) ;
#93895 = CARTESIAN_POINT ( 'NONE',  ( -6.195713011320790109, 9.211787032307496403, -1.082531754730537976 ) ) ;
#93896 = CARTESIAN_POINT ( 'NONE',  ( 4.421367491832282504, 5.291255174293369556, 1.082531754730549078 ) ) ;
#93897 = EDGE_LOOP ( 'NONE', ( #59705, #121406, #205426, #130842 ) ) ;
#93898 = CARTESIAN_POINT ( 'NONE',  ( 3.867814693791224112, -0.2004342644464084944, -2.006446243107910199 ) ) ;
#93900 = CARTESIAN_POINT ( 'NONE',  ( 2.360284975695529752, -2.062195451902974597, 0.04632573159841534699 ) ) ;
#93899 = CARTESIAN_POINT ( 'NONE',  ( 5.099838337034727331, 9.101561826515851550, -0.7998128361456281477 ) ) ;
#93901 = DIRECTION ( 'NONE',  ( -0.6029061840396265914, 0.7978120914393163066, 0.000000000000000000 ) ) ;
#93902 = CARTESIAN_POINT ( 'NONE',  ( 4.597623488365603528, 5.496887170248887067, -1.082531754730548412 ) ) ;
#93903 = CARTESIAN_POINT ( 'NONE',  ( 1.642778471875000035, -2.326041666188709112, -2.845375778867859751 ) ) ;
#93904 = CARTESIAN_POINT ( 'NONE',  ( -1.364683531249997417, 4.509375000341424133, 1.214306433183764966E-14 ) ) ;
#93905 = CARTESIAN_POINT ( 'NONE',  ( 5.121103774788174690, -2.081602751171758747, 0.6852947426586111224 ) ) ;
#93906 = CARTESIAN_POINT ( 'NONE',  ( 2.619767714365705658, 0.2496074646863334634, 2.000857082853441327 ) ) ;
#93907 = CARTESIAN_POINT ( 'NONE',  ( 2.630204301513817455, 0.2276190002089127917, 1.827071974840013269 ) ) ;
#93908 = EDGE_CURVE ( 'NONE', #112981, #26907, #12187, .T. ) ;
#93909 = CARTESIAN_POINT ( 'NONE',  ( 6.307567778855705853, 8.381915046796901692, -1.599625672291262513 ) ) ;
#93910 = CARTESIAN_POINT ( 'NONE',  ( 0.07661050522433668353, 0.008287133257128471639, -1.710863442170395432 ) ) ;
#93911 = CARTESIAN_POINT ( 'NONE',  ( -8.376239975144482486, 8.666701480623698828, 1.040834085586084257E-14 ) ) ;
#93913 = CARTESIAN_POINT ( 'NONE',  ( -5.829079699232685208, 5.765290835385048496, 0.000000000000000000 ) ) ;
#93912 = CARTESIAN_POINT ( 'NONE',  ( 5.577129106639307388, -0.04938619725537891220, -2.262140991306497373 ) ) ;
#93914 = CARTESIAN_POINT ( 'NONE',  ( 2.051528240825768012, -1.692106715078506296, -1.253703384363166196 ) ) ;
#93915 = CARTESIAN_POINT ( 'NONE',  ( -5.586841817283045408, 8.675676665875643678, 1.199719254218454489 ) ) ;
#93916 = CARTESIAN_POINT ( 'NONE',  ( 9.250740883225924804, 9.686952540052077509, 1.040834085586084257E-14 ) ) ;
#93917 = CARTESIAN_POINT ( 'NONE',  ( 5.492461626867537916, 9.421972641405202964, -0.7216878364870458196 ) ) ;
#93918 = B_SPLINE_CURVE_WITH_KNOTS ( 'NONE', 3,
 ( #95434, #80211, #125857, #211267, #94361, #61836, #9876, #44539, #192882, #142055 ),
 .UNSPECIFIED., .F., .F.,
 ( 4, 2, 2, 2, 4 ),
 ( 0.001603296788734610108, 0.001976506518550216057, 0.002349716248365820923, 0.002722925978181425788, 0.003096135707997031087 ),
 .UNSPECIFIED. ) ;
#93919 = CARTESIAN_POINT ( 'NONE',  ( -7.609150525767646833, 9.900428251527500834, -1.599625672291263179 ) ) ;
#93920 = CARTESIAN_POINT ( 'NONE',  ( -0.07933194154488912297, -7.246166700194011767, 9.499668754385634628 ) ) ;
#93921 = CARTESIAN_POINT ( 'NONE',  ( 6.575341312503417690, 10.61505593132193326, -0.7216878364870267237 ) ) ;
#93922 = CARTESIAN_POINT ( 'NONE',  ( 3.998447120444656555, 7.829958269474884602, 0.005269623924535754567 ) ) ;
#93923 = CARTESIAN_POINT ( 'NONE',  ( -7.700668062882059850, 11.92793714009701311, -0.7216878364870267237 ) ) ;
#93924 = CARTESIAN_POINT ( 'NONE',  ( 3.006315081767933606, -0.8967225907310495403, 2.032537921011686954 ) ) ;
#93925 = CARTESIAN_POINT ( 'NONE',  ( 6.883263157960374912, 7.629137130509066722, 2.546189081643289942 ) ) ;
#93926 = CARTESIAN_POINT ( 'NONE',  ( -4.938913097128142304, 8.984092056616635347, -0.7998128361456362523 ) ) ;
#93927 = CARTESIAN_POINT ( 'NONE',  ( 4.286349120214771879, 8.152491073559232859, -0.7998128361456221525 ) ) ;
#93928 = CARTESIAN_POINT ( 'NONE',  ( 4.879329150013382410, -0.09822140645733207220, 1.959542894978071992 ) ) ;
#93929 = CARTESIAN_POINT ( 'NONE',  ( 8.055515824813896941, 12.54985222892493368, 0.7998128361456462443 ) ) ;
#93930 = CARTESIAN_POINT ( 'NONE',  ( -5.312135015290653683, 6.384990658495349081, 1.125702006352300000 ) ) ;
#93931 = CARTESIAN_POINT ( 'NONE',  ( 4.369805582306193870, 3.992528022312320957, 1.214306433183764966E-14 ) ) ;
#93932 = CARTESIAN_POINT ( 'NONE',  ( 0.6823417656249882723, 0.9260416670080831025, -1.181850606188749264 ) ) ;
#93933 = CARTESIAN_POINT ( 'NONE',  ( -5.695833931516914639, 6.778132687258748845, 1.082531754730549078 ) ) ;
#93935 = ORIENTED_EDGE ( 'NONE', *, *, #211621, .T. ) ;
#93934 = CARTESIAN_POINT ( 'NONE',  ( -7.104109303880803417, 8.350844278358124484, 1.082531754730549967 ) ) ;
#93936 = VECTOR ( 'NONE', #198731, 1000.000000000000000 ) ;
#93937 = CARTESIAN_POINT ( 'NONE',  ( 3.410498715577559015, -2.118327196165440185, -0.1003008382433126094 ) ) ;
#93938 = CARTESIAN_POINT ( 'NONE',  ( -4.339491684825780737, 7.220434844675483355, -1.199719254218455378 ) ) ;
#93939 = CARTESIAN_POINT ( 'NONE',  ( 3.924826023212550030, 2.051882857192890430, 0.6804245187241527715 ) ) ;
#93940 = CARTESIAN_POINT ( 'NONE',  ( 3.491602800004707241, -1.839307750763185645, -0.08696504193297231733 ) ) ;
#93941 = CIRCLE ( 'NONE', #28195, 11.67999951260719804 ) ;
#93942 = CARTESIAN_POINT ( 'NONE',  ( -4.471757287801709779, 7.078374187635557924, 1.125421738336473299 ) ) ;
#93943 = CARTESIAN_POINT ( 'NONE',  ( -1.402160292154681736E-14, -0.2406249996585799189, -1.575800808251665908 ) ) ;
#93944 = CARTESIAN_POINT ( 'NONE',  ( 5.402228116617870946, 1.314032936993884793, -1.141193381800218232 ) ) ;
#93945 = DIRECTION ( 'NONE',  ( 0.000000000000000000, 0.000000000000000000, -1.000000000000000000 ) ) ;
#93946 = CARTESIAN_POINT ( 'NONE',  ( 3.877268743828270470, 5.546566172598190292, 1.443375672974062551 ) ) ;
#93947 = CARTESIAN_POINT ( 'NONE',  ( 10.91746247397144209, 8.226910605520304287, 4.997041797683915654 ) ) ;
#93948 = CARTESIAN_POINT ( 'NONE',  ( 3.362350911093567873, 0.9703303321016673033, 1.931748911306984784 ) ) ;
#93949 = CARTESIAN_POINT ( 'NONE',  ( 5.431017465639029318, 0.9912489969874547224, 1.755499476546865445 ) ) ;
#93950 = CARTESIAN_POINT ( 'NONE',  ( -7.117667457050096402, 10.28740055232499984, 1.082531754730549967 ) ) ;
#93951 = CARTESIAN_POINT ( 'NONE',  ( 2.237400686453533183, -1.931180590798301955, 0.9714560045831142077 ) ) ;
#93952 = CARTESIAN_POINT ( 'NONE',  ( 3.602765292730988556, 1.556248219076960870, -1.210034843411099681 ) ) ;
#93953 = LINE ( 'NONE', #206595, #20032 ) ;
#93954 = CARTESIAN_POINT ( 'NONE',  ( 4.493657767381210810, -1.941711754461509232, -0.04422589797668275563 ) ) ;
#93957 = ORIENTED_EDGE ( 'NONE', *, *, #129593, .T. ) ;
#93956 = EDGE_CURVE ( 'NONE', #194558, #184212, #205341, .T. ) ;
#93955 = CARTESIAN_POINT ( 'NONE',  ( -8.961576348508652146, 10.51788916375733685, -1.082531754730543083 ) ) ;
#93958 = CARTESIAN_POINT ( 'NONE',  ( -6.306477729012051725, 7.386587434382707151, 1.199719254218452047 ) ) ;
#93959 = CARTESIAN_POINT ( 'NONE',  ( 11.87828357750012565, 9.796897472595873069, 1.708055325888905962 ) ) ;
#93961 = EDGE_LOOP ( 'NONE', ( #5369, #105032, #40808, #214213, #191258 ) ) ;
#93960 = CARTESIAN_POINT ( 'NONE',  ( -5.679940009482361774, 5.591294530676332641, 0.7998128361456281477 ) ) ;
#93962 = CARTESIAN_POINT ( 'NONE',  ( -9.463228032214294316, 10.14278024711257764, 1.040834085586084257E-14 ) ) ;
#93963 = CARTESIAN_POINT ( 'NONE',  ( 1.764966765715753949, -1.560254191817540992, 1.560848541443552895 ) ) ;
#93964 = CARTESIAN_POINT ( 'NONE',  ( 3.285556943749998737, -1.305208332855376296, -1.896917185911906500 ) ) ;
#93965 = CARTESIAN_POINT ( 'NONE',  ( 6.860214158839045950, -1.961385418603446062, 0.04497666117601883257 ) ) ;
#93966 = CARTESIAN_POINT ( 'NONE',  ( -0.6823417656249969321, 5.780208333674756283, -1.181850606188749264 ) ) ;
#93967 = CARTESIAN_POINT ( 'NONE',  ( 1.499999999999990896, 4.556250000682819490, 1.214306433183764966E-14 ) ) ;
#93968 = CARTESIAN_POINT ( 'NONE',  ( 4.930363510330384003, 6.858250545851714008, -1.424563464522425882 ) ) ;
#93970 = CARTESIAN_POINT ( 'NONE',  ( -1.403499169902660437, 7.376709478543006071, -4.304123474984413278 ) ) ;
#93969 = DIRECTION ( 'NONE',  ( 0.000000000000000000, 0.000000000000000000, 1.000000000000000000 ) ) ;
#93971 = CARTESIAN_POINT ( 'NONE',  ( 5.472543265827003012, -0.04911201564661467345, -1.840652735559132669 ) ) ;
#93972 = ORIENTED_EDGE ( 'NONE', *, *, #116150, .F. ) ;
#93973 = CARTESIAN_POINT ( 'NONE',  ( -4.156403723172807449E-14, -1.046874999658554906, 1.570758158831744078 ) ) ;
#93974 = EDGE_CURVE ( 'NONE', #204603, #7595, #205921, .T. ) ;
#93975 = CARTESIAN_POINT ( 'NONE',  ( -6.347188469492005325, 10.55680364771601809, -0.7998128361456291469 ) ) ;
#93976 = CARTESIAN_POINT ( 'NONE',  ( -0.1216878429548678975, 3.463015919485879834, -1.996294584693599994 ) ) ;
#93977 = CARTESIAN_POINT ( 'NONE',  ( 5.871359616481898414, -1.819694913365289768, -1.088597390283413402 ) ) ;
#93978 = CARTESIAN_POINT ( 'NONE',  ( 8.812339285468201666, 13.17645074827856710, 8.077252134077332002 ) ) ;
#93979 = CARTESIAN_POINT ( 'NONE',  ( 3.985207087413062066, 6.736826471035503694, -1.199719254218452047 ) ) ;
#93980 = CARTESIAN_POINT ( 'NONE',  ( 0.08096513915848214948, -0.1534363407719694927, -2.027498111301667905 ) ) ;
#93983 = CARTESIAN_POINT ( 'NONE',  ( 3.913478945735289205, -0.9499487412085620974, -1.577145280185827447 ) ) ;
#93982 = CARTESIAN_POINT ( 'NONE',  ( 2.136937089482681795, -0.08731620468203694918, -1.859122327218107218 ) ) ;
#93981 = FACE_OUTER_BOUND ( 'NONE', #31572, .T. ) ;
#93984 = CARTESIAN_POINT ( 'NONE',  ( 7.579171565239241737, 8.801120566655981747, 1.199719254218462483 ) ) ;
#93985 = CARTESIAN_POINT ( 'NONE',  ( -9.367496997602099640, 14.48154074412328995, -7.499999999994433786 ) ) ;
#93986 = CARTESIAN_POINT ( 'NONE',  ( -5.661411662158206681, 8.762674818229999829, -1.199719254218452047 ) ) ;
#93988 = ORIENTED_EDGE ( 'NONE', *, *, #144354, .F. ) ;
#93987 = CARTESIAN_POINT ( 'NONE',  ( -2.788906526875773208E-15, 10.43750000000000000, -1.499999999999998446 ) ) ;
#93989 = CARTESIAN_POINT ( 'NONE',  ( 4.705825944637973990, -0.5905853116198942487, 2.126329296355852883 ) ) ;
#93990 = CARTESIAN_POINT ( 'NONE',  ( 6.011039796215681186, 1.991063742206979459, 1.074381780396720165 ) ) ;
#93991 = CARTESIAN_POINT ( 'NONE',  ( -6.751597309925468693, 6.979211071108916364, 0.7216878364870317197 ) ) ;
#93992 = CARTESIAN_POINT ( 'NONE',  ( 6.275650443109183740, 0.3000964294621047967, -1.786390703358155196 ) ) ;
#93993 = CARTESIAN_POINT ( 'NONE',  ( 0.1457207355009884908, 1.993892511249679034, -0.3006540981884687214 ) ) ;
#93994 = CARTESIAN_POINT ( 'NONE',  ( -4.197870329852986693, 3.573279226090503080, -2.499999999999996003 ) ) ;
#93995 = CARTESIAN_POINT ( 'NONE',  ( 5.928550619183988957, 1.803260976426118489, 0.4972845834502263584 ) ) ;
#93996 = CARTESIAN_POINT ( 'NONE',  ( 5.145129553670328981, 0.1446803459003667969, 1.906877450533930096 ) ) ;
#93997 = CARTESIAN_POINT ( 'NONE',  ( 2.195822763121351960E-15, 15.42895922032036715, 11.92238959702059731 ) ) ;
#93999 = EDGE_CURVE ( 'NONE', #206986, #178508, #52656, .T. ) ;
#93998 = COLOUR_RGB ( '', 0.31764706, 0.68627451, 0.89019608) ;
#94000 = CARTESIAN_POINT ( 'NONE',  ( 0.9537216069140028729, 1.868711056098860235, -0.08788249432020722729 ) ) ;
#94001 = CARTESIAN_POINT ( 'NONE',  ( 0.7609543035823238544, -0.05432987398422234326, -2.015980609757315190 ) ) ;
#94003 = CARTESIAN_POINT ( 'NONE',  ( 3.862027066150780730, 2.090197335813360979, -0.2575193119012611498 ) ) ;
#94002 = CARTESIAN_POINT ( 'NONE',  ( -9.236128959407555072, 11.79856975744075598, -1.599625672291263179 ) ) ;
#94004 = CARTESIAN_POINT ( 'NONE',  ( 9.043452155515161905, 10.50944792197790889, 1.199719254218453823 ) ) ;
#94006 = CARTESIAN_POINT ( 'NONE',  ( -8.045874094706015001, 11.47427131287732927, -1.199719254218446718 ) ) ;
#94005 = CARTESIAN_POINT ( 'NONE',  ( -1.500000000000015099, -0.3708333333333105331, -0.8660254037844383745 ) ) ;
#94007 = CARTESIAN_POINT ( 'NONE',  ( 11.45842088241066392, 10.00693529122952086, 3.566211699757795284 ) ) ;
#94008 = CARTESIAN_POINT ( 'NONE',  ( 3.304948908139183406, -0.3981353638667082806, -1.979975013379015936 ) ) ;
#94009 = CARTESIAN_POINT ( 'NONE',  ( -0.6823417656250212460, 3.551041667008085323, 1.181850606188767472 ) ) ;
#94010 = CARTESIAN_POINT ( 'NONE',  ( 2.846322183865124700, 5.408127416896231665, -1.199719254218446718 ) ) ;
#94011 = CARTESIAN_POINT ( 'NONE',  ( 3.884175197147401892, -1.069116497136082700, 1.878640351225938421 ) ) ;
#94012 = LINE ( 'NONE', #77728, #26214 ) ;
#94013 = CARTESIAN_POINT ( 'NONE',  ( 0.7499999999999902300, 4.816666666666684193, -1.299038105676658228 ) ) ;
#94015 = CARTESIAN_POINT ( 'NONE',  ( -9.498884310698281652, -9.746166700192997467, 0.1658036423878506416 ) ) ;
#94014 = CARTESIAN_POINT ( 'NONE',  ( 6.373214726875630731, 9.593111727067046957, 1.199719254218452047 ) ) ;
#94016 = CARTESIAN_POINT ( 'NONE',  ( 8.880227426826646564, 9.462612874160329923, 0.7216878364870458196 ) ) ;
#94018 = CARTESIAN_POINT ( 'NONE',  ( 8.715232613915466331, 14.87911529561621649, -8.250190486245246646 ) ) ;
#94017 = CARTESIAN_POINT ( 'NONE',  ( 0.4675213905811578807, 1.889292113317426969, 1.069767032291484288 ) ) ;
#94019 = CARTESIAN_POINT ( 'NONE',  ( -5.694061328059534688, 8.626526735169329996, 1.082531754730548412 ) ) ;
#94020 = CARTESIAN_POINT ( 'NONE',  ( 1.364683531249988757, 1.634375000341421691, 0.000000000000000000 ) ) ;
#94021 = CARTESIAN_POINT ( 'NONE',  ( 1.699035084177059174, 1.824418957995146195, 1.213967346723361596 ) ) ;
#94022 = CARTESIAN_POINT ( 'NONE',  ( 9.579603127937247109, -9.900000000000005684, -0.08720040834114990702 ) ) ;
#94023 = CARTESIAN_POINT ( 'NONE',  ( 2.641812911801244113, -1.676132216910112493, -1.519885475924544593 ) ) ;
#94024 = CARTESIAN_POINT ( 'NONE',  ( -5.831978632172702071, 9.955725504176825780, 0.7998128361456481317 ) ) ;
#94025 = CARTESIAN_POINT ( 'NONE',  ( 1.364683531249988535, 4.176041667008081326, 0.7879004041258500513 ) ) ;
#94026 = CARTESIAN_POINT ( 'NONE',  ( 6.137634773950260580, 6.983624353001562923, 0.9378011681944794509 ) ) ;
#94027 = AXIS2_PLACEMENT_3D ( 'NONE', #115609, #14834, #16958 ) ;
#94028 = CARTESIAN_POINT ( 'NONE',  ( -1.500000000000001110, 13.02083333333333393, 0.8660254037844419273 ) ) ;
#94029 = CARTESIAN_POINT ( 'NONE',  ( 7.349928672384120176, 7.747540670635879145, 0.7216878364870267237 ) ) ;
#94030 = CARTESIAN_POINT ( 'NONE',  ( 3.971743243459349149, 0.9813984145389564873, 1.472460009610305320 ) ) ;
#94031 = ADVANCED_FACE ( 'NONE', ( #46638 ), #157543, .T. ) ;
#94032 = CARTESIAN_POINT ( 'NONE',  ( 7.910292558569346433, 11.31609285405122556, -1.199719254218446718 ) ) ;
#94033 = CARTESIAN_POINT ( 'NONE',  ( 1.026558790958994383, 1.254618057004111886, -1.691278660206218420 ) ) ;
#94035 = CARTESIAN_POINT ( 'NONE',  ( 0.7499999999999885647, 0.7333333333333567072, 1.299038105676657340 ) ) ;
#94034 = CARTESIAN_POINT ( 'NONE',  ( 1.364683531249996529, 8.963541667008067648, 0.7879004041258405033 ) ) ;
#94036 = CARTESIAN_POINT ( 'NONE',  ( -3.637330350216213759, 7.465578851886037093, -0.7998128361456481317 ) ) ;
#94037 = CARTESIAN_POINT ( 'NONE',  ( 6.556263154800560322, -1.238474754573844816, 1.591913907798309769 ) ) ;
#94038 = ORIENTED_EDGE ( 'NONE', *, *, #122759, .T. ) ;
#94039 = AXIS2_PLACEMENT_3D ( 'NONE', #124481, #7416, #57262 ) ;
#94040 = CARTESIAN_POINT ( 'NONE',  ( 9.856941372335116469, 11.45851867493453291, 1.199719254218450271 ) ) ;
#94041 = CARTESIAN_POINT ( 'NONE',  ( 4.065207594588423845, 0.2294239933214488880, -1.856472568989680161 ) ) ;
#94042 = CARTESIAN_POINT ( 'NONE',  ( 4.733297664174529906, 0.005294743050891088411, -2.070434559870132585 ) ) ;
#94043 = CARTESIAN_POINT ( 'NONE',  ( -5.261973015435229328, 9.153069261400824885, 0.000000000000000000 ) ) ;
#94044 = CARTESIAN_POINT ( 'NONE',  ( 7.079328764629950754, 11.41096732537697633, 0.7998128361456462443 ) ) ;
#94045 = CARTESIAN_POINT ( 'NONE',  ( -1.506030227042769010, 8.670273769332156988, 2.548074190919186410 ) ) ;
#94046 = CARTESIAN_POINT ( 'NONE',  ( 0.000000000000000000, 3.000000000000002665, 0.000000000000000000 ) ) ;
#94047 = CARTESIAN_POINT ( 'NONE',  ( 10.39230484541330313, 3.447199233515649386, 5.999999999999906741 ) ) ;
#94048 = CARTESIAN_POINT ( 'NONE',  ( -1.364683531250010295, 5.551041667008087543, -0.7879004041258300672 ) ) ;
#94049 = CARTESIAN_POINT ( 'NONE',  ( 3.578520225191741844, 1.246510459297203610, -1.514941731618473009 ) ) ;
#94050 = CARTESIAN_POINT ( 'NONE',  ( 0.9310172746952742884, 0.9912447863934905623, 1.755501862388042067 ) ) ;
#94051 = CARTESIAN_POINT ( 'NONE',  ( -3.149236820124241110, 6.896136400112061970, -0.7998128361456481317 ) ) ;
#94053 = SURFACE_STYLE_FILL_AREA ( #44228 ) ;
#94052 = CARTESIAN_POINT ( 'NONE',  ( 8.718056468787178659, 10.12981962079525289, 1.199719254218462483 ) ) ;
#94054 = CARTESIAN_POINT ( 'NONE',  ( 1.458040028222376439, 0.7530789129696242590, 1.712431740859089668 ) ) ;
#94055 = CARTESIAN_POINT ( 'NONE',  ( -1.364683531250012516, 4.238541667008090208, -0.7879004041258300672 ) ) ;
#94056 = CARTESIAN_POINT ( 'NONE',  ( 2.918229521859570408, -2.010703624536396728, 0.1031290223681199103 ) ) ;
#94058 = CARTESIAN_POINT ( 'NONE',  ( 2.197004041102487371, 1.892657838527435299, 0.9490559450526787622 ) ) ;
#94057 = CARTESIAN_POINT ( 'NONE',  ( -6.155038550924159857, 8.203964280876741455, 1.443375672974078761 ) ) ;
#94059 = MANIFOLD_SOLID_BREP ( 'Sweep1[5]', #184790 ) ;
#94060 = CARTESIAN_POINT ( 'NONE',  ( 8.776224899084628106, 13.27471476138783224, 8.184001253707569035 ) ) ;
#94061 = CARTESIAN_POINT ( 'NONE',  ( 3.842288295254093100, -1.023014542950370975, 1.799900136785845817 ) ) ;
#94062 = CARTESIAN_POINT ( 'NONE',  ( 5.833751235630055376, 10.02806988486892514, 0.7998128361456331437 ) ) ;
#94064 = CARTESIAN_POINT ( 'NONE',  ( 3.728655938958122196, 4.308852335994623139, -1.199719254218446718 ) ) ;
#94063 = CARTESIAN_POINT ( 'NONE',  ( 6.492138175525482779, -0.5563555211482211771, -2.015168333173870785 ) ) ;
#94066 = VERTEX_POINT ( 'NONE', #200309 ) ;
#94065 = CARTESIAN_POINT ( 'NONE',  ( 5.719710266082651096, -1.780569991979109590, 0.4021758204828808081 ) ) ;
#94067 = CARTESIAN_POINT ( 'NONE',  ( 8.646349277213076334, 11.11049346154719508, 1.599625672291281386 ) ) ;
#94068 = DIRECTION ( 'NONE',  ( -0.000000000000000000, -1.000000000000000000, -0.000000000000000000 ) ) ;
#94069 = CARTESIAN_POINT ( 'NONE',  ( 11.72719273365024506, 8.694648967210921953, 4.374500150831954315 ) ) ;
#94070 = CARTESIAN_POINT ( 'NONE',  ( 6.247136877606230598, -1.867572634706683443, 1.175315980461520304 ) ) ;
#94071 = CARTESIAN_POINT ( 'NONE',  ( -8.012344526598182026E-15, 11.85937500034140157, -1.575800808251669460 ) ) ;
#94072 = CARTESIAN_POINT ( 'NONE',  ( 4.670513044250029999, 0.7352163052343118066, 1.765496816765201427 ) ) ;
#94073 = CARTESIAN_POINT ( 'NONE',  ( -7.700141177557535244, 11.07091624287075859, -1.199719254218446718 ) ) ;
#94074 = CIRCLE ( 'NONE', #17952, 0.08000000000000041800 ) ;
#94075 = CARTESIAN_POINT ( 'NONE',  ( 6.982612806237943559, 8.105135347821125436, -1.199719254218446718 ) ) ;
#94076 = AXIS2_PLACEMENT_3D ( 'NONE', #5599, #117321, #38148 ) ;
#94077 = CARTESIAN_POINT ( 'NONE',  ( 1.360316468749975805, 2.317708333674724841, -0.7853790794158961308 ) ) ;
#94078 = CARTESIAN_POINT ( 'NONE',  ( 3.917943204224906939, 5.594019709727598766, -1.443375672974051449 ) ) ;
#94079 = CARTESIAN_POINT ( 'NONE',  ( -3.844188154716629668, 7.347496864717369291, 0.5888589343297395695 ) ) ;
#94080 = CARTESIAN_POINT ( 'NONE',  ( 3.161022370280501814, 6.839609865302569425, 0.000000000000000000 ) ) ;
#94081 = ORIENTED_EDGE ( 'NONE', *, *, #167459, .F. ) ;
#94082 = ADVANCED_FACE ( 'NONE', ( #165702 ), #210170, .T. ) ;
#94083 = DIRECTION ( 'NONE',  ( 0.000000000000000000, 0.000000000000000000, 1.000000000000000000 ) ) ;
#94084 = CARTESIAN_POINT ( 'NONE',  ( 0.07700591528352926374, 4.093948292925152721, -2.465843965391618209 ) ) ;
#94085 = CARTESIAN_POINT ( 'NONE',  ( 7.517069824134078537, 7.734612647770044092, 0.000000000000000000 ) ) ;
#94086 = CARTESIAN_POINT ( 'NONE',  ( -0.3867890553498209427, 3.235871879154603725, 11.62250415223148003 ) ) ;
#94087 = CARTESIAN_POINT ( 'NONE',  ( -6.344338864096334518, 6.859745832460597548, 0.6559349933493059392 ) ) ;
#94088 =( BOUNDED_SURFACE ( )  B_SPLINE_SURFACE ( 3, 3, ( 
 ( #153237, #4808, #66613, #182521, #67683, #185717, #137000, #151124, #85035, #100221 ),
 ( #132760, #38422, #104502, #203028, #54669, #133828, #52535, #168422, #21069, #186794 ),
 ( #2689, #120817, #116532, #200889, #86106, #548, #35204, #167363, #68762, #166289 ),
 ( #170546, #134882, #18951, #22130, #119738, #36273, #83963, #184652, #102350, #150052 ),
 ( #20018, #199840, #51482, #152178, #3747, #135930, #69822, #125100, #192126, #106680 ),
 ( #141310, #57873, #191058, #204082, #88243, #40574, #126162, #207322, #58943, #172703 ),
 ( #10185, #108831, #24281, #42723, #122976, #174857, #26435, #92546, #91467, #55735 ) ),
 .UNSPECIFIED., .T., .F., .T. ) 
 B_SPLINE_SURFACE_WITH_KNOTS ( ( 4, 3, 4 ),
 ( 4, 1, 1, 1, 1, 1, 1, 4 ),
 ( 0.000000000000000000, 0.5000000000000000000, 1.000000000000000000 ),
 ( 0.000000000000000000, 0.09183773654504942541, 0.1838067853904964410, 0.2558923657893393822, 0.3606054339151033017, 0.5206678126786191685, 0.7335446035554463728, 1.000000000000000000 ),
 .UNSPECIFIED. ) 
 GEOMETRIC_REPRESENTATION_ITEM ( )  RATIONAL_B_SPLINE_SURFACE ( (
 ( 1.000000000000000222, 1.000000000000000222, 0.9999999999999997780, 1.000000000000000000, 1.000000000000000222, 0.9999999999999996669, 1.000000000000000222, 1.000000000000000444, 1.000000000000000000, 1.000000000000000000),
 ( 0.3333333333333334259, 0.3333333333333334814, 0.3333333333333333703, 0.3333333333333333703, 0.3333333333333333703, 0.3333333333333332593, 0.3333333333333334814, 0.3333333333333334814, 0.3333333333333333703, 0.3333333333333333703),
 ( 0.3333333333333334259, 0.3333333333333334814, 0.3333333333333333703, 0.3333333333333333703, 0.3333333333333333703, 0.3333333333333332593, 0.3333333333333334814, 0.3333333333333334814, 0.3333333333333333703, 0.3333333333333333703),
 ( 1.000000000000000222, 1.000000000000000222, 0.9999999999999997780, 1.000000000000000000, 1.000000000000000222, 0.9999999999999996669, 1.000000000000000222, 1.000000000000000444, 1.000000000000000000, 1.000000000000000000),
 ( 0.3333333333333334259, 0.3333333333333334814, 0.3333333333333333703, 0.3333333333333333703, 0.3333333333333333703, 0.3333333333333332593, 0.3333333333333334814, 0.3333333333333334814, 0.3333333333333333703, 0.3333333333333333703),
 ( 0.3333333333333334259, 0.3333333333333334814, 0.3333333333333333703, 0.3333333333333333703, 0.3333333333333333703, 0.3333333333333332593, 0.3333333333333334814, 0.3333333333333334814, 0.3333333333333333703, 0.3333333333333333703),
 ( 1.000000000000000222, 1.000000000000000222, 0.9999999999999997780, 1.000000000000000000, 1.000000000000000222, 0.9999999999999996669, 1.000000000000000222, 1.000000000000000444, 1.000000000000000000, 1.000000000000000000) ) ) 
 REPRESENTATION_ITEM ( '' )  SURFACE ( )  );
#94089 = CARTESIAN_POINT ( 'NONE',  ( -5.992340707560165569, 8.014150130285418783, 1.443375672974064550 ) ) ;
#94090 = CARTESIAN_POINT ( 'NONE',  ( 4.142179624174931796, 4.791296635414242111, 1.199719254218464037 ) ) ;
#94091 = CARTESIAN_POINT ( 'NONE',  ( 2.905082208348725548, -1.640047651136176565, 1.090064613274278837 ) ) ;
#94092 = CARTESIAN_POINT ( 'NONE',  ( 3.603138812553498216, -0.1455146663824242736, 2.011206757212272933 ) ) ;
#94093 = CARTESIAN_POINT ( 'NONE',  ( -7.640183256500752584, 8.872300873127729304, -1.199719254218446718 ) ) ;
#94094 = CARTESIAN_POINT ( 'NONE',  ( 4.206772801990143584, 8.129928378955675328, 0.7998128361456271485 ) ) ;
#94095 = CARTESIAN_POINT ( 'NONE',  ( 6.827182134110200806, 4.685259207053684705, 2.851548537572299313 ) ) ;
#94096 = CARTESIAN_POINT ( 'NONE',  ( 3.099763004921416876, -2.188912590334081809, 0.1079765428157742069 ) ) ;
#94097 = LINE ( 'NONE', #31212, #171409 ) ;
#94098 = CARTESIAN_POINT ( 'NONE',  ( 1.694233118518298165, -1.916858602850049609, -0.1915058630488040703 ) ) ;
#94099 = CARTESIAN_POINT ( 'NONE',  ( -9.155833807930273238, 9.576227618873799585, -0.7998128361456291469 ) ) ;
#94100 = CARTESIAN_POINT ( 'NONE',  ( -0.1296875068448159474, 0.7431874094961619104, -1.910093690679348200 ) ) ;
#94101 = CARTESIAN_POINT ( 'NONE',  ( 0.2333540202161792088, 6.948072531064760859, -2.640811564931430766 ) ) ;
#94102 = CARTESIAN_POINT ( 'NONE',  ( 3.431622278034673901, 7.017660067766835930, -1.734723475976807094E-15 ) ) ;
#94103 = CARTESIAN_POINT ( 'NONE',  ( 8.769426429940780920, 9.125419011219408461, 0.7998128361456462443 ) ) ;
#94104 = EDGE_CURVE ( 'NONE', #113693, #190459, #105776, .T. ) ;
#94105 = CARTESIAN_POINT ( 'NONE',  ( -0.3282377607281460885, 1.198664549684620662, -1.225000000000036726 ) ) ;
#94106 = CARTESIAN_POINT ( 'NONE',  ( 4.231553341240963384, 7.950912974840849579, -0.7216878364870357165 ) ) ;
#94107 = ORIENTED_EDGE ( 'NONE', *, *, #198698, .T. ) ;
#94109 = CARTESIAN_POINT ( 'NONE',  ( 2.332683495817444719, 1.313167467523576715, -1.525923137932885476 ) ) ;
#94108 = CARTESIAN_POINT ( 'NONE',  ( 6.181194517112824194, 1.274813594131599226, 1.328792456347933637 ) ) ;
#94110 = CARTESIAN_POINT ( 'NONE',  ( 4.341395233127314235, -1.327617041990782010, 1.876015773706960932 ) ) ;
#94112 = CARTESIAN_POINT ( 'NONE',  ( 2.359995855038379720, -1.860683555027684788, 0.03984664071272727565 ) ) ;
#94111 = CARTESIAN_POINT ( 'NONE',  ( -0.02880301295725678015, 0.2243704974793322426, -2.307247863525173859 ) ) ;
#94113 = CARTESIAN_POINT ( 'NONE',  ( -1.642778471874998480, -1.451041666188708446, 2.845375778867863303 ) ) ;
#94114 = CARTESIAN_POINT ( 'NONE',  ( -0.1290005225502675879, -0.006633637972621592160, -2.173875058097324064 ) ) ;
#94115 = CARTESIAN_POINT ( 'NONE',  ( 5.730699431777452446, 1.279516236652695316, -1.421498520143074540 ) ) ;
#94116 = CARTESIAN_POINT ( 'NONE',  ( -8.019811557683421910, 9.315200557840817908, 1.199719254218462483 ) ) ;
#94117 = CARTESIAN_POINT ( 'NONE',  ( -4.312902262922974295, 8.045820050136510915, 0.7216878364870338292 ) ) ;
#94119 = CARTESIAN_POINT ( 'NONE',  ( 3.555401268124198655, 0.4554524271490404952, -1.814226883376020671 ) ) ;
#94118 = CARTESIAN_POINT ( 'NONE',  ( 5.126549769544753055, 0.1549841644245806838, 2.085076985156742779 ) ) ;
#94120 = CARTESIAN_POINT ( 'NONE',  ( 5.653386867218496370, 9.539442411822841805, 1.040834085586084257E-14 ) ) ;
#94121 = EDGE_LOOP ( 'NONE', ( #205909, #167533, #192075, #86257 ) ) ;
#94122 = STYLED_ITEM ( 'NONE', ( #107970 ), #27695 ) ;
#94123 = CARTESIAN_POINT ( 'NONE',  ( 2.975976995527448654, 6.510311277507367045, -0.5630407789675599961 ) ) ;
#94124 = CARTESIAN_POINT ( 'NONE',  ( 0.2972806740312853857, -7.751137252134813416, -10.97067717498809891 ) ) ;
#94125 = CARTESIAN_POINT ( 'NONE',  ( 6.551377187490000864, -1.390289022577213984, -1.020726160236499203 ) ) ;
#94126 = CARTESIAN_POINT ( 'NONE',  ( -5.551173829791513192, 8.563787670477010394, 1.199719254218452047 ) ) ;
#94127 = CARTESIAN_POINT ( 'NONE',  ( 1.652526702274889514, 0.8913305402388423948, 1.487382274443969754 ) ) ;
#94128 = PRESENTATION_STYLE_ASSIGNMENT (( #74654 ) ) ;
#94129 = CARTESIAN_POINT ( 'NONE',  ( -11.04536101718726293, 13.40000000000000036, 1.099999999999996758 ) ) ;
#94130 = CARTESIAN_POINT ( 'NONE',  ( 6.297752264732417338, -1.566808387090750765, -1.503110733841714675 ) ) ;
#94131 = CARTESIAN_POINT ( 'NONE',  ( 3.949673224339702138, 0.6133576713117370183, -1.719707012317383432 ) ) ;
#94132 = CARTESIAN_POINT ( 'NONE',  ( 2.448037131198562921, -0.8433605282326918084, 1.771390271482737200 ) ) ;
#94133 = CARTESIAN_POINT ( 'NONE',  ( 0.3865160979802947927, -0.7177084582802439883, -1.991989965223327275 ) ) ;
#94134 = CARTESIAN_POINT ( 'NONE',  ( 9.406473631745788211, 4.446947634372973468, 7.380697509896862130 ) ) ;
#94135 = CARTESIAN_POINT ( 'NONE',  ( -9.236128959407555072, 11.79856975744075598, -1.599625672291263179 ) ) ;
#94136 = CARTESIAN_POINT ( 'NONE',  ( 7.239163954692881653, 10.53310948286200599, -1.199719254218441611 ) ) ;
#94137 = CARTESIAN_POINT ( 'NONE',  ( 2.895306150831237879, -0.1582170333116576511, -2.114654843180157950 ) ) ;
#94138 = CARTESIAN_POINT ( 'NONE',  ( -3.551873057100300990, 5.166937871415542283, 1.443375672974064550 ) ) ;
#94139 = CARTESIAN_POINT ( 'NONE',  ( 0.4356160240586420263, -9.063431457505059186, -9.626717610576610795 ) ) ;
#94140 = VECTOR ( 'NONE', #134213, 1000.000000000000000 ) ;
#94141 = CARTESIAN_POINT ( 'NONE',  ( -5.584559075236136039, 6.202510182859402477, -0.8982034194818852013 ) ) ;
#94142 = CARTESIAN_POINT ( 'NONE',  ( 0.8134373588399683719, -1.746984811521329339, -1.110588058507409936 ) ) ;
#94143 = CARTESIAN_POINT ( 'NONE',  ( -1.500000000000001110, 14.55208333401612819, 0.8660254037844419273 ) ) ;
#94145 = EDGE_LOOP ( 'NONE', ( #67247, #146507, #83493, #41859 ) ) ;
#94144 = CARTESIAN_POINT ( 'NONE',  ( 3.000855645084123946, -2.188801376007823762, -0.3777086580352209122 ) ) ;
#94146 = CARTESIAN_POINT ( 'NONE',  ( 0.8624555810839064085, -0.06381188527813246025, -2.297968782114163222 ) ) ;
#94148 = CARTESIAN_POINT ( 'NONE',  ( 5.471554536677815328, -0.3081364425130261320, 2.039334399838355960 ) ) ;
#94147 = CARTESIAN_POINT ( 'NONE',  ( 8.595506201383999567, 12.97191496834930113, 0.7216878364870438212 ) ) ;
#94150 = CARTESIAN_POINT ( 'NONE',  ( 3.475000000000000533, -1.604166666666667629, 2.006292185433948827 ) ) ;
#94149 = CARTESIAN_POINT ( 'NONE',  ( 5.337069745634900997, 6.255611453776062980, 1.199719254218452047 ) ) ;
#94151 = CARTESIAN_POINT ( 'NONE',  ( 0.2331563151865694850, 5.724144821786467219, -2.539778028485844441 ) ) ;
#94152 = CARTESIAN_POINT ( 'NONE',  ( 5.671403949121008203, 1.101820082107987098, 1.475039313902235305 ) ) ;
#94153 = DIRECTION ( 'NONE',  ( 0.000000000000000000, 0.000000000000000000, 1.000000000000000000 ) ) ;
#94154 = CARTESIAN_POINT ( 'NONE',  ( 4.729096653068339151, 4.411700938201493116, -0.7998128361456211532 ) ) ;
#94155 = CARTESIAN_POINT ( 'NONE',  ( 3.276077977556953513, -1.028358954114884094, 1.384488693430762085 ) ) ;
#94156 = CARTESIAN_POINT ( 'NONE',  ( 1.112517963266421939, 1.944731545904467396, 0.5331650539944567946 ) ) ;
#94157 = CARTESIAN_POINT ( 'NONE',  ( 2.883697495508124042, -0.6696099726914479522, -2.198986239785024388 ) ) ;
#94158 = CARTESIAN_POINT ( 'NONE',  ( 2.829655204463392693, -2.111994357890615071, 0.8116228763568857918 ) ) ;
#94159 = CARTESIAN_POINT ( 'NONE',  ( 5.338542076627605937, 2.074711179890481816, 0.3611063368853023592 ) ) ;
#94160 = CARTESIAN_POINT ( 'NONE',  ( -6.617788377246196951, 7.853746207276256719, -1.082531754730549967 ) ) ;
#94161 = CARTESIAN_POINT ( 'NONE',  ( 3.180641231044952555, -0.1265111898236283006, -1.765250312072360162 ) ) ;
#94162 = CARTESIAN_POINT ( 'NONE',  ( 4.313465427442102929, 8.184126765324453601, 0.7998128361456462443 ) ) ;
#94164 = CARTESIAN_POINT ( 'NONE',  ( 6.567932727852480390, -1.414834124515697011, 1.804577934655810401 ) ) ;
#94163 = CARTESIAN_POINT ( 'NONE',  ( 5.085717018457579286, 6.066329622022862189, -1.082531754730548412 ) ) ;
#94165 = CARTESIAN_POINT ( 'NONE',  ( 4.101369424419714527, -1.836060619117799497, 0.1375280490283348478 ) ) ;
#94166 = CARTESIAN_POINT ( 'NONE',  ( -5.610376637956639101, 5.439860920571172542, 0.000000000000000000 ) ) ;
#94167 = CARTESIAN_POINT ( 'NONE',  ( 5.544921637864819175, 7.492161215640853023, -1.443375672974057666 ) ) ;
#94168 = CARTESIAN_POINT ( 'NONE',  ( -1.500000000000013101, 3.129166666666689967, -0.8660254037844313801 ) ) ;
#94169 = PRESENTATION_LAYER_ASSIGNMENT (  '', '', ( #104674 ) ) ;
#94170 = CARTESIAN_POINT ( 'NONE',  ( 4.699289266375740404, -0.5861454505808120219, 2.111544493182772708 ) ) ;
#94171 = CARTESIAN_POINT ( 'NONE',  ( -4.517891501851816649, 6.293959390292322986, -1.599625672291256295 ) ) ;
#94172 = CARTESIAN_POINT ( 'NONE',  ( 0.4583599637079645572, 7.954360040268206866, -1.947354497276407415 ) ) ;
#94173 = LINE ( 'NONE', #110467, #138763 ) ;
#94174 =( BOUNDED_CURVE ( )  B_SPLINE_CURVE ( 2, ( #27165, #125828, #74866, #121562, #23958, #39163, #158261, #206979, #171287 ),
 .UNSPECIFIED., .F., .T. ) 
 B_SPLINE_CURVE_WITH_KNOTS ( ( 3, 2, 2, 2, 3 ),
 ( 0.4791666666666666852, 0.4861111111111111049, 0.5000000000000000000, 0.5138888888888888395, 0.5208333333333333703 ),
 .UNSPECIFIED. ) 
 CURVE ( )  GEOMETRIC_REPRESENTATION_ITEM ( )  RATIONAL_B_SPLINE_CURVE ( ( 0.9330127018922194093, 0.9330127018922196314, 1.000000000000000000, 0.8660254037844387076, 1.000000000000000000, 0.8660254037844387076, 1.000000000000000000, 0.9330127018922187432, 0.9330127018922192983 ) ) 
 REPRESENTATION_ITEM ( '' )  );
#94175 = CARTESIAN_POINT ( 'NONE',  ( -0.6823417656249969321, 4.967708333674755394, -1.181850606188749264 ) ) ;
#94176 = CARTESIAN_POINT ( 'NONE',  ( 3.404829243095872648, 1.518349439661485389, -1.185654278882039669 ) ) ;
#94177 = CARTESIAN_POINT ( 'NONE',  ( -1.364683531250010295, 8.380208333674730170, 0.7879004041258445001 ) ) ;
#94178 = CARTESIAN_POINT ( 'NONE',  ( -4.636525346193588248, 4.511627113421689650, 0.7216878364870317197 ) ) ;
#94179 = CARTESIAN_POINT ( 'NONE',  ( -0.03451705771533463557, -1.778989527951052141, 1.330178892887582398 ) ) ;
#94180 = ORIENTED_EDGE ( 'NONE', *, *, #146400, .T. ) ;
#94182 = CARTESIAN_POINT ( 'NONE',  ( -1.164422670175135899, 3.300000000000025135, -0.7116747751938151678 ) ) ;
#94181 = CARTESIAN_POINT ( 'NONE',  ( 4.517335436343452137, 8.499999999999996447, 0.7749999999999996891 ) ) ;
#94183 = CARTESIAN_POINT ( 'NONE',  ( 3.194917754314666514, 6.879154480009089134, 0.7998128361456321445 ) ) ;
#94184 = CARTESIAN_POINT ( 'NONE',  ( 6.183927461164522299, 6.387205924212962849, 0.000000000000000000 ) ) ;
#94185 = CARTESIAN_POINT ( 'NONE',  ( 1.499999999999993117, 11.13541666734946389, 0.8660254037844408170 ) ) ;
#94186 = FACE_OUTER_BOUND ( 'NONE', #197922, .T. ) ;
#94187 = DIRECTION ( 'NONE',  ( -0.000000000000000000, -1.000000000000000000, -0.000000000000000000 ) ) ;
#94188 = CARTESIAN_POINT ( 'NONE',  ( 0.1858947801188018389, -1.204007190563995078, -1.549573762531175625 ) ) ;
#94189 = CARTESIAN_POINT ( 'NONE',  ( -1.201851678989727383E-14, 1.134375000341418582, 1.575800808251672791 ) ) ;
#94190 = CARTESIAN_POINT ( 'NONE',  ( 6.614160618316515361, -1.014195557614630205, -1.909021090911746654 ) ) ;
#94191 = CARTESIAN_POINT ( 'NONE',  ( 5.336364984333265227, -1.091323163865608459, 1.630109012322231266 ) ) ;
#94192 = CARTESIAN_POINT ( 'NONE',  ( -8.971744963941075568, 11.49012176272984931, 1.599625672291269396 ) ) ;
#94193 = CARTESIAN_POINT ( 'NONE',  ( -5.788968402910818156, 7.776882441527838807, 1.443375672974064550 ) ) ;
#94194 = CARTESIAN_POINT ( 'NONE',  ( 5.682550338946039226, -2.108058120380253087, -0.4779004524640489970 ) ) ;
#94196 = ORIENTED_EDGE ( 'NONE', *, *, #124205, .F. ) ;
#94195 = CARTESIAN_POINT ( 'NONE',  ( -0.2106725631050176684, -0.004273297132624876912, -2.003483006309703995 ) ) ;
#94197 = CARTESIAN_POINT ( 'NONE',  ( -0.6823417656250212460, 5.051041667008086655, 1.181850606188767472 ) ) ;
#94198 = CARTESIAN_POINT ( 'NONE',  ( 0.7724589312842686795, -1.759198622581410021, -0.6360808729843556719 ) ) ;
#94199 = CARTESIAN_POINT ( 'NONE',  ( 6.028594920762765597, 1.707543762964639722, -0.2996114793598329551 ) ) ;
#94201 = CARTESIAN_POINT ( 'NONE',  ( 3.509492838045696672, -2.158849082856160173, 0.3763758916049686487 ) ) ;
#94200 = CARTESIAN_POINT ( 'NONE',  ( -0.6801582343750282034, 0.8489583336747236197, -1.178068619123876282 ) ) ;
#94202 = CARTESIAN_POINT ( 'NONE',  ( 3.311855287401725523, -0.4521268412439309325, 2.262704599374213643 ) ) ;
#94203 = CARTESIAN_POINT ( 'NONE',  ( 6.362583954249420692, -1.460576210990358614, 1.454072064785590479 ) ) ;
#94204 = CARTESIAN_POINT ( 'NONE',  ( 1.587728922880219384, -1.932555244376774617, -0.1907308274580049312 ) ) ;
#94205 = CARTESIAN_POINT ( 'NONE',  ( -7.022760381754429737, 7.295567988242705582, 1.040834085586084257E-14 ) ) ;
#94206 = CARTESIAN_POINT ( 'NONE',  ( 5.588068197455647201, 5.804839949401370269, -0.7313310425167540707 ) ) ;
#94207 = CARTESIAN_POINT ( 'NONE',  ( 5.080389167821143026, 1.047295930500062866, 1.843893106414703054 ) ) ;
#94208 = DIRECTION ( 'NONE',  ( 0.000000000000000000, 0.000000000000000000, 1.000000000000000000 ) ) ;
#94209 = CARTESIAN_POINT ( 'NONE',  ( 2.197888892816081796, 1.802417619043535701, 0.9041091288993635677 ) ) ;
#94210 = CARTESIAN_POINT ( 'NONE',  ( -7.036318535368094373, 7.311385834125318617, 0.7216878364870317197 ) ) ;
#94211 = CARTESIAN_POINT ( 'NONE',  ( 5.913141818906856528, 1.943543578741913969, 1.045239939247793792 ) ) ;
#94212 = CARTESIAN_POINT ( 'NONE',  ( 3.285556943750000514, -0.4010416661887095113, 1.896917185911906500 ) ) ;
#94213 = CARTESIAN_POINT ( 'NONE',  ( -2.298420387838187473, 5.509269730139584986, -0.7346435760097105305 ) ) ;
#94214 = CARTESIAN_POINT ( 'NONE',  ( 6.825078400183572924, 7.629137130509068498, 2.744348168701661095 ) ) ;
#94215 = CARTESIAN_POINT ( 'NONE',  ( -7.075376061485238566, 9.347967719856493218, 1.599625672291269396 ) ) ;
#94217 = CARTESIAN_POINT ( 'NONE',  ( -6.330731382938326490, 6.350551133041632212, 0.7998128361456282587 ) ) ;
#94216 = CARTESIAN_POINT ( 'NONE',  ( -4.636310691425048702, 8.434871236368708836, 0.4628797641644845084 ) ) ;
#94218 = CARTESIAN_POINT ( 'NONE',  ( -10.39320420135713263, 4.932286138528427344, 5.331284845095887626 ) ) ;
#94219 = ORIENTED_EDGE ( 'NONE', *, *, #37214, .F. ) ;
#94220 = CARTESIAN_POINT ( 'NONE',  ( 4.223548136977580469, -1.972658117897459151, 0.5965803236557595257 ) ) ;
#94221 = CARTESIAN_POINT ( 'NONE',  ( -2.353626204688216217E-14, 2.828125000341407347, -1.570758158831798257 ) ) ;
#94222 = ADVANCED_FACE ( 'NONE', ( #201369 ), #39713, .T. ) ;
#94223 = UNCERTAINTY_MEASURE_WITH_UNIT (LENGTH_MEASURE( 1.000000000000000082E-05 ), #192647, 'distance_accuracy_value', 'NONE');
#94224 = CARTESIAN_POINT ( 'NONE',  ( 0.3249880009247422818, 6.544903501124678336, -3.185264000678197149 ) ) ;
#94225 = CARTESIAN_POINT ( 'NONE',  ( -5.416646063859567484, 6.278174148379618735, 1.199719254218450271 ) ) ;
#94226 = CARTESIAN_POINT ( 'NONE',  ( -4.915125982297082530, 6.864361322996670012, 1.451325963391773888 ) ) ;
#94227 = CARTESIAN_POINT ( 'NONE',  ( 4.652993067401423488, 0.3473450764862345830, 1.989417523455960568 ) ) ;
#94228 = CARTESIAN_POINT ( 'NONE',  ( -1.201851678989727383E-14, 1.212500000000025002, 1.732050807568877637 ) ) ;
#94230 = CARTESIAN_POINT ( 'NONE',  ( 9.734391104931955141, 10.45913716528321125, 0.7216878364870438212 ) ) ;
#94229 = CARTESIAN_POINT ( 'NONE',  ( -5.490125858891038213, 5.369844688319787451, -0.7998128361456362523 ) ) ;
#94231 = CARTESIAN_POINT ( 'NONE',  ( 6.632963465583686435, 8.761543347979550589, -1.599625672291262513 ) ) ;
#94232 = CARTESIAN_POINT ( 'NONE',  ( 3.151298293300933029, -1.683901109147158737, -1.187873040408020886 ) ) ;
#94233 = CARTESIAN_POINT ( 'NONE',  ( 3.375625116643202972, -0.3961014713874110305, -1.976955985980306307 ) ) ;
#94234 = VERTEX_POINT ( 'NONE', #163312 ) ;
#94235 = CARTESIAN_POINT ( 'NONE',  ( -3.179715765502671321, 5.975770656120749535, 2.499999999999999556 ) ) ;
#94236 = CARTESIAN_POINT ( 'NONE',  ( 5.678167406024951624, 5.518950149984223508, 0.7998128361456341429 ) ) ;
#94238 = VERTEX_POINT ( 'NONE', #208839 ) ;
#94237 = CARTESIAN_POINT ( 'NONE',  ( -3.011287625495571607, 6.360174617139689346, -0.7852620323503290978 ) ) ;
#94239 = CARTESIAN_POINT ( 'NONE',  ( 2.776720060080526853, -1.994564479802892087, 0.2930246351905210211 ) ) ;
#94240 = CARTESIAN_POINT ( 'NONE',  ( 2.448939195788137013, 0.4911642875529352303, -1.774347143093172097 ) ) ;
#94241 = CARTESIAN_POINT ( 'NONE',  ( 1.120229914364691659, -2.250463172007353130, 0.5101417434775123994 ) ) ;
#94242 = CARTESIAN_POINT ( 'NONE',  ( 3.739016502318667445, 7.584212696005614873, 0.7998128361456271485 ) ) ;
#94243 = CARTESIAN_POINT ( 'NONE',  ( 2.495597164219889308, 1.669172397749154380, 1.373402732410613725 ) ) ;
#94244 = CARTESIAN_POINT ( 'NONE',  ( -6.600121851754250812, 6.594563670001734046, 0.7998128361456341429 ) ) ;
#94245 = ORIENTED_EDGE ( 'NONE', *, *, #153873, .F. ) ;
#94246 = CARTESIAN_POINT ( 'NONE',  ( -5.000000000000013323, 8.499999999999996447, -0.7750000000000013545 ) ) ;
#94247 = CARTESIAN_POINT ( 'NONE',  ( 1.111929834214450796, -0.8377583890188080584, -1.672643128629976772 ) ) ;
#94248 = ORIENTED_EDGE ( 'NONE', *, *, #170147, .T. ) ;
#94249 = EDGE_CURVE ( 'NONE', #100328, #53173, #179273, .T. ) ;
#94250 = CARTESIAN_POINT ( 'NONE',  ( 6.034049845351773023, 0.9722699467793812778, -1.714982496439126924 ) ) ;
#94252 = CARTESIAN_POINT ( 'NONE',  ( 8.473482818416664841, 10.90881592628469932, -1.443375672974063439 ) ) ;
#94251 = CARTESIAN_POINT ( 'NONE',  ( -1.364683531249997417, 3.259375000341423245, 1.214306433183764966E-14 ) ) ;
#94254 = CARTESIAN_POINT ( 'NONE',  ( 0.6103625832605160673, -2.195865045534075133, 0.2202409711149767024 ) ) ;
#94253 = CARTESIAN_POINT ( 'NONE',  ( -6.684333426737305572, 7.757142738403693727, -1.199719254218446718 ) ) ;
#94255 = CARTESIAN_POINT ( 'NONE',  ( 6.461392557816405535, 1.719054114842766268, 1.153505076091146053 ) ) ;
#94256 = CARTESIAN_POINT ( 'NONE',  ( 7.332262146892202459, 7.448727347662698506, -0.7998128361456281477 ) ) ;
#94257 = CARTESIAN_POINT ( 'NONE',  ( -4.225337428953291230, 8.081310767087481750, 0.7998128361456341429 ) ) ;
#94258 = CARTESIAN_POINT ( 'NONE',  ( 6.639320575229294086, 2.948176855103799454, 2.655556053213734558 ) ) ;
#94259 = CARTESIAN_POINT ( 'NONE',  ( 5.401234739183408351, 1.611344100708357097, 1.135629011227519358 ) ) ;
#94260 = CARTESIAN_POINT ( 'NONE',  ( 6.240491321897984278, 1.159586379754873331, -1.653562141909877603 ) ) ;
#94261 = CARTESIAN_POINT ( 'NONE',  ( 0.7499999999999885647, 0.5145833340161540814, 1.299038105676657340 ) ) ;
#94262 = CARTESIAN_POINT ( 'NONE',  ( 5.022255751415273473, -1.231121986244879452, -1.951710362602774307 ) ) ;
#94263 = CARTESIAN_POINT ( 'NONE',  ( 1.991156689281988745, 0.1981002678682428353, 2.053003549438499054 ) ) ;
#94264 = CARTESIAN_POINT ( 'NONE',  ( 8.107412671292047790, 8.560995659369956101, 0.7216878364870458196 ) ) ;
#94265 = CARTESIAN_POINT ( 'NONE',  ( 4.667750024854814050, 8.667735138964429709, -0.7998128361456381397 ) ) ;
#94266 = CARTESIAN_POINT ( 'NONE',  ( 3.739016502318667445, 7.584212696005614873, 0.7998128361456271485 ) ) ;
#94267 = CARTESIAN_POINT ( 'NONE',  ( -1.364683531250012516, 2.301041667008087988, -0.7879004041258289570 ) ) ;
#94268 = CARTESIAN_POINT ( 'NONE',  ( 5.415556014015861841, 5.282846535965431300, -0.7998128361456481317 ) ) ;
#94269 = CARTESIAN_POINT ( 'NONE',  ( 4.487385655998867406, 8.179107665399927285, 0.7216878364870438212 ) ) ;
#94270 = CARTESIAN_POINT ( 'NONE',  ( 4.773980394326226673, -2.130202496963151670, 0.4190362392007019876 ) ) ;
#94272 = CARTESIAN_POINT ( 'NONE',  ( 4.616662711240536510, -0.08544939198026380023, 1.839383977539174264 ) ) ;
#94271 = CARTESIAN_POINT ( 'NONE',  ( -3.131570295076647525, 6.597323077657299528, 1.040834085586084257E-14 ) ) ;
#94274 = CARTESIAN_POINT ( 'NONE',  ( 6.720655732516650716, 1.268691918110446570, 2.040305333170799429 ) ) ;
#94273 = DIRECTION ( 'NONE',  ( -0.9999980456341537316, 0.000000000000000000, -0.001977050295949902767 ) ) ;
#94275 = CARTESIAN_POINT ( 'NONE',  ( 6.023007056224171762, -2.064090639567913499, 0.7368321019862942300 ) ) ;
#94276 = DIRECTION ( 'NONE',  ( -5.578564026256490882E-16, -1.000000000000000000, -9.066213480720158442E-32 ) ) ;
#94277 = CARTESIAN_POINT ( 'NONE',  ( 6.069232182892009497, 0.1736634173518056545, -2.255917496054614446 ) ) ;
#94278 = ORIENTED_EDGE ( 'NONE', *, *, #184994, .F. ) ;
#94279 = CARTESIAN_POINT ( 'NONE',  ( -3.990254785474510513, 7.829054500403880290, -0.2746884413801879976 ) ) ;
#94280 = CARTESIAN_POINT ( 'NONE',  ( -2.974122065066389098, 6.685841390114815042, -0.001386224338680421084 ) ) ;
#94281 = CARTESIAN_POINT ( 'NONE',  ( 5.403926048761924505, 7.658933883257522446, 1.327442161737320436 ) ) ;
#94282 = AXIS2_PLACEMENT_3D ( 'NONE', #27452, #14120, #197155 ) ;
#94283 = CARTESIAN_POINT ( 'NONE',  ( -5.600926855776901192, 5.707038551260711579, -0.7216878364870338292 ) ) ;
#94284 = CARTESIAN_POINT ( 'NONE',  ( 4.909461021924256485, 4.900328411765999981, 0.7216878364870338292 ) ) ;
#94285 = CARTESIAN_POINT ( 'NONE',  ( 1.094210320218844679, -0.4249228298987791086, -1.717946482988210510 ) ) ;
#94286 = CARTESIAN_POINT ( 'NONE',  ( 4.951819039462027838, -1.425199631963388391, -1.421988410718623586 ) ) ;
#94287 = CARTESIAN_POINT ( 'NONE',  ( 5.307127064745490230, 8.279066444590018392, -1.199719254218452935 ) ) ;
#94288 = CARTESIAN_POINT ( 'NONE',  ( 4.331157237497373025, 0.1008371559532254685, 2.103664472247131378 ) ) ;
#94289 = CARTESIAN_POINT ( 'NONE',  ( 1.774859612008858667, 1.665787454739732221, -0.9457685036825744795 ) ) ;
#94290 = LINE ( 'NONE', #23911, #73989 ) ;
#94291 = CARTESIAN_POINT ( 'NONE',  ( 2.980859429886784984, 1.853565342000351501, 0.6662430357459552255 ) ) ;
#94292 = CARTESIAN_POINT ( 'NONE',  ( 6.047130097259819870, 0.2019483658235003143, 2.009690058136243351 ) ) ;
#94293 = CARTESIAN_POINT ( 'NONE',  ( 1.885419139999934934, 1.287927767047767125, 1.356919574424742203 ) ) ;
#94296 = VERTEX_POINT ( 'NONE', #144472 ) ;
#94295 = CARTESIAN_POINT ( 'NONE',  ( 1.617294888471169312, 1.591762500684265946, 1.059657513450793953 ) ) ;
#94294 = CARTESIAN_POINT ( 'NONE',  ( 5.479022876622000382, -0.04827441000932602283, -1.724383337574379116 ) ) ;
#94298 = CARTESIAN_POINT ( 'NONE',  ( 4.148431816101584957, 6.823292304551739740, -1.082531754730548412 ) ) ;
#94297 = CARTESIAN_POINT ( 'NONE',  ( 1.366164030173490973, 2.173753390890633685, -0.3800739277931909355 ) ) ;
#94299 = CARTESIAN_POINT ( 'NONE',  ( -0.6823417656250212460, 2.363541667008084435, 1.181850606188767472 ) ) ;
#94300 = CARTESIAN_POINT ( 'NONE',  ( 8.860417081730671995, 10.29590700256267155, 1.199719254218453823 ) ) ;
#94301 = CARTESIAN_POINT ( 'NONE',  ( 6.508674657442179878, 1.384610780642284711, -1.258058027910214927 ) ) ;
#94302 = SURFACE_SIDE_STYLE ('',( #110595 ) ) ;
#94303 = CARTESIAN_POINT ( 'NONE',  ( -4.822949958159302497, 6.649860922651057216, -1.599625672291256517 ) ) ;
#94304 = CYLINDRICAL_SURFACE ( 'NONE', #37236, 12.00000000000000178 ) ;
#94305 = EDGE_LOOP ( 'NONE', ( #15681, #94196, #118591, #87987 ) ) ;
#94306 = CARTESIAN_POINT ( 'NONE',  ( 2.471216696211364638, 1.848302923701108158, 0.9330170062570308787 ) ) ;
#94307 = CARTESIAN_POINT ( 'NONE',  ( 1.499999999999989120, 2.254166666666685970, 0.8660254037844524744 ) ) ;
#94308 = CARTESIAN_POINT ( 'NONE',  ( 5.178324605415663306, 8.128796908705222535, 1.199719254218462483 ) ) ;
#94309 = CARTESIAN_POINT ( 'NONE',  ( -6.340409392685171674, 10.54889472477470846, 0.7998128361456481317 ) ) ;
#94310 = CARTESIAN_POINT ( 'NONE',  ( 4.913904330310220558, 4.697586238308844919, 0.000000000000000000 ) ) ;
#94311 = CARTESIAN_POINT ( 'NONE',  ( 6.586587867412674768, -1.305319418013479948, 1.671791285998667442 ) ) ;
#94312 = CARTESIAN_POINT ( 'NONE',  ( 0.6823417656249899377, 2.592708333674753618, 1.181850606188767472 ) ) ;
#94313 = VERTEX_POINT ( 'NONE', #75159 ) ;
#94315 = CARTESIAN_POINT ( 'NONE',  ( 3.684065054611349144, 5.321161868511784299, -1.599625672291262513 ) ) ;
#94314 = CARTESIAN_POINT ( 'NONE',  ( -11.41267819554183127, 3.499999999999989342, 3.708203932499423150 ) ) ;
#94316 = CARTESIAN_POINT ( 'NONE',  ( 3.936874915731437774, 1.117662071392529377, 1.677747830363854664 ) ) ;
#94317 = CARTESIAN_POINT ( 'NONE',  ( 4.628101268237789334, 1.911029739866540345, 0.1345505791198585988 ) ) ;
#94318 = FILL_AREA_STYLE ('',( #28225 ) ) ;
#94319 = CARTESIAN_POINT ( 'NONE',  ( 3.140350738262797314, 0.5347024899306859202, 2.125194831261326911 ) ) ;
#94320 = CARTESIAN_POINT ( 'NONE',  ( 0.1335669894368343991, 0.2365985627143319114, -2.188050374159770772 ) ) ;
#94321 = CARTESIAN_POINT ( 'NONE',  ( -1.402160292154681736E-14, 0.4937500006828175469, 1.732050807568877637 ) ) ;
#94322 = CARTESIAN_POINT ( 'NONE',  ( 5.168231636832498310, 2.010700947019973039, -0.1031825239030410013 ) ) ;
#94323 = CARTESIAN_POINT ( 'NONE',  ( -5.910464900553636269, 8.982960586366182554, -1.199719254218440723 ) ) ;
#94325 = CARTESIAN_POINT ( 'NONE',  ( 6.327753876788817955, 0.8101538176374730726, -1.956283944203747849 ) ) ;
#94324 = CARTESIAN_POINT ( 'NONE',  ( -2.494337075234348777, 5.853884321174607663, -0.7216878364870267237 ) ) ;
#94326 = CARTESIAN_POINT ( 'NONE',  ( -1.364683531250010295, 9.192708333674733723, 0.7879004041258445001 ) ) ;
#94328 = CARTESIAN_POINT ( 'NONE',  ( -7.618755976236585958, 7.853246491889623648, 0.000000000000000000 ) ) ;
#94327 = CARTESIAN_POINT ( 'NONE',  ( 3.122686798916929352, 0.05371976762510695391, 2.090236283336026180 ) ) ;
#94330 = ORIENTED_EDGE ( 'NONE', *, *, #76833, .T. ) ;
#94329 = CARTESIAN_POINT ( 'NONE',  ( 2.291662735322400835, -0.7404417586454847822, 1.557896076775511451 ) ) ;
#94331 = CARTESIAN_POINT ( 'NONE',  ( 5.414351406770180120, -2.120778210838507150, 0.002142078463891750485 ) ) ;
#94332 = CARTESIAN_POINT ( 'NONE',  ( 4.299907273828439180, 8.168308919441841454, 1.040834085586084257E-14 ) ) ;
#94333 = AXIS2_PLACEMENT_3D ( 'NONE', #148694, #167078, #166003 ) ;
#94334 = CARTESIAN_POINT ( 'NONE',  ( -7.439168848973998216, -6.893137084989842123, -8.103009739377998955 ) ) ;
#94335 = CARTESIAN_POINT ( 'NONE',  ( 0.6124999999999932720, 0.9166666666666906105, -1.060881119635955327 ) ) ;
#94336 = CARTESIAN_POINT ( 'NONE',  ( -9.345711740228745512, 14.55696679586869458, 7.452166123624950345 ) ) ;
#94337 = CARTESIAN_POINT ( 'NONE',  ( 5.957918438201454059, 9.038323046955323292, -1.199719254218440723 ) ) ;
#94338 = ORIENTED_EDGE ( 'NONE', *, *, #94666, .T. ) ;
#94339 = CARTESIAN_POINT ( 'NONE',  ( 3.046854503058775254, 2.800000000000017586, 2.500000000000000444 ) ) ;
#94340 = CARTESIAN_POINT ( 'NONE',  ( 1.260107830910334181, 1.809384220011617028, 0.08917393313457448734 ) ) ;
#94341 = CARTESIAN_POINT ( 'NONE',  ( -4.869349725602420520, 8.832658446511480577, 1.040834085586084257E-14 ) ) ;
#94342 = VERTEX_POINT ( 'NONE', #46948 ) ;
#94343 = CARTESIAN_POINT ( 'NONE',  ( 2.842405760359353106, 6.467890487061221272, -0.7998128361456291469 ) ) ;
#94344 = ORIENTED_EDGE ( 'NONE', *, *, #31584, .T. ) ;
#94345 = CARTESIAN_POINT ( 'NONE',  ( 6.235824307642648279, 6.239826211863360506, 0.000000000000000000 ) ) ;
#94346 = CARTESIAN_POINT ( 'NONE',  ( 2.683996807801437789, 0.9705641499191748345, 1.529316921005590357 ) ) ;
#94347 = CARTESIAN_POINT ( 'NONE',  ( 0.6500564563262788420, 3.349926606758537151, -0.06808518787146825013 ) ) ;
#94348 = CARTESIAN_POINT ( 'NONE',  ( 4.662511749779700843, 6.863130753939731932, 1.222702295491843616 ) ) ;
#94349 = EDGE_CURVE ( 'NONE', #7772, #79400, #61039, .T. ) ;
#94350 = CARTESIAN_POINT ( 'NONE',  ( 3.543253484755361615, 1.683469864222198797, -0.7936445362404942472 ) ) ;
#94351 = CARTESIAN_POINT ( 'NONE',  ( 1.124461781556247431, 0.3751114458506888405, 1.878329865892948813 ) ) ;
#94352 = CARTESIAN_POINT ( 'NONE',  ( 1.096400207583309028, -0.4391605778215034173, -1.771851442210800709 ) ) ;
#94353 = CARTESIAN_POINT ( 'NONE',  ( -10.39025099420812204, 3.467171072964039702, 5.998814208453899788 ) ) ;
#94354 = DIRECTION ( 'NONE',  ( 0.000000000000000000, 0.000000000000000000, 1.000000000000000000 ) ) ;
#94355 = CARTESIAN_POINT ( 'NONE',  ( 5.871284023695358734, 7.173991544917035945, 1.145568358895364458 ) ) ;
#94356 =( LENGTH_UNIT ( ) NAMED_UNIT ( * ) SI_UNIT ( .MILLI., .METRE. ) );
#94357 = CARTESIAN_POINT ( 'NONE',  ( -2.982430605326328532, 5.462957558647244305, -1.082531754730543971 ) ) ;
#94358 = CARTESIAN_POINT ( 'NONE',  ( 7.944714827928050838, 9.331550723079971021, 1.082531754730558626 ) ) ;
#94359 = CARTESIAN_POINT ( 'NONE',  ( 5.348484190341658007, -1.954120660473107396, -0.2448405522006945334 ) ) ;
#94360 = CARTESIAN_POINT ( 'NONE',  ( -3.418627288940168096, 7.140148937072163804, -0.7998128361456281477 ) ) ;
#94361 = CARTESIAN_POINT ( 'NONE',  ( -0.4841690447253781393, 6.868374222573313759, 3.676448113726332068 ) ) ;
#94362 = CARTESIAN_POINT ( 'NONE',  ( 0.6739141125756157313, -1.159797070128726793, 1.739218980263528946 ) ) ;
#94363 = CARTESIAN_POINT ( 'NONE',  ( 7.476431642932036326, 10.80992178580769014, 1.199719254218460707 ) ) ;
#94364 = CARTESIAN_POINT ( 'NONE',  ( 4.893539313097565291, 1.427316681580325763, 1.293898783310668987 ) ) ;
#94365 = CARTESIAN_POINT ( 'NONE',  ( -4.394814349124112951, 8.279033840620114049, -0.7998128361456281477 ) ) ;
#94366 = CARTESIAN_POINT ( 'NONE',  ( 0.8326870614539466642, 0.1294382003846420159, 1.821050407652326619 ) ) ;
#94367 = CARTESIAN_POINT ( 'NONE',  ( 1.875870136999336246, 2.111227540014638304, -0.6426800678154331870 ) ) ;
#94368 = CARTESIAN_POINT ( 'NONE',  ( -6.162041457555802459, 6.982316563411976595, 0.9201402841920912623 ) ) ;
#94369 = CARTESIAN_POINT ( 'NONE',  ( -0.1581436608063293003, -1.178060542814472367, -1.506996232563104776 ) ) ;
#94370 =( BOUNDED_SURFACE ( )  B_SPLINE_SURFACE ( 3, 3, ( 
 ( #4811, #24284, #90390, #25370, #70893, #91470, #9126, #75202 ),
 ( #141313, #44860, #193213, #128316, #63213, #12313, #146629, #13389 ),
 ( #176972, #127243, #58946, #110964, #143442, #60012, #142371, #158588 ),
 ( #28589, #79465, #129377, #94677, #125103, #191061, #112044, #10188 ),
 ( #126165, #42726, #159654, #194279, #80533, #108834, #160719, #29661 ),
 ( #174860, #179110, #26439, #62158, #92549, #192129, #45924, #145582 ),
 ( #78394, #209439, #144514, #210522, #178045, #30732, #109907, #96815 ) ),
 .UNSPECIFIED., .T., .F., .F. ) 
 B_SPLINE_SURFACE_WITH_KNOTS ( ( 4, 3, 4 ),
 ( 4, 2, 2, 4 ),
 ( 0.000000000000000000, 0.5000000000000000000, 1.000000000000000000 ),
 ( 0.000000000000000000, 0.08643212109064293824, 0.5432160605453214552, 1.000000000000000000 ),
 .UNSPECIFIED. ) 
 GEOMETRIC_REPRESENTATION_ITEM ( )  RATIONAL_B_SPLINE_SURFACE ( (
 ( 1.000000000000000000, 1.000000000000000000, 1.000000000000000000, 1.000000000000000000, 1.000000000000000000, 1.000000000000000000, 1.000000000000000000, 1.000000000000000000),
 ( 0.3333333333333333703, 0.3333333333333333703, 0.3333333333333333703, 0.3333333333333333703, 0.3333333333333333703, 0.3333333333333333703, 0.3333333333333333703, 0.3333333333333333703),
 ( 0.3333333333333333703, 0.3333333333333333703, 0.3333333333333333703, 0.3333333333333333703, 0.3333333333333333703, 0.3333333333333333703, 0.3333333333333333703, 0.3333333333333333703),
 ( 1.000000000000000000, 1.000000000000000000, 1.000000000000000000, 1.000000000000000000, 1.000000000000000000, 1.000000000000000000, 1.000000000000000000, 1.000000000000000000),
 ( 0.3333333333333333703, 0.3333333333333333703, 0.3333333333333333703, 0.3333333333333333703, 0.3333333333333333703, 0.3333333333333333703, 0.3333333333333333703, 0.3333333333333333703),
 ( 0.3333333333333333703, 0.3333333333333333703, 0.3333333333333333703, 0.3333333333333333703, 0.3333333333333333703, 0.3333333333333333703, 0.3333333333333333703, 0.3333333333333333703),
 ( 1.000000000000000000, 1.000000000000000000, 1.000000000000000000, 1.000000000000000000, 1.000000000000000000, 1.000000000000000000, 1.000000000000000000, 1.000000000000000000) ) ) 
 REPRESENTATION_ITEM ( '' )  SURFACE ( )  );
#94371 = CARTESIAN_POINT ( 'NONE',  ( 0.4671662993806492414, 1.711898730999446228, 0.9738141270322558940 ) ) ;
#94372 = CARTESIAN_POINT ( 'NONE',  ( 3.017060306806388148, -1.870969668351904147, 0.5203628790987256947 ) ) ;
#94373 = CARTESIAN_POINT ( 'NONE',  ( 0.6673420201736457447, -0.6766069248959759586, -1.899328980164962877 ) ) ;
#94375 = CARTESIAN_POINT ( 'NONE',  ( 5.172628746253565168, 1.285086882066178937, -1.346197146212588347 ) ) ;
#94374 = CARTESIAN_POINT ( 'NONE',  ( -4.132202957115018727, 8.042930226601317401, 0.000000000000000000 ) ) ;
#94377 = CARTESIAN_POINT ( 'NONE',  ( 4.199993725183334803, 8.122019456014369254, -0.7998128361456362523 ) ) ;
#94376 = B_SPLINE_CURVE_WITH_KNOTS ( 'NONE', 3,
 ( #69031, #118941, #184921, #36545, #4025, #105871 ),
 .UNSPECIFIED., .F., .F.,
 ( 4, 2, 4 ),
 ( 0.000000000000000000, 0.0003038051859056658437, 0.0006076103718113316874 ),
 .UNSPECIFIED. ) ;
#94378 = DIRECTION ( 'NONE',  ( 5.551115123125765446E-17, 0.000000000000000000, -1.000000000000000000 ) ) ;
#94379 = CARTESIAN_POINT ( 'NONE',  ( 9.398826802771546696, 11.98838390803207865, -1.599625672291262513 ) ) ;
#94380 = CARTESIAN_POINT ( 'NONE',  ( -3.893162665418476109, 7.693773542963529444, 1.040834085586084257E-14 ) ) ;
#94381 = CARTESIAN_POINT ( 'NONE',  ( -7.370792787684826486, 8.628288336167626582, -1.199719254218452047 ) ) ;
#94382 = CARTESIAN_POINT ( 'NONE',  ( 1.101424459656743071, -0.5276332240332289869, 2.126988402630063835 ) ) ;
#94383 = CARTESIAN_POINT ( 'NONE',  ( 3.931501358282940117, 4.649468341827285300, -1.082531754730543083 ) ) ;
#94384 = CARTESIAN_POINT ( 'NONE',  ( 7.635176783151273128, 8.936736330878529699, 1.199719254218452935 ) ) ;
#94385 = FILL_AREA_STYLE ('',( #178827 ) ) ;
#94386 = CARTESIAN_POINT ( 'NONE',  ( 2.332394550857110893, 1.770734860448031300, 0.4440693575865002907 ) ) ;
#94387 = CARTESIAN_POINT ( 'NONE',  ( -4.322352044658376968, 3.937165561723182883, 0.7998128361456341429 ) ) ;
#94388 = CARTESIAN_POINT ( 'NONE',  ( -4.952806187693842510, 4.672695395264567786, 0.7998128361456341429 ) ) ;
#94389 = CIRCLE ( 'NONE', #115297, 0.1999999999999999833 ) ;
#94390 = CARTESIAN_POINT ( 'NONE',  ( -5.994696786504495556, 7.186261032347766253, -1.212264510017725394 ) ) ;
#94391 = FACE_OUTER_BOUND ( 'NONE', #211778, .T. ) ;
#94392 = CARTESIAN_POINT ( 'NONE',  ( 10.07778825365955733, 10.65184113889131012, -0.7998128361456281477 ) ) ;
#94393 = CIRCLE ( 'NONE', #174018, 1.250000000000000222 ) ;
#94394 = CARTESIAN_POINT ( 'NONE',  ( 1.471183419133621717, 0.1424870401847652956, -1.921283849777700947 ) ) ;
#94395 = CARTESIAN_POINT ( 'NONE',  ( 5.067221110791254368, 1.704927679941736329, 0.9703409489375603991 ) ) ;
#94396 = CARTESIAN_POINT ( 'NONE',  ( -8.389798128758148010, 8.682519326506312751, 0.7998128361456462443 ) ) ;
#94397 = CARTESIAN_POINT ( 'NONE',  ( 6.471319392424407901, 6.444294134116939077, 0.7998128361456341429 ) ) ;
#94398 = CARTESIAN_POINT ( 'NONE',  ( 5.003566749295822014, -2.181051155298455058, 0.2145382695054529609 ) ) ;
#94399 = CARTESIAN_POINT ( 'NONE',  ( 4.416205349749310116, 6.175325546172741653, 1.599625672291267175 ) ) ;
#94400 = ADVANCED_FACE ( 'NONE', ( #11205 ), #192082, .F. ) ;
#94401 = CARTESIAN_POINT ( 'NONE',  ( 4.539934223682924319, 1.348354173984022575, 1.571082123823979826 ) ) ;
#94403 = CARTESIAN_POINT ( 'NONE',  ( -1.402160292154681736E-14, 0.7593750003414168059, -1.575800808251659024 ) ) ;
#94402 = PLANE ( 'NONE',  #82325 ) ;
#94404 = ORIENTED_EDGE ( 'NONE', *, *, #4848, .F. ) ;
#94405 = CARTESIAN_POINT ( 'NONE',  ( 3.621995078338976715, 0.3387333280310041994, 2.273515639168000035 ) ) ;
#94407 = ORIENTED_EDGE ( 'NONE', *, *, #97869, .T. ) ;
#94406 = CARTESIAN_POINT ( 'NONE',  ( 8.459924665247367415, 8.972259652317825740, -0.7216878364870267237 ) ) ;
#94409 = CARTESIAN_POINT ( 'NONE',  ( -1.642778471875000035, -1.217708332855376607, -2.845375778867859751 ) ) ;
#94408 = CARTESIAN_POINT ( 'NONE',  ( 4.082413651490639062, 7.776916670132135501, 0.000000000000000000 ) ) ;
#94410 = CARTESIAN_POINT ( 'NONE',  ( -11.48806469435255373, 13.83089772872446943, 3.468902948106700634 ) ) ;
#94411 = LINE ( 'NONE', #160450, #2432 ) ;
#94412 = CARTESIAN_POINT ( 'NONE',  ( 3.925673184153520179, 1.037972095618071133, -1.641099617876127015 ) ) ;
#94413 = ORIENTED_EDGE ( 'NONE', *, *, #167966, .F. ) ;
#94414 = CARTESIAN_POINT ( 'NONE',  ( 5.666945020832219626, 5.713783400500051179, 0.7216878364870037421 ) ) ;
#94415 = ORIENTED_EDGE ( 'NONE', *, *, #174519, .F. ) ;
#94416 = CARTESIAN_POINT ( 'NONE',  ( 5.009976098083095408, -0.6827417919906975108, 1.786564173047608062 ) ) ;
#94417 = CARTESIAN_POINT ( 'NONE',  ( 5.877914075457827181, 1.031193140389017548, 1.382412309478407542 ) ) ;
#94418 = CARTESIAN_POINT ( 'NONE',  ( 4.575407832915947104, 1.497500392235490807, 1.350737390116145242 ) ) ;
#94419 = CARTESIAN_POINT ( 'NONE',  ( 3.524756749872931305, 7.056040608253012714, -0.7216878364870155105 ) ) ;
#94420 = CARTESIAN_POINT ( 'NONE',  ( 2.034064749695370100, -1.442962035976073309, -1.669870808145665020 ) ) ;
#94422 = CARTESIAN_POINT ( 'NONE',  ( -3.472296738875691346, 6.104744391113324120, 1.082531754730549967 ) ) ;
#94421 = CARTESIAN_POINT ( 'NONE',  ( -9.022061154889962964, 12.61315621642528129, -1.199719254218446718 ) ) ;
#94424 = CARTESIAN_POINT ( 'NONE',  ( 0.6547154952327862709, -1.491839214215221698, -0.9519326369243490404 ) ) ;
#94423 = CARTESIAN_POINT ( 'NONE',  ( 2.150438955405692631, -1.615297803084648098, 1.327229747913031055 ) ) ;
#94425 = CARTESIAN_POINT ( 'NONE',  ( 5.485000066852382616, -2.016597020608828839, 0.002808655738886777897 ) ) ;
#94427 = CARTESIAN_POINT ( 'NONE',  ( 2.941680396524527286, 0.8243158943622121981, -2.139088555740241038 ) ) ;
#94426 = CARTESIAN_POINT ( 'NONE',  ( 4.603875680292229156, 7.528882839386387360, 1.199719254218452047 ) ) ;
#94428 = CARTESIAN_POINT ( 'NONE',  ( 1.077605773158099023, -1.697095445269660496, -0.3847248992609655915 ) ) ;
#94429 = CIRCLE ( 'NONE', #198132, 9.500000000000001776 ) ;
#94430 = CARTESIAN_POINT ( 'NONE',  ( 3.076547362214879566, 0.9570632234598417387, 1.892448740577145738 ) ) ;
#94431 = CARTESIAN_POINT ( 'NONE',  ( 11.92619525870751573, 11.02622296793679979, -1.328859154004804699 ) ) ;
#94432 = CARTESIAN_POINT ( 'NONE',  ( 1.106332979110283610, 0.7092076354480534306, -1.582373438193741322 ) ) ;
#94433 = CARTESIAN_POINT ( 'NONE',  ( 0.6801582343749900117, 1.338541667008072533, -1.178068619123872729 ) ) ;
#94434 = CARTESIAN_POINT ( 'NONE',  ( -11.52888687719587146, 12.30576874894960682, 3.331331986263616152 ) ) ;
#94435 = CARTESIAN_POINT ( 'NONE',  ( 0.7663804396884700276, -2.160669279729439562, 0.2131170157090022665 ) ) ;
#94436 = CARTESIAN_POINT ( 'NONE',  ( 3.292204118033771110, -0.8216723425069611952, -1.841733987974409237 ) ) ;
#94437 = CARTESIAN_POINT ( 'NONE',  ( 3.531250000000002220, -0.7852924748301699509, -1.895863743164005744 ) ) ;
#94438 = CARTESIAN_POINT ( 'NONE',  ( -0.7500000000000215383, 1.472916667349486008, 1.299038105676659116 ) ) ;
#94439 = CARTESIAN_POINT ( 'NONE',  ( 6.164670984062957437, -1.360496472042394656, 1.364235590486153837 ) ) ;
#94440 = CARTESIAN_POINT ( 'NONE',  ( 1.364683531249997417, 13.48437500034139980, 2.602085213965210642E-15 ) ) ;
#94441 = CARTESIAN_POINT ( 'NONE',  ( 3.234858691920166951, 1.406421598713000432, -1.719528915531160385 ) ) ;
#94442 = VERTEX_POINT ( 'NONE', #109861 ) ;
#94443 = FACE_OUTER_BOUND ( 'NONE', #115437, .T. ) ;
#94444 = CARTESIAN_POINT ( 'NONE',  ( 0.7499999999999885647, -0.2666666666666442365, 1.299038105676657340 ) ) ;
#94445 = CARTESIAN_POINT ( 'NONE',  ( 7.228468454380276853, 11.58496363008569574, 1.040834085586084257E-14 ) ) ;
#94446 = CARTESIAN_POINT ( 'NONE',  ( -15.75000000000000000, 10.19999999999999929, -0.7000000000000009548 ) ) ;
#94447 = CARTESIAN_POINT ( 'NONE',  ( 5.741712943377584644, 1.738890731700697412, 0.07666446624409603561 ) ) ;
#94448 = CARTESIAN_POINT ( 'NONE',  ( 4.826587731031282580, -1.282962940432516907, 1.484285152025546672 ) ) ;
#94450 = CARTESIAN_POINT ( 'NONE',  ( -5.666945020832185875, 7.634521829102760115, 1.443375672974064550 ) ) ;
#94449 = CARTESIAN_POINT ( 'NONE',  ( 2.846322183865124700, 5.408127416896231665, -1.199719254218446718 ) ) ;
#94451 = CARTESIAN_POINT ( 'NONE',  ( -1.436299488671407332, 4.080021472972510388, 0.4486666144298727121 ) ) ;
#94452 = CARTESIAN_POINT ( 'NONE',  ( 4.394006599171666139, -0.8711832027283890056, 2.088141772348524050 ) ) ;
#94453 = VECTOR ( 'NONE', #108821, 1000.000000000000000 ) ;
#94454 = CARTESIAN_POINT ( 'NONE',  ( 2.436046450607622926, 1.266989887546982052, 1.627633791282004250 ) ) ;
#94455 = CARTESIAN_POINT ( 'NONE',  ( -7.705111371268023923, 7.883718109434487253, 1.040834085586084257E-14 ) ) ;
#94456 = VERTEX_POINT ( 'NONE', #142326 ) ;
#94457 = CARTESIAN_POINT ( 'NONE',  ( -1.500000000000001332, 0.9312500006828163812, 0.000000000000000000 ) ) ;
#94458 = CARTESIAN_POINT ( 'NONE',  ( 4.200366636497298245, -0.5845007089231197828, -1.776970133648393624 ) ) ;
#94459 = CARTESIAN_POINT ( 'NONE',  ( 2.742450610247765486, 1.725592070310760118, -0.1720703960508932762 ) ) ;
#94460 = CARTESIAN_POINT ( 'NONE',  ( 5.899973326018037589, -0.7874313895239596350, -2.045375389432432467 ) ) ;
#94461 = CARTESIAN_POINT ( 'NONE',  ( 1.431021430919703574, 2.126993092707793132, 0.5877070120439558121 ) ) ;
#94462 = CARTESIAN_POINT ( 'NONE',  ( 3.731458613173586514, -1.998165266068991253, 0.8252760040215676440 ) ) ;
#94463 = CARTESIAN_POINT ( 'NONE',  ( 4.857337426984369877, 1.920559571908975194, -0.2866867867914507650 ) ) ;
#94464 = CARTESIAN_POINT ( 'NONE',  ( 4.000000000000012434, 5.999999999999998224, 0.7500000000000006661 ) ) ;
#94465 = FILL_AREA_STYLE_COLOUR ( '', #24458 ) ;
#94466 = LINE ( 'NONE', #195147, #172998 ) ;
#94467 = CARTESIAN_POINT ( 'NONE',  ( -3.128205532383699694, 2.800000000000122835, -2.480558432692051785 ) ) ;
#94469 = CARTESIAN_POINT ( 'NONE',  ( 5.467422714486909641, -1.967887220244109558, -0.4390321945699494632 ) ) ;
#94468 =( GEOMETRIC_REPRESENTATION_CONTEXT ( 3 ) GLOBAL_UNCERTAINTY_ASSIGNED_CONTEXT ( ( #109455 ) ) GLOBAL_UNIT_ASSIGNED_CONTEXT ( ( #90516, #122019, #203157 ) ) REPRESENTATION_CONTEXT ( 'NONE', 'WORKASPACE' ) );
#94470 = CARTESIAN_POINT ( 'NONE',  ( -9.504429378379839477, 11.04725468198666150, 1.199719254218462483 ) ) ;
#94471 = CARTESIAN_POINT ( 'NONE',  ( 8.932124273304774320, 9.315233161810734686, 0.7998128361456462443 ) ) ;
#94472 = DIRECTION ( 'NONE',  ( -0.000000000000000000, -1.000000000000000000, -0.000000000000000000 ) ) ;
#94473 = CARTESIAN_POINT ( 'NONE',  ( 2.930095790256614485, 1.013914413367119627, -1.518051517300327502 ) ) ;
#94474 = CARTESIAN_POINT ( 'NONE',  ( 2.204404769108789797, -2.206272049354717879, 0.05393164079612459277 ) ) ;
#94475 = VERTEX_POINT ( 'NONE', #125061 ) ;
#94476 = CARTESIAN_POINT ( 'NONE',  ( -4.950135482320929370, 5.908151163196758482, -1.082531754730549967 ) ) ;
#94477 = EDGE_CURVE ( 'NONE', #88062, #56290, #175875, .T. ) ;
#94478 = CARTESIAN_POINT ( 'NONE',  ( -1.642778471875000035, -2.355208332855376341, -2.845375778867859751 ) ) ;
#94479 = CARTESIAN_POINT ( 'NONE',  ( -7.133561379084627063, 11.47423870890741782, 0.7998128361456481317 ) ) ;
#94480 = CARTESIAN_POINT ( 'NONE',  ( 0.6506561817731060238, 1.990614601344290691, 0.3409984238087642727 ) ) ;
#94481 = CARTESIAN_POINT ( 'NONE',  ( 0.7684181764250408442, 2.117871390293009526, -0.1079879263860619443 ) ) ;
#94483 = CARTESIAN_POINT ( 'NONE',  ( -7.247736482492767252, 15.00000000000521538, -10.57961706324489626 ) ) ;
#94482 = VECTOR ( 'NONE', #190863, 1000.000000000000000 ) ;
#94484 = VERTEX_POINT ( 'NONE', #207278 ) ;
#94485 = CARTESIAN_POINT ( 'NONE',  ( -5.529746549527323474, 7.544733289238903851, -1.599625672291271394 ) ) ;
#94486 = CARTESIAN_POINT ( 'NONE',  ( 1.762329786688419109, -0.6638292341827031207, -1.738725725234435693 ) ) ;
#94487 = CARTESIAN_POINT ( 'NONE',  ( 3.344057444064992168, 7.053150784717805877, 1.040834085586084257E-14 ) ) ;
#94488 = CARTESIAN_POINT ( 'NONE',  ( 0.2862814217290919894, -1.017545141758866789, 1.907252267444502269 ) ) ;
#94489 = CARTESIAN_POINT ( 'NONE',  ( 5.871720251644387822, -0.2986239867289949834, -1.994071864161291119 ) ) ;
#94490 = ORIENTED_EDGE ( 'NONE', *, *, #122294, .F. ) ;
#94491 = ORIENTED_EDGE ( 'NONE', *, *, #156739, .T. ) ;
#94492 = CARTESIAN_POINT ( 'NONE',  ( -7.947050595904583403, 12.42330946186405249, 0.7998128361456481317 ) ) ;
#94493 = CARTESIAN_POINT ( 'NONE',  ( 3.562960707638890501, -1.610701098693729350, -0.8595150645765645692 ) ) ;
#94495 = CARTESIAN_POINT ( 'NONE',  ( -5.512600778122673795, 6.408089294489160537, -1.271103323116394845 ) ) ;
#94494 = CARTESIAN_POINT ( 'NONE',  ( -4.573896719763875574, 6.429575154514868274, -1.599625672291271394 ) ) ;
#94496 = CARTESIAN_POINT ( 'NONE',  ( 6.367678427751853221, 6.924687757192571347, 0.8275186136274095272 ) ) ;
#94497 = CARTESIAN_POINT ( 'NONE',  ( 6.309922681198771421, -1.704675833164914778, 1.076154833852351000 ) ) ;
#94498 = CARTESIAN_POINT ( 'NONE',  ( 5.947170714876299336, 0.5300644225827764178, -1.763184533696081857 ) ) ;
#94499 = CARTESIAN_POINT ( 'NONE',  ( -0.02299388927990211537, 2.886218872804919400, -2.399728103386359557 ) ) ;
#94500 = CARTESIAN_POINT ( 'NONE',  ( 4.231326342634161186, 0.1110341807785204943, 2.305146914567071548 ) ) ;
#94501 = CARTESIAN_POINT ( 'NONE',  ( 5.367048706163317640, 7.354919138647580290, -1.599625672291281386 ) ) ;
#94502 = CARTESIAN_POINT ( 'NONE',  ( 6.397764797294555272, -0.7349420381566433846, 2.032942830986879557 ) ) ;
#94503 = CARTESIAN_POINT ( 'NONE',  ( 7.793239369756836510, 7.986534107671458216, 0.7998128361456341429 ) ) ;
#94504 = CARTESIAN_POINT ( 'NONE',  ( 1.751409898207861415, 1.936723520591139058, -0.1449614948935191994 ) ) ;
#94505 = ORIENTED_EDGE ( 'NONE', *, *, #156087, .T. ) ;
#94506 = CARTESIAN_POINT ( 'NONE',  ( 4.499567255430725332, 2.252980053716880704, 0.4539551632626090405 ) ) ;
#94507 = PLANE ( 'NONE',  #151847 ) ;
#94508 = CARTESIAN_POINT ( 'NONE',  ( -7.533490631048818109, 8.818102486758951031, -1.199719254218452047 ) ) ;
#94509 = CARTESIAN_POINT ( 'NONE',  ( 4.522238337509359773, 1.150754656758418593, -1.474723989322044959 ) ) ;
#94510 = EDGE_LOOP ( 'NONE', ( #94081, #205953, #59263, #193229 ) ) ;
#94513 = CARTESIAN_POINT ( 'NONE',  ( -5.906512197408906317, 6.919960980845699439, -1.199719254218453823 ) ) ;
#94512 = CARTESIAN_POINT ( 'NONE',  ( -1.500000000000015099, 0.4104166673494891726, -0.8660254037844383745 ) ) ;
#94511 = CARTESIAN_POINT ( 'NONE',  ( 2.566550162062298579, 0.6480892470011965223, 1.799338185917313870 ) ) ;
#94514 = CARTESIAN_POINT ( 'NONE',  ( 3.545738602337618506, -1.670889076328873069, -1.441789439710974063 ) ) ;
#94515 = CARTESIAN_POINT ( 'NONE',  ( -1.499999999999997558, 8.654128368560041196, -2.562285273914164829 ) ) ;
#94516 = CARTESIAN_POINT ( 'NONE',  ( 3.185802909086937973, 6.660594460669328143, 0.7216878364870317197 ) ) ;
#94517 = CARTESIAN_POINT ( 'NONE',  ( 6.360183458142179447, 6.592837920686898556, -0.7216878364870458196 ) ) ;
#94518 = CARTESIAN_POINT ( 'NONE',  ( -6.089020385868862739, 8.197219431637373432, -1.443375672974066548 ) ) ;
#94519 = CARTESIAN_POINT ( 'NONE',  ( 2.196496099369545263, -0.5219070890916230887, -1.900975273168264534 ) ) ;
#94520 = CARTESIAN_POINT ( 'NONE',  ( 1.571738265064129836, 0.1679657064320304316, -2.301541284809864862 ) ) ;
#94521 = CARTESIAN_POINT ( 'NONE',  ( 2.664445928352857429, -0.7481792696971515388, -1.813797970468238985 ) ) ;
#94522 = CARTESIAN_POINT ( 'NONE',  ( 4.570507181582611267, 8.346359121906111511, 0.000000000000000000 ) ) ;
#94523 = CARTESIAN_POINT ( 'NONE',  ( 5.594603800059450904, 2.031116569408123240, 0.3580809986778245024 ) ) ;
#94524 = CARTESIAN_POINT ( 'NONE',  ( 4.012850279964918165, 7.625483060026979842, -0.7216878364870197293 ) ) ;
#94525 = CARTESIAN_POINT ( 'NONE',  ( 5.987861119090863049, 7.014868056141362551, 1.199719254218452047 ) ) ;
#94526 = ORIENTED_EDGE ( 'NONE', *, *, #38147, .T. ) ;
#94527 = CARTESIAN_POINT ( 'NONE',  ( -2.788906526875773208E-15, 10.18750000000000000, -1.499999999999998446 ) ) ;
#94528 = CARTESIAN_POINT ( 'NONE',  ( -4.916039773278787273, 4.881957280557857715, 0.5603013081572870702 ) ) ;
#94529 = CARTESIAN_POINT ( 'NONE',  ( 2.806174607904299734, 5.257325561654889512, -1.082531754730543083 ) ) ;
#94530 = CARTESIAN_POINT ( 'NONE',  ( 2.149520630032801805, 1.890536112741852959, -1.067247343769129442 ) ) ;
#94531 = FACE_OUTER_BOUND ( 'NONE', #213135, .T. ) ;
#94532 = CARTESIAN_POINT ( 'NONE',  ( 0.000000000000000000, -0.9200000000000041478, 11.00000000000000178 ) ) ;
#94533 = CARTESIAN_POINT ( 'NONE',  ( 2.424885678431305092, -0.004389691185376768875, 1.870726058193001196 ) ) ;
#94534 = CARTESIAN_POINT ( 'NONE',  ( 6.626263010475290649, 1.250585457657760635, -1.762915812992614129 ) ) ;
#94536 = CARTESIAN_POINT ( 'NONE',  ( 3.446398949047553728, 6.321615207124993141, 1.107993529894048645 ) ) ;
#94535 = CARTESIAN_POINT ( 'NONE',  ( -0.02224634325196857623, 5.718740092702407907, -2.883150554214870098 ) ) ;
#94537 = CARTESIAN_POINT ( 'NONE',  ( -1.364683531250014514, -0.01145833299191483488, -0.7879004041258359514 ) ) ;
#94538 = CARTESIAN_POINT ( 'NONE',  ( 2.244649938279310142, 1.855272219182309668, 0.4629769397326845004 ) ) ;
#94539 = AXIS2_PLACEMENT_3D ( 'NONE', #194301, #174880, #26460 ) ;
#94540 = B_SPLINE_CURVE_WITH_KNOTS ( 'NONE', 3,
 ( #88874, #11854, #179715, #62740, #129975, #60614, #127856 ),
 .UNSPECIFIED., .F., .F.,
 ( 4, 3, 4 ),
 ( 0.000000000000000000, 4.270488675891472745E-05, 4.488495215206831637E-05 ),
 .UNSPECIFIED. ) ;
#94541 = CARTESIAN_POINT ( 'NONE',  ( 4.363939919551316216, 0.8349522575829392279, 1.560488599360178474 ) ) ;
#94542 = CARTESIAN_POINT ( 'NONE',  ( 1.822773347178743286, 1.416086463930026573, -1.285276961632122683 ) ) ;
#94543 = AXIS2_PLACEMENT_3D ( 'NONE', #87298, #168547, #137127 ) ;
#94544 = CARTESIAN_POINT ( 'NONE',  ( -5.928993247877788697, 5.811580298812519807, 0.7998128361456341429 ) ) ;
#94546 = CARTESIAN_POINT ( 'NONE',  ( -0.1532965272393977951, -1.712378426511364404, -0.8589627718659180733 ) ) ;
#94545 = SURFACE_STYLE_USAGE ( .BOTH. , #129252 ) ;
#94547 = CARTESIAN_POINT ( 'NONE',  ( -1.500000000000013101, 0.4208333333333572068, 0.8660254037844403729 ) ) ;
#94548 = CARTESIAN_POINT ( 'NONE',  ( 1.029834584532058672, 1.995790600324919506, -0.5504719462680053299 ) ) ;
#94549 = CARTESIAN_POINT ( 'NONE',  ( -1.364683531250014514, -0.9072916663252470482, 0.7879004041258379498 ) ) ;
#94550 = CARTESIAN_POINT ( 'NONE',  ( 8.014278199453780616, 8.522615118883788199, 0.000000000000000000 ) ) ;
#94551 = CARTESIAN_POINT ( 'NONE',  ( 5.049604242677837362, 0.5861553263475408615, -1.776501995420045832 ) ) ;
#94552 = CARTESIAN_POINT ( 'NONE',  ( 1.453431991042982041, 0.5316948868413253759, -1.746555546766684675 ) ) ;
#94554 = CARTESIAN_POINT ( 'NONE',  ( 5.094250900851895025, 7.824382189606214233, 1.140223938556598871 ) ) ;
#94553 = CARTESIAN_POINT ( 'NONE',  ( 4.248781725523794073, 0.5872999373685274804, 2.127227798101683387 ) ) ;
#94555 = CARTESIAN_POINT ( 'NONE',  ( 1.364683531249988757, -0.6156249996585803075, 0.000000000000000000 ) ) ;
#94556 = CARTESIAN_POINT ( 'NONE',  ( 2.910651161647914265, 0.6924047515337331538, 1.943132885215630878 ) ) ;
#94557 = CARTESIAN_POINT ( 'NONE',  ( -8.853638004923878313, 10.28799807962136548, 1.199719254218462483 ) ) ;
#94558 = CARTESIAN_POINT ( 'NONE',  ( 1.272148008267887986, 3.722367574780562460, -0.4878157535072898954 ) ) ;
#94559 = CARTESIAN_POINT ( 'NONE',  ( 1.499999999999990896, 8.627523663848661428, 2.580000000000000515 ) ) ;
#94560 = CARTESIAN_POINT ( 'NONE',  ( 6.964048179274811012, 8.153752959689313684, 1.199719254218452047 ) ) ;
#94561 = ORIENTED_EDGE ( 'NONE', *, *, #152940, .F. ) ;
#94562 = CARTESIAN_POINT ( 'NONE',  ( 5.248515149483167441, -2.054309126314420642, -0.2569322651706855143 ) ) ;
#94563 = CARTESIAN_POINT ( 'NONE',  ( -1.364683531250014514, 0.09270833367475767028, 0.7879004041258379498 ) ) ;
#94564 = CARTESIAN_POINT ( 'NONE',  ( 2.917419293707240069, -0.2150262876145451196, 2.150894318904146729 ) ) ;
#94565 = CARTESIAN_POINT ( 'NONE',  ( -4.646665375593996394, 8.329970469126573462, 0.4085986083085801912 ) ) ;
#94566 = CARTESIAN_POINT ( 'NONE',  ( 2.684245096118286877, 1.082265567382127758, 1.705031398228576078 ) ) ;
#94567 = CARTESIAN_POINT ( 'NONE',  ( -3.294945724223623085, 7.655198976062502325, 2.499999999999998668 ) ) ;
#94570 = CARTESIAN_POINT ( 'NONE',  ( 6.643132081016111634, 9.733775946952057723, 1.082531754730558626 ) ) ;
#94569 = CARTESIAN_POINT ( 'NONE',  ( -3.474999999999998312, -1.020833333333332815, 2.006292185433951047 ) ) ;
#94568 = CARTESIAN_POINT ( 'NONE',  ( 10.20634067979362669, 1.972237431424148646, 5.892633538918198965 ) ) ;
#94571 = CARTESIAN_POINT ( 'NONE',  ( -5.004368096775595021, 5.971422546727199077, 1.082531754730549078 ) ) ;
#94572 = CARTESIAN_POINT ( 'NONE',  ( 1.200408080392855181, 1.350732740426639822, -1.497504596960941958 ) ) ;
#94574 = CARTESIAN_POINT ( 'NONE',  ( 5.847271748948593029, 0.6375361197438635941, -2.096799129279611762 ) ) ;
#94573 = CARTESIAN_POINT ( 'NONE',  ( -5.416646063859567484, 6.278174148379618735, 1.199719254218450271 ) ) ;
#94575 = CARTESIAN_POINT ( 'NONE',  ( -1.499999999999997780, 4.431250000682819490, 1.214306433183764966E-14 ) ) ;
#94576 = CARTESIAN_POINT ( 'NONE',  ( 4.640819915729988310, 1.831716588661407963, 0.5496940206762626069 ) ) ;
#94577 = CARTESIAN_POINT ( 'NONE',  ( -3.307299406729781399, 5.945934176904983381, -1.199719254218452935 ) ) ;
#94578 = CARTESIAN_POINT ( 'NONE',  ( 6.602457619730767391, 7.765583980183128787, 1.082531754730558626 ) ) ;
#94580 = CARTESIAN_POINT ( 'NONE',  ( 3.040638836679772528, -1.525031945187466098, 1.319243992433154267 ) ) ;
#94579 = CARTESIAN_POINT ( 'NONE',  ( -9.463228032214294316, 10.14278024711257764, 1.040834085586084257E-14 ) ) ;
#94581 = CARTESIAN_POINT ( 'NONE',  ( 0.6823417656249969321, 14.33854166700806232, -1.181850606188757036 ) ) ;
#94582 = CARTESIAN_POINT ( 'NONE',  ( -2.830620210203090181, 6.524417021870718258, 0.000000000000000000 ) ) ;
#94583 = CARTESIAN_POINT ( 'NONE',  ( 5.034089265250761613, 0.8841871275974706457, -1.480748092288231454 ) ) ;
#94584 = CARTESIAN_POINT ( 'NONE',  ( 5.525830126021535449, 8.604496359403894346, -1.199719254218452047 ) ) ;
#94585 = AXIS2_PLACEMENT_3D ( 'NONE', #135843, #106587, #206156 ) ;
#94586 = CARTESIAN_POINT ( 'NONE',  ( 9.408995418203963013, 12.00024729270324286, 1.443375672974076540 ) ) ;
#94587 = CARTESIAN_POINT ( 'NONE',  ( -6.830415307812264025, 7.849261790823902629, -6.717278222822378630 ) ) ;
#94588 = CARTESIAN_POINT ( 'NONE',  ( -5.111060722671894929, 5.065251719313053513, 0.000000000000000000 ) ) ;
#94589 = CARTESIAN_POINT ( 'NONE',  ( 1.340777958403309267, -2.018934908790828597, -0.4573474576154838989 ) ) ;
#94590 = CARTESIAN_POINT ( 'NONE',  ( 6.877413708759195998, -0.1538780216673047430, 2.036608477593480959 ) ) ;
#94591 = ORIENTED_EDGE ( 'NONE', *, *, #52332, .T. ) ;
#94592 = CARTESIAN_POINT ( 'NONE',  ( 6.621734039712152686, -0.3858887922842542673, 1.776151629007856281 ) ) ;
#94593 = CARTESIAN_POINT ( 'NONE',  ( 4.369470645354133431, 8.319742529546998000, 0.7998128361456271485 ) ) ;
#94594 = CARTESIAN_POINT ( 'NONE',  ( -0.1759689521645991239, -0.7750936178016191169, -1.636263868569738600 ) ) ;
#94595 = EDGE_CURVE ( 'NONE', #160775, #55298, #77286, .T. ) ;
#94596 = CARTESIAN_POINT ( 'NONE',  ( 5.275531169048895741, 7.248148678680751189, -1.443375672974078761 ) ) ;
#94597 = CARTESIAN_POINT ( 'NONE',  ( -11.07790593930098311, 11.29999999999999893, -0.7000000000000009548 ) ) ;
#94598 = CARTESIAN_POINT ( 'NONE',  ( 2.713028398602938651, -0.2137989841624072795, 2.180988865010752509 ) ) ;
#94599 = VERTEX_POINT ( 'NONE', #194236 ) ;
#94600 = EDGE_CURVE ( 'NONE', #167139, #84713, #30691, .T. ) ;
#94602 = CARTESIAN_POINT ( 'NONE',  ( 8.402302512167096893, 10.82577223566020841, -1.599625672291268286 ) ) ;
#94601 = CARTESIAN_POINT ( 'NONE',  ( 0.8714495147512549833, -0.2914478312704605889, 1.939986204769503786 ) ) ;
#94603 = CARTESIAN_POINT ( 'NONE',  ( 5.202711523826980766, 1.771732004023411911, 0.7288693050919017313 ) ) ;
#94604 = AXIS2_PLACEMENT_3D ( 'NONE', #25356, #57862, #91456 ) ;
#94605 = CARTESIAN_POINT ( 'NONE',  ( -1.441115678600793926, 8.287243072884518114, 3.161846531485497991 ) ) ;
#94606 = CARTESIAN_POINT ( 'NONE',  ( -5.896403733238388511, 7.170697087194168873, 1.136063563240964802 ) ) ;
#94607 = CARTESIAN_POINT ( 'NONE',  ( -10.46159335054558781, 1.264806443676224301, 5.593087811558907774 ) ) ;
#94608 = CARTESIAN_POINT ( 'NONE',  ( 1.364683531249986537, 0.4052083336747511200, -0.7879004041258309554 ) ) ;
#94610 = ORIENTED_EDGE ( 'NONE', *, *, #111774, .T. ) ;
#94609 = CARTESIAN_POINT ( 'NONE',  ( 4.039966587192250103, 7.657118751792200584, 0.7216878364870298324 ) ) ;
#94611 = CARTESIAN_POINT ( 'NONE',  ( -9.178506806771670412, 9.810605484096178941, 1.040834085586084257E-14 ) ) ;
#94612 = CARTESIAN_POINT ( 'NONE',  ( 2.079201547314021070, -0.1057080177612122057, -2.159229931372666389 ) ) ;
#94613 = CARTESIAN_POINT ( 'NONE',  ( -4.553559489343377287, 6.405848385690952718, -1.599625672291271394 ) ) ;
#94614 = ADVANCED_FACE ( 'NONE', ( #112002 ), #90965, .T. ) ;
#94615 = CARTESIAN_POINT ( 'NONE',  ( 7.078765600110826561, 8.391552967285011988, -1.082531754730548412 ) ) ;
#94616 = CARTESIAN_POINT ( 'NONE',  ( 1.518276268637512194, 1.228937244518006011, -1.350148523839814096 ) ) ;
#94617 = CARTESIAN_POINT ( 'NONE',  ( 0.4330588727801780724, -9.006862915010128035, -9.570206894979136791 ) ) ;
#94618 = CARTESIAN_POINT ( 'NONE',  ( 4.172732250082421324, -1.703408510751417193, -0.6570589383413025786 ) ) ;
#94619 = CONICAL_SURFACE ( 'NONE', #1174, 2.000000000000006217, 0.01725463330310792257 ) ;
#94620 = CARTESIAN_POINT ( 'NONE',  ( 11.19153690645859456, 7.659836902099854683, -3.616912593835723388 ) ) ;
#94621 = CARTESIAN_POINT ( 'NONE',  ( 3.234525475359388391, 1.209690070866603406, -1.481213593849866950 ) ) ;
#94622 = ORIENTED_EDGE ( 'NONE', *, *, #65245, .F. ) ;
#94623 = CARTESIAN_POINT ( 'NONE',  ( 3.982825254072485777, 1.869399454171687180, 0.6202158817144760583 ) ) ;
#94624 = ORIENTED_EDGE ( 'NONE', *, *, #102016, .F. ) ;
#94625 = CARTESIAN_POINT ( 'NONE',  ( 6.286669113786358842, 1.687405947569386999, -0.9612952809280647104 ) ) ;
#94626 = ORIENTED_EDGE ( 'NONE', *, *, #144102, .T. ) ;
#94627 = CARTESIAN_POINT ( 'NONE',  ( -4.925354943514475003, 8.968274210734028529, 0.000000000000000000 ) ) ;
#94629 = CARTESIAN_POINT ( 'NONE',  ( 6.258074605086497932, 0.8102346573028992305, -1.959903593942226685 ) ) ;
#94628 = CARTESIAN_POINT ( 'NONE',  ( -4.125423880308188629, 8.035021303660014880, -0.7998128361456481317 ) ) ;
#94630 = CARTESIAN_POINT ( 'NONE',  ( 7.363486825553451354, 8.723727730301414240, -1.082531754730548412 ) ) ;
#94631 = CARTESIAN_POINT ( 'NONE',  ( 3.598220562318912741, -0.9401235635465958751, 1.665135908046413871 ) ) ;
#94632 = CARTESIAN_POINT ( 'NONE',  ( 5.563869425686542414, 6.377698570463163463, -1.204193420357344557 ) ) ;
#94633 = CARTESIAN_POINT ( 'NONE',  ( -0.5000000000000264233, 3.999999999999976019, -0.4500000000000458633 ) ) ;
#94634 = CARTESIAN_POINT ( 'NONE',  ( 3.040771591214902259, 6.769593633051179005, -0.7998128361456362523 ) ) ;
#94635 = CARTESIAN_POINT ( 'NONE',  ( 4.899092244908956673, -0.2488113327579875855, -1.997608342807774218 ) ) ;
#94636 = LINE ( 'NONE', #122940, #165668 ) ;
#94637 = CARTESIAN_POINT ( 'NONE',  ( 5.777927443424748510, 1.091106472389313131, 1.463626628978510702 ) ) ;
#94638 = CARTESIAN_POINT ( 'NONE',  ( 0.5728211633247158874, 1.428863753495920763, -1.498466819491943047 ) ) ;
#94639 = CARTESIAN_POINT ( 'NONE',  ( -6.697364695470783502, 10.75741654478384035, 0.7216878364870458196 ) ) ;
#94640 = CARTESIAN_POINT ( 'NONE',  ( -5.310352258326699548, 7.640991054048470232, -1.228972953101372223 ) ) ;
#94641 = CARTESIAN_POINT ( 'NONE',  ( 8.134310703387671364E-16, 2.000000000682804924, -1.225000000000021849 ) ) ;
#94642 = CARTESIAN_POINT ( 'NONE',  ( 6.614126560844452385, -0.8839695271746010885, -1.648598838400926692 ) ) ;
#94643 = CARTESIAN_POINT ( 'NONE',  ( 7.637320603199683866, 7.804628880021436288, -0.7998128361456281477 ) ) ;
#94644 = ADVANCED_FACE ( 'NONE', ( #181137, #177955, #165957 ), #212564, .F. ) ;
#94645 = DIRECTION ( 'NONE',  ( 1.000000000000000000, 1.156482317317869753E-15, 0.000000000000000000 ) ) ;
#94646 = CARTESIAN_POINT ( 'NONE',  ( -1.364683531250010295, 11.94270833367473017, 0.7879004041258445001 ) ) ;
#94647 = CARTESIAN_POINT ( 'NONE',  ( -4.086893239515592136, 6.855460315155083251, 1.199719254218464037 ) ) ;
#94649 = CARTESIAN_POINT ( 'NONE',  ( -6.257970421159510188, 9.458660037064859694, 1.199719254218452047 ) ) ;
#94648 = CARTESIAN_POINT ( 'NONE',  ( 1.981037863234367924, 3.482875600935791294, -0.4617754461039013658 ) ) ;
#94650 = CARTESIAN_POINT ( 'NONE',  ( 4.025767975679870325, -1.506360102045413596, 0.8590090823815172971 ) ) ;
#94651 = CARTESIAN_POINT ( 'NONE',  ( -5.413783410558481002, 5.210502155273325720, -0.7998128361456221525 ) ) ;
#94652 = CARTESIAN_POINT ( 'NONE',  ( 1.006788857090525013, 0.5974033793386055446, 1.982218910981221827 ) ) ;
#94653 = CARTESIAN_POINT ( 'NONE',  ( 3.427469813117941744, -1.604901852541072760, -1.381049200617268102 ) ) ;
#94654 = CARTESIAN_POINT ( 'NONE',  ( 4.005544317833563461, 6.760553239859419250, -1.199719254218452047 ) ) ;
#94655 = CARTESIAN_POINT ( 'NONE',  ( 9.074484886248265880, 9.481320543578137361, 0.7998128361456462443 ) ) ;
#94657 = EDGE_CURVE ( 'NONE', #162756, #123444, #78059, .T. ) ;
#94656 = CARTESIAN_POINT ( 'NONE',  ( 0.1613745041668577518, 6.492617261217120017, 3.107428622204797097 ) ) ;
#94658 = CARTESIAN_POINT ( 'NONE',  ( 0.9890311015656474414, 0.1392606914251882932, 1.964554613873798594 ) ) ;
#94659 = CARTESIAN_POINT ( 'NONE',  ( 4.133273095458231516, 7.653358944556723387, 0.7702195724684970379 ) ) ;
#94660 = CARTESIAN_POINT ( 'NONE',  ( 4.772106882330221289, 6.590544000850479200, -1.443375672974051449 ) ) ;
#94662 = DIRECTION ( 'NONE',  ( -8.638326563840814399E-31, 0.000000000000000000, -1.000000000000000000 ) ) ;
#94661 = CARTESIAN_POINT ( 'NONE',  ( -3.475000000000000533, -2.129166666666665542, -2.006292185433948827 ) ) ;
#94663 = CARTESIAN_POINT ( 'NONE',  ( 3.961076342171603315, 0.2821129637899103537, -2.274769079453589526 ) ) ;
#94664 = CARTESIAN_POINT ( 'NONE',  ( 0.9612317138737861422, 0.3586375672061762887, -1.789940867121169843 ) ) ;
#94665 = CARTESIAN_POINT ( 'NONE',  ( 3.216961742616857745, 1.504763323797538410, -1.180078671740567131 ) ) ;
#94666 = EDGE_CURVE ( 'NONE', #108640, #8935, #188610, .T. ) ;
#94667 = CARTESIAN_POINT ( 'NONE',  ( 5.855142236255289845, 7.924361590421551860, -1.599625672291281386 ) ) ;
#94668 = CARTESIAN_POINT ( 'NONE',  ( 6.656690234185433042, 7.828855363713562276, -1.082531754730543971 ) ) ;
#94669 = CARTESIAN_POINT ( 'NONE',  ( -8.809047120577080392, 11.30030761213851953, 1.599625672291269396 ) ) ;
#94670 = CARTESIAN_POINT ( 'NONE',  ( 1.881109812905419343, -1.842300511448742739, -0.8121059663154740482 ) ) ;
#94671 = CARTESIAN_POINT ( 'NONE',  ( 1.744895479173363517, -0.2825750800353257208, -1.941159045430330465 ) ) ;
#94672 = CARTESIAN_POINT ( 'NONE',  ( -8.350932551013499960, 11.83017284523606172, -1.199719254218446718 ) ) ;
#94673 = CARTESIAN_POINT ( 'NONE',  ( -7.497822643557261024, 8.706213491360317747, -1.199719254218446718 ) ) ;
#94674 = CARTESIAN_POINT ( 'NONE',  ( -11.77709913112472684, 7.702278142422434470, -2.066753809368463646 ) ) ;
#94676 = CARTESIAN_POINT ( 'NONE',  ( 3.133429157788733654, -1.187652617478820227, -1.312364946228376628 ) ) ;
#94675 = CARTESIAN_POINT ( 'NONE',  ( 5.015614203636001633, -1.117866415629315435, -1.766478577331761723 ) ) ;
#94677 = CARTESIAN_POINT ( 'NONE',  ( -1.724555757182492988, 14.99999999999692157, 11.68000002332616383 ) ) ;
#94679 = CARTESIAN_POINT ( 'NONE',  ( 5.894527261468666346, 1.877221869688485700, -1.315242172555250555 ) ) ;
#94678 = FILL_AREA_STYLE ('',( #7241 ) ) ;
#94680 = CARTESIAN_POINT ( 'NONE',  ( 4.716618446111438878, -0.08105245650613655817, 1.738572149171065062 ) ) ;
#94681 = CARTESIAN_POINT ( 'NONE',  ( 9.053093885623066939, 11.58502883802551153, -1.599625672291262513 ) ) ;
#94682 = SURFACE_STYLE_USAGE ( .BOTH. , #43798 ) ;
#94683 = CARTESIAN_POINT ( 'NONE',  ( 4.657415279524609986, -0.3804069660688877974, -1.691394979786196684 ) ) ;
#94684 = STYLED_ITEM ( 'NONE', ( #100968 ), #69155 ) ;
#94685 = CARTESIAN_POINT ( 'NONE',  ( 4.246645257758387970, -2.146983142244869747, -0.3225670219409969008 ) ) ;
#94686 = CARTESIAN_POINT ( 'NONE',  ( 2.496672843210871129, 6.064535417054653266, -0.7998128361456291469 ) ) ;
#94687 = CARTESIAN_POINT ( 'NONE',  ( -0.1880716927101276914, -1.308626981353334662, -1.665352682907685233 ) ) ;
#94688 = CARTESIAN_POINT ( 'NONE',  ( 6.000000000000004441, -3.414667428843525066E-13, -2.052068128417939619 ) ) ;
#94689 = AXIS2_PLACEMENT_3D ( 'NONE', #69701, #89198, #188810 ) ;
#94690 = CARTESIAN_POINT ( 'NONE',  ( -0.7500000000000215383, 5.472916667349482900, 1.299038105676671107 ) ) ;
#94691 = CARTESIAN_POINT ( 'NONE',  ( 2.872000511136533873, 1.029149822700244465, 1.628267440728261573 ) ) ;
#94692 = CARTESIAN_POINT ( 'NONE',  ( 1.499999999999997113, 10.42708333401613352, -0.8660254037844378194 ) ) ;
#94693 = CARTESIAN_POINT ( 'NONE',  ( 0.5049021242206577220, -2.205252279087748235, -0.2660074523756980058 ) ) ;
#94694 = VERTEX_POINT ( 'NONE', #49022 ) ;
#94695 = CARTESIAN_POINT ( 'NONE',  ( -0.2411972340275969906, 1.382285239182699854, -2.157708601731861187 ) ) ;
#94696 = CARTESIAN_POINT ( 'NONE',  ( 1.499999999999987121, 2.795833333333352488, -0.8660254037844262731 ) ) ;
#94697 = CARTESIAN_POINT ( 'NONE',  ( 4.638861114170084399, 8.563755066507100722, 0.7998128361456462443 ) ) ;
#94698 = CARTESIAN_POINT ( 'NONE',  ( 2.280208067491045654, 2.177836876428246971, -0.4364916025852043635 ) ) ;
#94699 = FACE_OUTER_BOUND ( 'NONE', #169669, .T. ) ;
#94700 = CARTESIAN_POINT ( 'NONE',  ( 7.239690840017413365, 10.42976116578691403, -1.082531754730537976 ) ) ;
#94701 = CARTESIAN_POINT ( 'NONE',  ( -10.26315909542058336, 11.07603315418659840, -0.7216878364870267237 ) ) ;
#94702 = CARTESIAN_POINT ( 'NONE',  ( 4.927462483923885195, 4.713404084191450849, -0.7998128361456481317 ) ) ;
#94703 = CARTESIAN_POINT ( 'NONE',  ( 0.4225002777262388265, -1.427939226333583500, -1.423959630194884696 ) ) ;
#94705 = CARTESIAN_POINT ( 'NONE',  ( 5.160619382589332282, -0.6916465251813638249, -1.943403241031741002 ) ) ;
#94704 = CARTESIAN_POINT ( 'NONE',  ( 8.052653171512838881, 11.48218023581863001, -1.199719254218446718 ) ) ;
#94706 = CARTESIAN_POINT ( 'NONE',  ( -5.278201874421821316, 5.052323696447222900, 0.7998128361456341429 ) ) ;
#94707 = CARTESIAN_POINT ( 'NONE',  ( -1.001543065824772872E-14, 4.993750000682814161, 1.732050807568877637 ) ) ;
#94708 = CARTESIAN_POINT ( 'NONE',  ( -0.6823417656250003738, 0.9677083336747521747, -1.181850606188749264 ) ) ;
#94709 = CARTESIAN_POINT ( 'NONE',  ( 0.6140562859980386312, 1.226574898224697119, -1.275979240986246710 ) ) ;
#94710 = CARTESIAN_POINT ( 'NONE',  ( 5.449791032962750137, -1.571470184986222263, -0.7336466892688772168 ) ) ;
#94711 = CARTESIAN_POINT ( 'NONE',  ( 6.005355179794888976, -1.726165566969834586, 0.2220549178573327509 ) ) ;
#94712 = CARTESIAN_POINT ( 'NONE',  ( 3.368946006165595364, 0.05471657373835739357, -2.291868861755571363 ) ) ;
#94713 = CARTESIAN_POINT ( 'NONE',  ( -1.602468905319636405E-14, -1.053124999658583638, -1.575800808251665908 ) ) ;
#94714 = CARTESIAN_POINT ( 'NONE',  ( 2.378628397106247849, 1.683441843134887428, -0.7459445200509451368 ) ) ;
#94715 = CARTESIAN_POINT ( 'NONE',  ( 8.048736748007069508, 12.54194330598362406, -0.7998128361456352531 ) ) ;
#94716 = CARTESIAN_POINT ( 'NONE',  ( 1.469576158976824342E-15, 3.999999999999998224, -12.00000000000000355 ) ) ;
#94717 = CARTESIAN_POINT ( 'NONE',  ( 2.080808903162992607, -0.08653491207171599975, -1.823647505904809174 ) ) ;
#94718 = CARTESIAN_POINT ( 'NONE',  ( 2.707657903872981553, 1.899618770239443366, 0.6767133375917554483 ) ) ;
#94719 = CARTESIAN_POINT ( 'NONE',  ( -3.836594282542926226, 5.499112634431936542, 1.443375672974064550 ) ) ;
#94720 = CARTESIAN_POINT ( 'NONE',  ( 6.871661793415180242, 16.00000000000000000, -9.446021445709373410 ) ) ;
#94721 = CARTESIAN_POINT ( 'NONE',  ( 4.419037640130375699, 1.924477966361681780, 0.8556825127635151462 ) ) ;
#94722 = CARTESIAN_POINT ( 'NONE',  ( -5.982172092127739482, 8.002286745614243912, -1.599625672291263179 ) ) ;
#94723 = CARTESIAN_POINT ( 'NONE',  ( 8.310125652063469204, 13.22383526519563368, 8.544412637909269748 ) ) ;
#94724 = CARTESIAN_POINT ( 'NONE',  ( 2.365759603224312446, -0.4558734232973959966, 2.019384234097781228 ) ) ;
#94725 = CARTESIAN_POINT ( 'NONE',  ( 3.005103603723342953, 6.657704637652544832, -0.7998128361456291469 ) ) ;
#94726 = CARTESIAN_POINT ( 'NONE',  ( 0.6801582343749900117, -0.4114583329919083154, -1.178068619123855409 ) ) ;
#94727 = CARTESIAN_POINT ( 'NONE',  ( 4.846395287928321416, 1.089488137594313510, -1.819044145143506208 ) ) ;
#94728 = CARTESIAN_POINT ( 'NONE',  ( 0.3285744372712772199, 1.843197283691574873, 0.5604049541020996728 ) ) ;
#94729 = ORIENTED_EDGE ( 'NONE', *, *, #61508, .F. ) ;
#94730 = CARTESIAN_POINT ( 'NONE',  ( -4.782994330570982555, 8.802186828966616972, 0.000000000000000000 ) ) ;
#94731 = CARTESIAN_POINT ( 'NONE',  ( 10.18233705906309972, 11.83814697611718714, 1.199719254218450271 ) ) ;
#94732 = CARTESIAN_POINT ( 'NONE',  ( 5.953438849732186178, 8.999410187112612647, -1.082531754730548412 ) ) ;
#94733 = CARTESIAN_POINT ( 'NONE',  ( -3.475000000000000533, -1.735416665710752371, -2.006292185433948827 ) ) ;
#94734 = CARTESIAN_POINT ( 'NONE',  ( -4.042302355168801320, 7.867769847672247074, 0.7998128361456341429 ) ) ;
#94735 = CARTESIAN_POINT ( 'NONE',  ( 6.240501835383900797, 1.219778281852833546, -1.734492557903525523 ) ) ;
#94736 = CARTESIAN_POINT ( 'NONE',  ( 1.536301591958776802, 1.038269187514633485, -1.832158284056581543 ) ) ;
#94737 = CARTESIAN_POINT ( 'NONE',  ( -5.829079699232685208, 5.765290835385048496, 0.000000000000000000 ) ) ;
#94738 = CARTESIAN_POINT ( 'NONE',  ( 8.432281472695482449, 11.92507992053172572, 1.199719254218450271 ) ) ;
#94739 = CARTESIAN_POINT ( 'NONE',  ( 5.348444835920818541, -1.846650980718677726, -0.2298375257220597323 ) ) ;
#94740 = CARTESIAN_POINT ( 'NONE',  ( 9.074484886248265880, 9.481320543578137361, 0.7998128361456462443 ) ) ;
#94741 = CARTESIAN_POINT ( 'NONE',  ( -0.4153311931458959494, 3.850000000000006306, 0.5000000000000064393 ) ) ;
#94742 = CARTESIAN_POINT ( 'NONE',  ( -3.851398154733808088, 6.650992392901508232, -1.199719254218450271 ) ) ;
#94743 = CARTESIAN_POINT ( 'NONE',  ( -4.302014814237876017, 3.913438792899272212, 0.7998128361456341429 ) ) ;
#94744 = CARTESIAN_POINT ( 'NONE',  ( -9.949568243101348131, 5.483630524090502334, 6.039417671888569039 ) ) ;
#94745 = DIRECTION ( 'NONE',  ( -5.551115123125766062E-17, 0.000000000000000000, 1.000000000000000000 ) ) ;
#94747 = CARTESIAN_POINT ( 'NONE',  ( 2.277722772326017608, -1.903703133612335119, 0.4737097981617058862 ) ) ;
#94746 = CARTESIAN_POINT ( 'NONE',  ( -7.477485413136760073, 8.682486722536401302, -1.199719254218446718 ) ) ;
#94748 = CARTESIAN_POINT ( 'NONE',  ( 1.077287230265553397, -0.05381693868444264311, -2.161191418701657430 ) ) ;
#94750 = CARTESIAN_POINT ( 'NONE',  ( -6.112394247781385737, 6.011859825068855301, 0.2949881747824866229 ) ) ;
#94749 = CARTESIAN_POINT ( 'NONE',  ( -5.692444392891315097, 7.734547439830227411, -1.599625672291271394 ) ) ;
#94751 = CARTESIAN_POINT ( 'NONE',  ( 1.364683531249986537, 1.113541667008082658, 0.7879004041258500513 ) ) ;
#94752 = CARTESIAN_POINT ( 'NONE',  ( 3.303724397909554078, -1.530444925530007216, 0.8147494179842218465 ) ) ;
#94753 = CARTESIAN_POINT ( 'NONE',  ( 1.886251080576596406, 1.515106702303461894, -0.8561229301769134326 ) ) ;
#94754 = CARTESIAN_POINT ( 'NONE',  ( 6.127922243696800386, 10.09306701771420656, -0.7216878364870267237 ) ) ;
#94755 = CARTESIAN_POINT ( 'NONE',  ( -11.01578653029999266, 5.045029590669321884, -4.264301349201883085 ) ) ;
#94756 = CARTESIAN_POINT ( 'NONE',  ( 0.9485920322965735174, 1.351945250224910744, 1.495824703658617416 ) ) ;
#94757 = CARTESIAN_POINT ( 'NONE',  ( 6.925078400183531713, 7.629137130509035636, 2.844348168701658075 ) ) ;
#94759 = AXIS2_PLACEMENT_3D ( 'NONE', #128302, #12299, #31783 ) ;
#94758 = CARTESIAN_POINT ( 'NONE',  ( -4.634908411025374875, 6.500755460986618495, 1.599625672291263179 ) ) ;
#94760 = CARTESIAN_POINT ( 'NONE',  ( 0.8835904138565253696, 1.322268204680861814, 1.462458760404183433 ) ) ;
#94761 = AXIS2_PLACEMENT_3D ( 'NONE', #123972, #25303, #41588 ) ;
#94763 = CARTESIAN_POINT ( 'NONE',  ( -4.638297949650955765, 8.425448351319163365, 0.7216878364870267237 ) ) ;
#94762 = CARTESIAN_POINT ( 'NONE',  ( 5.888906298306328502, -1.818048641159516476, -0.5935555146628914702 ) ) ;
#94764 = CARTESIAN_POINT ( 'NONE',  ( -5.600926855776877211, 9.548515408466085930, -0.7216878364870338292 ) ) ;
#94765 = CARTESIAN_POINT ( 'NONE',  ( 6.710359684120930091, 6.793450817754725257, 0.7998128361456352531 ) ) ;
#94766 = CARTESIAN_POINT ( 'NONE',  ( -5.824109505522200081, 8.952488968821326054, -1.199719254218452047 ) ) ;
#94767 = CARTESIAN_POINT ( 'NONE',  ( 0.9615888033541221125, -1.593469042607889463, -1.240847856016368489 ) ) ;
#94768 = CARTESIAN_POINT ( 'NONE',  ( 4.050101169753547836, 0.7808133845815302676, -2.171591319759837546 ) ) ;
#94769 = CARTESIAN_POINT ( 'NONE',  ( 6.197705743426439540, -1.420020466879829302, -1.353909852041992767 ) ) ;
#94770 = CARTESIAN_POINT ( 'NONE',  ( 2.746866186719683967, -0.3305370478365337039, -1.933541032166598672 ) ) ;
#94771 = CARTESIAN_POINT ( 'NONE',  ( 8.127223016387999266, 11.56917838817298616, 1.199719254218460707 ) ) ;
#94772 = CARTESIAN_POINT ( 'NONE',  ( -9.351007409505983858, 14.56055123930838668, 7.441777623061154756 ) ) ;
#94773 = ORIENTED_EDGE ( 'NONE', *, *, #20473, .T. ) ;
#94774 = CARTESIAN_POINT ( 'NONE',  ( 0.8665975061730617490, -2.067159395656243515, -0.4576585243742418152 ) ) ;
#94776 = CARTESIAN_POINT ( 'NONE',  ( -6.482770005628665011, 10.71498210654212002, 0.7998128361456481317 ) ) ;
#94775 = CARTESIAN_POINT ( 'NONE',  ( -3.653032323878261600, 6.349289246911547835, -1.199719254218452047 ) ) ;
#94777 = CARTESIAN_POINT ( 'NONE',  ( 2.167674216824653222, -1.133089441918342599, 1.451089449600144521 ) ) ;
#94778 = ORIENTED_EDGE ( 'NONE', *, *, #153278, .F. ) ;
#94779 = CARTESIAN_POINT ( 'NONE',  ( 11.95152720720105322, 7.668029601719960731, -1.099342792201368324 ) ) ;
#94780 = CARTESIAN_POINT ( 'NONE',  ( 2.426173717206762781, -2.096881089210366422, 0.3156149858808757203 ) ) ;
#94781 = CARTESIAN_POINT ( 'NONE',  ( -0.7499999999999972244, 3.889583334016149863, -1.299038105676652011 ) ) ;
#94782 = CARTESIAN_POINT ( 'NONE',  ( 7.567422294721922960, 11.98040977715095323, 0.7998128361456462443 ) ) ;
#94783 =( LENGTH_UNIT ( ) NAMED_UNIT ( * ) SI_UNIT ( .MILLI., .METRE. ) );
#94784 = CARTESIAN_POINT ( 'NONE',  ( 3.690745141589413691, -0.3983964448436724259, -2.021722667813256269 ) ) ;
#94786 = CARTESIAN_POINT ( 'NONE',  ( 0.3625324912872701089, 0.1813134127766780901, -1.832273687604975665 ) ) ;
#94785 = CARTESIAN_POINT ( 'NONE',  ( -9.013473194986783454, 9.410140237106395134, -0.7998128361456291469 ) ) ;
#94787 = CARTESIAN_POINT ( 'NONE',  ( 0.6823417656249899377, 3.676041667008085767, -1.181850606188754593 ) ) ;
#94788 = CARTESIAN_POINT ( 'NONE',  ( 0.07775346131142638062, 0.2253410668615995205, -2.322482355083537175 ) ) ;
#94789 =( BOUNDED_CURVE ( )  B_SPLINE_CURVE ( 2, ( #105508, #38346, #140144, #89250, #57798, #6884, #185646, #39413, #171540 ),
 .UNSPECIFIED., .F., .T. ) 
 B_SPLINE_CURVE_WITH_KNOTS ( ( 3, 2, 2, 2, 3 ),
 ( 0.4017857142857143016, 0.4047619047619047672, 0.4107142857142856984, 0.4166666666666666852, 0.4196428571428570953 ),
 .UNSPECIFIED. ) 
 CURVE ( )  GEOMETRIC_REPRESENTATION_ITEM ( )  RATIONAL_B_SPLINE_CURVE ( ( 0.9330127018922194093, 0.9330127018922194093, 1.000000000000000000, 0.8660254037844387076, 1.000000000000000000, 0.8660254037844387076, 1.000000000000000000, 0.9330127018922206306, 0.9330127018922194093 ) ) 
 REPRESENTATION_ITEM ( '' )  );
#94790 = CARTESIAN_POINT ( 'NONE',  ( 1.400320522945621482, 4.350623259974997659, -0.06109695461879249834 ) ) ;
#94791 = CARTESIAN_POINT ( 'NONE',  ( 0.3466626200071438180, 2.201290530325435757, 0.1579762268871589825 ) ) ;
#94792 = CARTESIAN_POINT ( 'NONE',  ( 3.040562418613635742, 2.244949603584453612, 0.2802003048723368805 ) ) ;
#94793 = CARTESIAN_POINT ( 'NONE',  ( -8.785320351975364872, 12.23299559640450518, 1.082531754730560403 ) ) ;
#94794 = CARTESIAN_POINT ( 'NONE',  ( 2.443383269832733795, -1.689004019812107460, 0.6554920229192174874 ) ) ;
#94795 = CARTESIAN_POINT ( 'NONE',  ( 3.555789339581526320, 1.068723753765013162, 1.589688962476828005 ) ) ;
#94796 = CARTESIAN_POINT ( 'NONE',  ( 4.053231837324381637, 1.750648263899981849, -1.104974720517466480 ) ) ;
#94797 = CARTESIAN_POINT ( 'NONE',  ( 0.6823417656249917140, 3.405208333674754506, 1.181850606188765695 ) ) ;
#94798 = CARTESIAN_POINT ( 'NONE',  ( 1.850399468497238242, 0.6164509289473228959, 1.872685729773468255 ) ) ;
#94799 = CARTESIAN_POINT ( 'NONE',  ( 0.1473221176215748218, -1.486828977120215001, -1.224531343831699592 ) ) ;
#94800 = CARTESIAN_POINT ( 'NONE',  ( 2.764352523130030548, -1.291370965961564421, 1.353630663414123969 ) ) ;
#94801 = ADVANCED_FACE ( 'NONE', ( #130344 ), #113172, .F. ) ;
#94803 = CARTESIAN_POINT ( 'NONE',  ( 4.624709440338444111, 8.453137518702421360, 0.3515692964491355932 ) ) ;
#94802 = CARTESIAN_POINT ( 'NONE',  ( 2.368180137760375281, 2.262835426277497675, -0.4520343961368147312 ) ) ;
#94804 = CARTESIAN_POINT ( 'NONE',  ( 2.804952713220637328, -1.548975583508698683, 1.031263495014663523 ) ) ;
#94805 = CARTESIAN_POINT ( 'NONE',  ( 1.364683531249988535, 2.905208333674754506, -0.7879004041258239610 ) ) ;
#94806 = CARTESIAN_POINT ( 'NONE',  ( 0.2333540202161610289, 0.003568502611739353923, -2.045944795905803471 ) ) ;
#94807 = CARTESIAN_POINT ( 'NONE',  ( -6.735703387890906946, 6.752742128827836865, -0.7998128361456291469 ) ) ;
#94808 = CARTESIAN_POINT ( 'NONE',  ( 5.913327553854682783, 10.05063257947248800, -0.7998128361456291469 ) ) ;
#94809 = CARTESIAN_POINT ( 'NONE',  ( -1.352862181796079533, 3.447832334330404258, -0.3040832447043430586 ) ) ;
#94810 = CARTESIAN_POINT ( 'NONE',  ( 6.001026715709635972, 1.723673884808615497, -1.209685691799726737 ) ) ;
#94811 = CARTESIAN_POINT ( 'NONE',  ( 0.6823417656249917140, 3.655208333674754506, 1.181850606188765695 ) ) ;
#94812 = CARTESIAN_POINT ( 'NONE',  ( 5.923154835166895893, -0.05960684409221649049, 2.160954015416292506 ) ) ;
#94813 = CARTESIAN_POINT ( 'NONE',  ( -0.08762443420157886576, -2.019435065594810119, -0.04520711721162430641 ) ) ;
#94814 = CARTESIAN_POINT ( 'NONE',  ( 1.364683531249986537, -0.3864583329919166199, 0.7879004041258500513 ) ) ;
#94815 = CARTESIAN_POINT ( 'NONE',  ( -4.826339496784927796, 5.693446170079573321, 1.082531754730560403 ) ) ;
#94818 = CARTESIAN_POINT ( 'NONE',  ( 5.016153647376212277, 5.914896012436124728, 1.082531754730558626 ) ) ;
#94817 = CARTESIAN_POINT ( 'NONE',  ( 6.925078400183545035, 3.707308446744279617, 2.270182774727365516 ) ) ;
#94816 = CARTESIAN_POINT ( 'NONE',  ( 5.338878628731272613, 9.450718510153643948, -0.7998128361456481317 ) ) ;
#94819 = CARTESIAN_POINT ( 'NONE',  ( -5.167592825464113915, 6.057888380243431570, 1.199719254218452935 ) ) ;
#94820 = CARTESIAN_POINT ( 'NONE',  ( 4.962125165302472496, -1.116212726388360998, 1.679221540125563905 ) ) ;
#94821 = CARTESIAN_POINT ( 'NONE',  ( -8.389798128758148010, 8.682519326506312751, 0.7998128361456462443 ) ) ;
#94823 = CARTESIAN_POINT ( 'NONE',  ( -7.878696662872776812, 8.364436659539265406, -0.7216878364870338292 ) ) ;
#94822 = CARTESIAN_POINT ( 'NONE',  ( -9.381879110976678149, 11.00824238663667565, 1.082531754730558626 ) ) ;
#94824 = CARTESIAN_POINT ( 'NONE',  ( -1.499999999999997780, 4.900000000000022560, 1.214306433183764966E-14 ) ) ;
#94826 = CARTESIAN_POINT ( 'NONE',  ( 0.6823417656249934904, 9.192708333674733723, 1.181850606188764807 ) ) ;
#94825 = CARTESIAN_POINT ( 'NONE',  ( 6.034075718726629844, 1.069613854859407631, -1.878468107683453514 ) ) ;
#94827 = CARTESIAN_POINT ( 'NONE',  ( -11.68195787049182854, 7.294744277220263307, 2.753462545645998016 ) ) ;
#94829 = CARTESIAN_POINT ( 'NONE',  ( 6.603150281434943203, -0.1430492952050037847, 1.984088717376513822 ) ) ;
#94828 = CARTESIAN_POINT ( 'NONE',  ( -5.707619481228817904, 8.642344580533519505, -1.082531754730537976 ) ) ;
#94830 = CARTESIAN_POINT ( 'NONE',  ( -1.364683531250014514, -0.6572916663252459379, 0.7879004041258379498 ) ) ;
#94831 = EDGE_CURVE ( 'NONE', #17720, #178508, #67510, .T. ) ;
#94832 = DIRECTION ( 'NONE',  ( 1.000000000000000000, -0.000000000000000000, -0.000000000000000000 ) ) ;
#94833 = CARTESIAN_POINT ( 'NONE',  ( 2.033451192367647042, -1.125475165956592694, -1.307177254964901003 ) ) ;
#94834 = CARTESIAN_POINT ( 'NONE',  ( 4.004454267989866700, 5.765225627445230927, 1.599625672291262513 ) ) ;
#94835 = CARTESIAN_POINT ( 'NONE',  ( 5.342795052237045539, 8.390955439988655229, -1.199719254218450271 ) ) ;
#94836 = CARTESIAN_POINT ( 'NONE',  ( -11.94017496638997500, 8.960613251662856271, 1.236227153985048677 ) ) ;
#94837 = CARTESIAN_POINT ( 'NONE',  ( 1.194210174654856127, -0.4229520329555501723, -1.718335688698314101 ) ) ;
#94838 = CARTESIAN_POINT ( 'NONE',  ( 0.8561085696928095734, 0.8139254773164643630, -1.841379974997810143 ) ) ;
#94839 = DIRECTION ( 'NONE',  ( 0.000000000000000000, 0.000000000000000000, 1.000000000000000000 ) ) ;
#94840 = CARTESIAN_POINT ( 'NONE',  ( 3.557846488308267663, 0.5383450771202847873, -2.139971664446515653 ) ) ;
#94841 = CARTESIAN_POINT ( 'NONE',  ( 5.717690620771469945, 0.4309847871033903877, -2.127713340945025511 ) ) ;
#94842 = ORIENTED_EDGE ( 'NONE', *, *, #68964, .T. ) ;
#94843 = CARTESIAN_POINT ( 'NONE',  ( 5.110497557708379546, 4.926945003606695295, -0.7998128361456481317 ) ) ;
#94844 = CARTESIAN_POINT ( 'NONE',  ( 8.717529583462649612, 10.23316793787035195, 1.082531754730558626 ) ) ;
#94846 = CARTESIAN_POINT ( 'NONE',  ( 3.374625213368151133, -0.3961236654455925765, -1.976952669325626299 ) ) ;
#94845 = CARTESIAN_POINT ( 'NONE',  ( 2.807414684038778141, 1.817529592918063708, -1.092056846721880969 ) ) ;
#94848 = ORIENTED_EDGE ( 'NONE', *, *, #119633, .F. ) ;
#94847 = CARTESIAN_POINT ( 'NONE',  ( 3.392628153686805259, -1.747241832701627473, -0.4783254123041839057 ) ) ;
#94849 = CARTESIAN_POINT ( 'NONE',  ( 5.875479466675786355, 7.948088359245467416, -1.599625672291283607 ) ) ;
#94850 = VERTEX_POINT ( 'NONE', #84704 ) ;
#94851 = CARTESIAN_POINT ( 'NONE',  ( 0.4966798268824790252, 1.557709316500059726, -1.035497600327957235 ) ) ;
#94852 = CARTESIAN_POINT ( 'NONE',  ( 6.311484202361478779, 7.322151976631905868, -1.199719254218446718 ) ) ;
#94854 = CARTESIAN_POINT ( 'NONE',  ( 1.428765994036251818, -1.616370030362016985, 1.027966131488191381 ) ) ;
#94853 = CARTESIAN_POINT ( 'NONE',  ( -4.497554271431319250, 6.270232621468402989, -1.599625672291256295 ) ) ;
#94855 = CARTESIAN_POINT ( 'NONE',  ( 0.07459516483346910476, 0.007201286963446154772, -1.755573347271716544 ) ) ;
#94856 = DIRECTION ( 'NONE',  ( -1.224646799147353207E-16, 0.000000000000000000, -1.000000000000000000 ) ) ;
#94857 = CARTESIAN_POINT ( 'NONE',  ( 0.6823417656249899377, 2.155208333674753174, 1.181850606188767472 ) ) ;
#94858 = CARTESIAN_POINT ( 'NONE',  ( 0.000000000000000000, 18.91999999999999815, 0.000000000000000000 ) ) ;
#94859 = CARTESIAN_POINT ( 'NONE',  ( -9.643927338022246332, 10.14567007064778004, -0.7998128361456291469 ) ) ;
#94860 = CARTESIAN_POINT ( 'NONE',  ( 5.260679775997886054, -1.568431141927080219, 1.487858469166832398 ) ) ;
#94861 = CARTESIAN_POINT ( 'NONE',  ( -4.773879485787619892, 7.623257595843924150, 1.082531754730549967 ) ) ;
#94862 = EDGE_CURVE ( 'NONE', #105253, #181416, #185392, .T. ) ;
#94863 = CARTESIAN_POINT ( 'NONE',  ( -6.936931872047518155, 8.122117267924091166, 1.199719254218452047 ) ) ;
#94864 = CARTESIAN_POINT ( 'NONE',  ( 3.603867943843573673, 1.538443694073919898, 1.459757404076333698 ) ) ;
#94866 = CARTESIAN_POINT ( 'NONE',  ( -11.58085191697663241, 6.132731128919016506, 5.153920277027906671 ) ) ;
#94865 = CARTESIAN_POINT ( 'NONE',  ( -0.02988540731103071432, 7.629137130509069387, -2.326318838967501357 ) ) ;
#94867 = CARTESIAN_POINT ( 'NONE',  ( 4.516842978191152547, 1.801120551983675266, 0.8018027747202867150 ) ) ;
#94868 = CARTESIAN_POINT ( 'NONE',  ( 0.2463402104127752068, 1.031448792800106595, -1.728751203700854111 ) ) ;
#94869 = ORIENTED_EDGE ( 'NONE', *, *, #159427, .F. ) ;
#94870 = CARTESIAN_POINT ( 'NONE',  ( 5.348860635491798909, -1.915306066586830669, -0.9028416433708542632 ) ) ;
#94871 = CARTESIAN_POINT ( 'NONE',  ( -2.026920941591053626, 3.691791674785632082, 11.39597588158940411 ) ) ;
#94872 = CARTESIAN_POINT ( 'NONE',  ( 0.6255436495894195481, 0.2045281481408110225, -2.060252820462626477 ) ) ;
#94874 = B_SPLINE_CURVE_WITH_KNOTS ( 'NONE', 3,
 ( #204597, #137511, #55182, #139656, #159075, #191554, #175345, #121328, #124533, #172135, #90897, #56249, #23730, #155884, #171052, #58377 ),
 .UNSPECIFIED., .F., .F.,
 ( 4, 2, 2, 2, 2, 2, 2, 4 ),
 ( 8.701399832109953910E-22, 0.001350634887644582482, 0.002701269775289164964, 0.004051904662933747230, 0.005402539550578328194, 0.006753174438222909158, 0.008103809325867490990, 0.01080507910115665465 ),
 .UNSPECIFIED. ) ;
#94873 = CARTESIAN_POINT ( 'NONE',  ( 2.870961461768199108, 1.843879596475753502, -0.6095136124301904212 ) ) ;
#94875 = ORIENTED_EDGE ( 'NONE', *, *, #17750, .F. ) ;
#94876 = CARTESIAN_POINT ( 'NONE',  ( -3.984117037569407938, 5.741498858621315371, 1.599625672291270506 ) ) ;
#94877 = CARTESIAN_POINT ( 'NONE',  ( 6.984385409695311964, 8.177479728513226576, 1.199719254218452935 ) ) ;
#94879 = CARTESIAN_POINT ( 'NONE',  ( 6.928380191783277908, 8.041863964290678624, 1.199719254218462483 ) ) ;
#94878 = CARTESIAN_POINT ( 'NONE',  ( 2.027394857466585432, -1.366561296588153063, -1.582253647643002914 ) ) ;
#94880 = CARTESIAN_POINT ( 'NONE',  ( 4.597623488365603528, 5.496887170248887067, -1.082531754730548412 ) ) ;
#94882 = ORIENTED_EDGE ( 'NONE', *, *, #80635, .T. ) ;
#94881 = CARTESIAN_POINT ( 'NONE',  ( -0.04078422793344065045, -1.398654746659812043, -1.150989216800960335 ) ) ;
#94883 = CARTESIAN_POINT ( 'NONE',  ( 4.336686996305870068, 2.164023489887345164, 0.4319772483800735086 ) ) ;
#94884 = CARTESIAN_POINT ( 'NONE',  ( 4.856179778084614540, 5.010200168423447842, 0.6077543439236311462 ) ) ;
#94885 = CARTESIAN_POINT ( 'NONE',  ( 3.557846488308267663, 0.5383450771202848983, -2.139971664446515653 ) ) ;
#94886 = CARTESIAN_POINT ( 'NONE',  ( -11.84103413958623818, 12.48995521526850361, 1.443924719788817423 ) ) ;
#94887 = ADVANCED_FACE ( 'NONE', ( #85771 ), #74515, .T. ) ;
#94888 = CARTESIAN_POINT ( 'NONE',  ( 1.260255548581414642, 1.910129771108992625, 0.09294656408432439010 ) ) ;
#94889 = CARTESIAN_POINT ( 'NONE',  ( 9.531545685607134999, 11.07889037375188401, 1.199719254218450271 ) ) ;
#94890 = CARTESIAN_POINT ( 'NONE',  ( 5.828598057497599960, -1.316348130051235410, 1.597988563933512074 ) ) ;
#94892 = CARTESIAN_POINT ( 'NONE',  ( 3.010779355932476253, 1.566693023359872372, -1.489686202715050145 ) ) ;
#94891 = CARTESIAN_POINT ( 'NONE',  ( -1.499999999999972689, 3.879166666666685082, -0.8660254037844548058 ) ) ;
#94893 = CARTESIAN_POINT ( 'NONE',  ( 4.423480980095358284, -1.348712413769267426, -1.727291790683552541 ) ) ;
#94894 = ORIENTED_EDGE ( 'NONE', *, *, #110555, .F. ) ;
#94895 = CYLINDRICAL_SURFACE ( 'NONE', #207657, 1.250000000000000000 ) ;
#94896 = CARTESIAN_POINT ( 'NONE',  ( -0.4800000000000244071, 2.999999999999999112, 2.420000000000000373 ) ) ;
#94897 = CARTESIAN_POINT ( 'NONE',  ( -0.1479172090191771538, 8.281400213891689788, 2.000566733410582110 ) ) ;
#94898 = CARTESIAN_POINT ( 'NONE',  ( 5.574337433874081427, 6.532423756721743580, -1.199719254218452047 ) ) ;
#94899 = CARTESIAN_POINT ( 'NONE',  ( 1.642778471875000035, -3.113541666188709200, -2.845375778867859751 ) ) ;
#94900 = CARTESIAN_POINT ( 'NONE',  ( -4.142898457427624415, 6.991076079377632091, 1.199719254218452935 ) ) ;
#94902 = CARTESIAN_POINT ( 'NONE',  ( 0.5279704824466545654, -1.728000714500482982, 1.038995864524896673 ) ) ;
#94901 = VECTOR ( 'NONE', #7551, 1000.000000000000000 ) ;
#94903 = CARTESIAN_POINT ( 'NONE',  ( -8.270110514656041190, 10.67154823856396817, 1.443375672974090751 ) ) ;
#94904 = CARTESIAN_POINT ( 'NONE',  ( 4.899292406491845497, 6.809203455697518947, -1.599625672291273171 ) ) ;
#94905 = CARTESIAN_POINT ( 'NONE',  ( 5.084861876562203342, 1.979495018489594305, 0.6061691862097525751 ) ) ;
#94906 = CARTESIAN_POINT ( 'NONE',  ( 3.000521647167487593, -0.5595019940488660248, -1.843462078654713343 ) ) ;
#94907 = CARTESIAN_POINT ( 'NONE',  ( 6.503513627744350600, -2.053693679520858684, 0.5143327402655095693 ) ) ;
#94908 = AXIS2_PLACEMENT_3D ( 'NONE', #189690, #172393, #138833 ) ;
#94909 = CARTESIAN_POINT ( 'NONE',  ( 4.286349120214771879, 8.152491073559232859, -0.7998128361456221525 ) ) ;
#94911 = ADVANCED_FACE ( 'NONE', ( #170214 ), #23954, .T. ) ;
#94910 = CARTESIAN_POINT ( 'NONE',  ( 9.453622214572602545, 4.518459228531209959, 7.392429638475896070 ) ) ;
#94912 = CARTESIAN_POINT ( 'NONE',  ( 3.555474331475856786, 1.549626312082365898, 1.215309171139463684 ) ) ;
#94913 = CARTESIAN_POINT ( 'NONE',  ( 0.2522424171345696298, 0.8426718423822797677, 2.023156535103701970 ) ) ;
#94914 = CARTESIAN_POINT ( 'NONE',  ( 4.494645072041675071, -0.4025399330690944133, -1.780595394402582077 ) ) ;
#94915 = EDGE_CURVE ( 'NONE', #182073, #106638, #81037, .T. ) ;
#94916 = CARTESIAN_POINT ( 'NONE',  ( 5.722950238744187956, 9.690876021928001904, 0.7216878364870317197 ) ) ;
#94917 = CARTESIAN_POINT ( 'NONE',  ( 4.080641047588898118, 5.783833860318930320, -1.443375672974051449 ) ) ;
#94918 = CARTESIAN_POINT ( 'NONE',  ( -7.130662446144611977, 7.283804040115648526, 0.000000000000000000 ) ) ;
#94919 = CARTESIAN_POINT ( 'NONE',  ( 3.379725431556547477, 7.165039780116438273, -1.734723475976807094E-15 ) ) ;
#94920 = ORIENTED_EDGE ( 'NONE', *, *, #185104, .F. ) ;
#94922 = CARTESIAN_POINT ( 'NONE',  ( 5.010025764882303001, -0.7205479882510434919, 1.880027049715059073 ) ) ;
#94921 = CARTESIAN_POINT ( 'NONE',  ( 1.206327419354651820, 1.623952629372883427, 0.8676893986077349741 ) ) ;
#94923 = CARTESIAN_POINT ( 'NONE',  ( 0.7382080005397623212, -2.165046367600947708, -0.7717227881791683952 ) ) ;
#94924 = CARTESIAN_POINT ( 'NONE',  ( 5.295737746731337126, -1.384591195607473235, -1.390005841682784959 ) ) ;
#94925 = CARTESIAN_POINT ( 'NONE',  ( -6.880926654135487652, 7.986501503701545879, 1.199719254218450271 ) ) ;
#94926 = CARTESIAN_POINT ( 'NONE',  ( 0.2333690889706682703, 0.003390530909083006028, -2.053566628440507635 ) ) ;
#94927 = CARTESIAN_POINT ( 'NONE',  ( -3.918470089549458635, 4.530302178351167441, -1.199719254218452047 ) ) ;
#94928 = CARTESIAN_POINT ( 'NONE',  ( -7.842350841322885735, -5.412329794880682776, 7.657759090810040803 ) ) ;
#94929 = CARTESIAN_POINT ( 'NONE',  ( -4.098307573080856692, 8.003385611894792362, 0.7998128361456352531 ) ) ;
#94931 = CARTESIAN_POINT ( 'NONE',  ( 6.631742710195931423, -1.160100399838214891, -1.336722620761298330 ) ) ;
#94930 = CARTESIAN_POINT ( 'NONE',  ( 1.769195444908505888, 1.999712852614519143, -0.6101556835421716452 ) ) ;
#94932 = CARTESIAN_POINT ( 'NONE',  ( -0.001026545178582605970, 7.078193277237621928, 2.121339347286388399 ) ) ;
#94933 = CARTESIAN_POINT ( 'NONE',  ( -0.1104750535120268828, 2.006893987364383403, -2.517811492722863864 ) ) ;
#94934 = CARTESIAN_POINT ( 'NONE',  ( 1.399541807966601104, -0.6259456572170263300, -1.624154832779246993 ) ) ;
#94935 = CARTESIAN_POINT ( 'NONE',  ( 5.799137018343234473, 7.788745826199009237, -1.599625672291262513 ) ) ;
#94937 = CARTESIAN_POINT ( 'NONE',  ( 5.517805331081858888, 5.539787095791365523, 1.040834085586084257E-14 ) ) ;
#94936 = CARTESIAN_POINT ( 'NONE',  ( 4.080641032480825103, 5.783833874167997102, -1.249999999999999334 ) ) ;
#94938 = CARTESIAN_POINT ( 'NONE',  ( 1.629113003107704793, -1.625012167801738183, 0.5787621435916143753 ) ) ;
#94939 = CARTESIAN_POINT ( 'NONE',  ( 1.593588134247824639, -0.7342643958434189599, 2.065040727587868830 ) ) ;
#94940 = CARTESIAN_POINT ( 'NONE',  ( 3.879664727460280904, 2.078262106501146622, -0.7427522710690689367 ) ) ;
#94941 = CARTESIAN_POINT ( 'NONE',  ( -11.55090974143167060, 4.033601484819619110, -5.407241547083907918 ) ) ;
#94942 = CARTESIAN_POINT ( 'NONE',  ( 1.376089442288459752, -2.118726187661602367, 0.4732455120740781673 ) ) ;
#94943 = CARTESIAN_POINT ( 'NONE',  ( 1.066719475142905216, -1.649486405746130258, -0.7827983987617056494 ) ) ;
#94944 = CARTESIAN_POINT ( 'NONE',  ( 3.011064194431464003, 0.05668958241028876355, 2.116758953476727267 ) ) ;
#94945 = CARTESIAN_POINT ( 'NONE',  ( 6.539320575229249144, 0.007148032025052972194, 1.896977914940492393 ) ) ;
#94946 = ORIENTED_EDGE ( 'NONE', *, *, #116636, .F. ) ;
#94948 = CARTESIAN_POINT ( 'NONE',  ( -0.6823417656250003738, 0.03020833367475134201, -1.181850606188749264 ) ) ;
#94947 = CARTESIAN_POINT ( 'NONE',  ( 3.544716187562162446, -1.873399702441876480, 1.320855843532109608 ) ) ;
#94949 = CARTESIAN_POINT ( 'NONE',  ( 0.07755575628184004089, 7.629137130509076492, -2.788902932953695846 ) ) ;
#94950 = CARTESIAN_POINT ( 'NONE',  ( 5.027376032568989572, 4.759693547618927489, 0.7998128361456341429 ) ) ;
#94951 = CARTESIAN_POINT ( 'NONE',  ( 6.217462558288930019, 1.845152235743243052, 1.236491063047394201 ) ) ;
#94952 = CARTESIAN_POINT ( 'NONE',  ( -5.260200412422196159, 9.080724881227137502, -0.7216878364870207285 ) ) ;
#94953 = CARTESIAN_POINT ( 'NONE',  ( 4.365362273920244007, 6.116008624372160973, 1.443375672974062551 ) ) ;
#94954 = CARTESIAN_POINT ( 'NONE',  ( -6.493992390821436977, 10.52014885602626393, 0.7216878364870458196 ) ) ;
#94955 = CARTESIAN_POINT ( 'NONE',  ( 3.906157654512984134, 7.571284673658201569, -0.7216878364870338292 ) ) ;
#94956 = VERTEX_POINT ( 'NONE', #43443 ) ;
#94957 = CARTESIAN_POINT ( 'NONE',  ( 3.692029868468839737, 1.730865839653324079, 1.034166058993556181 ) ) ;
#94959 = CARTESIAN_POINT ( 'NONE',  ( 2.008709601793839283, 0.6428708581102732245, 1.959923294053036669 ) ) ;
#94958 = CARTESIAN_POINT ( 'NONE',  ( 5.612185521052973414, 8.634967976948757951, -1.199719254218440723 ) ) ;
#94960 = DIRECTION ( 'NONE',  ( 0.7978120914393141971, 0.6029061840396293670, 0.000000000000000000 ) ) ;
#94961 = CARTESIAN_POINT ( 'NONE',  ( 5.085717018457579286, 6.066329622022862189, -1.082531754730548412 ) ) ;
#94962 = CARTESIAN_POINT ( 'NONE',  ( -3.619663825168619731, 7.166765529431275539, 1.040834085586084257E-14 ) ) ;
#94963 = CARTESIAN_POINT ( 'NONE',  ( -1.201851678989727383E-14, 4.946875000341420581, -1.575800808251660134 ) ) ;
#94964 = CARTESIAN_POINT ( 'NONE',  ( 5.402338782601354694, 1.661146971675907302, -1.429436781345946317 ) ) ;
#94965 = CARTESIAN_POINT ( 'NONE',  ( 1.899064777474347654, -0.9530127170578571727, -1.777010740487514173 ) ) ;
#94966 = CARTESIAN_POINT ( 'NONE',  ( 2.542321706073047416, -1.529623444112483632, 1.024600984555257277 ) ) ;
#94967 = TOROIDAL_SURFACE ( 'NONE', #1520, 0.8299999999999999600, 0.08000000000000000167 ) ;
#94968 = CARTESIAN_POINT ( 'NONE',  ( 6.714312387265682247, 8.856450423275211037, 1.599625672291281386 ) ) ;
#94969 = CARTESIAN_POINT ( 'NONE',  ( 2.281250000000002220, 0.7852924748301068902, 1.895863743164037718 ) ) ;
#94970 = CARTESIAN_POINT ( 'NONE',  ( 5.350558509363329662, 0.5315954154057299652, 1.746479326997903092 ) ) ;
#94971 =( BOUNDED_CURVE ( )  B_SPLINE_CURVE ( 2, ( #97895, #193236, #13412, #181244, #11274, #79487, #163955, #115253, #145606 ),
 .UNSPECIFIED., .F., .T. ) 
 B_SPLINE_CURVE_WITH_KNOTS ( ( 3, 2, 2, 2, 3 ),
 ( 0.7232142857142856984, 0.7261904761904761640, 0.7321428571428570953, 0.7380952380952381375, 0.7410714285714286031 ),
 .UNSPECIFIED. ) 
 CURVE ( )  GEOMETRIC_REPRESENTATION_ITEM ( )  RATIONAL_B_SPLINE_CURVE ( ( 0.9330127018922194093, 0.9330127018922194093, 1.000000000000000000, 0.8660254037844387076, 1.000000000000000000, 0.8660254037844387076, 1.000000000000000000, 0.9330127018922194093, 0.9330127018922194093 ) ) 
 REPRESENTATION_ITEM ( '' )  );
#94972 = CARTESIAN_POINT ( 'NONE',  ( 6.170546107226446253, 1.392543322632183722, 1.458558933167881211 ) ) ;
#94973 = CARTESIAN_POINT ( 'NONE',  ( -6.042130013184518589, 10.20090211535728031, -0.7998128361456291469 ) ) ;
#94975 = CARTESIAN_POINT ( 'NONE',  ( -6.479871072688648148, 6.524547437750345402, 0.000000000000000000 ) ) ;
#94974 = CARTESIAN_POINT ( 'NONE',  ( 5.998944898715565799, 1.853732409352136568, -1.296943227565182877 ) ) ;
#94976 = CARTESIAN_POINT ( 'NONE',  ( 0.2410290108679030985, 0.3623031737408002884, 2.074505700167991407 ) ) ;
#94977 = CARTESIAN_POINT ( 'NONE',  ( -5.725286006720766707, 9.901527117808042178, 0.7998128361456291469 ) ) ;
#94978 = CARTESIAN_POINT ( 'NONE',  ( 8.751951852821344247, 10.16936423550178503, -1.199719254218446718 ) ) ;
#94979 = CARTESIAN_POINT ( 'NONE',  ( -9.578206935409053102, -9.746166700193986898, 0.1671882239534360770 ) ) ;
#94980 = CARTESIAN_POINT ( 'NONE',  ( 8.378074386686847674, 23.21445602483911941, 19.17578233593941661 ) ) ;
#94981 = CARTESIAN_POINT ( 'NONE',  ( -7.690499447449645309, 9.995335326823163058, 1.599625672291295375 ) ) ;
#94982 = UNCERTAINTY_MEASURE_WITH_UNIT (LENGTH_MEASURE( 1.000000000000000082E-05 ), #159440, 'distance_accuracy_value', 'NONE');
#94983 = CARTESIAN_POINT ( 'NONE',  ( 7.580882385732059525, -6.105993949506566487, 7.580882385732033768 ) ) ;
#94984 = CARTESIAN_POINT ( 'NONE',  ( 7.632877294369377452, 8.967740267261513409, -1.082531754730537976 ) ) ;
#94985 = CARTESIAN_POINT ( 'NONE',  ( 4.118656133465138147, 7.671478758617087834, -0.7332979114653701558 ) ) ;
#94986 = CARTESIAN_POINT ( 'NONE',  ( -8.026063749610043985, 12.30756544127966912, -0.7216878364870267237 ) ) ;
#94988 = CARTESIAN_POINT ( 'NONE',  ( 2.408681662258719047, -2.215777464676274011, -0.1586666079704464882 ) ) ;
#94987 = CARTESIAN_POINT ( 'NONE',  ( 1.389100911873580646, -2.015333191458138273, -0.6601287711371638389 ) ) ;
#94989 = CARTESIAN_POINT ( 'NONE',  ( 0.000000000000000000, 9.719999999999998863, 0.000000000000000000 ) ) ;
#94990 = CARTESIAN_POINT ( 'NONE',  ( -6.017840079619296567, 8.114175741012878973, -1.599625672291271394 ) ) ;
#94991 = CARTESIAN_POINT ( 'NONE',  ( 7.122110765880372618, 7.203550736482235095, 0.7998128361456341429 ) ) ;
#94992 = CARTESIAN_POINT ( 'NONE',  ( 3.859774877264535053, -0.5717695562157121270, 1.876676618968641019 ) ) ;
#94993 = CARTESIAN_POINT ( 'NONE',  ( 9.738834413317897898, 10.25639499182604730, 0.000000000000000000 ) ) ;
#94994 = CARTESIAN_POINT ( 'NONE',  ( -4.471757287801709779, 7.078374187635557924, 1.125421738336473299 ) ) ;
#94995 = CARTESIAN_POINT ( 'NONE',  ( 4.090809663021327758, 5.795697244990093644, 1.599625672291267398 ) ) ;
#94996 = CARTESIAN_POINT ( 'NONE',  ( -4.502716413514310290, 6.346531463890372926, -1.443375672974066548 ) ) ;
#94998 = ORIENTED_EDGE ( 'NONE', *, *, #90295, .F. ) ;
#94997 = CARTESIAN_POINT ( 'NONE',  ( -7.375272376154101472, 7.706831981708990753, -0.7216878364870278340 ) ) ;
#94999 = CARTESIAN_POINT ( 'NONE',  ( 2.549219474610735947, 0.2639673528169217964, 2.104066465523121376 ) ) ;
#95000 = CARTESIAN_POINT ( 'NONE',  ( -6.310394152517827315, 6.326824364217716656, 0.7998128361456281477 ) ) ;
#95001 = CARTESIAN_POINT ( 'NONE',  ( 4.065412822539622439, 0.2671453805177248508, -2.145074402785766665 ) ) ;
#95002 = CARTESIAN_POINT ( 'NONE',  ( 3.755264181858388284, 1.826884192416846853, -0.2291247506851084581 ) ) ;
#95003 = CARTESIAN_POINT ( 'NONE',  ( -4.868194452378435955, 6.719997196398590056, 1.250117667640719077 ) ) ;
#95004 = CARTESIAN_POINT ( 'NONE',  ( -1.364683531250014514, 0.5510416670080878765, -0.7879004041258289570 ) ) ;
#95005 = CARTESIAN_POINT ( 'NONE',  ( 5.824081541776103599, 1.678935111502709354, 0.4578980800337121848 ) ) ;
#95006 = DIRECTION ( 'NONE',  ( -2.126226658603517140E-31, 1.665334536937738015E-16, 1.000000000000000000 ) ) ;
#95007 = CARTESIAN_POINT ( 'NONE',  ( 3.226477370372293763, 6.708047998835573900, 0.7216878364870317197 ) ) ;
#95008 = CARTESIAN_POINT ( 'NONE',  ( -1.201851678989727383E-14, 3.618750000682816381, -1.732050807568863648 ) ) ;
#95009 = CARTESIAN_POINT ( 'NONE',  ( 3.485389320157119997, 1.955090977548096687, -0.9225387301767663528 ) ) ;
#95010 = CARTESIAN_POINT ( 'NONE',  ( 5.764999918528635803, -2.016288307888712161, -0.002809016773450134351 ) ) ;
#95011 = CARTESIAN_POINT ( 'NONE',  ( -9.937763408692600109, 10.69640485300394417, -0.7216878364870267237 ) ) ;
#95012 = CARTESIAN_POINT ( 'NONE',  ( 2.202237438260604030, -2.161223104231101644, 0.05255616829508147347 ) ) ;
#95013 = CARTESIAN_POINT ( 'NONE',  ( 3.620352162249322880, 1.253078330817010588, -1.521826374184510389 ) ) ;
#95014 = CARTESIAN_POINT ( 'NONE',  ( -0.09381621004311831158, -0.9424329983100244723, -1.976553698157037076 ) ) ;
#95015 = CARTESIAN_POINT ( 'NONE',  ( 4.581548892214976298, -0.9124856661332171326, 1.714327114426909882 ) ) ;
#95018 = ORIENTED_EDGE ( 'NONE', *, *, #77726, .F. ) ;
#95017 = CARTESIAN_POINT ( 'NONE',  ( 7.978162878861384755, -5.230039540835521805, -7.573156686838170337 ) ) ;
#95016 = CARTESIAN_POINT ( 'NONE',  ( -9.612367721964622191, 10.31677655182129527, -0.7216878364870267237 ) ) ;
#95019 = CARTESIAN_POINT ( 'NONE',  ( -7.306918443122272677, 7.489436036589583345, 0.7998128361456341429 ) ) ;
#95020 = CARTESIAN_POINT ( 'NONE',  ( -11.86239285000045918, 12.21999999999998288, 1.812080536912751061 ) ) ;
#95022 = ORIENTED_EDGE ( 'NONE', *, *, #25859, .F. ) ;
#95021 = CARTESIAN_POINT ( 'NONE',  ( -4.492547798081878874, 6.334668079219206049, 1.599625672291263179 ) ) ;
#95023 = CARTESIAN_POINT ( 'NONE',  ( -8.229436053370685400, 10.62409470039771442, 1.443375672974090751 ) ) ;
#95024 = CARTESIAN_POINT ( 'NONE',  ( 0.8157880970438775581, -0.3219574891645953785, 2.183050487710703536 ) ) ;
#95025 = CARTESIAN_POINT ( 'NONE',  ( 3.285556943749998737, -2.005208332855377140, -1.896917185911906500 ) ) ;
#95026 = CARTESIAN_POINT ( 'NONE',  ( 6.368018226480639754, -1.947316962026977682, 0.2367824842242904348 ) ) ;
#95027 = CARTESIAN_POINT ( 'NONE',  ( 1.364683531249990311, 5.176041667008085767, 0.7879004041258500513 ) ) ;
#95028 = CARTESIAN_POINT ( 'NONE',  ( -1.201851678989727383E-14, 3.618750000682816381, -1.732050807568863648 ) ) ;
#95029 = CARTESIAN_POINT ( 'NONE',  ( 5.634486230560368902, 6.328851001874927107, -1.145628596103397623 ) ) ;
#95030 = CARTESIAN_POINT ( 'NONE',  ( 0.07479286986303290696, 5.725009232006174287, -2.449550298930736059 ) ) ;
#95031 = CARTESIAN_POINT ( 'NONE',  ( 5.331922971087851515, 1.814509544241477146, 0.3110680438872318043 ) ) ;
#95032 = ORIENTED_EDGE ( 'NONE', *, *, #128454, .T. ) ;
#95033 = CARTESIAN_POINT ( 'NONE',  ( -1.352083138863443345E-14, -0.9218749996585863249, -1.570758158831792262 ) ) ;
#95034 = CARTESIAN_POINT ( 'NONE',  ( -7.049349804101573191, 10.31165964050546258, -1.199719254218440723 ) ) ;
#95035 = CARTESIAN_POINT ( 'NONE',  ( 7.253242555595320162, -7.896420114628004860, -6.595517585942703320 ) ) ;
#95036 = CARTESIAN_POINT ( 'NONE',  ( 6.486587849989844834, -1.303813291173651301, 1.673118453357678392 ) ) ;
#95037 = CARTESIAN_POINT ( 'NONE',  ( 9.969705528599281052, 9.873875388196676539, 6.618200077599721176 ) ) ;
#95038 = CARTESIAN_POINT ( 'NONE',  ( 4.202137545231717120, 6.989912005157271402, 1.199719254218462483 ) ) ;
#95039 = EDGE_CURVE ( 'NONE', #22324, #3985, #98791, .T. ) ;
#95040 = CARTESIAN_POINT ( 'NONE',  ( 6.362583954249420692, -1.460576210990358614, 1.454072064785590479 ) ) ;
#95043 = CARTESIAN_POINT ( 'NONE',  ( 3.597050949361340511, -0.5310884314010614338, 1.763007376093472800 ) ) ;
#95042 = CARTESIAN_POINT ( 'NONE',  ( 1.697469458906812667, -1.344883679737416404, -1.286638954052413908 ) ) ;
#95041 = CYLINDRICAL_SURFACE ( 'NONE', #111199, 0.3999999999999997446 ) ;
#95044 = CARTESIAN_POINT ( 'NONE',  ( 6.421758314367153275, 10.64380180007036891, -0.7998128361456291469 ) ) ;
#95045 = FACE_OUTER_BOUND ( 'NONE', #42591, .T. ) ;
#95046 = CARTESIAN_POINT ( 'NONE',  ( -5.769876891067536206, 8.889217585290882795, 1.199719254218454489 ) ) ;
#95048 = EDGE_LOOP ( 'NONE', ( #209268, #99788, #57330, #107558, #77283, #68687, #38603 ) ) ;
#95047 = CARTESIAN_POINT ( 'NONE',  ( 0.4382560683119269829, -7.666862915010147717, -10.99126615174920296 ) ) ;
#95049 = CARTESIAN_POINT ( 'NONE',  ( 3.387540773601561916, 1.995160029947869340, -0.9435142334218297178 ) ) ;
#95050 = CARTESIAN_POINT ( 'NONE',  ( 5.624405936800197736, 1.354097840178031475, -1.812292894430814094 ) ) ;
#95051 = CARTESIAN_POINT ( 'NONE',  ( -6.236387472606153892, 8.298871356172400127, -1.443375672974059665 ) ) ;
#95052 = CARTESIAN_POINT ( 'NONE',  ( 5.748286673958676651, 0.8850744635948673000, -1.580567631948928797 ) ) ;
#95053 = CARTESIAN_POINT ( 'NONE',  ( 6.104688764726555306, 1.790162971792093272, 0.6826718079199489697 ) ) ;
#95054 = EDGE_CURVE ( 'NONE', #119587, #150638, #34621, .T. ) ;
#95055 = CARTESIAN_POINT ( 'NONE',  ( 3.921423297084294823, 8.995353878514519508, 0.7749999999999996891 ) ) ;
#95056 = CARTESIAN_POINT ( 'NONE',  ( 6.543822781336226413, 0.7137633992815132222, -1.729328153040734506 ) ) ;
#95057 = EDGE_CURVE ( 'NONE', #17507, #193127, #126547, .T. ) ;
#95058 = CARTESIAN_POINT ( 'NONE',  ( 5.531871257421491883, -1.864710570029969317, 0.4231498525801706823 ) ) ;
#95059 = CARTESIAN_POINT ( 'NONE',  ( 1.387358672525639269, 7.251968950354889643, 4.302625267139791987 ) ) ;
#95060 = AXIS2_PLACEMENT_3D ( 'NONE', #75981, #93325, #24013 ) ;
#95061 = CARTESIAN_POINT ( 'NONE',  ( 1.147088892781012781, -1.472398045354219365, -1.153743250124287689 ) ) ;
#95062 = CARTESIAN_POINT ( 'NONE',  ( 1.762908039156896978, -0.1037823317905466058, -2.014007988105172231 ) ) ;
#95064 = CARTESIAN_POINT ( 'NONE',  ( 3.071027892464781583, -1.946086441943569723, -0.8056474276203289264 ) ) ;
#95063 = CARTESIAN_POINT ( 'NONE',  ( -9.287498920561160887, 10.79416914786490089, -1.199719254218441611 ) ) ;
#95065 = CIRCLE ( 'NONE', #109022, 0.08000000000000020983 ) ;
#95066 = CARTESIAN_POINT ( 'NONE',  ( 7.425061681778431399, 11.81432239538354345, 0.7998128361456462443 ) ) ;
#95068 = CARTESIAN_POINT ( 'NONE',  ( -9.664264568442742842, 10.16939683947169115, -0.7998128361456291469 ) ) ;
#95067 = CARTESIAN_POINT ( 'NONE',  ( -1.500000000000015099, -0.8708333333333129200, -0.8660254037844383745 ) ) ;
#95069 = CARTESIAN_POINT ( 'NONE',  ( -11.84668730067608600, 10.89999999999998259, 1.399999999999998579 ) ) ;
#95070 = CARTESIAN_POINT ( 'NONE',  ( 2.672133692126318127, 2.009681031688851593, -0.2020390005853574256 ) ) ;
#95071 = CARTESIAN_POINT ( 'NONE',  ( 1.364683531249990311, 2.884375000341422801, 1.214306433183764966E-14 ) ) ;
#95072 = CARTESIAN_POINT ( 'NONE',  ( 4.681643115420508039, 4.356338477612361260, 0.7998128361456341429 ) ) ;
#95073 = CARTESIAN_POINT ( 'NONE',  ( 3.251412196806032995, -1.765091617811213931, -1.247493029685270649 ) ) ;
#95074 = CARTESIAN_POINT ( 'NONE',  ( 6.502017186205484300, 9.743381262951846367, -1.199719254218452047 ) ) ;
#95075 = CARTESIAN_POINT ( 'NONE',  ( 0.7499999999999920064, 4.983333333333353821, 1.299038105676669330 ) ) ;
#95077 = CARTESIAN_POINT ( 'NONE',  ( -2.482948226198895103, 5.072301959192136778, 2.420000000000010587 ) ) ;
#95076 = CARTESIAN_POINT ( 'NONE',  ( 7.289443866002793371, 8.533381260871966134, 1.199719254218452047 ) ) ;
#95078 = CARTESIAN_POINT ( 'NONE',  ( 8.392133896734668141, 9.853539636687704828, 1.082531754730558626 ) ) ;
#95080 = CARTESIAN_POINT ( 'NONE',  ( 9.105083262974959624, 14.28913828790224194, -7.747438832664901298 ) ) ;
#95079 = CARTESIAN_POINT ( 'NONE',  ( 0.3621003815536598669, -0.5783089063249653439, 2.092656953901766315 ) ) ;
#95081 = VECTOR ( 'NONE', #149504, 1000.000000000000000 ) ;
#95082 = CARTESIAN_POINT ( 'NONE',  ( -5.083944415444539899, 8.875092884753202682, 0.000000000000000000 ) ) ;
#95083 = CARTESIAN_POINT ( 'NONE',  ( 1.364683531249986537, 1.155208333674754728, -0.7879004041258239610 ) ) ;
#95084 = CARTESIAN_POINT ( 'NONE',  ( 2.366952063387484095, 0.1042156695447923470, -2.189191704635709890 ) ) ;
#95085 = CARTESIAN_POINT ( 'NONE',  ( 6.983263157960366563, 3.694515354052980260, 2.467960814016751936 ) ) ;
#95086 = CARTESIAN_POINT ( 'NONE',  ( 2.290224401178039049, -0.9674489778378884131, 2.045383877150886320 ) ) ;
#95087 = CARTESIAN_POINT ( 'NONE',  ( -8.193204901359996128, 8.453160561208463264, 1.040834085586084257E-14 ) ) ;
#95088 = CARTESIAN_POINT ( 'NONE',  ( -4.731432421044888592, 4.622352034081546712, -0.7216878364870207285 ) ) ;
#95089 = CARTESIAN_POINT ( 'NONE',  ( -1.201851678989727383E-14, 4.759375000341419693, -1.575800808251660134 ) ) ;
#95090 = CARTESIAN_POINT ( 'NONE',  ( 5.960708871395055120, 7.108654626955757116, 1.090683939682752124 ) ) ;
#95091 = CARTESIAN_POINT ( 'NONE',  ( -0.7500000000000006661, 11.70833333333333393, -1.299038105676657340 ) ) ;
#95092 = CARTESIAN_POINT ( 'NONE',  ( 6.875393295905841917, 7.193916064744513506, 0.000000000000000000 ) ) ;
#95093 = CARTESIAN_POINT ( 'NONE',  ( 4.042088942692352305, 1.761052656288846663, 0.1752445044498444349 ) ) ;
#95094 = CARTESIAN_POINT ( 'NONE',  ( 10.08456733046637765, 10.65975006183261087, 0.000000000000000000 ) ) ;
#95096 = AXIS2_PLACEMENT_3D ( 'NONE', #201079, #184836, #205363 ) ;
#95095 = CARTESIAN_POINT ( 'NONE',  ( 0.3586045525620683017, 0.8063113102214304329, 1.945692106844071789 ) ) ;
#95097 = CARTESIAN_POINT ( 'NONE',  ( 0.6823417656249969321, 9.276041667008065872, -1.181850606188757036 ) ) ;
#95098 = CARTESIAN_POINT ( 'NONE',  ( -5.123001941117347080, 7.070197912760590064, 1.599625672291263179 ) ) ;
#95099 = CARTESIAN_POINT ( 'NONE',  ( 6.485953897545715385, -2.015913262743720402, 0.05231248585663844652 ) ) ;
#95100 = VERTEX_POINT ( 'NONE', #125044 ) ;
#95101 = CARTESIAN_POINT ( 'NONE',  ( 8.238550898598388628, 12.76339314834017102, 0.7998128361456462443 ) ) ;
#95102 = CARTESIAN_POINT ( 'NONE',  ( 3.133525119713890472, -1.255248497922526463, -1.387151338369890574 ) ) ;
#95103 = CARTESIAN_POINT ( 'NONE',  ( 3.291909242638372923, -1.386922682245657734, -1.537212927083357217 ) ) ;
#95104 = CARTESIAN_POINT ( 'NONE',  ( -5.926322542504872892, 8.007405281046052536, -1.443375672974066548 ) ) ;
#95105 = DIRECTION ( 'NONE',  ( 0.000000000000000000, 0.000000000000000000, 1.000000000000000000 ) ) ;
#95106 = CARTESIAN_POINT ( 'NONE',  ( 7.618792255875527886, 10.97600916757510170, 1.199719254218460707 ) ) ;
#95107 = CARTESIAN_POINT ( 'NONE',  ( -1.550536438491968427, 8.693843051952859113, 2.505472492508749038 ) ) ;
#95108 = CARTESIAN_POINT ( 'NONE',  ( 6.614160618316515361, -1.014195557614630427, -1.909021090911746876 ) ) ;
#95109 = CARTESIAN_POINT ( 'NONE',  ( -0.6823417656249969321, 5.530208333674756283, -1.181850606188749264 ) ) ;
#95110 = AXIS2_PLACEMENT_3D ( 'NONE', #172149, #155896, #7484 ) ;
#95111 = CARTESIAN_POINT ( 'NONE',  ( 2.892962425504439050, 0.2373818416543191367, 1.947367909387688112 ) ) ;
#95112 = CARTESIAN_POINT ( 'NONE',  ( 1.018907413236518789, 2.013924516646655949, -0.09611688112247382398 ) ) ;
#95113 = ADVANCED_FACE ( 'NONE', ( #176911 ), #180780, .T. ) ;
#95114 = CARTESIAN_POINT ( 'NONE',  ( -3.984117037569407938, 5.741498858621315371, 1.599625672291270506 ) ) ;
#95116 = CARTESIAN_POINT ( 'NONE',  ( -11.48243876534946217, 12.29999999999998295, 3.199999999999997957 ) ) ;
#95115 = CARTESIAN_POINT ( 'NONE',  ( 6.936968151686458306, 11.24487994360957188, 0.7998128361456462443 ) ) ;
#95117 = CARTESIAN_POINT ( 'NONE',  ( 1.071320448993583918, 1.804315561281001123, -0.4931735697189034151 ) ) ;
#95118 = CARTESIAN_POINT ( 'NONE',  ( 1.364683531249988535, 3.863541667008087543, 0.7879004041258500513 ) ) ;
#95119 = CARTESIAN_POINT ( 'NONE',  ( 3.410405542056849981, -2.011076457950426555, -0.09466423678533388009 ) ) ;
#95121 = CARTESIAN_POINT ( 'NONE',  ( 1.810321443220731075, 1.215999664948445913, -1.733040945678490319 ) ) ;
#95120 = CARTESIAN_POINT ( 'NONE',  ( -6.575341312947811545, 6.773579074634973551, 1.040834085586084257E-14 ) ) ;
#95122 = FACE_OUTER_BOUND ( 'NONE', #26784, .T. ) ;
#95123 = CARTESIAN_POINT ( 'NONE',  ( 4.053231837324381637, 1.750648263899981849, -1.104974720517466480 ) ) ;
#95124 = CARTESIAN_POINT ( 'NONE',  ( 7.075376061485196821, 9.347967719856493218, 1.599625672291268286 ) ) ;
#95126 = CARTESIAN_POINT ( 'NONE',  ( 3.541704441667858472, 5.155074486744371853, -1.599625672291262513 ) ) ;
#95125 = CARTESIAN_POINT ( 'NONE',  ( 0.02900754732045561154, -1.909850462538491778, 0.8511534736125156986 ) ) ;
#95128 = VERTEX_POINT ( 'NONE', #205710 ) ;
#95127 = CARTESIAN_POINT ( 'NONE',  ( 5.209893869493905427, -1.816617279468687229, 0.1804919988709560719 ) ) ;
#95129 = CARTESIAN_POINT ( 'NONE',  ( 9.562578416340237197, 10.05076299535211781, 0.7998128361456462443 ) ) ;
#95130 = CARTESIAN_POINT ( 'NONE',  ( 5.736990052193561063, 5.898621588832019036, -2.499999999999135802 ) ) ;
#95131 = CARTESIAN_POINT ( 'NONE',  ( 11.09909601403977852, 9.551700265434966752, 4.072285437489899351 ) ) ;
#95132 = CARTESIAN_POINT ( 'NONE',  ( 6.528370574810466564, 1.275976099532463603, -1.800301716031265764 ) ) ;
#95133 = CARTESIAN_POINT ( 'NONE',  ( 0.6823417656249934904, 12.50520833367473017, 1.181850606188764807 ) ) ;
#95134 = CARTESIAN_POINT ( 'NONE',  ( 4.565046243057500952, -1.533749416048999947, 1.141898535029245432 ) ) ;
#95135 = CARTESIAN_POINT ( 'NONE',  ( -9.541187415715041809, 12.15447128979948310, -1.599625672291263179 ) ) ;
#95136 = CARTESIAN_POINT ( 'NONE',  ( 5.982172092127724383, 8.002286745614243912, -1.599625672291262513 ) ) ;
#95137 = FACE_OUTER_BOUND ( 'NONE', #20784, .T. ) ;
#95138 = CARTESIAN_POINT ( 'NONE',  ( 9.499262961676938843, -8.008893676011952678, -0.1288460037566319938 ) ) ;
#95139 = CARTESIAN_POINT ( 'NONE',  ( 3.147464216666835402, 6.823792019419957278, -0.7998128361456291469 ) ) ;
#95140 = ORIENTED_EDGE ( 'NONE', *, *, #11493, .F. ) ;
#95141 = CARTESIAN_POINT ( 'NONE',  ( -6.994027139803241866, 9.253060644560830994, -1.599625672291271394 ) ) ;
#95142 = CARTESIAN_POINT ( 'NONE',  ( 4.938664768831324992, 0.3182328507864222722, 1.843102042236575366 ) ) ;
#95143 = CARTESIAN_POINT ( 'NONE',  ( -0.02319159430949797526, 7.629137130509074716, -2.410989586153565067 ) ) ;
#95144 = CARTESIAN_POINT ( 'NONE',  ( 7.530627977747744062, 7.750430493652658015, -0.7998128361456341429 ) ) ;
#95145 = CARTESIAN_POINT ( 'NONE',  ( 7.013428937081407355, 5.939655416065874327, -2.436399677959149468 ) ) ;
#95146 = CARTESIAN_POINT ( 'NONE',  ( -6.041007162748570636, 7.066593642038220935, 1.036256717389577586 ) ) ;
#95147 = CARTESIAN_POINT ( 'NONE',  ( -6.724481002698130538, 7.907944593645035880, -1.082531754730544860 ) ) ;
#95148 = CARTESIAN_POINT ( 'NONE',  ( 3.714044015139744914, 6.420469553383295391, 1.199719254218462483 ) ) ;
#95149 = CARTESIAN_POINT ( 'NONE',  ( 0.9890311015656474414, 0.1392606914251882932, 1.964554613873798594 ) ) ;
#95150 = CARTESIAN_POINT ( 'NONE',  ( 3.040638836679772528, -1.525031945187466098, 1.319243992433154267 ) ) ;
#95151 = CARTESIAN_POINT ( 'NONE',  ( -7.344766530301162000, 9.591980256816594164, 1.599625672291295375 ) ) ;
#95152 = CARTESIAN_POINT ( 'NONE',  ( 5.879395890181562834, 6.888325289080478697, -1.199719254218452047 ) ) ;
#95154 = EDGE_CURVE ( 'NONE', #197280, #40132, #89867, .T. ) ;
#95153 = CARTESIAN_POINT ( 'NONE',  ( 6.727182134110167411, 4.685720203848058318, 2.851561905840187983 ) ) ;
#95155 = CARTESIAN_POINT ( 'NONE',  ( 3.310656966840678894, 1.981231107410564851, 0.9368519390955745152 ) ) ;
#95156 = CARTESIAN_POINT ( 'NONE',  ( -5.579056995618064008, 5.838737027418012815, -0.5808829061496860735 ) ) ;
#95157 = CARTESIAN_POINT ( 'NONE',  ( 2.485270279442112429, 1.762041721199611333, -0.7789696210150058864 ) ) ;
#95158 = CARTESIAN_POINT ( 'NONE',  ( -10.62011439820619429, 11.28455497419572318, -0.7998128361456221525 ) ) ;
#95159 = CARTESIAN_POINT ( 'NONE',  ( -0.1296875068448125057, 0.2507808023153486054, -1.861542470327881560 ) ) ;
#95160 = CARTESIAN_POINT ( 'NONE',  ( 0.1331565106231606399, 5.723858289613107608, -2.539976893513963052 ) ) ;
#95161 = EDGE_CURVE ( 'NONE', #27525, #109221, #38432, .T. ) ;
#95162 = CARTESIAN_POINT ( 'NONE',  ( 2.957086901556340575, 6.464035461875470290, 0.7216878364870257245 ) ) ;
#95163 = CARTESIAN_POINT ( 'NONE',  ( 7.446452682403650769, 9.710614100936176385, -1.599625672291262513 ) ) ;
#95164 = CARTESIAN_POINT ( 'NONE',  ( 5.799137018343234473, 7.788745826199009237, -1.599625672291262513 ) ) ;
#95165 = CARTESIAN_POINT ( 'NONE',  ( -2.487170525094521079, 8.243531156566744400, -2.499999999999995559 ) ) ;
#95166 = CARTESIAN_POINT ( 'NONE',  ( 5.722950238744209273, 6.809768379023969587, 1.082531754730549967 ) ) ;
#95167 = VERTEX_POINT ( 'NONE', #28041 ) ;
#95169 = CARTESIAN_POINT ( 'NONE',  ( 2.192043262494451916, 1.240095455230303401, 1.585687145212981042 ) ) ;
#95168 = CARTESIAN_POINT ( 'NONE',  ( 4.563899478665734755, -1.199029595066217313, 1.397436126395680267 ) ) ;
#95170 = CARTESIAN_POINT ( 'NONE',  ( 4.323764262282871584, -1.706850429308865547, 1.539420282360188574 ) ) ;
#95172 = CARTESIAN_POINT ( 'NONE',  ( 2.008444763995967275, 0.5780311502073384178, 1.769000597778628947 ) ) ;
#95171 = CARTESIAN_POINT ( 'NONE',  ( -0.02880301295726198432, 2.855735178999906587, -2.761736421759506399 ) ) ;
#95173 = CARTESIAN_POINT ( 'NONE',  ( 1.001543065824772753E-15, -2.471874999522041705, 3.793834371823811669 ) ) ;
#95174 = CARTESIAN_POINT ( 'NONE',  ( -8.014278199453791274, 8.522615118883788199, 1.530808498934192557E-16 ) ) ;
#95175 = CARTESIAN_POINT ( 'NONE',  ( 5.590081826628392925, 1.144292256163012667, 1.532101299821154949 ) ) ;
#95176 = CARTESIAN_POINT ( 'NONE',  ( -8.290974629956718189, 9.631557475493025322, -1.199719254218446718 ) ) ;
#95177 = CARTESIAN_POINT ( 'NONE',  ( -5.641601317062247212, 7.675230518029648508, -1.443375672974066548 ) ) ;
#95179 = CARTESIAN_POINT ( 'NONE',  ( 3.010468980803046257, 1.356049738124785353, -1.288842618233053683 ) ) ;
#95178 = CARTESIAN_POINT ( 'NONE',  ( 4.423432795095141756, -1.287707899167778169, -1.647015592753127589 ) ) ;
#95180 = CARTESIAN_POINT ( 'NONE',  ( 6.724481002698112775, 8.868313807946373473, -1.443375672974057666 ) ) ;
#95181 = DIRECTION ( 'NONE',  ( 0.000000000000000000, -1.000000000000000000, 0.000000000000000000 ) ) ;
#95182 = CARTESIAN_POINT ( 'NONE',  ( 4.161989969715261140, 4.726297878971393196, -7.499999999999991118 ) ) ;
#95183 = CARTESIAN_POINT ( 'NONE',  ( 4.898908426394765314, 1.431408964483871227, -0.9620984105884394788 ) ) ;
#95184 = CARTESIAN_POINT ( 'NONE',  ( -6.063521013809733518, 8.097193820909906137, 1.599625672291283607 ) ) ;
#95185 = CARTESIAN_POINT ( 'NONE',  ( 0.7735316488602840268, 1.530413877909537979, -0.8155550471512038602 ) ) ;
#95186 = FACE_OUTER_BOUND ( 'NONE', #203216, .T. ) ;
#95187 = SURFACE_STYLE_FILL_AREA ( #128809 ) ;
#95188 = CARTESIAN_POINT ( 'NONE',  ( 5.594640809421455252, 2.137687854117083841, 0.3785394800270032167 ) ) ;
#95189 = CARTESIAN_POINT ( 'NONE',  ( 4.811078068098579408, 1.589968679568127596, 0.8971634079883783475 ) ) ;
#95190 = CARTESIAN_POINT ( 'NONE',  ( 2.430452978529148655, -1.210835280720125917, 1.543375930141199115 ) ) ;
#95191 = CARTESIAN_POINT ( 'NONE',  ( -0.01776408051935850912, -2.116861762172245420, -0.04693027993646693707 ) ) ;
#95192 = CARTESIAN_POINT ( 'NONE',  ( 9.527745260137857386, 12.67567440174593152, -7.221966599662466457 ) ) ;
#95193 = CARTESIAN_POINT ( 'NONE',  ( 3.733524485140252480, 7.410126666105652404, 2.500000000000107025 ) ) ;
#95194 = CARTESIAN_POINT ( 'NONE',  ( 7.670162217029129259, 9.971608557999250166, 1.599625672291281386 ) ) ;
#95195 = CARTESIAN_POINT ( 'NONE',  ( 2.262495435604610527, 2.120074037919957632, 0.04929290001921824566 ) ) ;
#95196 = CARTESIAN_POINT ( 'NONE',  ( -4.175548123328963079, 4.934189567714277302, 1.082531754730560403 ) ) ;
#95197 = CONICAL_SURFACE ( 'NONE', #57152, 11.49999999999998934, 0.7853981633974396193 ) ;
#95198 = CARTESIAN_POINT ( 'NONE',  ( 4.098537063712264228, 7.253343185014818673, 1.055677455976588686 ) ) ;
#95199 = EDGE_CURVE ( 'NONE', #80954, #40283, #124565, .T. ) ;
#95200 = CARTESIAN_POINT ( 'NONE',  ( -5.513283157632952403, 6.248865724650796594, -0.9728955443181900309 ) ) ;
#95201 = CARTESIAN_POINT ( 'NONE',  ( 1.094682738308445202, 2.038987083759949304, 0.3576228084290478115 ) ) ;
#95203 = CARTESIAN_POINT ( 'NONE',  ( 1.499999999999993117, 14.38541666734946389, 0.8660254037844409281 ) ) ;
#95202 = FACE_OUTER_BOUND ( 'NONE', #3427, .T. ) ;
#95206 = ORIENTED_EDGE ( 'NONE', *, *, #50038, .T. ) ;
#95205 = CARTESIAN_POINT ( 'NONE',  ( 2.403257875557132994, -0.3827610287685556112, -2.187935401104672994 ) ) ;
#95204 = AXIS2_PLACEMENT_3D ( 'NONE', #55484, #205987, #24032 ) ;
#95207 = CARTESIAN_POINT ( 'NONE',  ( 0.2648075084464130979, 2.141788565065712913, -0.8351287359565621182 ) ) ;
#95209 = CARTESIAN_POINT ( 'NONE',  ( 5.366109125895877519, -2.053123361074739250, 0.1969011160823062045 ) ) ;
#95208 = CARTESIAN_POINT ( 'NONE',  ( 2.333974999846879061, 5.874721266463329705, -0.7998128361456291469 ) ) ;
#95211 = CARTESIAN_POINT ( 'NONE',  ( -3.474999999999998312, -2.770833333333333037, 2.006292185433951047 ) ) ;
#95210 = CARTESIAN_POINT ( 'NONE',  ( 6.364626766972446781, 6.390095747748157251, 0.7998128361456352531 ) ) ;
#95212 = CARTESIAN_POINT ( 'NONE',  ( 4.850785098639300408, 8.881276058379668825, -0.7998128361456481317 ) ) ;
#95213 = CARTESIAN_POINT ( 'NONE',  ( 0.1331565106231571705, 6.948071080078889850, -2.540993614958915181 ) ) ;
#95214 = CARTESIAN_POINT ( 'NONE',  ( 5.020983453748395497, -1.746657797055195305, 0.5827527221545365510 ) ) ;
#95215 = CARTESIAN_POINT ( 'NONE',  ( 4.715538499454675403, 4.395883092318884522, 1.214306433183764966E-14 ) ) ;
#95216 = CARTESIAN_POINT ( 'NONE',  ( 0.000000000000000000, 0.000000000000000000, 0.000000000000000000 ) ) ;
#95217 = CARTESIAN_POINT ( 'NONE',  ( 3.416762500535154068, 1.558979225792535006, 0.7381585831351898941 ) ) ;
#95218 = CARTESIAN_POINT ( 'NONE',  ( 1.428923106112218067, -1.700960256238340573, 1.082842518468102089 ) ) ;
#95219 = CARTESIAN_POINT ( 'NONE',  ( 3.217717873326145117, 2.243214920517083044, 0.5014430322199947554 ) ) ;
#95220 = CARTESIAN_POINT ( 'NONE',  ( -1.364683531250010295, 4.092708333674751842, 0.7879004041258379498 ) ) ;
#95221 = CARTESIAN_POINT ( 'NONE',  ( 2.548426268707996822, 2.261836392764454473, 0.05785012348054861114 ) ) ;
#95222 = CARTESIAN_POINT ( 'NONE',  ( 3.668672709498523865, -1.414518211590541252, 1.560516469030509334 ) ) ;
#95223 = CARTESIAN_POINT ( 'NONE',  ( -7.770231434407805615, 8.237893892996801526, 0.000000000000000000 ) ) ;
#95224 = CARTESIAN_POINT ( 'NONE',  ( 3.690472162876729190, -0.3426837954879756731, -1.736044821310823938 ) ) ;
#95225 = CARTESIAN_POINT ( 'NONE',  ( 4.625302960556422427, 8.547937220624488575, 1.040834085586084257E-14 ) ) ;
#95227 = CARTESIAN_POINT ( 'NONE',  ( 6.058190142838977721, -1.623990863767441617, 1.618158029567408729 ) ) ;
#95226 = CARTESIAN_POINT ( 'NONE',  ( 3.973948422136968084, 5.729635473950147606, -1.443375672974068769 ) ) ;
#95228 = CARTESIAN_POINT ( 'NONE',  ( 5.015489797737916255, -0.9877249803392706973, -1.553577481828890106 ) ) ;
#95229 = CARTESIAN_POINT ( 'NONE',  ( -5.447678794592645701, 5.250046769979851646, 0.000000000000000000 ) ) ;
#95230 = EDGE_CURVE ( 'NONE', #102449, #138623, #98936, .T. ) ;
#95231 = UNCERTAINTY_MEASURE_WITH_UNIT (LENGTH_MEASURE( 1.000000000000000082E-05 ), #120207, 'distance_accuracy_value', 'NONE');
#95232 = CARTESIAN_POINT ( 'NONE',  ( 4.650083499362856365, 8.368921815991249957, 0.7216878364870438212 ) ) ;
#95233 = CARTESIAN_POINT ( 'NONE',  ( -0.7499999999999972244, 3.108333333333358706, -1.299038105676652011 ) ) ;
#95234 = CARTESIAN_POINT ( 'NONE',  ( 4.154361996720875361, -1.624486827992781990, 1.471056368041193441 ) ) ;
#95235 = CARTESIAN_POINT ( 'NONE',  ( -5.596818484342970912, 5.424043074688562172, -0.7998128361456221525 ) ) ;
#95236 = CARTESIAN_POINT ( 'NONE',  ( 0.5049859354315242577, 7.739806959121696472, -1.936057643312006471 ) ) ;
#95237 = CARTESIAN_POINT ( 'NONE',  ( 5.526144005543697446, 7.442112546579989996, -1.248357989223557452 ) ) ;
#95238 = CARTESIAN_POINT ( 'NONE',  ( -1.364683531250010295, 5.030208333674757171, 0.7879004041258379498 ) ) ;
#95239 = CARTESIAN_POINT ( 'NONE',  ( 2.965364049027201965, 0.2823637808789316028, -1.905579842893694975 ) ) ;
#95240 = CARTESIAN_POINT ( 'NONE',  ( 1.364683531250000303, 8.755208333674731946, -0.7879004041258355073 ) ) ;
#95242 = CARTESIAN_POINT ( 'NONE',  ( -3.307826292054310890, 5.842585859829892314, -1.082531754730549967 ) ) ;
#95241 = AXIS2_PLACEMENT_3D ( 'NONE', #140971, #142029, #205914 ) ;
#95243 = CARTESIAN_POINT ( 'NONE',  ( 0.1061415085658158342, 1.651838695520141398, 1.485519503937395402 ) ) ;
#95244 = CARTESIAN_POINT ( 'NONE',  ( -4.828112100242283766, 7.686528979374367410, -1.082531754730549967 ) ) ;
#95245 = ORIENTED_EDGE ( 'NONE', *, *, #148514, .F. ) ;
#95247 = CARTESIAN_POINT ( 'NONE',  ( -11.92619526913699879, 10.90000000000000036, -1.328859060402686199 ) ) ;
#95246 = CARTESIAN_POINT ( 'NONE',  ( -3.838366886444665393, 7.492195444245147939, 0.000000000000000000 ) ) ;
#95248 = CARTESIAN_POINT ( 'NONE',  ( 3.330499290451326200, 7.037332938835193730, -0.7998128361456291469 ) ) ;
#95249 = CARTESIAN_POINT ( 'NONE',  ( -2.393657244693855990, 0.2279079664470276545, -0.4206872822309645210 ) ) ;
#95250 = CARTESIAN_POINT ( 'NONE',  ( 0.4588732936604926760, 6.941177952499809400, -3.888237269999677004 ) ) ;
#95251 = CARTESIAN_POINT ( 'NONE',  ( -0.6823417656249969321, 4.030208333674754506, -1.181850606188749264 ) ) ;
#95252 = CARTESIAN_POINT ( 'NONE',  ( 2.050002923743666550, -1.344770872215072632, 1.104816081682137963 ) ) ;
#95253 = CARTESIAN_POINT ( 'NONE',  ( 6.773846765317333762, -7.246166700180801001, 6.773846765317311558 ) ) ;
#95254 = CARTESIAN_POINT ( 'NONE',  ( 0.4144086874100678664, 0.7473079093508437909, 1.814158889769983185 ) ) ;
#95255 = CARTESIAN_POINT ( 'NONE',  ( 1.364683531249986537, 1.217708333674754950, -0.7879004041258239610 ) ) ;
#95256 = CARTESIAN_POINT ( 'NONE',  ( -0.3405876332337993695, 3.079852035184914794, -0.4461735512528283154 ) ) ;
#95257 = CARTESIAN_POINT ( 'NONE',  ( 6.772347375734490527, -1.334533509509854943, 1.701269717329929820 ) ) ;
#95258 = CARTESIAN_POINT ( 'NONE',  ( -9.053093885623068715, 11.58502883802551153, -1.599625672291263179 ) ) ;
#95259 = CARTESIAN_POINT ( 'NONE',  ( -6.114364089638801403, 8.156510742710487705, 1.443375672974078761 ) ) ;
#95260 = MECHANICAL_DESIGN_GEOMETRIC_PRESENTATION_REPRESENTATION (  '', ( #119428 ), #123010 ) ;
#95261 = CARTESIAN_POINT ( 'NONE',  ( 5.207972885698374022, -2.151664816535401314, 0.2080130470862306957 ) ) ;
#95263 = ORIENTED_EDGE ( 'NONE', *, *, #183348, .T. ) ;
#95262 = DIRECTION ( 'NONE',  ( 0.000000000000000000, 0.000000000000000000, 1.000000000000000000 ) ) ;
#95264 = CARTESIAN_POINT ( 'NONE',  ( -1.201851678989727383E-14, 3.821875000341423689, 1.575800808251672791 ) ) ;
#95265 = CARTESIAN_POINT ( 'NONE',  ( 6.889933812677610625, -0.8438472966565238043, 1.779621742589713618 ) ) ;
#95266 = CARTESIAN_POINT ( 'NONE',  ( 6.696678128945787734, -1.136521523357211017, -1.309519827187540564 ) ) ;
#95268 = CARTESIAN_POINT ( 'NONE',  ( 3.491892070630482348, -2.189115664112693871, -0.1057334378413293807 ) ) ;
#95267 = CARTESIAN_POINT ( 'NONE',  ( -1.360316468750008667, 0.1197916670080665519, -0.7853790794159001276 ) ) ;
#95269 = CARTESIAN_POINT ( 'NONE',  ( 2.819673282491507393, -0.2271757706859862669, 2.296386706371948527 ) ) ;
#95270 = CARTESIAN_POINT ( 'NONE',  ( 5.729779026133646092, -1.304086877343976880, -1.595700086769378023 ) ) ;
#95271 = CARTESIAN_POINT ( 'NONE',  ( 0.6912261618599843116, -0.6995774015170745930, 1.811736774657431548 ) ) ;
#95272 = CARTESIAN_POINT ( 'NONE',  ( -5.382223794500835545, 8.262716279350872384, -1.082531754730543971 ) ) ;
#95273 = TOROIDAL_SURFACE ( 'NONE', #112631, 0.1600000000000000033, 0.08000000000000000167 ) ;
#95274 = DIRECTION ( 'NONE',  ( 0.000000000000000000, 0.000000000000000000, -1.000000000000000000 ) ) ;
#95275 = CARTESIAN_POINT ( 'NONE',  ( -9.453429866517900848, 14.52868746961063096, 7.391430727348221374 ) ) ;
#95276 = CARTESIAN_POINT ( 'NONE',  ( 3.691739789689612472, 1.995538565534977549, -0.7177698711837015022 ) ) ;
#95277 = CARTESIAN_POINT ( 'NONE',  ( 0.000000000000000000, 5.000000000000000888, 0.000000000000000000 ) ) ;
#95278 = CARTESIAN_POINT ( 'NONE',  ( 2.830704105008190030, 0.7231396562890278767, -1.882474209725725434 ) ) ;
#95279 = CARTESIAN_POINT ( 'NONE',  ( -4.894130264408862452, 7.693273827576896373, -1.082531754730548412 ) ) ;
#95280 = CARTESIAN_POINT ( 'NONE',  ( 5.333140672905051893, 0.1575165696711364749, 2.201206011701982934 ) ) ;
#95281 = CARTESIAN_POINT ( 'NONE',  ( -1.642778471875000035, -0.2552083328553750308, -2.845375778867859751 ) ) ;
#95282 = CARTESIAN_POINT ( 'NONE',  ( -3.231971923028420957, -3.070585806845580024, 1.214571025355801304 ) ) ;
#95283 = CARTESIAN_POINT ( 'NONE',  ( 11.96215121607992771, 12.27166446219175988, -0.9565349792967603459 ) ) ;
#95284 = CARTESIAN_POINT ( 'NONE',  ( -7.774674742793745708, 8.035151719539642912, 0.7998128361456341429 ) ) ;
#95286 = CARTESIAN_POINT ( 'NONE',  ( 6.825078400183554272, 2.951006455646578264, 2.596623860847916188 ) ) ;
#95285 = CARTESIAN_POINT ( 'NONE',  ( -5.066182726705734218, 7.967045547422810792, 1.194666625917781611 ) ) ;
#95287 = CARTESIAN_POINT ( 'NONE',  ( -9.811677024507259759, 4.107325997343203028, 6.339424533126782002 ) ) ;
#95288 = ORIENTED_EDGE ( 'NONE', *, *, #123001, .F. ) ;
#95289 = CARTESIAN_POINT ( 'NONE',  ( 4.856353099686935515, 0.7867916563346208925, 1.904994776275979129 ) ) ;
#95290 = CARTESIAN_POINT ( 'NONE',  ( -6.522881301506166629, 9.663759714182251770, 1.082531754730549967 ) ) ;
#95291 = B_SPLINE_CURVE_WITH_KNOTS ( 'NONE', 3,
 ( #174616, #54442, #92307, #120584, #203859, #7799, #171382, #137837, #154077, #106442 ),
 .UNSPECIFIED., .F., .F.,
 ( 4, 3, 3, 4 ),
 ( 0.000000000000000000, 3.125146907026659298E-05, 6.069395767275096592E-05, 9.014634065022558457E-05 ),
 .UNSPECIFIED. ) ;
#95292 = CARTESIAN_POINT ( 'NONE',  ( 0.4875569042710574674, 6.863504106564645824, -3.669039421667600998 ) ) ;
#95293 = CARTESIAN_POINT ( 'NONE',  ( -4.391951695823077984, 7.211361847513815704, 1.199719254218464037 ) ) ;
#95294 = CARTESIAN_POINT ( 'NONE',  ( -4.465841460056652501, 7.274597540891426739, 1.282467851283217275 ) ) ;
#95295 = CARTESIAN_POINT ( 'NONE',  ( 3.756514258062096712, 2.010158954970509892, 0.1956256540626959695 ) ) ;
#95296 = CARTESIAN_POINT ( 'NONE',  ( -1.500000000000013101, 1.379166666666689745, -0.8660254037844313801 ) ) ;
#95298 = CARTESIAN_POINT ( 'NONE',  ( 10.07334494527360569, 10.85458331234846696, 0.000000000000000000 ) ) ;
#95297 = CARTESIAN_POINT ( 'NONE',  ( -3.969505113751027547, 7.853116076009993840, 1.214306433183764966E-14 ) ) ;
#95299 = CARTESIAN_POINT ( 'NONE',  ( 6.337546739384100292, 9.481222731668410120, 1.199719254218460707 ) ) ;
#95300 = CARTESIAN_POINT ( 'NONE',  ( 2.694271958740936945, -2.055289539400024790, -0.1528356987768857700 ) ) ;
#95301 = CARTESIAN_POINT ( 'NONE',  ( 2.637342451166882373, 0.6819965276749391236, 1.897697610567940174 ) ) ;
#95302 = VERTEX_POINT ( 'NONE', #193729 ) ;
#95303 = CARTESIAN_POINT ( 'NONE',  ( -6.468692700515624949, 6.719432036793461904, 1.751973777778555601E-06 ) ) ;
#95304 = CARTESIAN_POINT ( 'NONE',  ( 3.571683402196252910, 6.254382171615883834, 1.199719254218462483 ) ) ;
#95306 = ORIENTED_EDGE ( 'NONE', *, *, #64923, .T. ) ;
#95305 = CARTESIAN_POINT ( 'NONE',  ( -0.1465803529718747722, 8.209140712741593404, -2.038183922479917420 ) ) ;
#95307 = CARTESIAN_POINT ( 'NONE',  ( 2.917342117414220670, 0.6766092434087739305, 1.899328150365031664 ) ) ;
#95308 = CARTESIAN_POINT ( 'NONE',  ( 2.466542765887615563, 0.09048117372523720170, -1.839033023284454060 ) ) ;
#95309 = CARTESIAN_POINT ( 'NONE',  ( 0.2589922964784003301, 0.8893095213439340396, 2.129655304206728328 ) ) ;
#95310 = CARTESIAN_POINT ( 'NONE',  ( 6.073126464278658432, 6.050012061272033392, 0.000000000000000000 ) ) ;
#95311 = CARTESIAN_POINT ( 'NONE',  ( 2.583474834239877449, 1.977432880963815309, -0.8734481387390122809 ) ) ;
#95312 = CARTESIAN_POINT ( 'NONE',  ( -5.738125327081750271, 7.717565519727259904, 1.599625672291269396 ) ) ;
#95313 = CARTESIAN_POINT ( 'NONE',  ( 4.540305813605725938, 0.8135460886731570307, 1.954998174167394520 ) ) ;
#95314 = ADVANCED_FACE ( 'NONE', ( #57344 ), #81605, .T. ) ;
#95315 = CARTESIAN_POINT ( 'NONE',  ( 2.689158180196444814, -1.321807234245642615, -1.880123443969876629 ) ) ;
#95316 = ORIENTED_EDGE ( 'NONE', *, *, #115695, .F. ) ;
#95317 = CARTESIAN_POINT ( 'NONE',  ( 5.381422217466640845, 4.322449550048925282, -2.440471613107405346 ) ) ;
#95318 = CIRCLE ( 'NONE', #5258, 0.08000000000000040412 ) ;
#95319 = CARTESIAN_POINT ( 'NONE',  ( 1.762360912074714125, -1.325010844092512796, 1.320751239342173200 ) ) ;
#95320 = CARTESIAN_POINT ( 'NONE',  ( 6.086792475191005636, -0.2889037430471863566, -1.950060635722290936 ) ) ;
#95322 = CARTESIAN_POINT ( 'NONE',  ( 9.707274797260268429, 10.42750147299956964, 0.000000000000000000 ) ) ;
#95321 = CARTESIAN_POINT ( 'NONE',  ( -1.201851678989727383E-14, 2.821875000341418804, 1.575800808251672791 ) ) ;
#95324 = CARTESIAN_POINT ( 'NONE',  ( 1.120068590173186163, -2.152398693614396397, 0.4866647226241942459 ) ) ;
#95323 = CARTESIAN_POINT ( 'NONE',  ( -6.364663046611467756, 9.512858423433634414, 1.199719254218452047 ) ) ;
#95325 = CARTESIAN_POINT ( 'NONE',  ( 6.760220206081136496, -2.069995208266177666, 0.04663682477341199450 ) ) ;
#95326 = CARTESIAN_POINT ( 'NONE',  ( 5.524057522564145728, 8.532151978711786100, 1.199719254218462483 ) ) ;
#95327 = CARTESIAN_POINT ( 'NONE',  ( -5.388475986427523345, 8.373973519885682393, 1.199719254218452047 ) ) ;
#95328 = CARTESIAN_POINT ( 'NONE',  ( 6.539320575229294441, 2.949125184229839380, 2.655650464557571144 ) ) ;
#95329 = CARTESIAN_POINT ( 'NONE',  ( 5.489129097700779170, 1.738912991666073715, -0.9288780838571459864 ) ) ;
#95330 = CARTESIAN_POINT ( 'NONE',  ( -0.1225938595818750754, -1.897163925677572305, -0.9476133185889324961 ) ) ;
#95331 = CARTESIAN_POINT ( 'NONE',  ( -1.402160292154681736E-14, 0.4937500006828175469, 1.732050807568877637 ) ) ;
#95332 = CARTESIAN_POINT ( 'NONE',  ( 4.283989073270632275, 1.505461842163426933, 1.749087475023381133 ) ) ;
#95333 = CARTESIAN_POINT ( 'NONE',  ( 2.061455334089828284, 1.712470851095546642, 1.149345886162132402 ) ) ;
#95334 = CARTESIAN_POINT ( 'NONE',  ( 6.304178240674458422, 10.29869901418813782, 1.040834085586084257E-14 ) ) ;
#95335 = ADVANCED_FACE ( 'NONE', ( #23762 ), #135259, .T. ) ;
#95336 = CARTESIAN_POINT ( 'NONE',  ( 5.692444392891300886, 7.734547439830227411, -1.599625672291281386 ) ) ;
#95337 = CARTESIAN_POINT ( 'NONE',  ( 4.061549535745618833, 6.896169004081968090, -1.199719254218452047 ) ) ;
#95338 = CARTESIAN_POINT ( 'NONE',  ( 0.6823417656249899377, 1.905208333674752952, 1.181850606188755259 ) ) ;
#95339 = CARTESIAN_POINT ( 'NONE',  ( -1.667727920668650388, 14.55184893431462356, 11.87324708719159183 ) ) ;
#95340 = CARTESIAN_POINT ( 'NONE',  ( 6.792271770322100721, 7.026664608238323950, -0.7216878364870257245 ) ) ;
#95341 = CARTESIAN_POINT ( 'NONE',  ( 4.457605324860562490, 1.741341149747036576, 1.296620029562136400 ) ) ;
#95343 = CARTESIAN_POINT ( 'NONE',  ( 3.702549152423353807, 1.581054339307564449, 0.9433870219286569769 ) ) ;
#95342 = CARTESIAN_POINT ( 'NONE',  ( -2.657034918598338180, 6.043698471765932112, -0.7216878364870267237 ) ) ;
#95345 = CARTESIAN_POINT ( 'NONE',  ( 6.720655732516645386, 3.710664525043025019, 2.240930934554703491 ) ) ;
#95344 = CARTESIAN_POINT ( 'NONE',  ( -0.6823417656249969321, 5.717708333674756283, -1.181850606188749264 ) ) ;
#95346 = CARTESIAN_POINT ( 'NONE',  ( 4.968408144156593487, -2.063508908063705238, -0.7385586828293493333 ) ) ;
#95347 = CARTESIAN_POINT ( 'NONE',  ( 1.416814887940403445, 7.999555336178682197, -9.899480522462175358 ) ) ;
#95348 = CARTESIAN_POINT ( 'NONE',  ( 6.368092757517858082, 1.156555634672886246, 1.944455297613384204 ) ) ;
#95349 = EDGE_LOOP ( 'NONE', ( #188042, #49853, #143188 ) ) ;
#95350 = CARTESIAN_POINT ( 'NONE',  ( -4.172464037091858202, 7.595707080679858336, -0.9154354581521230161 ) ) ;
#95351 = CARTESIAN_POINT ( 'NONE',  ( 4.595358334023878832, 8.489709390108890474, -0.01759220550971198060 ) ) ;
#95352 = CARTESIAN_POINT ( 'NONE',  ( -5.112833325684916552, 7.058334528089422300, -1.443375672974066548 ) ) ;
#95353 = CARTESIAN_POINT ( 'NONE',  ( 4.584065335196271462, 5.481069324884694005, 1.082531754730549078 ) ) ;
#95354 = CARTESIAN_POINT ( 'NONE',  ( 0.7250502862299773588, -1.682426168213309703, 0.5495948440489316633 ) ) ;
#95355 = CARTESIAN_POINT ( 'NONE',  ( 5.461592787958983841, -1.588467041389821421, -1.236575366846304647 ) ) ;
#95356 = CARTESIAN_POINT ( 'NONE',  ( 6.982612806237943559, 8.105135347821125436, -1.199719254218446718 ) ) ;
#95357 = CARTESIAN_POINT ( 'NONE',  ( 3.874133602078254413, 1.168181435743149921, 1.752046721337781054 ) ) ;
#95358 = CARTESIAN_POINT ( 'NONE',  ( 2.038566206862189478, -1.479296367703235360, 1.217016582141629666 ) ) ;
#95359 = CARTESIAN_POINT ( 'NONE',  ( 3.009020027229115879, 5.597941567487558778, -1.199719254218446718 ) ) ;
#95360 = CARTESIAN_POINT ( 'NONE',  ( 2.734760313433327372, -1.883857982319175450, -0.5745676990022812181 ) ) ;
#95361 = CARTESIAN_POINT ( 'NONE',  ( 5.010023637874760460, -0.7231455074051349463, 1.886094130455595375 ) ) ;
#95362 = CARTESIAN_POINT ( 'NONE',  ( 1.199835987674138460, -1.870836310881810682, -0.003643258294119822160 ) ) ;
#95365 = VERTEX_POINT ( 'NONE', #31250 ) ;
#95364 = CARTESIAN_POINT ( 'NONE',  ( 0.9844543725016400293, -1.211084316286781037, 1.480072698922259455 ) ) ;
#95363 = CARTESIAN_POINT ( 'NONE',  ( 4.969259055160575755, 0.1640942704066571667, -1.717058449848630985 ) ) ;
#95367 = CARTESIAN_POINT ( 'NONE',  ( 4.880572111239557920, 4.796348339308675435, -0.7216878364870197293 ) ) ;
#95366 = CARTESIAN_POINT ( 'NONE',  ( 0.9794701899953797142, -0.05759512415488829418, -2.206297691287119722 ) ) ;
#95368 = CARTESIAN_POINT ( 'NONE',  ( -1.402160292154681736E-14, 2.509375000341417028, -1.575800808251660134 ) ) ;
#95369 = CARTESIAN_POINT ( 'NONE',  ( 8.697719238366680372, 10.10609285197134533, 1.199719254218462483 ) ) ;
#95371 = CARTESIAN_POINT ( 'NONE',  ( 11.91826848676304529, 11.00833707238745696, 1.400000051402190193 ) ) ;
#95370 = AXIS2_PLACEMENT_3D ( 'NONE', #75946, #110650, #91156 ) ;
#95372 = FILL_AREA_STYLE ('',( #28208 ) ) ;
#95373 = CARTESIAN_POINT ( 'NONE',  ( 6.631696427350994405, 1.982895789845315671, -0.5951614246157420629 ) ) ;
#95374 =( BOUNDED_SURFACE ( )  B_SPLINE_SURFACE ( 1, 2, ( 
 ( #82683, #31826, #81623, #144546, #147707, #162891, #63245, #112073, #148765, #47019, #177002, #213726, #65349, #13419, #98956, #211609, #210553, #49143, #334, #45953, #115259, #14474, #165007, #16601, #62189, #178075, #113134, #30764, #28618, #29693, #127272, #193244, #78424, #94707, #79494, #179141, #96844, #160749, #12344, #195388, #80563, #194312, #146662, #161831, #212676, #64316, #130461, #196451, #48094, #114206, #180204, #149842, #17665, #86962, #37136, #70679, #52331, #101066, #67474, #133620, #136791, #154102, #199622, #202817, #168212, #185512, #54466, #1412, #51268, #118460, #184446, #198551, #183388, #21921, #120610, #83751, #66407, #167153, #36064, #102146, #186587, #103217, #68551, #84825, #50200, #18740, #132552, #151972, #19811, #117392, #34994, #134678, #100012, #38215, #150913, #2474, #153031, #169277, #104288, #85898, #200681, #3546, #69616, #170336, #135725, #201748, #20863, #53389, #88029, #116318, #182309, #4604, #119526, #33938, #166077, #137865, #191908, #106466, #55529, #7825, #72830, #74984, #8904, #206035, #73917, #24079, #43571, #203885, #189789, #171410, #142149, #105372, #71749, #187651, #173582, #174641, #172493, #138933, #121684, #190847, #141092, #109690, #208164, #9970, #27284, #25152, #175694, #91253, #41440, #122766, #207103, #39277, #22999, #90184, #59795, #140010, #125952, #155171, #6755, #92335, #93390, #5671, #89117, #204954, #156247, #56602, #58731, #188726, #40363, #57669, #76047, #123826, #124883, #108614, #107548, #42508, #157313, #26219, #158377, #115004, #79245, #209218, #130208, #64063, #45702, #65103, #29440, #28361, #47843, #60860, #161580, #12102, #14214, #162640, #145364, #13167, #177823, #197246, #77104, #129157, #110749, #81374, #44634, #11026, #127021, #112884, #113954, #111820, #78172, #143228, #196201, #80309, #48885, #147457, #163707, #181002, #178896, #32622, #30510, #195133, #61934, #146409, #192980, #176747, #95531, #213479, #211363, #131259, #94457, #160497, #31573, #159426, #144300, #210293, #128092, #62988, #194050, #212422, #46770, #96591, #179950, #15289, #97648, #3293, #201491, #116062, #69361, #134427, #34740, #83494, #54211, #18490, #148518, #135469, #53137, #199365, #4354, #183134, #182052, #119268, #186325, #17410, #102959, #200430, #185253, #86704, #33682, #149576, #84568, #2219, #16347, #1160, #120349, #152773, #49941, #98699, #51011, #150656, #68294, #70422, #36877, #100813, #117132, #82428, #166898, #164758, #184191, #52076, #67223, #133358, #118203, #132294, #136540, #99757, #165826, #169018, #20616, #202559, #35813, #101890, #167955, #19559, #84, #85635, #151721, #66149, #198300, #75789, #141896, #153848, #190587, #138673, #89928, #157056, #170079, #9713, #204693, #21666, #37960, #71498, #57404, #8645, #106209, #39027, #23823, #121425, #105110, #172235, #140829, #158122, #139751, #188465, #123569, #203625, #155979, #58474, #108357 ),
 ( #7566, #87772, #154914, #207907, #25959, #55276, #104033, #56343, #73652, #205776, #92064, #74724, #40096, #122504, #5419, #189532, #137609, #41180, #107287, #88859, #171150, #173309, #187395, #59528, #22741, #6498, #124629, #206841, #42244, #24888, #72573, #90993, #174379, #125688, #94197, #78975, #96328, #46498, #15027, #81118, #93129, #129956, #77914, #29174, #162383, #109430, #163447, #144033, #27021, #193790, #44369, #112622, #194865, #177562, #45439, #210029, #147204, #175436, #161312, #142961, #113694, #76842, #43311, #159168, #145095, #146148, #61670, #110492, #10767, #13961, #178632, #213229, #179697, #195944, #64861, #211099, #191646, #62723, #12896, #160237, #30244, #208963, #60596, #127838, #31313, #111553, #97391, #126754, #192714, #63798, #176491, #28102, #11836, #95264, #128884, #80045, #212163, #47580, #184999, #84314, #168766, #150399, #100566, #33432, #200179, #196998, #82173, #898, #52883, #133105, #36624, #65899, #132045, #3038, #152520, #119018, #102708, #198054, #17161, #181799, #183945, #16089, #20371, #148267, #201242, #86456, #35555, #19303, #214266, #101635, #166638, #66966, #115811, #4105, #50748, #180748, #167701, #85383, #83235, #131006, #199103, #49684, #151467, #48633, #99509, #135229, #18230, #69107, #114750, #165566, #149320, #116877, #34492, #32375, #182876, #98440, #164505, #1967, #68031, #134171, #51832, #117950, #127319, #109983, #75277, #91552, #202306, #173871, #136286, #158666, #42804, #124119, #206329, #141392, #106761, #61157, #156540, #24362, #93685, #43867, #77404, #59021, #107843, #74216, #140311, #143521, #190082, #174935, #192205, #142446, #111042, #177049, #189018, #11326, #25445, #125177, #175993, #56889, #44934, #157609, #123064, #207402, #57954, #208454, #76339, #191139, #108913, #9205, #28666, #40660, #26516, #90473, #209516, #172790, #8130, #41734, #92624, #27587, #10264, #60086, #126244, #159727, #193289, #94751, #160799, #70174, #33977, #96888, #181293, #31869, #16643, #162937, #161877, #64360, #79540, #212721, #211654, #82727, #63292, #29736, #196493, #145658, #148804, #194356, #100052, #129452, #32920, #98996, #195435, #210602, #47064, #13464, #147751, #373, #14518, #179185, #113181, #30808, #165051, #80612, #130506, #66447, #48135, #62231, #146705, #131537, #114248, #178121, #180245, #97948, #65390, #164002, #15578, #81665, #213769, #132589, #197539, #49184, #115303, #198591, #50238, #116358, #182348, #12390, #78469, #144588, #128389, #45999, #112118, #95818, #121723, #18776, #35029, #170374, #102183, #51305, #133658, #166116, #2514, #137902, #103254, #68587, #120646, #186625, #134712, #200719, #38252, #187688, #104326, #20899, #21961, #71787, #183428, #118499, #199659, #150950, #184481, #201786, #86995, #52370, #83788, #17701, #117430, #185550, #136828, #19849, #167189, #152008, #101102, #84862, #85936, #54502, #203921, #53426, #168250, #37179, #36098 ) ),
 .UNSPECIFIED., .F., .F., .T. ) 
 B_SPLINE_SURFACE_WITH_KNOTS ( ( 2, 2 ),
 ( 3, 2, 2, 2, 2, 2, 2, 2, 2, 2, 2, 2, 2, 2, 2, 2, 2, 2, 2, 2, 2, 2, 2, 2, 2, 2, 2, 2, 2, 2, 2, 2, 2, 2, 2, 2, 2, 2, 2, 2, 2, 2, 2, 2, 2, 2, 2, 2, 2, 2, 2, 2, 2, 2, 2, 2, 2, 2, 2, 2, 2, 2, 2, 2, 2, 2, 2, 2, 2, 2, 2, 2, 2, 2, 2, 2, 2, 2, 2, 2, 2, 2, 2, 2, 2, 2, 2, 2, 2, 2, 2, 2, 2, 2, 2, 2, 2, 2, 2, 2, 2, 2, 2, 2, 2, 2, 2, 2, 2, 2, 2, 2, 2, 2, 2, 2, 2, 2, 2, 2, 2, 2, 2, 2, 2, 2, 2, 2, 2, 2, 2, 2, 2, 2, 2, 2, 2, 2, 2, 2, 2, 2, 2, 2, 2, 2, 2, 2, 2, 2, 2, 2, 2, 2, 2, 2, 2, 2, 2, 2, 2, 2, 2, 2, 2, 2, 2, 2, 3 ),
 ( 0.000000000000000000, 1.000000000000000000 ),
 ( 0.000000000000000000, 0.005952380952380952051, 0.01190476190476190410, 0.01785714285714285615, 0.02380952380952380820, 0.02976190476190476025, 0.03571428571428571230, 0.04166666666666666435, 0.04761904761904761640, 0.05357142857142856845, 0.05952380952380952051, 0.06547619047619047949, 0.07142857142857142461, 0.07738095238095238360, 0.08333333333333332871, 0.08928571428571428770, 0.09523809523809523281, 0.1011904761904761918, 0.1071428571428571369, 0.1130952380952380959, 0.1190476190476190410, 0.1250000000000000000, 0.1309523809523809590, 0.1369047619047619180, 0.1428571428571428492, 0.1488095238095238082, 0.1547619047619047672, 0.1607142857142857262, 0.1666666666666666574, 0.1726190476190476164, 0.1785714285714285754, 0.1845238095238095344, 0.1904761904761904656, 0.1964285714285714246, 0.2023809523809523836, 0.2083333333333333426, 0.2142857142857142738, 0.2202380952380952328, 0.2261904761904761918, 0.2321428571428571508, 0.2380952380952380820, 0.2440476190476190410, 0.2500000000000000000, 0.2559523809523809312, 0.2619047619047619180, 0.2678571428571428492, 0.2738095238095238360, 0.2797619047619047672, 0.2857142857142856984, 0.2916666666666666852, 0.2976190476190476164, 0.3035714285714285476, 0.3095238095238095344, 0.3154761904761904656, 0.3214285714285714524, 0.3273809523809523836, 0.3333333333333333148, 0.3392857142857143016, 0.3452380952380952328, 0.3511904761904761640, 0.3571428571428571508, 0.3630952380952380820, 0.3690476190476190688, 0.3750000000000000000, 0.3809523809523809312, 0.3869047619047619180, 0.3928571428571428492, 0.3988095238095238360, 0.4047619047619047672, 0.4107142857142856984, 0.4166666666666666852, 0.4226190476190476164, 0.4285714285714285476, 0.4345238095238095344, 0.4404761904761904656, 0.4464285714285714524, 0.4523809523809523836, 0.4583333333333333148, 0.4642857142857143016, 0.4702380952380952328, 0.4761904761904761640, 0.4821428571428571508, 0.4880952380952380820, 0.4940476190476190688, 0.5000000000000000000, 0.5059523809523809312, 0.5119047619047618625, 0.5178571428571429047, 0.5238095238095238360, 0.5297619047619047672, 0.5357142857142856984, 0.5416666666666666297, 0.5476190476190476719, 0.5535714285714286031, 0.5595238095238095344, 0.5654761904761904656, 0.5714285714285713969, 0.5773809523809523281, 0.5833333333333333703, 0.5892857142857143016, 0.5952380952380952328, 0.6011904761904761640, 0.6071428571428570953, 0.6130952380952381375, 0.6190476190476190688, 0.6250000000000000000, 0.6309523809523809312, 0.6369047619047618625, 0.6428571428571429047, 0.6488095238095238360, 0.6547619047619047672, 0.6607142857142856984, 0.6666666666666666297, 0.6726190476190476719, 0.6785714285714286031, 0.6845238095238095344, 0.6904761904761904656, 0.6964285714285713969, 0.7023809523809523281, 0.7083333333333333703, 0.7142857142857143016, 0.7202380952380952328, 0.7261904761904761640, 0.7321428571428570953, 0.7380952380952381375, 0.7440476190476190688, 0.7500000000000000000, 0.7559523809523809312, 0.7619047619047618625, 0.7678571428571429047, 0.7738095238095238360, 0.7797619047619047672, 0.7857142857142856984, 0.7916666666666666297, 0.7976190476190476719, 0.8035714285714286031, 0.8095238095238095344, 0.8154761904761904656, 0.8214285714285713969, 0.8273809523809523281, 0.8333333333333333703, 0.8392857142857143016, 0.8452380952380952328, 0.8511904761904761640, 0.8571428571428570953, 0.8630952380952381375, 0.8690476190476190688, 0.8750000000000000000, 0.8809523809523809312, 0.8869047619047618625, 0.8928571428571429047, 0.8988095238095238360, 0.9047619047619047672, 0.9107142857142856984, 0.9166666666666666297, 0.9226190476190476719, 0.9285714285714286031, 0.9345238095238095344, 0.9404761904761904656, 0.9464285714285713969, 0.9523809523809523281, 0.9583333333333333703, 0.9642857142857143016, 0.9702380952380952328, 0.9761904761904761640, 0.9821428571428570953, 0.9880952380952381375, 0.9940476190476190688, 1.000000000000000000 ),
 .UNSPECIFIED. ) 
 GEOMETRIC_REPRESENTATION_ITEM ( )  RATIONAL_B_SPLINE_SURFACE ( (
 ( 1.000000000000000000, 0.8660254037844387076, 1.000000000000000000, 0.8660254037844387076, 1.000000000000000000, 0.8660254037844387076, 1.000000000000000000, 0.8660254037844387076, 1.000000000000000000, 0.8660254037844387076, 1.000000000000000000, 0.8660254037844387076, 1.000000000000000000, 0.8660254037844387076, 1.000000000000000000, 0.8660254037844387076, 1.000000000000000000, 0.8660254037844387076, 1.000000000000000000, 0.8660254037844387076, 1.000000000000000000, 0.8660254037844387076, 1.000000000000000000, 0.8660254037844387076, 1.000000000000000000, 0.8660254037844387076, 1.000000000000000000, 0.8660254037844387076, 1.000000000000000000, 0.8660254037844387076, 1.000000000000000000, 0.8660254037844387076, 1.000000000000000000, 0.8660254037844387076, 1.000000000000000000, 0.8660254037844387076, 1.000000000000000000, 0.8660254037844387076, 1.000000000000000000, 0.8660254037844387076, 1.000000000000000000, 0.8660254037844387076, 1.000000000000000000, 0.8660254037844387076, 1.000000000000000000, 0.8660254037844387076, 1.000000000000000000, 0.8660254037844387076, 1.000000000000000000, 0.8660254037844387076, 1.000000000000000000, 0.8660254037844387076, 1.000000000000000000, 0.8660254037844387076, 1.000000000000000000, 0.8660254037844387076, 1.000000000000000000, 0.8660254037844387076, 1.000000000000000000, 0.8660254037844387076, 1.000000000000000000, 0.8660254037844387076, 1.000000000000000000, 0.8660254037844387076, 1.000000000000000000, 0.8660254037844387076, 1.000000000000000000, 0.8660254037844387076, 1.000000000000000000, 0.8660254037844387076, 1.000000000000000000, 0.8660254037844387076, 1.000000000000000000, 0.8660254037844387076, 1.000000000000000000, 0.8660254037844387076, 1.000000000000000000, 0.8660254037844387076, 1.000000000000000000, 0.8660254037844387076, 1.000000000000000000, 0.8660254037844387076, 1.000000000000000000, 0.8660254037844387076, 1.000000000000000000, 0.8660254037844387076, 1.000000000000000000, 0.8660254037844387076, 1.000000000000000000, 0.8660254037844387076, 1.000000000000000000, 0.8660254037844387076, 1.000000000000000000, 0.8660254037844387076, 1.000000000000000000, 0.8660254037844387076, 1.000000000000000000, 0.8660254037844387076, 1.000000000000000000, 0.8660254037844387076, 1.000000000000000000, 0.8660254037844387076, 1.000000000000000000, 0.8660254037844387076, 1.000000000000000000, 0.8660254037844387076, 1.000000000000000000, 0.8660254037844387076, 1.000000000000000000, 0.8660254037844387076, 1.000000000000000000, 0.8660254037844387076, 1.000000000000000000, 0.8660254037844387076, 1.000000000000000000, 0.8660254037844387076, 1.000000000000000000, 0.8660254037844387076, 1.000000000000000000, 0.8660254037844387076, 1.000000000000000000, 0.8660254037844387076, 1.000000000000000000, 0.8660254037844387076, 1.000000000000000000, 0.8660254037844387076, 1.000000000000000000, 0.8660254037844387076, 1.000000000000000000, 0.8660254037844387076, 1.000000000000000000, 0.8660254037844387076, 1.000000000000000000, 0.8660254037844387076, 1.000000000000000000, 0.8660254037844387076, 1.000000000000000000, 0.8660254037844387076, 1.000000000000000000, 0.8660254037844387076, 1.000000000000000000, 0.8660254037844387076, 1.000000000000000000, 0.8660254037844387076, 1.000000000000000000, 0.8660254037844387076, 1.000000000000000000, 0.8660254037844387076, 1.000000000000000000, 0.8660254037844387076, 1.000000000000000000, 0.8660254037844387076, 1.000000000000000000, 0.8660254037844387076, 1.000000000000000000, 0.8660254037844387076, 1.000000000000000000, 0.8660254037844387076, 1.000000000000000000, 0.8660254037844387076, 1.000000000000000000, 0.8660254037844387076, 1.000000000000000000, 0.8660254037844387076, 1.000000000000000000, 0.8660254037844387076, 1.000000000000000000, 0.8660254037844387076, 1.000000000000000000, 0.8660254037844387076, 1.000000000000000000, 0.8660254037844387076, 1.000000000000000000, 0.8660254037844387076, 1.000000000000000000, 0.8660254037844387076, 1.000000000000000000, 0.8660254037844387076, 1.000000000000000000, 0.8660254037844387076, 1.000000000000000000, 0.8660254037844387076, 1.000000000000000000, 0.8660254037844387076, 1.000000000000000000, 0.8660254037844387076, 1.000000000000000000, 0.8660254037844387076, 1.000000000000000000, 0.8660254037844387076, 1.000000000000000000, 0.8660254037844387076, 1.000000000000000000, 0.8660254037844387076, 1.000000000000000000, 0.8660254037844387076, 1.000000000000000000, 0.8660254037844387076, 1.000000000000000000, 0.8660254037844387076, 1.000000000000000000, 0.8660254037844387076, 1.000000000000000000, 0.8660254037844387076, 1.000000000000000000, 0.8660254037844387076, 1.000000000000000000, 0.8660254037844387076, 1.000000000000000000, 0.8660254037844387076, 1.000000000000000000, 0.8660254037844387076, 1.000000000000000000, 0.8660254037844387076, 1.000000000000000000, 0.8660254037844387076, 1.000000000000000000, 0.8660254037844387076, 1.000000000000000000, 0.8660254037844387076, 1.000000000000000000, 0.8660254037844387076, 1.000000000000000000, 0.8660254037844387076, 1.000000000000000000, 0.8660254037844387076, 1.000000000000000000, 0.8660254037844387076, 1.000000000000000000, 0.8660254037844387076, 1.000000000000000000, 0.8660254037844387076, 1.000000000000000000, 0.8660254037844387076, 1.000000000000000000, 0.8660254037844387076, 1.000000000000000000, 0.8660254037844387076, 1.000000000000000000, 0.8660254037844387076, 1.000000000000000000, 0.8660254037844387076, 1.000000000000000000, 0.8660254037844387076, 1.000000000000000000, 0.8660254037844387076, 1.000000000000000000, 0.8660254037844387076, 1.000000000000000000, 0.8660254037844387076, 1.000000000000000000, 0.8660254037844387076, 1.000000000000000000, 0.8660254037844387076, 1.000000000000000000, 0.8660254037844387076, 1.000000000000000000, 0.8660254037844387076, 1.000000000000000000, 0.8660254037844387076, 1.000000000000000000, 0.8660254037844387076, 1.000000000000000000, 0.8660254037844387076, 1.000000000000000000, 0.8660254037844387076, 1.000000000000000000, 0.8660254037844387076, 1.000000000000000000, 0.8660254037844387076, 1.000000000000000000, 0.8660254037844387076, 1.000000000000000000, 0.8660254037844387076, 1.000000000000000000, 0.8660254037844387076, 1.000000000000000000, 0.8660254037844387076, 1.000000000000000000, 0.8660254037844387076, 1.000000000000000000, 0.8660254037844387076, 1.000000000000000000, 0.8660254037844387076, 1.000000000000000000, 0.8660254037844387076, 1.000000000000000000, 0.8660254037844387076, 1.000000000000000000, 0.8660254037844387076, 1.000000000000000000, 0.8660254037844387076, 1.000000000000000000, 0.8660254037844387076, 1.000000000000000000, 0.8660254037844387076, 1.000000000000000000, 0.8660254037844387076, 1.000000000000000000, 0.8660254037844387076, 1.000000000000000000, 0.8660254037844387076, 1.000000000000000000, 0.8660254037844387076, 1.000000000000000000, 0.8660254037844387076, 1.000000000000000000, 0.8660254037844387076, 1.000000000000000000, 0.8660254037844387076, 1.000000000000000000, 0.8660254037844387076, 1.000000000000000000, 0.8660254037844387076, 1.000000000000000000, 0.8660254037844387076, 1.000000000000000000, 0.8660254037844387076, 1.000000000000000000, 0.8660254037844387076, 1.000000000000000000, 0.8660254037844387076, 1.000000000000000000, 0.8660254037844387076, 1.000000000000000000, 0.8660254037844387076, 1.000000000000000000, 0.8660254037844387076, 1.000000000000000000, 0.8660254037844387076, 1.000000000000000000, 0.8660254037844387076, 1.000000000000000000, 0.8660254037844387076, 1.000000000000000000, 0.8660254037844387076, 1.000000000000000000),
 ( 1.000000000000000000, 0.8660254037844387076, 1.000000000000000000, 0.8660254037844387076, 1.000000000000000000, 0.8660254037844387076, 1.000000000000000000, 0.8660254037844387076, 1.000000000000000000, 0.8660254037844387076, 1.000000000000000000, 0.8660254037844387076, 1.000000000000000000, 0.8660254037844387076, 1.000000000000000000, 0.8660254037844387076, 1.000000000000000000, 0.8660254037844387076, 1.000000000000000000, 0.8660254037844387076, 1.000000000000000000, 0.8660254037844387076, 1.000000000000000000, 0.8660254037844387076, 1.000000000000000000, 0.8660254037844387076, 1.000000000000000000, 0.8660254037844387076, 1.000000000000000000, 0.8660254037844387076, 1.000000000000000000, 0.8660254037844387076, 1.000000000000000000, 0.8660254037844387076, 1.000000000000000000, 0.8660254037844387076, 1.000000000000000000, 0.8660254037844387076, 1.000000000000000000, 0.8660254037844387076, 1.000000000000000000, 0.8660254037844387076, 1.000000000000000000, 0.8660254037844387076, 1.000000000000000000, 0.8660254037844387076, 1.000000000000000000, 0.8660254037844387076, 1.000000000000000000, 0.8660254037844387076, 1.000000000000000000, 0.8660254037844387076, 1.000000000000000000, 0.8660254037844387076, 1.000000000000000000, 0.8660254037844387076, 1.000000000000000000, 0.8660254037844387076, 1.000000000000000000, 0.8660254037844387076, 1.000000000000000000, 0.8660254037844387076, 1.000000000000000000, 0.8660254037844387076, 1.000000000000000000, 0.8660254037844387076, 1.000000000000000000, 0.8660254037844387076, 1.000000000000000000, 0.8660254037844387076, 1.000000000000000000, 0.8660254037844387076, 1.000000000000000000, 0.8660254037844387076, 1.000000000000000000, 0.8660254037844387076, 1.000000000000000000, 0.8660254037844387076, 1.000000000000000000, 0.8660254037844387076, 1.000000000000000000, 0.8660254037844387076, 1.000000000000000000, 0.8660254037844387076, 1.000000000000000000, 0.8660254037844387076, 1.000000000000000000, 0.8660254037844387076, 1.000000000000000000, 0.8660254037844387076, 1.000000000000000000, 0.8660254037844387076, 1.000000000000000000, 0.8660254037844387076, 1.000000000000000000, 0.8660254037844387076, 1.000000000000000000, 0.8660254037844387076, 1.000000000000000000, 0.8660254037844387076, 1.000000000000000000, 0.8660254037844387076, 1.000000000000000000, 0.8660254037844387076, 1.000000000000000000, 0.8660254037844387076, 1.000000000000000000, 0.8660254037844387076, 1.000000000000000000, 0.8660254037844387076, 1.000000000000000000, 0.8660254037844387076, 1.000000000000000000, 0.8660254037844387076, 1.000000000000000000, 0.8660254037844387076, 1.000000000000000000, 0.8660254037844387076, 1.000000000000000000, 0.8660254037844387076, 1.000000000000000000, 0.8660254037844387076, 1.000000000000000000, 0.8660254037844387076, 1.000000000000000000, 0.8660254037844387076, 1.000000000000000000, 0.8660254037844387076, 1.000000000000000000, 0.8660254037844387076, 1.000000000000000000, 0.8660254037844387076, 1.000000000000000000, 0.8660254037844387076, 1.000000000000000000, 0.8660254037844387076, 1.000000000000000000, 0.8660254037844387076, 1.000000000000000000, 0.8660254037844387076, 1.000000000000000000, 0.8660254037844387076, 1.000000000000000000, 0.8660254037844387076, 1.000000000000000000, 0.8660254037844387076, 1.000000000000000000, 0.8660254037844387076, 1.000000000000000000, 0.8660254037844387076, 1.000000000000000000, 0.8660254037844387076, 1.000000000000000000, 0.8660254037844387076, 1.000000000000000000, 0.8660254037844387076, 1.000000000000000000, 0.8660254037844387076, 1.000000000000000000, 0.8660254037844387076, 1.000000000000000000, 0.8660254037844387076, 1.000000000000000000, 0.8660254037844387076, 1.000000000000000000, 0.8660254037844387076, 1.000000000000000000, 0.8660254037844387076, 1.000000000000000000, 0.8660254037844387076, 1.000000000000000000, 0.8660254037844387076, 1.000000000000000000, 0.8660254037844387076, 1.000000000000000000, 0.8660254037844387076, 1.000000000000000000, 0.8660254037844387076, 1.000000000000000000, 0.8660254037844387076, 1.000000000000000000, 0.8660254037844387076, 1.000000000000000000, 0.8660254037844387076, 1.000000000000000000, 0.8660254037844387076, 1.000000000000000000, 0.8660254037844387076, 1.000000000000000000, 0.8660254037844387076, 1.000000000000000000, 0.8660254037844387076, 1.000000000000000000, 0.8660254037844387076, 1.000000000000000000, 0.8660254037844387076, 1.000000000000000000, 0.8660254037844387076, 1.000000000000000000, 0.8660254037844387076, 1.000000000000000000, 0.8660254037844387076, 1.000000000000000000, 0.8660254037844387076, 1.000000000000000000, 0.8660254037844387076, 1.000000000000000000, 0.8660254037844387076, 1.000000000000000000, 0.8660254037844387076, 1.000000000000000000, 0.8660254037844387076, 1.000000000000000000, 0.8660254037844387076, 1.000000000000000000, 0.8660254037844387076, 1.000000000000000000, 0.8660254037844387076, 1.000000000000000000, 0.8660254037844387076, 1.000000000000000000, 0.8660254037844387076, 1.000000000000000000, 0.8660254037844387076, 1.000000000000000000, 0.8660254037844387076, 1.000000000000000000, 0.8660254037844387076, 1.000000000000000000, 0.8660254037844387076, 1.000000000000000000, 0.8660254037844387076, 1.000000000000000000, 0.8660254037844387076, 1.000000000000000000, 0.8660254037844387076, 1.000000000000000000, 0.8660254037844387076, 1.000000000000000000, 0.8660254037844387076, 1.000000000000000000, 0.8660254037844387076, 1.000000000000000000, 0.8660254037844387076, 1.000000000000000000, 0.8660254037844387076, 1.000000000000000000, 0.8660254037844387076, 1.000000000000000000, 0.8660254037844387076, 1.000000000000000000, 0.8660254037844387076, 1.000000000000000000, 0.8660254037844387076, 1.000000000000000000, 0.8660254037844387076, 1.000000000000000000, 0.8660254037844387076, 1.000000000000000000, 0.8660254037844387076, 1.000000000000000000, 0.8660254037844387076, 1.000000000000000000, 0.8660254037844387076, 1.000000000000000000, 0.8660254037844387076, 1.000000000000000000, 0.8660254037844387076, 1.000000000000000000, 0.8660254037844387076, 1.000000000000000000, 0.8660254037844387076, 1.000000000000000000, 0.8660254037844387076, 1.000000000000000000, 0.8660254037844387076, 1.000000000000000000, 0.8660254037844387076, 1.000000000000000000, 0.8660254037844387076, 1.000000000000000000, 0.8660254037844387076, 1.000000000000000000, 0.8660254037844387076, 1.000000000000000000, 0.8660254037844387076, 1.000000000000000000, 0.8660254037844387076, 1.000000000000000000, 0.8660254037844387076, 1.000000000000000000, 0.8660254037844387076, 1.000000000000000000, 0.8660254037844387076, 1.000000000000000000, 0.8660254037844387076, 1.000000000000000000, 0.8660254037844387076, 1.000000000000000000, 0.8660254037844387076, 1.000000000000000000, 0.8660254037844387076, 1.000000000000000000, 0.8660254037844387076, 1.000000000000000000, 0.8660254037844387076, 1.000000000000000000, 0.8660254037844387076, 1.000000000000000000, 0.8660254037844387076, 1.000000000000000000, 0.8660254037844387076, 1.000000000000000000, 0.8660254037844387076, 1.000000000000000000, 0.8660254037844387076, 1.000000000000000000, 0.8660254037844387076, 1.000000000000000000, 0.8660254037844387076, 1.000000000000000000, 0.8660254037844387076, 1.000000000000000000, 0.8660254037844387076, 1.000000000000000000, 0.8660254037844387076, 1.000000000000000000, 0.8660254037844387076, 1.000000000000000000, 0.8660254037844387076, 1.000000000000000000, 0.8660254037844387076, 1.000000000000000000, 0.8660254037844387076, 1.000000000000000000, 0.8660254037844387076, 1.000000000000000000) ) ) 
 REPRESENTATION_ITEM ( '' )  SURFACE ( )  );
#95375 = CARTESIAN_POINT ( 'NONE',  ( 1.047426762419433777, 1.826728496382063582, -0.9743617655595809834 ) ) ;
#95377 = CARTESIAN_POINT ( 'NONE',  ( 0.7499999999999902300, 2.483333333333351156, 1.299038105676669330 ) ) ;
#95376 = MECHANICAL_DESIGN_GEOMETRIC_PRESENTATION_REPRESENTATION (  '', ( #88547 ), #123270 ) ;
#95378 = CARTESIAN_POINT ( 'NONE',  ( 7.122110765880372618, 7.203550736482235095, 0.7998128361456341429 ) ) ;
#95379 = CARTESIAN_POINT ( 'NONE',  ( -8.227100285394159940, 8.492705175914988303, 0.7998128361456602331 ) ) ;
#95380 = CARTESIAN_POINT ( 'NONE',  ( 4.746236293235721604, 7.694970221153795364, 1.199719254218451159 ) ) ;
#95381 = CARTESIAN_POINT ( 'NONE',  ( 5.408877457991549953, -0.5154355754800542533, -2.056752310636373426 ) ) ;
#95382 = CARTESIAN_POINT ( 'NONE',  ( 0.6823417656249899377, 2.092708333674753174, 1.181850606188767472 ) ) ;
#95383 = CARTESIAN_POINT ( 'NONE',  ( 1.499999999999987121, 3.295833333333354709, -0.8660254037844262731 ) ) ;
#95385 = CARTESIAN_POINT ( 'NONE',  ( 2.672928840188529609, 6.270167413528593414, 0.000000000000000000 ) ) ;
#95384 = CARTESIAN_POINT ( 'NONE',  ( 6.795372052238223048, -1.752927774724974297, 0.8811163259476795240 ) ) ;
#95386 = CARTESIAN_POINT ( 'NONE',  ( 3.901720107437017582, 0.2930258228103881368, 1.994564303527603499 ) ) ;
#95387 = EDGE_CURVE ( 'NONE', #192862, #82080, #101761, .T. ) ;
#95388 = CARTESIAN_POINT ( 'NONE',  ( 4.610495038435900916, 1.835019742331613690, 0.5502660077172877306 ) ) ;
#95389 = FACE_OUTER_BOUND ( 'NONE', #30934, .T. ) ;
#95390 = CARTESIAN_POINT ( 'NONE',  ( 2.718528139169604341, 2.064530135181973591, 0.7356957861901700646 ) ) ;
#95391 = CARTESIAN_POINT ( 'NONE',  ( -11.07790593930098311, 11.29999999999999893, -0.7000000000000009548 ) ) ;
#95392 = CARTESIAN_POINT ( 'NONE',  ( 0.7499999999999885647, 0.3479166673494848983, -1.299038105676652899 ) ) ;
#95393 = CARTESIAN_POINT ( 'NONE',  ( 4.869394097828703138, -1.702981969582622046, -1.073415598185305964 ) ) ;
#95394 = CARTESIAN_POINT ( 'NONE',  ( -5.343885102080728977, 9.386283052402845328, 0.7998128361456481317 ) ) ;
#95396 = CARTESIAN_POINT ( 'NONE',  ( 5.624650681053017465, 0.4137061758265787592, 2.076257688556768066 ) ) ;
#95395 = CARTESIAN_POINT ( 'NONE',  ( -3.307826292054310890, 5.842585859829892314, -1.082531754730549967 ) ) ;
#95397 = FACE_OUTER_BOUND ( 'NONE', #184303, .T. ) ;
#95399 = CARTESIAN_POINT ( 'NONE',  ( -7.456058132872594335, 7.663432341298296535, 0.000000000000000000 ) ) ;
#95398 = CARTESIAN_POINT ( 'NONE',  ( 3.087527064991796077, -0.8449906179068911172, 1.912563079267016297 ) ) ;
#95401 = ORIENTED_EDGE ( 'NONE', *, *, #134348, .T. ) ;
#95400 = CARTESIAN_POINT ( 'NONE',  ( 1.395042272690392604, 1.302445673786157831, 1.130794771346554928 ) ) ;
#95402 = CARTESIAN_POINT ( 'NONE',  ( 4.746395313581045272, 1.087821826000659131, -1.820160695957805608 ) ) ;
#95403 = CARTESIAN_POINT ( 'NONE',  ( 4.286349120214771879, 8.152491073559232859, -0.7998128361456221525 ) ) ;
#95404 = SURFACE_SIDE_STYLE ('',( #177699 ) ) ;
#95405 = CARTESIAN_POINT ( 'NONE',  ( 1.224999999999947020, 0.8958333333333403647, -0.7072540797573197979 ) ) ;
#95406 = CARTESIAN_POINT ( 'NONE',  ( -0.03870269234685246723, -9.454881121928412568, 9.603712783164930045 ) ) ;
#95407 = CARTESIAN_POINT ( 'NONE',  ( 7.481401836642521452, 7.622723652371411696, 1.040834085586084257E-14 ) ) ;
#95408 = ORIENTED_EDGE ( 'NONE', *, *, #23468, .F. ) ;
#95409 = FACE_BOUND ( 'NONE', #11984, .T. ) ;
#95411 = CARTESIAN_POINT ( 'NONE',  ( 1.576514528963068429, -1.280961997807128938, 1.281107859597712118 ) ) ;
#95410 = CARTESIAN_POINT ( 'NONE',  ( 5.367048706163317640, 7.354919138647580290, -1.599625672291281386 ) ) ;
#95413 = CARTESIAN_POINT ( 'NONE',  ( -5.045605722580076780, 9.038290442985410067, -0.7998128361456231517 ) ) ;
#95412 = CIRCLE ( 'NONE', #195732, 0.07999999999999993228 ) ;
#95414 = CARTESIAN_POINT ( 'NONE',  ( 2.855963913973019963, 6.483708332943829866, 0.000000000000000000 ) ) ;
#95415 = ORIENTED_EDGE ( 'NONE', *, *, #125962, .T. ) ;
#95416 = CARTESIAN_POINT ( 'NONE',  ( 5.468734858265785093, 7.473552982767158070, 1.599625672291269396 ) ) ;
#95417 = CARTESIAN_POINT ( 'NONE',  ( 2.490610001455384470, -1.733883600701890737, -0.5244944224890700779 ) ) ;
#95418 = CARTESIAN_POINT ( 'NONE',  ( 6.639320575229259447, 2.969246179279591225, 2.450030562065998119 ) ) ;
#95419 = DIRECTION ( 'NONE',  ( 1.084202172485506406E-15, -0.5005768354468324022, -0.8656921114426507913 ) ) ;
#95420 = CARTESIAN_POINT ( 'NONE',  ( 4.117415066209698438, 7.437700365148243620, 0.6807796091479866307 ) ) ;
#95421 = ORIENTED_EDGE ( 'NONE', *, *, #199200, .T. ) ;
#95422 = CARTESIAN_POINT ( 'NONE',  ( 4.105780043149899861, 0.6285678624660723246, -1.751810336424673542 ) ) ;
#95423 = CARTESIAN_POINT ( 'NONE',  ( 1.089294787249419194, -0.4641297292061612456, 1.858405954227143386 ) ) ;
#95424 = CARTESIAN_POINT ( 'NONE',  ( 6.124042008734975617, -1.070608276503826950, -1.601302156493543905 ) ) ;
#95425 = DIRECTION ( 'NONE',  ( 0.000000000000000000, 0.000000000000000000, -1.000000000000000000 ) ) ;
#95426 = CARTESIAN_POINT ( 'NONE',  ( -1.347971487989957070E-14, -3.018749999044084475, 3.475000000000000089 ) ) ;
#95427 = AXIS2_PLACEMENT_3D ( 'NONE', #192874, #45598, #159325 ) ;
#95428 = CARTESIAN_POINT ( 'NONE',  ( 4.633164669693822901, 8.325607986553848150, 0.3865003237762173471 ) ) ;
#95429 = FACE_OUTER_BOUND ( 'NONE', #139348, .T. ) ;
#95430 = CARTESIAN_POINT ( 'NONE',  ( -3.795919822146293754, 4.491289883001181593, -1.082531754730549967 ) ) ;
#95431 = CARTESIAN_POINT ( 'NONE',  ( 6.968527767744088663, 11.07377346243604599, 0.7216878364870438212 ) ) ;
#95432 = CARTESIAN_POINT ( 'NONE',  ( 5.928554213991230171, -1.252361881311152558, 1.519918492727867054 ) ) ;
#95433 = CARTESIAN_POINT ( 'NONE',  ( -4.069418662396130593, 7.899405539437467816, -0.7998128361456281477 ) ) ;
#95434 = CARTESIAN_POINT ( 'NONE',  ( -9.828980619278564011E-14, 7.054063922337708625, 3.955400951015630273 ) ) ;
#95435 = EDGE_CURVE ( 'NONE', #73782, #10073, #179629, .T. ) ;
#95436 = CIRCLE ( 'NONE', #130121, 0.07999999999999993228 ) ;
#95437 = CARTESIAN_POINT ( 'NONE',  ( 0.4629771330677232011, 0.2027323353172970355, -2.080777175944429125 ) ) ;
#95438 = CARTESIAN_POINT ( 'NONE',  ( 5.206133053153118695, 6.319824444209305447, 1.213385250716643604 ) ) ;
#95439 = CARTESIAN_POINT ( 'NONE',  ( 4.963854806921006002, 1.905440169433350484, -0.2825122895667788181 ) ) ;
#95440 = CARTESIAN_POINT ( 'NONE',  ( -7.314787569772770226, 8.492672571945082183, -1.199719254218452935 ) ) ;
#95441 = CARTESIAN_POINT ( 'NONE',  ( 1.237009950130557590, -1.652246606862219025, 0.7767072072360350354 ) ) ;
#95442 = CARTESIAN_POINT ( 'NONE',  ( 1.805583701156989518, 1.836052299496168771, 1.224139149458243425 ) ) ;
#95443 = SURFACE_SIDE_STYLE ('',( #111727 ) ) ;
#95444 = CARTESIAN_POINT ( 'NONE',  ( 0.2110004604562870645, 1.588762659912812403, -1.064147093309028680 ) ) ;
#95445 = EDGE_CURVE ( 'NONE', #96829, #108458, #104885, .T. ) ;
#95446 = ORIENTED_EDGE ( 'NONE', *, *, #115968, .F. ) ;
#95447 = CARTESIAN_POINT ( 'NONE',  ( 0.8011416495431540330, -1.691081937322042483, 1.009368880822520298 ) ) ;
#95448 = CARTESIAN_POINT ( 'NONE',  ( 1.224054851709508451, 1.872146073007043610, 0.5162294149947727062 ) ) ;
#95449 = CARTESIAN_POINT ( 'NONE',  ( 0.3509351863830567075, -0.9528684895154272416, 1.776737725368633614 ) ) ;
#95451 = CARTESIAN_POINT ( 'NONE',  ( 5.770303593930925956, -0.8350939829899912681, -1.663081984830430793 ) ) ;
#95450 = CARTESIAN_POINT ( 'NONE',  ( -4.932134020321308654, 8.976183133675331050, 0.7998128361456291469 ) ) ;
#95452 = CARTESIAN_POINT ( 'NONE',  ( 4.376249722160992839, 8.327651452488305850, 0.000000000000000000 ) ) ;
#95454 = EDGE_CURVE ( 'NONE', #180844, #80984, #106183, .T. ) ;
#95453 = CARTESIAN_POINT ( 'NONE',  ( -4.028292277495545193, 3.858391361152785581, 2.500000000000000000 ) ) ;
#95455 = CARTESIAN_POINT ( 'NONE',  ( 6.509000000000010111, 6.037005099786168394, 2.594901386363585694 ) ) ;
#95456 = CARTESIAN_POINT ( 'NONE',  ( -6.240830780992103755, 6.175390754112560110, 1.040834085586084257E-14 ) ) ;
#95457 = CARTESIAN_POINT ( 'NONE',  ( -7.422162748838431412, 7.623887726591770608, -0.7998128361456362523 ) ) ;
#95458 = CARTESIAN_POINT ( 'NONE',  ( 1.751786407749492014, 2.185395279939935431, -0.1653414253460702699 ) ) ;
#95459 = CARTESIAN_POINT ( 'NONE',  ( 3.199361063144961825, 6.676412307070352270, -0.7216878364870267237 ) ) ;
#95460 = CARTESIAN_POINT ( 'NONE',  ( 6.933015448541703485, 9.181880338089085214, 1.599625672291268286 ) ) ;
#95461 = DIRECTION ( 'NONE',  ( -5.551115123125764829E-17, 0.000000000000000000, 1.000000000000000000 ) ) ;
#95462 = CARTESIAN_POINT ( 'NONE',  ( 2.648829494986388422, -1.517897411861212076, 1.014145048410304284 ) ) ;
#95463 = CARTESIAN_POINT ( 'NONE',  ( -4.485049888022365927, 4.126979712314507331, 0.7998128361456341429 ) ) ;
#95464 = CARTESIAN_POINT ( 'NONE',  ( -3.928111819657352566, 5.605883094398769195, 1.599625672291267398 ) ) ;
#95465 =( BOUNDED_SURFACE ( )  B_SPLINE_SURFACE ( 3, 2, ( 
 ( #26596, #58036, #61239 ),
 ( #110058, #123149, #92697 ),
 ( #76411, #142521, #126321 ),
 ( #192282, #176070, #193368 ),
 ( #177126, #146788, #145737 ),
 ( #46076, #163018, #13546 ),
 ( #213852, #178202, #62308 ),
 ( #95903, #63375, #94827 ),
 ( #211737, #16726, #79618 ),
 ( #161955, #129531, #195511 ),
 ( #47148, #128467, #98031 ),
 ( #64441, #112196, #197621 ),
 ( #113264, #194435, #29819 ),
 ( #181381, #212803, #14600 ),
 ( #160879, #180325, #148887 ),
 ( #196575, #114329, #48217 ),
 ( #78548, #31947, #165135 ),
 ( #80697, #164085, #179269 ),
 ( #30892, #96970, #130585 ),
 ( #99083, #15666, #81753 ),
 ( #49266, #147835, #28743 ),
 ( #65473, #131623, #115387 ),
 ( #66528, #33004, #82810 ),
 ( #144666, #460, #132671 ),
 ( #198677, #111123, #12473 ),
 ( #210679, #183507, #22043 ),
 ( #103335, #53514, #185631 ),
 ( #199749, #87080, #166194 ) ),
 .UNSPECIFIED., .F., .F., .T. ) 
 B_SPLINE_SURFACE_WITH_KNOTS ( ( 4, 2, 2, 2, 2, 2, 2, 2, 2, 2, 2, 2, 2, 4 ),
 ( 3, 3 ),
 ( 1.301042606982605321E-18, 0.001582303952082990970, 0.002373455928124485696, 0.003164607904165980638, 0.003955759880207476015, 0.004746911856248970524, 0.006329215808331960409, 0.007120367784373455786, 0.007911519760414950295, 0.008702671736456444804, 0.009493823712497939313, 0.01028497568853943556, 0.01107612766458093007, 0.01265843161666391908 ),
 ( 0.000000000000000000, 1.000000000000000000 ),
 .UNSPECIFIED. ) 
 GEOMETRIC_REPRESENTATION_ITEM ( )  RATIONAL_B_SPLINE_SURFACE ( (
 ( 1.000000000000000000, 0.8462409035377600475, 1.000000000000000000),
 ( 1.000000000000000000, 0.8465427114078758475, 1.000000000000000000),
 ( 1.000000000000000000, 0.8465641366848090099, 1.000000000000000000),
 ( 1.000000000000000000, 0.8467900531823037147, 1.000000000000000000),
 ( 1.000000000000000000, 0.8468781625786160339, 1.000000000000000000),
 ( 1.000000000000000000, 0.8471120945301685579, 1.000000000000000000),
 ( 1.000000000000000000, 0.8472463485371222180, 1.000000000000000000),
 ( 1.000000000000000000, 0.8473012231814394113, 1.000000000000000000),
 ( 1.000000000000000000, 0.8468507819384271107, 1.000000000000000000),
 ( 1.000000000000000000, 0.8460871546575347013, 1.000000000000000000),
 ( 1.000000000000000000, 0.8457728595780946712, 1.000000000000000000),
 ( 1.000000000000000000, 0.8456955564162187411, 1.000000000000000000),
 ( 1.000000000000000000, 0.8472150014537547236, 1.000000000000000000),
 ( 1.000000000000000000, 0.8472169592757342604, 1.000000000000000000),
 ( 1.000000000000000000, 0.8467840124556752501, 1.000000000000000000),
 ( 1.000000000000000000, 0.8461344581662409992, 1.000000000000000000),
 ( 1.000000000000000000, 0.8459097183282422439, 1.000000000000000000),
 ( 1.000000000000000000, 0.8459637398922701390, 1.000000000000000000),
 ( 1.000000000000000000, 0.8462437954697883402, 1.000000000000000000),
 ( 1.000000000000000000, 0.8469148800072623384, 1.000000000000000000),
 ( 1.000000000000000000, 0.8472862011760097234, 1.000000000000000000),
 ( 1.000000000000000000, 0.8472609020320528428, 1.000000000000000000),
 ( 1.000000000000000000, 0.8471586627785127055, 1.000000000000000000),
 ( 1.000000000000000000, 0.8469901278039179138, 1.000000000000000000),
 ( 1.000000000000000000, 0.8469207196612665856, 1.000000000000000000),
 ( 1.000000000000000000, 0.8466859688974881504, 1.000000000000000000),
 ( 1.000000000000000000, 0.8465495423952427156, 1.000000000000000000),
 ( 1.000000000000000000, 0.8462407054814423679, 1.000000000000000000) ) ) 
 REPRESENTATION_ITEM ( '' )  SURFACE ( )  );
#95466 = CARTESIAN_POINT ( 'NONE',  ( -6.245422037512663671, 7.006708691962935553, -1.003398212925192157 ) ) ;
#95467 = CARTESIAN_POINT ( 'NONE',  ( 6.509000000000039421, 4.695815278351551214, 2.562658139094181386 ) ) ;
#95468 = CARTESIAN_POINT ( 'NONE',  ( 8.809047120577066181, 11.30030761213851953, 1.599625672291281386 ) ) ;
#95469 = CARTESIAN_POINT ( 'NONE',  ( 0.8031968939124977114, 1.574386321349549700, 1.110025428916910917 ) ) ;
#95470 = CARTESIAN_POINT ( 'NONE',  ( 5.629730433169950921, 1.891637868780412068, -0.5196590155819302836 ) ) ;
#95471 = CARTESIAN_POINT ( 'NONE',  ( -6.852756576703439961, 10.08230087520760954, 1.199719254218453823 ) ) ;
#95472 = CARTESIAN_POINT ( 'NONE',  ( 5.015626762051672571, 7.938982758113895422, 1.199719254218462483 ) ) ;
#95473 = CARTESIAN_POINT ( 'NONE',  ( 5.073855206572205567, -1.217758175834412260, 1.821886007100224969 ) ) ;
#95474 = EDGE_CURVE ( 'NONE', #177299, #164705, #202643, .T. ) ;
#95475 = CARTESIAN_POINT ( 'NONE',  ( 5.169736645512481132, 4.925780929386340823, 0.7998128361456341429 ) ) ;
#95476 = CARTESIAN_POINT ( 'NONE',  ( 3.907136544319700810, -1.695332804699274387, 1.187946514627869821 ) ) ;
#95478 = CARTESIAN_POINT ( 'NONE',  ( 1.364683531249988757, 0.6968750003414209138, 0.000000000000000000 ) ) ;
#95477 = CARTESIAN_POINT ( 'NONE',  ( 8.133143982689912121, 14.25145509247576570, 8.763746397669734733 ) ) ;
#95479 = ORIENTED_EDGE ( 'NONE', *, *, #200733, .F. ) ;
#95480 = CARTESIAN_POINT ( 'NONE',  ( 3.569189921330259807, -1.132127473341357771, 2.000487910885457854 ) ) ;
#95482 = EDGE_LOOP ( 'NONE', ( #160901, #43735, #34267, #190104, #175458, #204454, #167647, #25162 ) ) ;
#95481 = CARTESIAN_POINT ( 'NONE',  ( 6.426201623197458801, 9.480690412830290015, -1.082531754730537088 ) ) ;
#95484 = CARTESIAN_POINT ( 'NONE',  ( -3.285556943750000514, -0.1385416661887106660, -1.896917185911906500 ) ) ;
#95483 = CARTESIAN_POINT ( 'NONE',  ( 7.187230829020130329, 7.557726520044554697, 0.7216878364870267237 ) ) ;
#95485 = CARTESIAN_POINT ( 'NONE',  ( -11.52460864928264961, 13.87999999999998302, 3.346683403123524858 ) ) ;
#95486 = CARTESIAN_POINT ( 'NONE',  ( -10.31399889198507402, 4.822877898269746666, -6.141096068735103053 ) ) ;
#95487 = CARTESIAN_POINT ( 'NONE',  ( 3.556523421261322149, -1.712991659986836002, -0.9147756334835445147 ) ) ;
#95488 = VERTEX_POINT ( 'NONE', #154707 ) ;
#95489 = CARTESIAN_POINT ( 'NONE',  ( 3.714570900464321479, 7.277490450609501949, 0.7216878364870685791 ) ) ;
#95490 = ORIENTED_EDGE ( 'NONE', *, *, #110826, .F. ) ;
#95491 = CARTESIAN_POINT ( 'NONE',  ( 5.449440537890920311, -1.726199344983204265, 0.8234401749890255529 ) ) ;
#95492 = CARTESIAN_POINT ( 'NONE',  ( 6.721745554788610022, -1.671375598274482677, 0.4255071719459716517 ) ) ;
#95493 = CARTESIAN_POINT ( 'NONE',  ( 4.223842396274177347, 0.8578445224393380641, -1.825075645057252727 ) ) ;
#95494 = DIRECTION ( 'NONE',  ( 1.000000000000000000, 0.000000000000000000, -3.491481338843133355E-15 ) ) ;
#95495 = CARTESIAN_POINT ( 'NONE',  ( 1.348561525465460820, 2.204488851003219896, 0.1053889787279923829 ) ) ;
#95497 = CARTESIAN_POINT ( 'NONE',  ( -5.017926250833627755, 5.026871178826882947, 0.7216878364870257245 ) ) ;
#95496 = CARTESIAN_POINT ( 'NONE',  ( -8.967828540435322182, 12.54988483289483980, 1.199719254218462483 ) ) ;
#95499 = CARTESIAN_POINT ( 'NONE',  ( 6.784453145350711090, -1.736176628054094007, -0.3419908188336401311 ) ) ;
#95498 = CARTESIAN_POINT ( 'NONE',  ( 1.517645033149318978, -1.162591604200275963, -1.737351732476496657 ) ) ;
#95500 = CARTESIAN_POINT ( 'NONE',  ( 5.572888750952301073, -0.9041123360693378297, 1.802415994888312722 ) ) ;
#95502 = CARTESIAN_POINT ( 'NONE',  ( 2.590095216689162427, -2.286210222917249180, -0.1672752534159216153 ) ) ;
#95501 = CARTESIAN_POINT ( 'NONE',  ( 3.413620815590684199, 7.204584394822967752, 0.7998128361456281477 ) ) ;
#95503 = CARTESIAN_POINT ( 'NONE',  ( 0.9369944060461411484, 0.7087284392868421490, -1.589666227069729265 ) ) ;
#95504 = DIRECTION ( 'NONE',  ( 0.000000000000000000, -0.5005768354468324022, 0.8656921114426507913 ) ) ;
#95505 = CARTESIAN_POINT ( 'NONE',  ( 1.422726403049366706, 0.6964842469411072212, 1.588000322196560399 ) ) ;
#95506 = CARTESIAN_POINT ( 'NONE',  ( 1.360316468749945606, 0.06770833367471427999, -0.7853790794159161148 ) ) ;
#95507 = CARTESIAN_POINT ( 'NONE',  ( 11.55950211276791251, 11.37999999999998302, 3.221476510067114329 ) ) ;
#95508 = CARTESIAN_POINT ( 'NONE',  ( 1.645237833728605548, -0.3177867502775574837, -2.147667186158049191 ) ) ;
#95509 = CARTESIAN_POINT ( 'NONE',  ( 2.887907956677421506, -2.014008092954455265, 0.1037802451031161477 ) ) ;
#95510 = CARTESIAN_POINT ( 'NONE',  ( 4.781250000000003553, 0.7852924748302358982, 1.895863743163977100 ) ) ;
#95511 = CARTESIAN_POINT ( 'NONE',  ( 1.499999999999989120, 1.056250000682816603, 0.000000000000000000 ) ) ;
#95512 = CARTESIAN_POINT ( 'NONE',  ( 6.199827818874126706, -0.6464308959919072839, 1.814938386029739892 ) ) ;
#95513 = CARTESIAN_POINT ( 'NONE',  ( -0.6823417656250039265, 12.81770833367473017, -1.181850606188755259 ) ) ;
#95514 = CARTESIAN_POINT ( 'NONE',  ( 3.059039825962418746, 0.5433887813283566626, 2.153793114424791710 ) ) ;
#95515 = ORIENTED_EDGE ( 'NONE', *, *, #72633, .T. ) ;
#95516 = CARTESIAN_POINT ( 'NONE',  ( -9.578219923806457814, -9.914766490055704651, 0.1663656176996666236 ) ) ;
#95517 = CARTESIAN_POINT ( 'NONE',  ( 0.7499999999999867883, -0.4333333333333133641, -1.299038105676652899 ) ) ;
#95518 = CARTESIAN_POINT ( 'NONE',  ( 6.753933077901968396, 11.03133902419432566, 0.7998128361456462443 ) ) ;
#95519 = DIRECTION ( 'NONE',  ( 0.000000000000000000, 0.000000000000000000, -1.000000000000000000 ) ) ;
#95520 = CARTESIAN_POINT ( 'NONE',  ( 5.864775363713938816, 0.1190308195875185160, -1.736441914165016476 ) ) ;
#95521 = CARTESIAN_POINT ( 'NONE',  ( 4.035565188342554954, 1.848088059160474694, -0.6588067414724924076 ) ) ;
#95523 = CARTESIAN_POINT ( 'NONE',  ( -6.751597309925468693, 6.979211071108916364, 0.7216878364870317197 ) ) ;
#95522 = CARTESIAN_POINT ( 'NONE',  ( 4.356247428692526569, 3.976710176429713250, 0.7998128361456341429 ) ) ;
#95524 = CARTESIAN_POINT ( 'NONE',  ( -1.499577476386907859, 4.449079813965669317, -0.09296422598484958832 ) ) ;
#95525 = CARTESIAN_POINT ( 'NONE',  ( 4.218261219551087571, -1.158436920226207034, -1.943184041606202950 ) ) ;
#95526 = CARTESIAN_POINT ( 'NONE',  ( 1.768110600389400933, -2.047337470793224146, 0.2504565381693297788 ) ) ;
#95527 = CARTESIAN_POINT ( 'NONE',  ( -7.152089726408780379, 8.302858421353754181, -1.199719254218446718 ) ) ;
#95528 = PRESENTATION_LAYER_ASSIGNMENT (  '', '', ( #88547 ) ) ;
#95529 = CARTESIAN_POINT ( 'NONE',  ( 2.202381998968961696, -2.261980054776930427, 0.05578962468580014183 ) ) ;
#95530 = ORIENTED_EDGE ( 'NONE', *, *, #114707, .T. ) ;
#95531 = CARTESIAN_POINT ( 'NONE',  ( 0.7499999999999902300, 1.014583334016154526, 1.299038105676657340 ) ) ;
#95532 = CARTESIAN_POINT ( 'NONE',  ( 3.286256049847174676, -1.842268013383094427, -0.3231441395407097517 ) ) ;
#95533 = CARTESIAN_POINT ( 'NONE',  ( 2.549097654585132045, -1.194521797001405927, 1.257391726941985421 ) ) ;
#95534 = CARTESIAN_POINT ( 'NONE',  ( -0.05846771364293941453, -1.777572824190313261, -1.447063799157372044 ) ) ;
#95535 = CARTESIAN_POINT ( 'NONE',  ( 6.493248230727125758, 2.012220109224418518, -1.129477038640940734 ) ) ;
#95536 = CARTESIAN_POINT ( 'NONE',  ( 4.170900312159072421, -2.016029151617684256, -0.7805680927704603533 ) ) ;
#95537 = CARTESIAN_POINT ( 'NONE',  ( 4.769442245286214188, 1.119358777157190010, 1.586704836592154333 ) ) ;
#95538 = CARTESIAN_POINT ( 'NONE',  ( -10.65400978224035811, 11.32409958890225710, 1.040834085586084257E-14 ) ) ;
#95539 = CARTESIAN_POINT ( 'NONE',  ( 6.380143124955812262, -1.000617425381218561, 1.580232162242324545 ) ) ;
#95540 = CARTESIAN_POINT ( 'NONE',  ( 4.084722907606431974, 7.479936734012107458, 0.5927516458891276541 ) ) ;
#95541 = DIRECTION ( 'NONE',  ( 0.000000000000000000, -1.000000000000000000, 0.000000000000000000 ) ) ;
#95542 = CARTESIAN_POINT ( 'NONE',  ( 0.000000000000000000, 0.9200000000000041478, 0.000000000000000000 ) ) ;
#95543 = CARTESIAN_POINT ( 'NONE',  ( 5.256482491209823138, 1.942542154241846397, -0.5404887192124520068 ) ) ;
#95544 = CARTESIAN_POINT ( 'NONE',  ( -3.972175818679615222, 4.696921878956699103, 1.082531754730558626 ) ) ;
#95545 = CARTESIAN_POINT ( 'NONE',  ( 7.202405917357655341, 9.425892875049191488, 1.599625672291281386 ) ) ;
#95546 = CARTESIAN_POINT ( 'NONE',  ( 2.719161800852238464, -0.1789327596440904167, 1.816892639718168390 ) ) ;
#95547 = CARTESIAN_POINT ( 'NONE',  ( 1.940722911589174204, 2.182806717142399489, 0.3235914145361811767 ) ) ;
#95548 = VERTEX_POINT ( 'NONE', #191451 ) ;
#95549 = CARTESIAN_POINT ( 'NONE',  ( -5.465345319640241506, 5.548860092434608760, 0.7216878364870257245 ) ) ;
#95550 = CARTESIAN_POINT ( 'NONE',  ( -3.285556943750000514, -3.726041666188710799, -1.896917185911906500 ) ) ;
#95552 = CARTESIAN_POINT ( 'NONE',  ( -8.019811557683421910, 9.315200557840817908, 1.199719254218462483 ) ) ;
#95551 = B_SPLINE_CURVE_WITH_KNOTS ( 'NONE', 3,
 ( #145949, #26822, #162178, #95055, #194657, #161105, #10567 ),
 .UNSPECIFIED., .F., .F.,
 ( 4, 3, 4 ),
 ( 0.000000000000000000, 2.778074687866575757E-05, 5.739355541052443402E-05 ),
 .UNSPECIFIED. ) ;
#95553 = CARTESIAN_POINT ( 'NONE',  ( 1.547134890100225535, 0.2020692043026971751, 2.009678023649637879 ) ) ;
#95554 = CARTESIAN_POINT ( 'NONE',  ( 1.278162280329109279, 2.088516533416693743, -0.3659721813360562459 ) ) ;
#95555 = EDGE_LOOP ( 'NONE', ( #147856, #130378, #210413, #176896 ) ) ;
#95556 = CARTESIAN_POINT ( 'NONE',  ( -3.962726036944197894, 7.845207153068690431, -0.7998128361456481317 ) ) ;
#95557 = CARTESIAN_POINT ( 'NONE',  ( 1.639267886685547460, 1.721996695667164845, -0.7061035538288776836 ) ) ;
#95558 = CARTESIAN_POINT ( 'NONE',  ( 5.352771719296971042, 5.139321848801576387, 0.7998128361456341429 ) ) ;
#95559 = CARTESIAN_POINT ( 'NONE',  ( 6.819229409281153842, -0.1590044787766713985, 2.026160355490718601 ) ) ;
#95560 = CARTESIAN_POINT ( 'NONE',  ( 6.399064592084179992, -0.9530083391863402031, -1.777013033299412292 ) ) ;
#95561 = ORIENTED_EDGE ( 'NONE', *, *, #48296, .T. ) ;
#95562 = ORIENTED_EDGE ( 'NONE', *, *, #4605, .T. ) ;
#95563 = CARTESIAN_POINT ( 'NONE',  ( -8.299562589859897699, 12.83457345481192036, -0.7998128361456281477 ) ) ;
#95564 = CARTESIAN_POINT ( 'NONE',  ( 4.090329635444483358, -1.806102819543849769, -0.2658631594732660530 ) ) ;
#95565 = AXIS2_PLACEMENT_3D ( 'NONE', #189665, #8782, #22878 ) ;
#95567 = CARTESIAN_POINT ( 'NONE',  ( -4.851289806644571989, 6.918820993438449030, -1.443092038473028582 ) ) ;
#95566 = CARTESIAN_POINT ( 'NONE',  ( -4.522526758610270647, 7.433975764090723359, -1.199719254218453823 ) ) ;
#95568 = CARTESIAN_POINT ( 'NONE',  ( 6.569431593124095414, 6.790062804044275424, 0.3413723397009699734 ) ) ;
#95569 = CARTESIAN_POINT ( 'NONE',  ( 6.503279807981923177, 1.993766592317405051, 0.2985777636397292101 ) ) ;
#95570 = CARTESIAN_POINT ( 'NONE',  ( 5.859284738525260217, 1.813109059707292747, -0.3191327317438249489 ) ) ;
#95571 = CARTESIAN_POINT ( 'NONE',  ( 0.07680821025396293578, 0.7488618828427398011, -1.895266105024134839 ) ) ;
#95572 = CARTESIAN_POINT ( 'NONE',  ( 3.950101280099535650, 0.7789643570827823327, -2.172381230931414109 ) ) ;
#95573 = CARTESIAN_POINT ( 'NONE',  ( 5.692444392891300886, 7.734547439830227411, -1.599625672291281386 ) ) ;
#95574 = CARTESIAN_POINT ( 'NONE',  ( 5.940740243836844847, 0.4152237956781511530, 2.121177236311201586 ) ) ;
#95575 = CARTESIAN_POINT ( 'NONE',  ( 6.819914962873951936, 7.915321197229798322, -1.199719254218446718 ) ) ;
#95576 = CARTESIAN_POINT ( 'NONE',  ( 1.224054851709508451, 1.872146073007043610, 0.5162294149947727062 ) ) ;
#95577 = VERTEX_POINT ( 'NONE', #73437 ) ;
#95578 = EDGE_CURVE ( 'NONE', #205093, #126234, #78209, .T. ) ;
#95579 = CARTESIAN_POINT ( 'NONE',  ( 4.200743080572525656, -1.581147070632774598, -1.668312408496865684 ) ) ;
#95580 = CARTESIAN_POINT ( 'NONE',  ( 4.000000000000022204, 0.000000000000000000, 2.024999999999999023 ) ) ;
#95581 = CARTESIAN_POINT ( 'NONE',  ( -3.654804927335652209, 6.421633627603656080, 1.199719254218452935 ) ) ;
#95582 = CARTESIAN_POINT ( 'NONE',  ( 5.014452206985246185, 1.289541220462528504, -1.355370375751355105 ) ) ;
#95583 = VERTEX_POINT ( 'NONE', #125489 ) ;
#95586 = CARTESIAN_POINT ( 'NONE',  ( -4.990283058281743678, 7.979691447040783814, -1.199719254218453823 ) ) ;
#95585 = CARTESIAN_POINT ( 'NONE',  ( 1.499999999999989120, 0.05625000068281565957, 0.000000000000000000 ) ) ;
#95584 = CARTESIAN_POINT ( 'NONE',  ( 2.267699027020404490, 0.5063876334258295975, -1.844086191983687062 ) ) ;
#95587 = CARTESIAN_POINT ( 'NONE',  ( 3.580891165198408110, -2.126768340858419926, -0.5889919780145411732 ) ) ;
#95588 = CARTESIAN_POINT ( 'NONE',  ( 6.883263157960401557, 2.461427291499204362, 2.229941283862615808 ) ) ;
#95589 = DIRECTION ( 'NONE',  ( 0.7592566023653005702, -0.6507913734559639396, 0.000000000000000000 ) ) ;
#95590 = CARTESIAN_POINT ( 'NONE',  ( 5.790741006368192778, 8.809596036521288198, -1.082531754730548412 ) ) ;
#95591 = CARTESIAN_POINT ( 'NONE',  ( -4.796887421136680985, 4.490790167614548523, 1.214306433183764966E-14 ) ) ;
#95592 = CIRCLE ( 'NONE', #5680, 2.025000000000006573 ) ;
#95593 = CARTESIAN_POINT ( 'NONE',  ( -6.604230223188181093, 6.877559146573883453, 0.7216878364870317197 ) ) ;
#95594 = CARTESIAN_POINT ( 'NONE',  ( 2.020718154849282744, 1.838011538856450855, 0.7131330410372925810 ) ) ;
#95595 = CARTESIAN_POINT ( 'NONE',  ( 0.9214421848816763960, 2.133375822355741303, 0.8800392910873405805 ) ) ;
#95596 = CARTESIAN_POINT ( 'NONE',  ( 2.189831975649577878, -1.279155337443920404, -1.487614327915102841 ) ) ;
#95597 = CARTESIAN_POINT ( 'NONE',  ( -6.459533842268148973, 6.500820668926428958, 0.000000000000000000 ) ) ;
#95598 = CARTESIAN_POINT ( 'NONE',  ( 4.768458259026512103, -0.8772815012083650110, -1.866809563962401164 ) ) ;
#95599 = CARTESIAN_POINT ( 'NONE',  ( 5.992340707560163793, 6.093411701682730275, 0.7216878364870317197 ) ) ;
#95600 = CARTESIAN_POINT ( 'NONE',  ( 5.903649544107831382, 5.852288987739402870, -0.7998128361456481317 ) ) ;
#95601 = ORIENTED_EDGE ( 'NONE', *, *, #191572, .F. ) ;
#95602 = CARTESIAN_POINT ( 'NONE',  ( 1.364683531249992088, 5.696875000341418804, 1.214306433183764966E-14 ) ) ;
#95603 = CARTESIAN_POINT ( 'NONE',  ( -6.007394966791244961, 6.077829431809393945, -0.6506939885215150543 ) ) ;
#95604 = CARTESIAN_POINT ( 'NONE',  ( 8.211434591371064684, 12.73175745657494851, -0.7998128361456352531 ) ) ;
#95605 = CARTESIAN_POINT ( 'NONE',  ( 0.5323791783840629011, 1.248846938226945369, 1.775765033185220387 ) ) ;
#95606 = CARTESIAN_POINT ( 'NONE',  ( 6.391743074199809804, 6.421731439513382433, -0.7998128361456481317 ) ) ;
#95607 = CARTESIAN_POINT ( 'NONE',  ( 11.46094690312845898, 3.019799309332868553, -3.723887386306110159 ) ) ;
#95608 = CARTESIAN_POINT ( 'NONE',  ( -15.75000000000000000, 12.69999999999999929, -1.100000000000000311 ) ) ;
#95609 = CARTESIAN_POINT ( 'NONE',  ( 2.249088872875557144, -1.499603784168266563, -1.117866018216478574 ) ) ;
#95610 = CARTESIAN_POINT ( 'NONE',  ( 6.919229410208834530, -0.1638780278429008419, 2.126154539342207883 ) ) ;
#95612 = CARTESIAN_POINT ( 'NONE',  ( 6.827182134110227452, 2.468179810210658687, 2.195371296381436022 ) ) ;
#95611 = CARTESIAN_POINT ( 'NONE',  ( 0.07775346131141076811, 6.946779003630084048, -2.883989925229225815 ) ) ;
#95613 = CARTESIAN_POINT ( 'NONE',  ( -1.364683531250014514, -0.4697916663252449943, 0.7879004041258379498 ) ) ;
#95614 = CARTESIAN_POINT ( 'NONE',  ( 2.385291144485178982, 0.09204604084523881902, -1.910175020619097275 ) ) ;
#95615 = CARTESIAN_POINT ( 'NONE',  ( 3.924454612484959082, 1.680539001619888229, 0.5552615287828834845 ) ) ;
#95616 = CARTESIAN_POINT ( 'NONE',  ( 1.893074787327468700, -0.09523556418119562272, -1.910042277862213034 ) ) ;
#95617 = CARTESIAN_POINT ( 'NONE',  ( -5.229694566569281555, 7.124396299129368337, 1.599625672291267398 ) ) ;
#95619 = CARTESIAN_POINT ( 'NONE',  ( 5.976186790766067958, -1.906884764771042517, -0.1824196792480689000 ) ) ;
#95618 = DIRECTION ( 'NONE',  ( -0.8583236685137333177, -0.5131086435338296781, 0.000000000000000000 ) ) ;
#95620 = CARTESIAN_POINT ( 'NONE',  ( 6.320757381585181633, -1.393903556229304730, 1.391728847557841542 ) ) ;
#95621 = CARTESIAN_POINT ( 'NONE',  ( -1.500000000000011324, 5.129166666666691299, -0.8660254037844313801 ) ) ;
#95622 = CARTESIAN_POINT ( 'NONE',  ( 2.566775492539817627, 0.7186216927172992541, 1.995234744298620910 ) ) ;
#95623 = PRESENTATION_STYLE_ASSIGNMENT (( #29531 ) ) ;
#95624 = CARTESIAN_POINT ( 'NONE',  ( 5.242975984329111050, -1.603930480038592510, 0.9624218375651683033 ) ) ;
#95626 = VERTEX_POINT ( 'NONE', #188253 ) ;
#95625 = CARTESIAN_POINT ( 'NONE',  ( 1.699542765152612711, -0.6164703606487754728, 1.718597393154073671 ) ) ;
#95628 = CARTESIAN_POINT ( 'NONE',  ( 4.596293493935747598, 8.372084169494645067, 0.08663659024946840370 ) ) ;
#95627 = CARTESIAN_POINT ( 'NONE',  ( 5.110101661328442901, -2.196521081226535443, 0.2136625748923453583 ) ) ;
#95629 = CARTESIAN_POINT ( 'NONE',  ( 0.6823417656249864960, -0.5739583329919112353, -1.181850606188749264 ) ) ;
#95630 = CARTESIAN_POINT ( 'NONE',  ( 2.330602656244503468, -1.270745551583628785, 1.624662076113972065 ) ) ;
#95631 = CARTESIAN_POINT ( 'NONE',  ( 6.959412922516382771, 7.013736585890911535, 0.7998128361456341429 ) ) ;
#95632 = B_SPLINE_CURVE_WITH_KNOTS ( 'NONE', 3,
 ( #40238, #105250, #41319, #122643, #104174, #189669, #38102 ),
 .UNSPECIFIED., .F., .F.,
 ( 4, 3, 4 ),
 ( 1.399251010623063628E-17, 0.0008000000000005097218, 0.002977368225425562100 ),
 .UNSPECIFIED. ) ;
#95633 = CARTESIAN_POINT ( 'NONE',  ( -7.015454420067433361, 10.27211502579893754, 1.199719254218453823 ) ) ;
#95634 = CARTESIAN_POINT ( 'NONE',  ( 1.491588839496432728, 3.267857031437547466, -0.1769418395740485206 ) ) ;
#95635 = CARTESIAN_POINT ( 'NONE',  ( 1.000000000000001554, 6.468705557303653819, -4.925226524755053958 ) ) ;
#95636 = CARTESIAN_POINT ( 'NONE',  ( 6.343235766347262938, 8.493804042195527870, -1.599625672291281386 ) ) ;
#95637 = VERTEX_POINT ( 'NONE', #42044 ) ;
#95638 = CARTESIAN_POINT ( 'NONE',  ( 5.863751307568212390, -0.5067217619753560109, 2.007263066363853987 ) ) ;
#95639 = CARTESIAN_POINT ( 'NONE',  ( 0.6823417656249864960, -0.7614583329919113464, -1.181850606188749264 ) ) ;
#95640 = CARTESIAN_POINT ( 'NONE',  ( 2.249508738127777630, -1.734628566516350556, -1.289557925820798090 ) ) ;
#95641 = CARTESIAN_POINT ( 'NONE',  ( -4.606532530031762995, 8.380852375923623754, -0.1178885281021696541 ) ) ;
#95642 = CARTESIAN_POINT ( 'NONE',  ( 3.651039828637154372, 0.2984016815541118417, 1.997388552288078545 ) ) ;
#95643 = CARTESIAN_POINT ( 'NONE',  ( 6.720655732516665815, 7.629137130509056064, 2.773739711112707340 ) ) ;
#95644 = PRODUCT_DEFINITION_SHAPE ( 'NONE', 'NONE',  #214427 ) ;
#95645 = ORIENTED_EDGE ( 'NONE', *, *, #214139, .F. ) ;
#95647 = CARTESIAN_POINT ( 'NONE',  ( 7.619319141200070256, 8.951922421897323900, 1.082531754730558626 ) ) ;
#95646 = CARTESIAN_POINT ( 'NONE',  ( 3.475000000000000533, -0.5541666666666681396, 2.006292185433948827 ) ) ;
#95648 = CARTESIAN_POINT ( 'NONE',  ( -3.133342898089680695, 6.669667457830990465, 0.7216878364870338292 ) ) ;
#95649 = CARTESIAN_POINT ( 'NONE',  ( 1.903530124611974017, -1.954778955200174861, 0.4946342604733033887 ) ) ;
#95650 = CARTESIAN_POINT ( 'NONE',  ( 5.776942576169182608, 2.025397260235710206, -0.8375503648087383457 ) ) ;
#95651 =( BOUNDED_CURVE ( )  B_SPLINE_CURVE ( 2, ( #167074, #145536, #132476 ),
 .UNSPECIFIED., .F., .T. ) 
 B_SPLINE_CURVE_WITH_KNOTS ( ( 3, 3 ),
 ( 0.000000000000000000, 0.005017554178699702196 ),
 .UNSPECIFIED. ) 
 CURVE ( )  GEOMETRIC_REPRESENTATION_ITEM ( )  RATIONAL_B_SPLINE_CURVE ( ( 1.000000000000000000, 0.9193330245902806563, 0.9358062698725861939 ) ) 
 REPRESENTATION_ITEM ( '' )  );
#95652 = CARTESIAN_POINT ( 'NONE',  ( 1.499999999999990896, 4.306250000682819490, 1.214306433183764966E-14 ) ) ;
#95653 = CARTESIAN_POINT ( 'NONE',  ( 4.412309042748480792, -1.912102599942141268, -0.04143165621695726192 ) ) ;
#95654 = CARTESIAN_POINT ( 'NONE',  ( -4.925689880466507908, 4.641059703499347044, -0.7998128361456221525 ) ) ;
#95655 = CARTESIAN_POINT ( 'NONE',  ( 5.612712405933139692, 9.491988873656591608, 1.040834085586084257E-14 ) ) ;
#95657 = CARTESIAN_POINT ( 'NONE',  ( 2.232046197884657968, 2.016035414700023676, 0.04665772616015140262 ) ) ;
#95656 = CARTESIAN_POINT ( 'NONE',  ( -8.120970824461345217, 12.41829036193951730, 0.7216878364870458196 ) ) ;
#95658 = CARTESIAN_POINT ( 'NONE',  ( 1.364683531250000303, 14.31770833367473372, -0.7879004041258355073 ) ) ;
#95659 = CARTESIAN_POINT ( 'NONE',  ( -3.156015896931072540, 6.904045323053366268, 0.000000000000000000 ) ) ;
#95660 = CARTESIAN_POINT ( 'NONE',  ( 5.561458258421018819, 0.3325557151471290052, -1.692213012293216190 ) ) ;
#95661 = DIRECTION ( 'NONE',  ( 0.000000000000000000, 0.000000000000000000, 1.000000000000000000 ) ) ;
#95662 = CARTESIAN_POINT ( 'NONE',  ( 10.22248463502393001, 11.02857961705718282, 0.7216878364870438212 ) ) ;
#95663 = CARTESIAN_POINT ( 'NONE',  ( 4.192495815123822744, 5.914331089109666983, -1.599625672291255185 ) ) ;
#95664 = CARTESIAN_POINT ( 'NONE',  ( 11.96215121607992771, 9.771664462191758105, -0.9565349792967603459 ) ) ;
#95665 = CARTESIAN_POINT ( 'NONE',  ( 1.252880909328603964, -0.4992908342843912495, -2.009044966204868388 ) ) ;
#95666 = ORIENTED_EDGE ( 'NONE', *, *, #117363, .F. ) ;
#95667 = CARTESIAN_POINT ( 'NONE',  ( 4.652869415276386533, 0.3145016728411016982, 1.783790502623605834 ) ) ;
#95668 = CARTESIAN_POINT ( 'NONE',  ( 4.797606254389322089, 6.690569611577942943, 1.599625672291268286 ) ) ;
#95669 = CARTESIAN_POINT ( 'NONE',  ( 6.410821795378537580, -0.4906875946298261959, -1.743675775721682752 ) ) ;
#95670 = CARTESIAN_POINT ( 'NONE',  ( 4.041739190205284160, 7.729463131965888856, 0.000000000000000000 ) ) ;
#95671 = CARTESIAN_POINT ( 'NONE',  ( -0.6823417656249969321, 3.280208333674754062, -1.181850606188749264 ) ) ;
#95672 = CARTESIAN_POINT ( 'NONE',  ( 3.363397379774799134, 2.138023915923603635, -0.4802275100637617977 ) ) ;
#95673 = ORIENTED_EDGE ( 'NONE', *, *, #186210, .T. ) ;
#95675 = CARTESIAN_POINT ( 'NONE',  ( 8.890396042259068210, 11.39521468743417998, -1.599625672291257406 ) ) ;
#95674 = CARTESIAN_POINT ( 'NONE',  ( 0.3440982351944205653, -0.9282241650855774795, 1.728402704573737125 ) ) ;
#95676 = CARTESIAN_POINT ( 'NONE',  ( 5.079654255714375566, -0.6853159911496645718, 1.789018848640187231 ) ) ;
#95677 = CARTESIAN_POINT ( 'NONE',  ( -1.499999999999996003, 8.226475397238283804, 3.114076396432755800 ) ) ;
#95678 = DIRECTION ( 'NONE',  ( 0.000000000000000000, 0.000000000000000000, 1.000000000000000000 ) ) ;
#95679 = CARTESIAN_POINT ( 'NONE',  ( 0.6823417656249882723, 0.3427083336747516196, 1.181850606188755259 ) ) ;
#95681 = ORIENTED_EDGE ( 'NONE', *, *, #89791, .T. ) ;
#95680 = CARTESIAN_POINT ( 'NONE',  ( 4.026408433578586354, 7.641300905909586660, 1.040834085586084257E-14 ) ) ;
#95682 = CARTESIAN_POINT ( 'NONE',  ( -8.188761592974046266, 10.57664116326830595, -1.443375672974059665 ) ) ;
#95683 = CARTESIAN_POINT ( 'NONE',  ( 2.167066695894452888, -1.976221826324360720, -0.8764929760368762590 ) ) ;
#95684 = CARTESIAN_POINT ( 'NONE',  ( -5.483346782084204563, 5.361935765378481378, 0.000000000000000000 ) ) ;
#95685 = CARTESIAN_POINT ( 'NONE',  ( 3.715816618597135523, 6.492813934075403637, -1.199719254218453823 ) ) ;
#95686 = CARTESIAN_POINT ( 'NONE',  ( 2.239018641000252607, -1.631965468365924377, 0.8183158014263000046 ) ) ;
#95687 = CARTESIAN_POINT ( 'NONE',  ( -2.605138072120212200, 6.191078184115536232, -0.7998128361456281477 ) ) ;
#95688 = CARTESIAN_POINT ( 'NONE',  ( 4.243042751400435186, -1.588269943899191183, 0.8999137264355041577 ) ) ;
#95689 = CARTESIAN_POINT ( 'NONE',  ( 12.51849242037993371, 7.545148564283970849, -4.094730316256000258 ) ) ;
#95690 = ORIENTED_EDGE ( 'NONE', *, *, #60102, .T. ) ;
#95691 = CARTESIAN_POINT ( 'NONE',  ( 4.228926779721821738, -1.836881627057206590, -0.7110872907168819257 ) ) ;
#95692 = VERTEX_POINT ( 'NONE', #91867 ) ;
#95693 = CARTESIAN_POINT ( 'NONE',  ( 5.565949569975685129, -1.228723311412585950, 1.503964349303931192 ) ) ;
#95694 = EDGE_LOOP ( 'NONE', ( #66715, #22591, #149720, #199791 ) ) ;
#95695 = CARTESIAN_POINT ( 'NONE',  ( -6.394605727500880299, 7.489403432619674561, -1.199719254218452047 ) ) ;
#95697 = CARTESIAN_POINT ( 'NONE',  ( 5.484674493353773883, -1.343714522216314489, 1.640574901390474460 ) ) ;
#95696 = CARTESIAN_POINT ( 'NONE',  ( 5.559725510055676168, 8.644040974110419384, 1.199719254218451159 ) ) ;
#95699 = EDGE_CURVE ( 'NONE', #179471, #203057, #122297, .T. ) ;
#95698 = CARTESIAN_POINT ( 'NONE',  ( 6.983858524370782028, 8.280828045588322084, 1.082531754730549967 ) ) ;
#95700 = CARTESIAN_POINT ( 'NONE',  ( 3.229067839489424330, 1.729836904712976686, 0.8154208365811002057 ) ) ;
#95701 = CARTESIAN_POINT ( 'NONE',  ( 4.298292216229534723, 7.460037067547172107, -1.072071942351945584 ) ) ;
#95702 = CARTESIAN_POINT ( 'NONE',  ( 6.983263157960370116, 6.036630394911544073, 2.541087343977180613 ) ) ;
#95703 = EDGE_LOOP ( 'NONE', ( #126596, #100548, #45869, #185252 ) ) ;
#95704 = CARTESIAN_POINT ( 'NONE',  ( 3.054329744828568227, 6.785411478933790264, 0.000000000000000000 ) ) ;
#95705 = CARTESIAN_POINT ( 'NONE',  ( 5.004545975878083475, -1.998138528169653316, -0.2443019910301855169 ) ) ;
#95706 = CARTESIAN_POINT ( 'NONE',  ( -5.681296809623264110, 6.286896183989623133, -1.175774015649774462 ) ) ;
#95707 = CARTESIAN_POINT ( 'NONE',  ( 5.918537399722813674, 1.222626809077583587, -1.356019982345892050 ) ) ;
#95708 = CARTESIAN_POINT ( 'NONE',  ( 0.9946828900261883710, 2.039433816042154124, 0.3556643922909968891 ) ) ;
#95709 = CARTESIAN_POINT ( 'NONE',  ( -6.873620692448438874, 10.96304854125777695, 0.000000000000000000 ) ) ;
#95710 = VECTOR ( 'NONE', #122115, 1000.000000000000000 ) ;
#95711 = CARTESIAN_POINT ( 'NONE',  ( -6.005252172667468358, 7.091917859149008407, -1.064983193601161338 ) ) ;
#95712 = CARTESIAN_POINT ( 'NONE',  ( 0.000000000000000000, 8.500000000000000000, 0.000000000000000000 ) ) ;
#95713 = CARTESIAN_POINT ( 'NONE',  ( 1.642778471875001811, -2.792708332855376785, 2.845375778867859751 ) ) ;
#95714 = CARTESIAN_POINT ( 'NONE',  ( 6.100279051144945619, 9.204410428722734849, -1.199719254218440723 ) ) ;
#95715 = FACE_OUTER_BOUND ( 'NONE', #48237, .T. ) ;
#95716 = CIRCLE ( 'NONE', #2270, 0.5000000000000004441 ) ;
#95717 = CARTESIAN_POINT ( 'NONE',  ( -0.6823417656250003738, 10.21354166700806587, 1.181850606188754593 ) ) ;
#95718 = CARTESIAN_POINT ( 'NONE',  ( -4.517891501851816649, 6.293959390292322986, -1.599625672291256295 ) ) ;
#95720 = CARTESIAN_POINT ( 'NONE',  ( -6.084577077482911101, 10.32070003369722144, 0.000000000000000000 ) ) ;
#95719 = CARTESIAN_POINT ( 'NONE',  ( -11.97929049433705551, 11.29999999999999893, -0.7046979865771820783 ) ) ;
#95721 = CARTESIAN_POINT ( 'NONE',  ( 3.656634503061773067, 0.9670403524725273980, 1.439223064172075350 ) ) ;
#95722 = CARTESIAN_POINT ( 'NONE',  ( -3.958090780185743451, 6.705190779270287393, -1.199719254218452047 ) ) ;
#95723 = CARTESIAN_POINT ( 'NONE',  ( 1.164989683304976875, 1.570165760251106990, -1.349419213858449318 ) ) ;
#95724 = ADVANCED_FACE ( 'NONE', ( #138464 ), #126685, .F. ) ;
#95725 = CARTESIAN_POINT ( 'NONE',  ( 1.915762678288157383, -1.385565726045881130, -1.600959455242874974 ) ) ;
#95726 = CARTESIAN_POINT ( 'NONE',  ( 4.976006071415387311, 5.764094157194782575, 1.199719254218462483 ) ) ;
#95727 = CARTESIAN_POINT ( 'NONE',  ( 9.264299036839600987, 9.702770385934682551, -0.7998128361456281477 ) ) ;
#95728 = DIRECTION ( 'NONE',  ( 0.000000000000000000, -1.000000000000000000, 0.000000000000000000 ) ) ;
#95729 = CARTESIAN_POINT ( 'NONE',  ( 1.164831386079593134, 1.494809975433964100, -1.282432929305108438 ) ) ;
#95730 = CARTESIAN_POINT ( 'NONE',  ( 5.274334856052985465, 6.586744271544701768, 1.367809967355391398 ) ) ;
#95731 = CARTESIAN_POINT ( 'NONE',  ( 4.853455804012216213, 6.685451076146141425, 1.443375672974062551 ) ) ;
#95733 = FACE_OUTER_BOUND ( 'NONE', #101230, .T. ) ;
#95732 = CARTESIAN_POINT ( 'NONE',  ( 3.475000000000000533, -2.945833333333332416, -2.006292185433951047 ) ) ;
#95734 = CARTESIAN_POINT ( 'NONE',  ( 2.906493132324819761, 1.659771084382713369, -1.581246672503307638 ) ) ;
#95735 = CARTESIAN_POINT ( 'NONE',  ( 0.4514209555319322331, 0.5758240286459561652, -1.732582669633643047 ) ) ;
#95736 = CARTESIAN_POINT ( 'NONE',  ( 3.129067941553372645, 1.730785544086024696, 0.8136490247460312908 ) ) ;
#95737 = AXIS2_PLACEMENT_3D ( 'NONE', #69340, #37941, #187379 ) ;
#95738 = CARTESIAN_POINT ( 'NONE',  ( 7.205232291019763480, 7.370802192470005565, -0.7998128361456341429 ) ) ;
#95739 = CARTESIAN_POINT ( 'NONE',  ( 7.334597914868727919, 9.580116872145431728, -1.443375672974058777 ) ) ;
#95740 = CARTESIAN_POINT ( 'NONE',  ( 1.758066197707741640, 0.7666020408202559588, -1.861725765494412599 ) ) ;
#95741 = CARTESIAN_POINT ( 'NONE',  ( 1.604273143990111672, 1.959273547513197711, 0.1016356785708133759 ) ) ;
#95742 = CARTESIAN_POINT ( 'NONE',  ( -8.459397779922852578, 11.95671561229694824, 1.199719254218453823 ) ) ;
#95743 = CARTESIAN_POINT ( 'NONE',  ( -7.226659571283968297, 8.389856573708110332, 1.199719254218450271 ) ) ;
#95744 = CARTESIAN_POINT ( 'NONE',  ( -11.95450884322492158, 8.100199754937611019, 0.5427143782397774174 ) ) ;
#95746 = CARTESIAN_POINT ( 'NONE',  ( 3.836565602288672938, 0.2594712388852594143, 1.750573784680304890 ) ) ;
#95745 = CARTESIAN_POINT ( 'NONE',  ( 5.033190428309433528, -1.478027449723118725, -1.478843810762977995 ) ) ;
#95748 = CARTESIAN_POINT ( 'NONE',  ( 0.1292129718690297469, -2.001788180159810970, 0.8922102942980969509 ) ) ;
#95747 = DIRECTION ( 'NONE',  ( 0.000000000000000000, 1.000000000000000000, 0.000000000000000000 ) ) ;
#95749 = CARTESIAN_POINT ( 'NONE',  ( 4.980260712887213614, -0.2176769249225460612, -1.726585916463187376 ) ) ;
#95750 = CARTESIAN_POINT ( 'NONE',  ( 9.399880572976245574, 9.860948844760784482, 0.7998128361456462443 ) ) ;
#95751 = CARTESIAN_POINT ( 'NONE',  ( 7.461813752226484020, -6.074287852078599670, -6.844806938814754105 ) ) ;
#95752 = CARTESIAN_POINT ( 'NONE',  ( 4.885968428070557756, -0.08385511083567295798, 1.731956597358391470 ) ) ;
#95753 = CARTESIAN_POINT ( 'NONE',  ( 4.949771893170417769, 1.605651206033286815, 1.461634471724428064 ) ) ;
#95754 = CARTESIAN_POINT ( 'NONE',  ( 3.684065054611349144, 5.321161868511784299, -1.599625672291262513 ) ) ;
#95755 = CARTESIAN_POINT ( 'NONE',  ( 6.034388706570055660, 0.6371486477873434806, 1.913263546360920220 ) ) ;
#95756 = CARTESIAN_POINT ( 'NONE',  ( 5.562500000000004441, -1.451031289061337937, -1.451031289060889851 ) ) ;
#95757 = CARTESIAN_POINT ( 'NONE',  ( -1.500000000000011324, 5.202083334016151639, 0.8660254037844403729 ) ) ;
#95758 = CARTESIAN_POINT ( 'NONE',  ( 3.487250860276095210, 1.742034520097140771, -0.8226350277544016709 ) ) ;
#95759 = CARTESIAN_POINT ( 'NONE',  ( -1.500000000000001110, 10.05208333401613174, 0.8660254037844419273 ) ) ;
#95760 = CARTESIAN_POINT ( 'NONE',  ( 0.4873737393681918384, -2.093643541511390538, -0.7425801828774351021 ) ) ;
#95761 = EDGE_LOOP ( 'NONE', ( #26386, #163150, #31522, #153611 ) ) ;
#95762 = CARTESIAN_POINT ( 'NONE',  ( 6.983263157960401202, 2.460233018525457727, 2.229759568558951965 ) ) ;
#95763 = CARTESIAN_POINT ( 'NONE',  ( -1.201851678989727383E-14, 2.462500000000023004, 1.732050807568877637 ) ) ;
#95764 = CARTESIAN_POINT ( 'NONE',  ( 4.313465427442102929, 8.184126765324453601, 0.7998128361456462443 ) ) ;
#95765 = CARTESIAN_POINT ( 'NONE',  ( 2.754761814426693434, 2.204812966250285999, 0.2695357242936818332 ) ) ;
#95766 = CARTESIAN_POINT ( 'NONE',  ( 6.478960399985357554, 1.830089090633261417, 0.7073212282268787066 ) ) ;
#95767 = CARTESIAN_POINT ( 'NONE',  ( 6.629573927402440781, 10.67832731537079383, 1.040834085586084257E-14 ) ) ;
#95768 = CARTESIAN_POINT ( 'NONE',  ( -9.693716643646601128, 12.33242205571964512, 1.443375672974076540 ) ) ;
#95769 = CARTESIAN_POINT ( 'NONE',  ( 3.203469434578891661, 6.959407783642502565, -0.7998128361456362523 ) ) ;
#95770 = CARTESIAN_POINT ( 'NONE',  ( -3.201133666602369310, 6.748756687762456963, -0.7216878364870458196 ) ) ;
#95772 = CARTESIAN_POINT ( 'NONE',  ( 5.723111435942265679, -1.863175293877845418, -0.8853075346121098699 ) ) ;
#95771 = CARTESIAN_POINT ( 'NONE',  ( 8.866142388332804103, 12.43125098877526113, -1.199719254218446718 ) ) ;
#95773 = DIRECTION ( 'NONE',  ( 0.000000000000000000, 0.000000000000000000, -1.000000000000000000 ) ) ;
#95774 = CARTESIAN_POINT ( 'NONE',  ( -4.790108344329849110, 4.482881244673243337, 0.7998128361456341429 ) ) ;
#95775 = CARTESIAN_POINT ( 'NONE',  ( 0.6823417656249882723, 0.6760416670080898749, -1.181850606188749264 ) ) ;
#95777 = B_SPLINE_CURVE_WITH_KNOTS ( 'NONE', 3,
 ( #13936, #80019, #146122, #63771, #130980, #129930, #214242, #195918, #47555, #179670, #31290, #97365, #163423, #14999, #196971, #48608, #180723, #156513, #37405, #90445, #56863, #187913, #103479, #7015, #88304, #123037, #24337, #39543, #181772, #87227, #188988, #875, #120875, #99484, #40632, #4867, #55790, #155429, #105644, #169541, #21121, #38481, #73090, #153291, #119791, #66940, #89380, #17135, #165542, #115783, #172762, #171671, #186849, #140284, #70945, #185772, #137056, #203081, #54726, #33405, #104558, #8102, #83211, #74192, #22189, #53659, #139191, #49660, #170602, #135986, #202000, #154366, #106735, #5944, #72015, #138128, #149294, #23268, #204137, #121947, #205221, #193263, #28640, #13440, #26489, #141365, #45974, #175968, #44910, #111018, #174911, #57928, #191113, #192180, #173843, #25420, #43841, #92599, #27562, #161852, #124093, #160772, #208429, #94727, #76313, #112095, #177023, #190056, #79517, #42780, #158641, #109957, #91526, #10238, #126219, #93658, #78444, #207378, #142420, #143495, #12365, #77379, #209491, #41708, #206304, #60063, #61132, #107818, #157584, #9177, #125154, #178097, #144564, #159701, #210574, #11300, #29714, #62208, #75252, #58998, #108888, #127292, #128365, #194332, #95795, #147728, #167170, #162913, #145635, #49162, #100032, #149861, #98975, #115279, #211631, #213745, #15556, #146683, #80585, #182327, #47041, #212699, #32897, #96865, #179162, #17682, #50218, #30786, #33956, #101081, #197518, #199639, #196472, #166094, #133638, #165027, #18757, #16621, #81643, #65368, #117410, #183406, #66425, #63266, #180224, #1429, #14495, #131515, #195412, #51285, #97923, #148782, #83768, #132568, #48114, #114226, #64340, #31846, #129428, #130482, #163981, #67493, #113157, #181271, #82703, #35010, #198569, #352, #116337, #69634, #168231, #151987, #135742, #3561, #2492, #201764, #118477, #136807, #105390, #169293, #84842, #137882, #171429, #53405, #184462, #102163, #119543, #55548, #202833, #86977, #103233, #68567, #104304, #36080, #38230, #19828, #154119, #121702, #85913, #185528, #37154, #39296, #4622, #170353, #21938, #20878, #150931, #153047, #70694, #134694, #54482, #89134, #120627, #203902, #23017, #88048, #200698, #5689, #186603, #71766, #52350, #187666, #155188, #196107, #98602, #68193, #15191, #132199, #113859, #51981, #16245, #67125, #166795, #50909, #114906, #180903, #81282, #32527, #47743, #131161, #197152, #100718, #31477, #179854, #130117, #184091, #199265, #198206, #151619, #164663, #48789, #82331, #148423, #73002, #97552, #66055, #147358, #17315, #35710, #49841, #63962, #150558, #101787, #115969, #213385, #65009, #181957, #134325, #165727, #33586, #99658, #163610, #117037, #83393, #133258, #149477, #18389, #200331, #1060, #183032, #34648, #84466, #2118, #118106, #167856, #19453, #85529, #3178, #54101, #184084, #202445, #35702, #185138, #171037, #67117, #167846, #34641, #133250, #55167, #21554, #4243, #199256, #22634, #51974, #19446, #119155, #183025, #85523, #135366, #102851, #38913, #18381, #1052, #36765, #169968, #5302, #168906, #20510, #50902, #69249, #151609, #86595, #100712, #166787, #121312, #2111, #152661, #84459, #150549, #87664, #120237, #68185, #103924, #101778, #104997, #117028, #187286, #70314, #134316, #153734, #88744, #136430, #186213, #201382, #37845, #200324, #53022 ),
 .UNSPECIFIED., .F., .F.,
 ( 4, 1, 1, 1, 1, 1, 1, 1, 1, 1, 1, 1, 1, 1, 1, 1, 1, 1, 1, 1, 1, 1, 1, 1, 1, 1, 1, 1, 1, 1, 1, 1, 1, 1, 1, 1, 1, 1, 1, 1, 1, 1, 1, 1, 1, 1, 1, 1, 1, 1, 1, 1, 1, 1, 1, 1, 1, 1, 1, 1, 1, 1, 1, 1, 1, 1, 1, 1, 1, 1, 1, 1, 1, 1, 1, 1, 1, 1, 1, 1, 1, 1, 1, 1, 1, 1, 1, 1, 1, 1, 1, 1, 1, 1, 1, 1, 1, 1, 1, 1, 1, 1, 1, 1, 1, 1, 1, 1, 1, 1, 1, 1, 1, 1, 1, 1, 1, 1, 1, 1, 1, 1, 1, 1, 1, 1, 1, 1, 1, 1, 1, 1, 1, 1, 1, 1, 1, 1, 1, 1, 1, 1, 1, 1, 1, 1, 1, 1, 1, 1, 1, 1, 1, 1, 1, 1, 1, 1, 1, 1, 1, 1, 1, 1, 1, 1, 1, 1, 1, 1, 1, 1, 1, 1, 1, 1, 1, 1, 1, 1, 1, 1, 1, 1, 1, 1, 1, 1, 1, 1, 1, 1, 1, 1, 1, 1, 1, 1, 1, 1, 1, 1, 1, 1, 1, 1, 1, 1, 1, 1, 1, 1, 1, 1, 1, 1, 1, 1, 1, 1, 1, 1, 1, 1, 1, 1, 1, 1, 1, 1, 1, 1, 1, 1, 1, 1, 1, 1, 1, 1, 1, 1, 1, 1, 1, 1, 1, 1, 1, 1, 1, 1, 1, 1, 1, 1, 1, 1, 1, 1, 1, 1, 1, 1, 1, 1, 1, 1, 1, 1, 1, 1, 1, 1, 1, 1, 1, 1, 1, 1, 1, 1, 1, 1, 1, 1, 1, 1, 1, 1, 1, 1, 1, 1, 1, 1, 1, 1, 1, 1, 1, 1, 1, 1, 1, 1, 1, 1, 1, 1, 1, 1, 1, 1, 1, 1, 1, 1, 1, 1, 1, 1, 1, 1, 1, 1, 1, 1, 1, 1, 1, 1, 1, 1, 1, 1, 1, 1, 1, 1, 1, 1, 1, 1, 1, 1, 1, 1, 1, 1, 1, 1, 1, 1, 1, 1, 1, 1, 1, 1, 1, 1, 1, 1, 1, 1, 1, 1, 1, 1, 1, 1, 1, 1, 1, 1, 1, 1, 1, 1, 1, 1, 1, 1, 4 ),
 ( 0.000000000000000000, 0.002599942752653872004, 0.005208763852970823248, 0.007813103504395044890, 0.01041666580238601383, 0.01302040446826325734, 0.01562503794709516405, 0.01822898659850798186, 0.02083325479626091381, 0.02343751936515397344, 0.02604147156932860516, 0.02864593660736421826, 0.03124971754428982826, 0.03385421962853985695, 0.03645805019290717514, 0.03906245553539786086, 0.04166655880408994678, 0.04427067902208449424, 0.04687506736766395427, 0.04947890482860387018, 0.05208340383233839299, 0.05468718329397467132, 0.05729165635893663372, 0.05989559287350183087, 0.06249988401580178210, 0.06510415622071820396, 0.06770810475871495704, 0.07031256650665723695, 0.07291634835701975292, 0.07552085129243907291, 0.07812468146351797538, 0.08072908640827750060, 0.08333318980393969455, 0.08593730989448074287, 0.08854169822802662737, 0.09114553558425014801, 0.09375003453682481669, 0.09635381396055957282, 0.09895828689139142542, 0.1015622234206122604, 0.1041665143989399522, 0.1067707866525781646, 0.1093747350801187734, 0.1119791968332524285, 0.1145829786367304204, 0.1171874814968899975, 0.1197913116783300008, 0.1223957164865987768, 0.1249998199429257079, 0.1276039399106482508, 0.1302083283009266290, 0.1328121656006459317, 0.1354166645410730119, 0.1380204439687620910, 0.1406249168095159707, 0.1432288533966223909, 0.1458331442541831724, 0.1484374165996726891, 0.1510413649597071029, 0.1536458267615184170, 0.1562496085608837959, 0.1588541113892728840, 0.1614579416238982879, 0.1640623463390579739, 0.1666664498991252963, 0.1692705697871219883, 0.1718749582774928841, 0.1744787955635339893, 0.1770832945353020271, 0.1796870740097127606, 0.1822915468038420750, 0.1848954834917516388, 0.1874997742717963711, 0.1901040467523684718, 0.1927079950878241021, 0.1953124569817516476, 0.1979162388197689970, 0.2005207416598733527, 0.2031245719904950509, 0.2057289766559125821, 0.2083330803627857220, 0.2109372002141371993, 0.2135415888479497148, 0.2161454261631269858, 0.2187499252097131475, 0.2213537047736018060, 0.2239581775645482220, 0.2265621143961681627, 0.2291664051419355919, 0.2317706778008114532, 0.2343746261546043874, 0.2369790881840763974, 0.2395828701034999064, 0.2421873729987945312, 0.2447912034682135918, 0.2473956081272447038, 0.2499997120239797754, 0.2526038318817556694, 0.2552082207023498306, 0.2578120580894675551, 0.2604165572543392093, 0.2630203369504529598, 0.2656248097816475973, 0.2682287467998764607, 0.2708330375545950908, 0.2734373104349877015, 0.2760412588500244513, 0.2786457210584605826, 0.2812495031020356140, 0.2838540060959860445, 0.2864578367469951536, 0.2890622414429859233, 0.2916663455726313803, 0.2942704654798921071, 0.2968748545306000852, 0.2994786920324540302, 0.3020831913590704687, 0.3046869712301484290, 0.3072914441450140810, 0.3098953813927431966, 0.3124996721996327054, 0.3151039453447485039, 0.3177078938639273376, 0.3203123562947402525, 0.3229161385052047861, 0.3255206416412691484, 0.3281244725166545528, 0.3307288772929431464, 0.3333329816985414751, 0.3359371016983396796, 0.3385414910224879836, 0.3411453286818670882, 0.3437498282136811634, 0.3463536083024566503, 0.3489580813444087548, 0.3515620188645239841, 0.3541663097667969717, 0.3567705832198370119, 0.3593745318860498972, 0.3619789945826469846, 0.3645827770027332826, 0.3671872803243637073, 0.3697911114669067967, 0.3723955163668249413, 0.3749996210914142147, 0.3776037412267966853, 0.3802081308677072724, 0.3828119687273952576, 0.3854164685078552144, 0.3880202488570567709, 0.3906247220695055478, 0.3932286599048890885, 0.3958329509457525486, 0.3984372247499146091, 0.4010411736060487398, 0.4036456366118335581, 0.4062494192842699414, 0.4088539228349143406, 0.4114577542873927851, 0.4140621593542673784, 0.4166662644408827831, 0.4192703847548917562, 0.4218747747558840855, 0.4244786128586610641, 0.4270831129312115948, 0.4296868935835649328, 0.4322913670099168826, 0.4348953052034483235, 0.4374995964261053638, 0.4401038706245853915, 0.4427078197135246862, 0.4453122830718987402, 0.4479160660394111426, 0.4505205698625146526, 0.4531244016677045128, 0.4557288069448597878, 0.4583329124365353446, 0.4609370329722101700, 0.4635414233766025904, 0.4661452617652466213, 0.4687497621733308639, 0.4713535431715604185, 0.4739580168552197104, 0.4765619554497781962, 0.4791662468974299260, 0.4817705215334236457, 0.4843744708980504132, 0.4869789346524148743, 0.4895827179577280641, 0.4921872220967347111, 0.4947910542974118808, 0.4973954598281701278, 0.4999995657679404681, 0.5026036865683194410, 0.5052080774194306345, 0.5078119161367193879, 0.5104164169237808135, 0.5130201983106112973, 0.5156246722949818784, 0.5182286113334474420, 0.5208329030492938605, 0.5234371781659985512, 0.5260411278491948783, 0.5286455920429519173, 0.5312493757287917173, 0.5338538802271461936, 0.5364577128660878991, 0.5390621186937718523, 0.5416662251246735504, 0.5442703462327953545, 0.5468747375739465566, 0.5494785766626585355, 0.5520830778721422805, 0.5546868596903002935, 0.5572913340187868325, 0.5598952735440421158, 0.5624995655712847764, 0.5651038412119004928, 0.5677077912565504647, 0.5703122559331050834, 0.5729160400421993149, 0.5755205449433484777, 0.5781243780633351648, 0.5807287842312690573, 0.5833328911963423513, 0.5859370126552478908, 0.5885414045297637786, 0.5911452440326808722, 0.5937497457080352925, 0.5963535280002507655, 0.5989580027162609843, 0.6015619427711926814, 0.6041662351530351360, 0.6067705113607667622, 0.6093744618097575172, 0.6119789270125192138, 0.6145827115875999169, 0.6171872169349945647, 0.6197910505788110092, 0.6223954571303226269, 0.6249995646726131948, 0.6276036865253464825, 0.6302080789765573954, 0.6328119189364656005, 0.6354164211211439373, 0.6380202039301521300, 0.6406246790770983024, 0.6432286197045988807, 0.6458329124842493441, 0.6484371893023079814, 0.6510411401985315427, 0.6536456059709156996, 0.6562493910547204656, 0.6588538968918166150, 0.6614577311022542538, 0.6640621380806766005, 0.6666662462432366709, 0.6692703685328477148, 0.6718747616040910975, 0.6744786020637821844, 0.6770831048012443398, 0.6796868881697873954, 0.6822913637910873463, 0.6848953050340567117, 0.6874995982547292828, 0.6901038757263339152, 0.6927078271126885234, 0.6953122934981186276, 0.6979160791333920422, 0.7005205855036529261, 0.7031244203235108570, 0.7057288277721832648, 0.7083329365980738368, 0.7109370593676189731, 0.7135414531022405971, 0.7161452941045143294, 0.7187497974382286436, 0.7213535814090563658, 0.7239580575481356917, 0.7265619994494829648, 0.7291662931543987369, 0.7317705713227778963, 0.7343745232421703406, 0.7369789902840787610, 0.7395827765135741805, 0.7421872834604720248, 0.7447911189325585601, 0.7473955268948287989, 0.7499996364271210858, 0.7526037597196653106, 0.7552081541610216053, 0.7578119957486867397, 0.7604164997221309896, 0.7630202843380037292, 0.7656247610382975743, 0.7682287036409420899, 0.7708329978733315935, 0.7734372767817252470, 0.7760412292770711984, 0.7786456970189011839, 0.7812494838853828449, 0.7838539914523996455, 0.7864578276195345330, 0.7890622361387605865, 0.7916663464205372369, 0.7942704702791556493, 0.7968748654706151457, 0.7994787076864910969, 0.8020832123431549388, 0.8046869976468442598, 0.8072914749517984268, 0.8098954182986718431, 0.8124997131017763774, 0.8151039927934364826, 0.8177079459076636025, 0.8203124143928716139, 0.8229162019391148553, 0.8255207101697450423, 0.8281245470747605752, 0.8307289561943111966, 0.8333330672686687368, 0.8359371917364484261, 0.8385415877213925340, 0.8411454306083117061, 0.8437499359916976749, 0.8463537220259882421, 0.8489581999790609679, 0.8515621441131088210, 0.8541664395301816759, 0.8567707200483754004, 0.8593746738244238959, 0.8619791430964799384, 0.8645829313652741988, 0.8671874403030259693, 0.8697912779887684298, 0.8723956877520262498, 0.8749997996620757501, 0.8776039247821166844, 0.8802083216039426894, 0.8828121652047509205, 0.8854166713583762061, 0.8880204581660676721, 0.8906249368107317377, 0.8932288817749149956, 0.8958331778492237829, 0.8984374592372342816, 0.9010414137180589034, 0.9036458838204490807, 0.9062496728545991198, 0.9088541825429954368, 0.9114580210523274273, 0.9140624315026897317, 0.9166665442915585826, 0.9192706701069754960, 0.9218750678090992245, 0.9244789121666602272, 0.9270834191340497910, 0.9296872067579531329, 0.9322916861377325004, 0.9348956319750387767, 0.9374999287497546296, 0.9401042110508202043, 0.9427081662796877870, 0.9453126372565492375, 0.9479164270979697493, 0.9505209375757615042, 0.9531247769568838013, 0.9557291881641908349, 0.9583333018366511080, 0.9609374282806871781, 0.9635418271385329803, 0.9661456726567504427, 0.9687501794391485399, 0.9713539669241311181, 0.9739584505366999378, 0.9765624007674321705, 0.9791666904763859369, 0.9817709514985233366, 0.9843749191276834898, 0.9869795472165283634, 0.9895832986789295793, 0.9921868791097946394, 0.9947912178632822844, 0.9974000636350187632, 1.000000000000000000 ),
 .UNSPECIFIED. ) ;
#95776 = CARTESIAN_POINT ( 'NONE',  ( 6.696569769017397533, -0.4992639023812006638, -1.802638941973549569 ) ) ;
#95778 = CARTESIAN_POINT ( 'NONE',  ( 6.399014502872731214, -0.8263350558326795214, -1.524632933908439902 ) ) ;
#95779 = CARTESIAN_POINT ( 'NONE',  ( 5.460439331044164568, -1.576930981450849867, -0.7368137880037448628 ) ) ;
#95780 = CARTESIAN_POINT ( 'NONE',  ( 3.263489799031735750, 2.236134436263835568, -0.5039766086074470852 ) ) ;
#95781 = CARTESIAN_POINT ( 'NONE',  ( 1.364683531249988535, 5.717708333674752730, -0.7879004041258300672 ) ) ;
#95782 = CARTESIAN_POINT ( 'NONE',  ( 0.7789528443887736575, 1.234723402293058214, 1.365900241759879119 ) ) ;
#95783 = PLANE ( 'NONE',  #143491 ) ;
#95784 = CARTESIAN_POINT ( 'NONE',  ( -9.604686356149276349, 3.999999999999997335, 7.193747284969079558 ) ) ;
#95785 = CARTESIAN_POINT ( 'NONE',  ( 2.414841169274529520, 1.629557050654990791, 0.8231356554938076275 ) ) ;
#95786 = CARTESIAN_POINT ( 'NONE',  ( 2.654922836763852878, 1.081066371885472277, 1.701947380796410059 ) ) ;
#95787 = CARTESIAN_POINT ( 'NONE',  ( 0.6916816545035618935, -0.7852976098030055585, 2.046091368998310678 ) ) ;
#95788 = CARTESIAN_POINT ( 'NONE',  ( 9.796344284928359514, 14.76695548050556894, -7.811462394769543849 ) ) ;
#95789 = CARTESIAN_POINT ( 'NONE',  ( 4.665121749186112332, -1.880042215448823661, -0.9491155671061396459 ) ) ;
#95790 = CARTESIAN_POINT ( 'NONE',  ( -6.551614543901706611, 8.666636272683888365, 1.599625672291283607 ) ) ;
#95791 = CARTESIAN_POINT ( 'NONE',  ( 8.296867357720381975, 13.24864518393002832, 8.548329535528976564 ) ) ;
#95792 = CARTESIAN_POINT ( 'NONE',  ( 1.522023487246677798, 2.040062638832959241, -0.3519594530456415793 ) ) ;
#95793 = CARTESIAN_POINT ( 'NONE',  ( 3.845709127770629010, 7.638411082374393146, 0.7998128361456321445 ) ) ;
#95794 = CARTESIAN_POINT ( 'NONE',  ( -0.6801582343750403048, -0.5364583329919083710, 1.178068619123807004 ) ) ;
#95795 = CARTESIAN_POINT ( 'NONE',  ( 4.125719030757846184, -0.3612518283466863434, 2.089324717668067599 ) ) ;
#95796 = CIRCLE ( 'NONE', #43843, 11.89429233241351902 ) ;
#95797 = CARTESIAN_POINT ( 'NONE',  ( 6.182242880246401562, -0.9723386526096773341, 1.545037271442825100 ) ) ;
#95798 = ORIENTED_EDGE ( 'NONE', *, *, #125182, .T. ) ;
#95799 = CARTESIAN_POINT ( 'NONE',  ( -6.317173229324657413, 6.334733287159020954, 0.000000000000000000 ) ) ;
#95800 = CARTESIAN_POINT ( 'NONE',  ( -11.33772463945037146, 11.00902469614650236, -3.600000000000000977 ) ) ;
#95801 = CARTESIAN_POINT ( 'NONE',  ( 6.997416677984476863, 7.336276677169590421, 0.000000000000000000 ) ) ;
#95802 = CARTESIAN_POINT ( 'NONE',  ( -1.737499999999997824, -2.347916665710752415, 3.009438278150925683 ) ) ;
#95803 = CARTESIAN_POINT ( 'NONE',  ( -4.608882153641705059, 7.464447381635583412, -1.199719254218452047 ) ) ;
#95804 = CARTESIAN_POINT ( 'NONE',  ( 6.328397690248316110, -1.000878058022572903, -1.869571840794107986 ) ) ;
#95805 = CARTESIAN_POINT ( 'NONE',  ( 0.8507726699197988296, 0.6114878368043925594, 2.015236747771311343 ) ) ;
#95806 = CARTESIAN_POINT ( 'NONE',  ( -5.818384198920079520, 6.817144982608731141, 1.199719254218452935 ) ) ;
#95807 = CARTESIAN_POINT ( 'NONE',  ( 7.944187942603509356, 11.35563746875774882, 1.199719254218460707 ) ) ;
#95808 = CARTESIAN_POINT ( 'NONE',  ( 4.908966729185230804, -1.496192014157717631, 1.106395937811145203 ) ) ;
#95809 = CARTESIAN_POINT ( 'NONE',  ( 6.916630921265960019, 11.22115317478565188, 0.7998128361456462443 ) ) ;
#95810 = CARTESIAN_POINT ( 'NONE',  ( -5.000000000000009770, 3.850000000000006306, 0.5000000000000064393 ) ) ;
#95811 = CARTESIAN_POINT ( 'NONE',  ( -5.144392941742557568, 4.966489618313220333, -0.7998128361456362523 ) ) ;
#95812 = CARTESIAN_POINT ( 'NONE',  ( -9.408995418203979000, 12.00024729270324286, 1.443375672974076540 ) ) ;
#95814 = CARTESIAN_POINT ( 'NONE',  ( 2.312880826517309085, -1.518475810973318074, 1.242258525517292433 ) ) ;
#95813 = CARTESIAN_POINT ( 'NONE',  ( -7.019370843573183194, 9.212351955633947043, 1.599625672291283607 ) ) ;
#95815 = CARTESIAN_POINT ( 'NONE',  ( 0.9542513359644848592, 2.159166806557303531, -0.1069676271590186134 ) ) ;
#95817 = CARTESIAN_POINT ( 'NONE',  ( -5.609631208091558463, 6.340496262503443781, 1.197921296376257994 ) ) ;
#95816 = CARTESIAN_POINT ( 'NONE',  ( -4.990283058281743678, 7.979691447040783814, -1.199719254218453823 ) ) ;
#95818 = CARTESIAN_POINT ( 'NONE',  ( -1.364683531250014514, -0.2614583329919080157, -0.7879004041258359514 ) ) ;
#95819 = CARTESIAN_POINT ( 'NONE',  ( 3.338897068646465627, -1.034916488738941709, 1.390885369450091336 ) ) ;
#95820 = CARTESIAN_POINT ( 'NONE',  ( 2.554330413957212276, -1.514043700042773111, -0.8579764065595529843 ) ) ;
#95821 = CARTESIAN_POINT ( 'NONE',  ( 6.588899466561449536, 9.670504563421618016, -1.082531754730537088 ) ) ;
#95822 = CARTESIAN_POINT ( 'NONE',  ( -11.82816107619417778, 7.167718870070345361, 1.885585305228718589 ) ) ;
#95823 = CARTESIAN_POINT ( 'NONE',  ( 2.829428133295128323, -1.924058217741884125, 0.7386292696346643538 ) ) ;
#95824 = EDGE_CURVE ( 'NONE', #124513, #45649, #184616, .T. ) ;
#95825 = AXIS2_PLACEMENT_3D ( 'NONE', #122496, #142954, #159161 ) ;
#95826 = CARTESIAN_POINT ( 'NONE',  ( 1.475935241056694602, 1.776738309990203213, 0.9528675108748105860 ) ) ;
#95827 = CARTESIAN_POINT ( 'NONE',  ( 6.825078400183548055, -0.008500281443135982926, 2.244262395727573356 ) ) ;
#95828 = CARTESIAN_POINT ( 'NONE',  ( -3.634467696915153034, 6.397906858779740524, 1.199719254218452935 ) ) ;
#95829 = CARTESIAN_POINT ( 'NONE',  ( 1.586731204520151151, -0.2873679327500404668, -1.950290023627434755 ) ) ;
#95830 = AXIS2_PLACEMENT_3D ( 'NONE', #5341, #3221, #184123 ) ;
#95832 = CARTESIAN_POINT ( 'NONE',  ( -4.977251789992602760, 8.820894498384422633, 0.000000000000000000 ) ) ;
#95831 = CARTESIAN_POINT ( 'NONE',  ( 5.765855477156511810, 0.5488314196105298359, -1.831976909803390896 ) ) ;
#95833 = CARTESIAN_POINT ( 'NONE',  ( -5.926322542504864899, 8.967774495347393682, -1.082531754730549967 ) ) ;
#95834 = CARTESIAN_POINT ( 'NONE',  ( 8.174640274396848483, 8.501778173076651512, 0.7998128361456291469 ) ) ;
#95835 = ADVANCED_FACE ( 'NONE', ( #89727 ), #44170, .F. ) ;
#95836 = CARTESIAN_POINT ( 'NONE',  ( -6.257970421159510188, 9.458660037064859694, 1.199719254218452047 ) ) ;
#95837 = CARTESIAN_POINT ( 'NONE',  ( 0.8209702097039422997, 1.527776094787479444, -1.321057435245088341 ) ) ;
#95838 = FACE_OUTER_BOUND ( 'NONE', #155577, .T. ) ;
#95839 = CARTESIAN_POINT ( 'NONE',  ( 4.770747201329826659, -1.511217855519477293, 1.743977600800976857 ) ) ;
#95840 = CARTESIAN_POINT ( 'NONE',  ( 6.320756440275016708, -1.388331291134708767, 1.386421665916007795 ) ) ;
#95841 = CARTESIAN_POINT ( 'NONE',  ( 1.990992145637654698, 0.1870960246039363450, 1.952785824368876710 ) ) ;
#95842 = CARTESIAN_POINT ( 'NONE',  ( 9.236128959407556849, 11.79856975744075598, -1.599625672291262513 ) ) ;
#95843 = CARTESIAN_POINT ( 'NONE',  ( -9.523545777995696682, 15.37723649748560284, 7.300907475062111907 ) ) ;
#95844 = EDGE_LOOP ( 'NONE', ( #173067, #24232, #211941, #192750 ) ) ;
#95845 = CARTESIAN_POINT ( 'NONE',  ( 1.376322447316252306, -2.107681897322019271, -0.2017570171880012919 ) ) ;
#95847 = CARTESIAN_POINT ( 'NONE',  ( -7.640183256500752584, 8.872300873127729304, -1.199719254218446718 ) ) ;
#95846 = CARTESIAN_POINT ( 'NONE',  ( -3.249150368769345043, 6.942425863539538611, 0.7998128361456341429 ) ) ;
#95848 = CARTESIAN_POINT ( 'NONE',  ( 0.4097734724025984820, 1.271762808003698009, -1.331557029818277060 ) ) ;
#95849 = ORIENTED_EDGE ( 'NONE', *, *, #90474, .F. ) ;
#95850 = CARTESIAN_POINT ( 'NONE',  ( 4.715793416201278454, 0.4818634375548909166, -2.116767182733831021 ) ) ;
#95851 = CARTESIAN_POINT ( 'NONE',  ( 11.28150220813606452, 8.887219049998511977, 4.094115087793253061 ) ) ;
#95852 = CARTESIAN_POINT ( 'NONE',  ( 3.480829117359967917, -1.421471314662653196, 1.573842340227212366 ) ) ;
#95853 = CARTESIAN_POINT ( 'NONE',  ( 0.7499999999999920064, 4.014583334016149863, 1.299038105676669330 ) ) ;
#95854 = CARTESIAN_POINT ( 'NONE',  ( 8.751951852821344247, 10.16936423550178503, -1.199719254218446718 ) ) ;
#95855 =( NAMED_UNIT ( * ) PLANE_ANGLE_UNIT ( ) SI_UNIT ( $, .RADIAN. ) );
#95856 = CARTESIAN_POINT ( 'NONE',  ( 3.374343653733542059, -1.230474546199412877, 1.652924668896506688 ) ) ;
#95858 = CARTESIAN_POINT ( 'NONE',  ( 0.3800845246329161431, -0.2246070939678334044, -1.827447590993152682 ) ) ;
#95857 = CARTESIAN_POINT ( 'NONE',  ( -8.040148788103921973, 9.338927326664741457, 1.199719254218462483 ) ) ;
#95859 = CARTESIAN_POINT ( 'NONE',  ( 0.6823417656249899377, 3.176041667008085323, -1.181850606188754593 ) ) ;
#95860 = CARTESIAN_POINT ( 'NONE',  ( -3.475000000000000533, -2.800000000000000266, 0.000000000000000000 ) ) ;
#95861 = CARTESIAN_POINT ( 'NONE',  ( 1.273728293839817116, 3.712158128753963560, 0.4850152072975459361 ) ) ;
#95862 = CARTESIAN_POINT ( 'NONE',  ( 0.000000000000000000, 7.000000000000000000, 0.000000000000000000 ) ) ;
#95863 = CARTESIAN_POINT ( 'NONE',  ( 3.005426500355699915, 1.909594650917462388, 1.212984053805040041 ) ) ;
#95864 = CARTESIAN_POINT ( 'NONE',  ( -9.164948653157990677, 11.71552606681625619, -1.443375672974059665 ) ) ;
#95866 = EDGE_CURVE ( 'NONE', #207276, #17744, #6289, .T. ) ;
#95865 = CARTESIAN_POINT ( 'NONE',  ( 2.882852291059742278, -1.675512013591500482, -0.6893320933419128105 ) ) ;
#95867 = CARTESIAN_POINT ( 'NONE',  ( 2.044013137410850778, 0.8228895493161382246, 1.730149048491230301 ) ) ;
#95868 = CARTESIAN_POINT ( 'NONE',  ( 2.664580169416390643, -0.7900844611210651180, -1.913877855911281234 ) ) ;
#95869 = CARTESIAN_POINT ( 'NONE',  ( -1.364683531250012516, 2.801041667008090652, -0.7879004041258289570 ) ) ;
#95870 = CONICAL_SURFACE ( 'NONE', #130554, 11.49999999999998934, 0.7853981633974396193 ) ;
#95871 = CARTESIAN_POINT ( 'NONE',  ( 1.762511527598693784, -1.395553132451602174, 1.392767733363926119 ) ) ;
#95872 = CARTESIAN_POINT ( 'NONE',  ( 0.3231025844343059505, -0.09812569541690382979, 1.924018777033975836 ) ) ;
#95873 = CARTESIAN_POINT ( 'NONE',  ( 3.326877442632663939, 0.04465521416292458912, 1.870282673472216439 ) ) ;
#95875 = CARTESIAN_POINT ( 'NONE',  ( 5.142555292688428814, 7.778213139218437711, -1.168464917166486039 ) ) ;
#95874 = CARTESIAN_POINT ( 'NONE',  ( 1.594773108836315956, -2.296930430523877575, -0.2226743027769726713 ) ) ;
#95876 = CARTESIAN_POINT ( 'NONE',  ( 2.383057912469242812, -0.003606268183664260163, 1.861241884763777499 ) ) ;
#95877 = CARTESIAN_POINT ( 'NONE',  ( 1.364683531249988535, 3.613541667008086211, 0.7879004041258500513 ) ) ;
#95878 = CARTESIAN_POINT ( 'NONE',  ( 5.828601243409065269, -1.311231720126609490, 1.592247268936395121 ) ) ;
#95879 = CARTESIAN_POINT ( 'NONE',  ( -6.423865854776591000, 6.388931673527803667, 1.040834085586084257E-14 ) ) ;
#95880 = CARTESIAN_POINT ( 'NONE',  ( 6.588372581236919601, 9.773852880496709972, -1.199719254218440723 ) ) ;
#95881 = CARTESIAN_POINT ( 'NONE',  ( -1.378728738066232307, 3.613591550242559070, -0.5908528300941753297 ) ) ;
#95882 = CARTESIAN_POINT ( 'NONE',  ( 5.895568648972373538, 1.592330039046478740, 1.378332891347531231 ) ) ;
#95883 = EDGE_CURVE ( 'NONE', #112218, #115335, #15880, .T. ) ;
#95884 = CARTESIAN_POINT ( 'NONE',  ( 1.364683531249988535, 2.926041667008082658, 0.7879004041258500513 ) ) ;
#95885 = CARTESIAN_POINT ( 'NONE',  ( 5.940740243836844847, 0.4152237956781511530, 2.121177236311201586 ) ) ;
#95886 = CARTESIAN_POINT ( 'NONE',  ( 6.463536886191197262, -1.623326069159360063, -1.201424211086026261 ) ) ;
#95887 = CARTESIAN_POINT ( 'NONE',  ( 1.364683531249986537, -0.1364583329919154264, 0.7879004041258500513 ) ) ;
#95888 = AXIS2_PLACEMENT_3D ( 'NONE', #210011, #208944, #160220 ) ;
#95889 = CARTESIAN_POINT ( 'NONE',  ( -4.392478581147607031, 7.108013530438723748, 1.082531754730560403 ) ) ;
#95890 = EDGE_CURVE ( 'NONE', #22324, #153466, #181937, .T. ) ;
#95893 = CARTESIAN_POINT ( 'NONE',  ( 4.012850279964918165, 7.625483060026979842, -0.7216878364870197293 ) ) ;
#95892 = CARTESIAN_POINT ( 'NONE',  ( 0.000000000000000000, -0.1968749995220437643, -3.793834371823813001 ) ) ;
#95891 = CARTESIAN_POINT ( 'NONE',  ( 5.875479466675786355, 7.948088359245467416, -1.599625672291283607 ) ) ;
#95894 = CARTESIAN_POINT ( 'NONE',  ( -4.142898457427624415, 6.991076079377632091, 1.199719254218452935 ) ) ;
#95895 = CARTESIAN_POINT ( 'NONE',  ( 5.173064673083394460, 1.776168143800487043, -0.9548534231369476544 ) ) ;
#95896 = CARTESIAN_POINT ( 'NONE',  ( -7.202405917357668663, 9.425892875049191488, 1.599625672291295375 ) ) ;
#95898 = CARTESIAN_POINT ( 'NONE',  ( -6.902509602688821744, 8.185920970292658083, -1.082531754730549967 ) ) ;
#95897 = CARTESIAN_POINT ( 'NONE',  ( -9.164948653157999559, 10.75515685251491504, -1.082531754730539753 ) ) ;
#95899 = CARTESIAN_POINT ( 'NONE',  ( -1.201851678989727383E-14, 5.196875000341422357, -1.575800808251660134 ) ) ;
#95901 = CARTESIAN_POINT ( 'NONE',  ( 1.364683531249996529, 8.713541667008067648, 0.7879004041258403923 ) ) ;
#95900 = CARTESIAN_POINT ( 'NONE',  ( 6.051685545382852638, 0.6321331830463626789, -2.067208725892249799 ) ) ;
#95902 = CARTESIAN_POINT ( 'NONE',  ( 7.664830294503436114, -5.907420853759296264, -7.777967379493309075 ) ) ;
#95903 = CARTESIAN_POINT ( 'NONE',  ( -11.62998601542303945, 7.357621451758071807, 2.777426515790095696 ) ) ;
#95905 = CARTESIAN_POINT ( 'NONE',  ( -0.1236200418614826352, -0.4170706148690634385, -1.876090511053402965 ) ) ;
#95904 = CARTESIAN_POINT ( 'NONE',  ( -5.531363484251157203, 9.397081798360927607, 0.000000000000000000 ) ) ;
#95906 = CARTESIAN_POINT ( 'NONE',  ( -0.6823417656250003738, -0.4697916663252491021, -1.181850606188749264 ) ) ;
#95907 = CARTESIAN_POINT ( 'NONE',  ( 1.629113003107704793, -1.625012167801738183, 0.5787621435916143753 ) ) ;
#95908 = CARTESIAN_POINT ( 'NONE',  ( 4.736594563127852098, 6.619389305106191834, -1.599625672291273171 ) ) ;
#95909 = CARTESIAN_POINT ( 'NONE',  ( 5.987861119090863049, 7.014868056141362551, 1.199719254218452047 ) ) ;
#95910 = CARTESIAN_POINT ( 'NONE',  ( -11.94110265860324560, 8.911089186573638798, 1.226694517427904696 ) ) ;
#95911 = PRODUCT_DEFINITION ( 'UNKNOWN', '', #104116, #199818 ) ;
#95912 = CARTESIAN_POINT ( 'NONE',  ( 6.134044790494318278, 0.9221746925026914621, -1.627378824227587062 ) ) ;
#95913 = CARTESIAN_POINT ( 'NONE',  ( 1.225244855396601551, 1.776329837998322780, 0.9471711224926461226 ) ) ;
#95914 = FACE_OUTER_BOUND ( 'NONE', #2434, .T. ) ;
#95915 = CARTESIAN_POINT ( 'NONE',  ( 3.241465689944766915, -1.947025830926933043, 1.038692105600529159 ) ) ;
#95916 = CARTESIAN_POINT ( 'NONE',  ( 5.893482054836863604, -1.966010524246808666, 0.9213097603111667366 ) ) ;
#95917 = ORIENTED_EDGE ( 'NONE', *, *, #137329, .T. ) ;
#95918 = CARTESIAN_POINT ( 'NONE',  ( -0.7500000000000006661, -0.6416666666666446250, -1.299038105676652011 ) ) ;
#95919 = CARTESIAN_POINT ( 'NONE',  ( 9.693716643646595799, 11.37205284141829686, 1.082531754730548412 ) ) ;
#95921 = CARTESIAN_POINT ( 'NONE',  ( 2.812125237574264247, 1.117814398428567557, -1.678018709429726307 ) ) ;
#95920 = CARTESIAN_POINT ( 'NONE',  ( 3.352298257493666167, 0.9517314053594098100, -1.894962337767625904 ) ) ;
#95923 = VERTEX_POINT ( 'NONE', #110290 ) ;
#95922 = CARTESIAN_POINT ( 'NONE',  ( 1.810541516808946039, -0.4857983738905074511, -1.745121406981971157 ) ) ;
#95924 = CARTESIAN_POINT ( 'NONE',  ( 5.794130544993763898, 7.853181283949808744, 1.599625672291269396 ) ) ;
#95925 = CARTESIAN_POINT ( 'NONE',  ( 4.801558957534076022, 8.753569217098425170, 0.7998128361456462443 ) ) ;
#95927 = CARTESIAN_POINT ( 'NONE',  ( 1.868237732200584977, -1.879526469796377164, -0.3696609625283857614 ) ) ;
#95926 = CARTESIAN_POINT ( 'NONE',  ( -4.578903193113314174, 6.365139696764064325, 1.599625672291267398 ) ) ;
#95928 = CARTESIAN_POINT ( 'NONE',  ( -2.674941732306335140, 0.4431148209949185568, -0.1136209127918899470 ) ) ;
#95929 = CARTESIAN_POINT ( 'NONE',  ( -11.94655611907589865, 12.44799055453095882, -1.134828163062138628 ) ) ;
#95930 = CARTESIAN_POINT ( 'NONE',  ( 5.680503174001485078, 6.689970460165617361, -1.082531754730543083 ) ) ;
#95931 = CARTESIAN_POINT ( 'NONE',  ( 1.364683531249988757, 0.6968750003414209138, 0.000000000000000000 ) ) ;
#95932 = DIRECTION ( 'NONE',  ( 0.000000000000000000, 0.000000000000000000, -1.000000000000000000 ) ) ;
#95933 = CARTESIAN_POINT ( 'NONE',  ( -8.727698198895085469, 11.20540053684285553, -1.599625672291263179 ) ) ;
#95934 = CARTESIAN_POINT ( 'NONE',  ( 4.838837662799537753, 0.3661284547709364734, 2.130314178654398205 ) ) ;
#95935 = CARTESIAN_POINT ( 'NONE',  ( -3.851925040058333582, 7.508013290127760087, -0.7216878364870458196 ) ) ;
#95936 = CARTESIAN_POINT ( 'NONE',  ( 4.529832720741620022, 7.338536369956936589, -1.082531754730548412 ) ) ;
#95937 = CARTESIAN_POINT ( 'NONE',  ( 2.549219474610735947, 0.2639673528169218519, 2.104066465523121376 ) ) ;
#95939 = CARTESIAN_POINT ( 'NONE',  ( -10.90754186426655004, 4.636108433425617292, 4.485516275142084730 ) ) ;
#95938 = CARTESIAN_POINT ( 'NONE',  ( 0.1753634416057497925, 7.629137130509101361, -2.744001747789548418 ) ) ;
#95940 = CARTESIAN_POINT ( 'NONE',  ( 3.778557292509187260, -1.899022758751211182, -0.5288098451153611101 ) ) ;
#95941 = CARTESIAN_POINT ( 'NONE',  ( 5.273660385517703553, 0.3669835118517566497, -1.876681294024808988 ) ) ;
#95942 = VERTEX_POINT ( 'NONE', #10570 ) ;
#95943 = CIRCLE ( 'NONE', #158088, 9.499999999999992895 ) ;
#95944 = FACE_OUTER_BOUND ( 'NONE', #158160, .T. ) ;
#95945 = CARTESIAN_POINT ( 'NONE',  ( 0.4497787391488928810, 1.533077660697563793, 1.391591089521776681 ) ) ;
#95946 = CARTESIAN_POINT ( 'NONE',  ( 2.730336461235380430, 0.2382978201147344655, 1.927214864610910183 ) ) ;
#95947 = ORIENTED_EDGE ( 'NONE', *, *, #103038, .T. ) ;
#95948 = CARTESIAN_POINT ( 'NONE',  ( -4.277974919820238142, 7.286213140905228869, -0.9367534487179690617 ) ) ;
#95950 = CARTESIAN_POINT ( 'NONE',  ( 6.851666526859736983, 9.086973262793417661, -1.599625672291269396 ) ) ;
#95949 = CARTESIAN_POINT ( 'NONE',  ( -7.295696057929500711, 7.684269287105433222, 0.7216878364870317197 ) ) ;
#95952 = CARTESIAN_POINT ( 'NONE',  ( 5.575427483717746213, 7.527751369135936343, 1.599625672291267398 ) ) ;
#95951 = CARTESIAN_POINT ( 'NONE',  ( 2.818400364232038768, 1.968743758771305918, 0.7038092692753412649 ) ) ;
#95954 = EDGE_CURVE ( 'NONE', #7565, #212473, #74525, .T. ) ;
#95953 = CARTESIAN_POINT ( 'NONE',  ( 4.434925645001613681, 5.307073019657559065, -1.082531754730548412 ) ) ;
#95956 = ORIENTED_EDGE ( 'NONE', *, *, #139645, .T. ) ;
#95955 = CARTESIAN_POINT ( 'NONE',  ( 0.6799528615496954753, 0.8915946574989388473, 1.576789060086491778 ) ) ;
#95957 = CARTESIAN_POINT ( 'NONE',  ( 3.950008152305323428, 0.7444041667201055645, -2.077678867657362538 ) ) ;
#95958 = CARTESIAN_POINT ( 'NONE',  ( 3.188704395469597497, -2.173853526369253331, -0.3788738375181537332 ) ) ;
#95959 = CARTESIAN_POINT ( 'NONE',  ( 8.555358625423188812, 9.940005470203933768, 1.199719254218462483 ) ) ;
#95960 = SURFACE_STYLE_USAGE ( .BOTH. , #211796 ) ;
#95961 = CARTESIAN_POINT ( 'NONE',  ( 1.576665144504853400, -1.351504567317940664, 1.353124384123285617 ) ) ;
#95962 = CARTESIAN_POINT ( 'NONE',  ( 11.43190902327453529, 13.65522128257866363, -3.649704988378122739 ) ) ;
#95963 = CARTESIAN_POINT ( 'NONE',  ( 4.668459276380106715, -0.8822503692092443783, -1.873099891353036561 ) ) ;
#95965 = CARTESIAN_POINT ( 'NONE',  ( 2.553791647773369089, 0.5774160426356907960, -2.083079400968433248 ) ) ;
#95964 = FACE_OUTER_BOUND ( 'NONE', #59640, .T. ) ;
#95966 = CARTESIAN_POINT ( 'NONE',  ( 4.669572502782517454, 1.262004115398765780, 1.791526714441132873 ) ) ;
#95967 = CARTESIAN_POINT ( 'NONE',  ( 9.398826802771546696, 11.98838390803207865, -1.599625672291262513 ) ) ;
#95968 = FACE_OUTER_BOUND ( 'NONE', #113034, .T. ) ;
#95969 = CARTESIAN_POINT ( 'NONE',  ( -0.5049859354315073823, 7.739806959121713348, 1.936057643311939858 ) ) ;
#95970 = CARTESIAN_POINT ( 'NONE',  ( 6.225128807330042591, 7.291680359087043151, -1.199719254218452047 ) ) ;
#95971 = CARTESIAN_POINT ( 'NONE',  ( -3.285556943750000070, -2.296874999522042327, 0.000000000000000000 ) ) ;
#95972 = EDGE_CURVE ( 'NONE', #702, #7565, #96412, .T. ) ;
#95973 = CARTESIAN_POINT ( 'NONE',  ( -4.899292406491858820, 6.809203455697518947, -1.599625672291271394 ) ) ;
#95974 = CARTESIAN_POINT ( 'NONE',  ( 0.01820432788856435335, -1.842448466851685840, 0.8197770699841927522 ) ) ;
#95975 = CARTESIAN_POINT ( 'NONE',  ( -7.524412065904404479, 11.72230514362308185, 0.000000000000000000 ) ) ;
#95976 = TOROIDAL_SURFACE ( 'NONE', #140825, 11.92000000000000348, 0.08000000000000000167 ) ;
#95977 = CARTESIAN_POINT ( 'NONE',  ( 4.698136132249701724, 0.8899761679339033282, -1.869364561350304488 ) ) ;
#95978 = CARTESIAN_POINT ( 'NONE',  ( 2.965364049027201965, 0.2823637808789316028, -1.905579842893694975 ) ) ;
#95979 = CARTESIAN_POINT ( 'NONE',  ( 5.571900387404195243, -0.9513999510230609635, 1.891474119154999745 ) ) ;
#95980 = CARTESIAN_POINT ( 'NONE',  ( 5.555090253297246150, 7.504024600312024340, 1.599625672291267398 ) ) ;
#95981 = CARTESIAN_POINT ( 'NONE',  ( 4.740893929121448025, 8.308742936830851633, 0.7931989123739242586 ) ) ;
#95982 = CARTESIAN_POINT ( 'NONE',  ( 4.012523933672189180, 0.7048025691861439235, 1.839212210364450151 ) ) ;
#95983 = CARTESIAN_POINT ( 'NONE',  ( 6.263675073536269622, 1.173004239817846850, 1.969288764181243989 ) ) ;
#95984 = CARTESIAN_POINT ( 'NONE',  ( 3.984828715814022981, -0.1808549858164226476, -1.816707794649790708 ) ) ;
#95985 = CARTESIAN_POINT ( 'NONE',  ( 5.560252395380198998, 9.501061871336672127, 0.7216878364870317197 ) ) ;
#95986 = CARTESIAN_POINT ( 'NONE',  ( 5.165293336682183600, 5.128523102325077687, -0.7216878364870197293 ) ) ;
#95987 = CARTESIAN_POINT ( 'NONE',  ( -7.442499979258930587, 7.647614495415686164, -0.7998128361456362523 ) ) ;
#95988 = CARTESIAN_POINT ( 'NONE',  ( 5.529746549527311039, 7.544733289238903851, -1.599625672291281386 ) ) ;
#95989 = ORIENTED_EDGE ( 'NONE', *, *, #175486, .F. ) ;
#95991 = CARTESIAN_POINT ( 'NONE',  ( 5.256112987848621465, 0.8120324739511315393, -1.842333132669704554 ) ) ;
#95990 = CARTESIAN_POINT ( 'NONE',  ( 1.804012939494209267, 1.363607186100148638, -1.237405090928713092 ) ) ;
#95992 = CARTESIAN_POINT ( 'NONE',  ( 5.889324137892314681, -0.8237033142024595689, -2.146187584169775953 ) ) ;
#95993 = CARTESIAN_POINT ( 'NONE',  ( 6.051606296966551390, 1.483190043545830505, 1.284043323103729595 ) ) ;
#95994 = CARTESIAN_POINT ( 'NONE',  ( -5.669280788808708671, 9.765911353585494226, 0.7998128361456481317 ) ) ;
#95995 = CARTESIAN_POINT ( 'NONE',  ( -4.273844736805832767, 6.009238164405336313, 1.599625672291267398 ) ) ;
#95996 = CARTESIAN_POINT ( 'NONE',  ( -6.120580001926503755, 6.105374521861167914, -0.7998128361456362523 ) ) ;
#95998 = CARTESIAN_POINT ( 'NONE',  ( 6.332837517263664395, 0.1779433324526000226, 1.760853854254845530 ) ) ;
#95997 = CARTESIAN_POINT ( 'NONE',  ( 1.224293845215556953, 2.015865829440838031, 0.5543246906533367824 ) ) ;
#95999 = CARTESIAN_POINT ( 'NONE',  ( -0.3911212198684586583, 3.085581642975291139, 2.026362403383771937 ) ) ;
#96000 = CARTESIAN_POINT ( 'NONE',  ( -0.1106727585415940990, -0.002281114264979232885, -2.003378291782103027 ) ) ;
#96001 = B_SPLINE_CURVE_WITH_KNOTS ( 'NONE', 3,
 ( #8267, #52748, #184868, #87396, #3970, #70038, #202171, #203249 ),
 .UNSPECIFIED., .F., .F.,
 ( 4, 2, 2, 4 ),
 ( 4.385326393719464467E-18, 0.0006692579211854246318, 0.001003886881778133641, 0.001338515842370842758 ),
 .UNSPECIFIED. ) ;
#96002 = CARTESIAN_POINT ( 'NONE',  ( 1.030331162470259354, -1.574104619921200765, 0.7428470239391560259 ) ) ;
#96003 = CARTESIAN_POINT ( 'NONE',  ( 5.276094334012385367, 9.307193822989793475, 1.040834085586084257E-14 ) ) ;
#96005 = DIRECTION ( 'NONE',  ( 1.276756478318932585E-15, -1.000000000000000000, 1.665334536937738262E-16 ) ) ;
#96004 = CYLINDRICAL_SURFACE ( 'NONE', #131089, 1.500000000000000222 ) ;
#96006 = CARTESIAN_POINT ( 'NONE',  ( 1.717014342725260656, -0.2134408525867482198, 1.711538560699257916 ) ) ;
#96007 = CARTESIAN_POINT ( 'NONE',  ( 2.050558489324630251, -1.691691439650149897, 1.393213601605561180 ) ) ;
#96008 = CARTESIAN_POINT ( 'NONE',  ( -0.1054646484276201696, -0.7404878594409001202, -1.567598555697255369 ) ) ;
#96009 = CARTESIAN_POINT ( 'NONE',  ( 3.897267319706390065, 1.864829029706360330, -1.179861312946443697 ) ) ;
#96010 = DIRECTION ( 'NONE',  ( 0.8002608041566210417, 0.5996521035822340862, 0.000000000000000000 ) ) ;
#96011 = CIRCLE ( 'NONE', #61354, 0.07999999999999961309 ) ;
#96012 = CARTESIAN_POINT ( 'NONE',  ( 1.762787986429158016, -0.7786651900678620564, -2.026813006651595028 ) ) ;
#96013 = CARTESIAN_POINT ( 'NONE',  ( 1.270904146967301473, 3.084693569853256268, -0.7749999999999910294 ) ) ;
#96014 = CARTESIAN_POINT ( 'NONE',  ( 3.274719840360585721, -0.4174103159439371824, -2.075633323822536180 ) ) ;
#96015 = CARTESIAN_POINT ( 'NONE',  ( 6.539320575229256249, 4.699150603835311912, 2.459441311396874941 ) ) ;
#96016 = ORIENTED_EDGE ( 'NONE', *, *, #83952, .F. ) ;
#96018 = CARTESIAN_POINT ( 'NONE',  ( 0.6823417656249882723, 0.2385416670080825474, -1.181850606188749264 ) ) ;
#96017 = CARTESIAN_POINT ( 'NONE',  ( 3.281108521976669135, 2.071599159226782838, -0.9818635949487266590 ) ) ;
#96019 = CARTESIAN_POINT ( 'NONE',  ( 5.529027716274630855, 5.344953845275508542, 1.040834085586084257E-14 ) ) ;
#96020 = AXIS2_PLACEMENT_3D ( 'NONE', #56449, #188572, #189637 ) ;
#96021 = CARTESIAN_POINT ( 'NONE',  ( 5.619863295618399590, -0.5416267994347803150, 2.154155341088887177 ) ) ;
#96022 = CARTESIAN_POINT ( 'NONE',  ( -7.402388683381436074, 7.738467673474211495, 0.7216878364870317197 ) ) ;
#96023 = ADVANCED_FACE ( 'NONE', ( #112419 ), #180546, .F. ) ;
#96024 = CARTESIAN_POINT ( 'NONE',  ( 5.395781948558860286, 6.357795697149212444, -1.082531754730542195 ) ) ;
#96025 = B_SPLINE_CURVE_WITH_KNOTS ( 'NONE', 3,
 ( #114341, #62319, #45024, #163030, #112207, #13558 ),
 .UNSPECIFIED., .F., .F.,
 ( 4, 2, 4 ),
 ( 0.000000000000000000, 0.5000000000000000000, 1.000000000000000000 ),
 .UNSPECIFIED. ) ;
#96026 = CARTESIAN_POINT ( 'NONE',  ( -6.331294547457448019, 10.33033470543493770, 0.7216878364870458196 ) ) ;
#96027 = CARTESIAN_POINT ( 'NONE',  ( 5.587368702607580673, 5.691220705896524734, -0.7216878364870458196 ) ) ;
#96028 = ORIENTED_EDGE ( 'NONE', *, *, #125182, .F. ) ;
#96029 = CARTESIAN_POINT ( 'NONE',  ( 3.586564705785996843, -0.5826563296015655480, 1.930417576838711957 ) ) ;
#96031 = CARTESIAN_POINT ( 'NONE',  ( 2.325117943063298664, -1.883989625962046555, -0.8399396378151212650 ) ) ;
#96030 = CARTESIAN_POINT ( 'NONE',  ( 7.135668919494039031, 7.219368582364847242, 1.040834085586084257E-14 ) ) ;
#96032 = CARTESIAN_POINT ( 'NONE',  ( -9.579698345292687378, -7.154544010627095219, -0.07602376731354575090 ) ) ;
#96033 = CARTESIAN_POINT ( 'NONE',  ( 5.519577934094861860, 6.572500690266394940, 1.082531754730549078 ) ) ;
#96034 = DIRECTION ( 'NONE',  ( 0.000000000000000000, -1.000000000000000000, 0.000000000000000000 ) ) ;
#96035 = CARTESIAN_POINT ( 'NONE',  ( -0.6823417656249969321, 4.467708333674755394, -1.181850606188749264 ) ) ;
#96036 = CARTESIAN_POINT ( 'NONE',  ( 5.138714532536901913, -1.880766731008373993, 1.124575086929799239 ) ) ;
#96037 = CARTESIAN_POINT ( 'NONE',  ( 2.848279904836711118, 0.2930702634792031747, -1.994869876753922799 ) ) ;
#96038 = CARTESIAN_POINT ( 'NONE',  ( 1.680954830071922812, 1.270413995023990106, 1.332975479855981416 ) ) ;
#96039 = VECTOR ( 'NONE', #187095, 1000.000000000000000 ) ;
#96040 = CARTESIAN_POINT ( 'NONE',  ( 6.662942426112080874, 9.860851032851066122, 1.199719254218460707 ) ) ;
#96041 = CARTESIAN_POINT ( 'NONE',  ( 4.963791182761823961, 1.805510465697376610, -0.2690417022049585438 ) ) ;
#96042 = CARTESIAN_POINT ( 'NONE',  ( 5.731092321990707283, 2.014232586630093191, 0.09613807139101374077 ) ) ;
#96043 = CARTESIAN_POINT ( 'NONE',  ( -8.538937818508475885, 8.856515631215026829, 1.040834085586084257E-14 ) ) ;
#96045 = CARTESIAN_POINT ( 'NONE',  ( -6.038177310039794854, 8.137902509836795417, -1.599625672291271394 ) ) ;
#96044 = CARTESIAN_POINT ( 'NONE',  ( 5.348581951612152885, 0.6511601234850499242, 2.166799557567296919 ) ) ;
#96046 = CARTESIAN_POINT ( 'NONE',  ( 1.119907265981748168, -2.054334215221398807, 0.4631877017708794231 ) ) ;
#96047 = CARTESIAN_POINT ( 'NONE',  ( -6.587282531393266360, 8.778525268082516320, 1.599625672291269396 ) ) ;
#96048 = CARTESIAN_POINT ( 'NONE',  ( 8.757677159423465696, 12.30470822171437284, 1.199719254218450271 ) ) ;
#96049 = CARTESIAN_POINT ( 'NONE',  ( -1.360316468750048635, 2.651041667008094738, -0.7853790794159161148 ) ) ;
#96050 = DIRECTION ( 'NONE',  ( 0.006773480265431362779, -1.101949923320552235E-22, 0.9999770597194186372 ) ) ;
#96051 = CARTESIAN_POINT ( 'NONE',  ( -8.227100285394159940, 8.492705175914988303, 0.7998128361456602331 ) ) ;
#96052 = CARTESIAN_POINT ( 'NONE',  ( 0.2756800312742226367, 7.029902384775073898, 4.006536513033384317 ) ) ;
#96053 = CARTESIAN_POINT ( 'NONE',  ( 7.147083253059300922, 8.367293879104554577, 1.199719254218452935 ) ) ;
#96054 = CARTESIAN_POINT ( 'NONE',  ( 5.538030394937467626, 6.199453712711876285, -0.9301498999644899346 ) ) ;
#96055 = CARTESIAN_POINT ( 'NONE',  ( -8.676855123066019360, 11.14608361504227574, -1.443375672974059665 ) ) ;
#96056 = CARTESIAN_POINT ( 'NONE',  ( 2.549351761953377427, 0.2766319664159795355, 2.204086880180194274 ) ) ;
#96057 = DIRECTION ( 'NONE',  ( 0.000000000000000000, 1.000000000000000000, 0.000000000000000000 ) ) ;
#96058 = CARTESIAN_POINT ( 'NONE',  ( -5.261446130555064826, 8.296048364692991228, 1.199719254218452935 ) ) ;
#96059 = CARTESIAN_POINT ( 'NONE',  ( 5.829115978871627135, 8.888053511070525659, 1.199719254218462483 ) ) ;
#96060 = CARTESIAN_POINT ( 'NONE',  ( 3.174217076811707727, -0.9646401420641316227, -1.708233030250068785 ) ) ;
#96061 = CARTESIAN_POINT ( 'NONE',  ( 6.498435699651741615, 6.475929825882159818, -0.7998128361456281477 ) ) ;
#96063 =( BOUNDED_CURVE ( )  B_SPLINE_CURVE ( 2, ( #33175, #134964, #49431 ),
 .UNSPECIFIED., .F., .T. ) 
 B_SPLINE_CURVE_WITH_KNOTS ( ( 3, 3 ),
 ( 0.5176136498557766252, 0.5249999999999998002 ),
 .UNSPECIFIED. ) 
 CURVE ( )  GEOMETRIC_REPRESENTATION_ITEM ( )  RATIONAL_B_SPLINE_CURVE ( ( 0.9730109806173230513, 0.8812500066305124502, 0.9999999999999964473 ) ) 
 REPRESENTATION_ITEM ( '' )  );
#96062 = CARTESIAN_POINT ( 'NONE',  ( -4.105200985651542567, 7.499488806860944656, 0.5979674706809139373 ) ) ;
#96064 = CARTESIAN_POINT ( 'NONE',  ( 3.009020027229115879, 5.597941567487558778, -1.199719254218446718 ) ) ;
#96065 = CARTESIAN_POINT ( 'NONE',  ( -4.746763178560296836, 6.631252689777363152, 1.443375672974058777 ) ) ;
#96066 = CARTESIAN_POINT ( 'NONE',  ( -5.748293942514169252, 9.650167333001109071, -0.7216878364870207285 ) ) ;
#96067 = CARTESIAN_POINT ( 'NONE',  ( 2.127334043950947606, 1.896359100603739911, 0.9491756072362851349 ) ) ;
#96068 = CARTESIAN_POINT ( 'NONE',  ( -5.957882158562513908, 5.915560371269843465, -0.7998128361456362523 ) ) ;
#96069 = CARTESIAN_POINT ( 'NONE',  ( 4.680646922328831394, -2.095996545452833981, -0.5284188670612932626 ) ) ;
#96070 = CARTESIAN_POINT ( 'NONE',  ( 2.331387312403776946, 0.8663521307504215008, -1.624669977836174839 ) ) ;
#96071 = CARTESIAN_POINT ( 'NONE',  ( -5.357213605067637552, 6.353687308821166724, 1.098221101205157035 ) ) ;
#96072 = CARTESIAN_POINT ( 'NONE',  ( 0.6823417656249882723, -0.01145833299191073573, -1.181850606188749264 ) ) ;
#96073 = EDGE_CURVE ( 'NONE', #82527, #99453, #163245, .T. ) ;
#96074 = CARTESIAN_POINT ( 'NONE',  ( 5.841712918432809154, 1.738692355929325029, 0.07866246996769517275 ) ) ;
#96075 = CARTESIAN_POINT ( 'NONE',  ( 0.08053691275167890185, 14.48153890507870223, 11.99972973886013961 ) ) ;
#96076 = CARTESIAN_POINT ( 'NONE',  ( 4.039966587192259873, 5.736380323189513852, 1.443375672974062551 ) ) ;
#96077 = CARTESIAN_POINT ( 'NONE',  ( -1.219727444046192488E-15, -7.721243112841094103, 10.98746396341379317 ) ) ;
#96078 = CARTESIAN_POINT ( 'NONE',  ( 2.799875798528407511, -0.6792266858460673795, 2.052276964324008635 ) ) ;
#96079 = CARTESIAN_POINT ( 'NONE',  ( 5.009138659175729202, 2.010518709310470609, 0.1511151588593287465 ) ) ;
#96080 = CARTESIAN_POINT ( 'NONE',  ( -8.473482818416670170, 10.90881592628469932, -1.443375672974058777 ) ) ;
#96081 = CARTESIAN_POINT ( 'NONE',  ( 2.079201547314021070, -0.1057080177612122196, -2.159229931372666389 ) ) ;
#96082 = CARTESIAN_POINT ( 'NONE',  ( 2.969950176076568749, 1.051608646734447650, 1.667261953242512140 ) ) ;
#96083 = CARTESIAN_POINT ( 'NONE',  ( 2.905482715143858030, -1.942096844255640109, 0.5424705965835219246 ) ) ;
#96084 = CARTESIAN_POINT ( 'NONE',  ( 6.509000000000035868, 7.629137130509092479, 2.600000000000000977 ) ) ;
#96085 = CARTESIAN_POINT ( 'NONE',  ( 5.021012369077997306, -1.842940949158570207, 0.6126725321249880674 ) ) ;
#96087 = ORIENTED_EDGE ( 'NONE', *, *, #2718, .T. ) ;
#96086 = CARTESIAN_POINT ( 'NONE',  ( -7.822691444960700125, 11.10992853822074444, -1.082531754730543083 ) ) ;
#96088 = CARTESIAN_POINT ( 'NONE',  ( -3.648552735408990166, 6.310376387068841630, -1.082531754730546636 ) ) ;
#96089 = CARTESIAN_POINT ( 'NONE',  ( 3.736153849017632922, 6.516540702899320081, -1.199719254218453823 ) ) ;
#96090 = ADVANCED_FACE ( 'NONE', ( #15889 ), #27902, .F. ) ;
#96092 = VERTEX_POINT ( 'NONE', #162182 ) ;
#96091 = CARTESIAN_POINT ( 'NONE',  ( -3.793249116773374396, 7.647484079536056356, 0.7998128361456352531 ) ) ;
#96093 = CARTESIAN_POINT ( 'NONE',  ( -9.612367721964622191, 10.31677655182129527, -0.7216878364870267237 ) ) ;
#96094 = CARTESIAN_POINT ( 'NONE',  ( 1.677102584378454608, -2.095606157416990190, -0.6917391671936305997 ) ) ;
#96095 = CARTESIAN_POINT ( 'NONE',  ( 1.642778471875001811, -1.742708332855374298, 2.845375778867859751 ) ) ;
#96096 = CARTESIAN_POINT ( 'NONE',  ( 5.506681978947471912, 0.5658967987182733639, 1.878394690154854496 ) ) ;
#96097 = CARTESIAN_POINT ( 'NONE',  ( -1.364683531250012516, 5.051041667008085767, -0.7879004041258300672 ) ) ;
#96098 = CARTESIAN_POINT ( 'NONE',  ( 1.499999999999989120, 4.535416667349484676, 0.8660254037844524744 ) ) ;
#96099 = CARTESIAN_POINT ( 'NONE',  ( 5.722549628727856330, 6.269105753387675506, -1.057781258018471782 ) ) ;
#96100 = CARTESIAN_POINT ( 'NONE',  ( 4.055297343818932809, 7.745280977848486792, 0.7216878364870341622 ) ) ;
#96101 = CARTESIAN_POINT ( 'NONE',  ( 4.786955173189685553, 1.366302399619228725, 1.234289508136581670 ) ) ;
#96102 = ORIENTED_EDGE ( 'NONE', *, *, #37661, .F. ) ;
#96103 = CARTESIAN_POINT ( 'NONE',  ( -0.6801582343750161019, -0.9010416663252431846, -1.178068619123869398 ) ) ;
#96104 = CARTESIAN_POINT ( 'NONE',  ( -7.374745490829552885, 10.69128794168811680, -1.199719254218446718 ) ) ;
#96105 = CARTESIAN_POINT ( 'NONE',  ( 0.09478498853002972901, -7.830875036364503024E-15, 1.351550957883141058 ) ) ;
#96106 = CARTESIAN_POINT ( 'NONE',  ( 6.205353461901607304, 1.844339991697005798, -1.046509186232460697 ) ) ;
#96107 = CARTESIAN_POINT ( 'NONE',  ( 8.812662591969752768, 13.17658495047174760, -8.076872458326402437 ) ) ;
#96108 = CARTESIAN_POINT ( 'NONE',  ( 6.043183783389218355, 8.073467052085995022, 1.599625672291267398 ) ) ;
#96109 = CARTESIAN_POINT ( 'NONE',  ( 6.749297902460969389, -1.652236475679531580, -1.231405567270830170 ) ) ;
#96112 = CARTESIAN_POINT ( 'NONE',  ( 3.421284184235491743, -1.099380227797893905, -1.476844927387373163 ) ) ;
#96111 = CARTESIAN_POINT ( 'NONE',  ( 1.468971578825052804, 1.639158939101122758, 0.8813203298513817563 ) ) ;
#96110 = CARTESIAN_POINT ( 'NONE',  ( 3.732121546690903457, 4.106948192567998035, -0.9424847539492161586 ) ) ;
#96113 = CARTESIAN_POINT ( 'NONE',  ( 6.934105498385400246, 10.17720795050327354, -1.199719254218441611 ) ) ;
#96114 = DIRECTION ( 'NONE',  ( 0.000000000000000000, -1.000000000000000000, 0.000000000000000000 ) ) ;
#96115 = CARTESIAN_POINT ( 'NONE',  ( -7.618755976236585958, 7.853246491889623648, 0.000000000000000000 ) ) ;
#96116 = CARTESIAN_POINT ( 'NONE',  ( 6.610000000000009202, 6.036727194997777879, 2.594899704271665275 ) ) ;
#96117 = CIRCLE ( 'NONE', #61596, 4.500000000000000000 ) ;
#96118 = CARTESIAN_POINT ( 'NONE',  ( 2.877765823869771644, 2.095344539500657799, -0.6929138170133213315 ) ) ;
#96119 = CARTESIAN_POINT ( 'NONE',  ( 5.993528260394247020, 1.707464403934123798, 1.484360591965392828 ) ) ;
#96120 = CARTESIAN_POINT ( 'NONE',  ( -6.914295153289458540, 7.169025221700239925, 0.7216878364870317197 ) ) ;
#96121 = CARTESIAN_POINT ( 'NONE',  ( 6.293201719952925544, -0.09848415459409513850, -1.809066888985458199 ) ) ;
#96122 = CARTESIAN_POINT ( 'NONE',  ( 0.1984543448181053105, 1.387095780679182377, -1.463931301963219855 ) ) ;
#96123 = CARTESIAN_POINT ( 'NONE',  ( -6.471393748265538370, 5.229711127717889596, -2.499999999999995115 ) ) ;
#96124 = CARTESIAN_POINT ( 'NONE',  ( 6.244977087980838171, -1.579202250953464670, 1.002420361074819688 ) ) ;
#96125 = CARTESIAN_POINT ( 'NONE',  ( 6.267989458847986306, -1.846849288558198188, 0.2287129521939580412 ) ) ;
#96126 = CARTESIAN_POINT ( 'NONE',  ( 4.039966587192257208, 6.696749537490852333, 1.082531754730558626 ) ) ;
#96127 = TOROIDAL_SURFACE ( 'NONE', #58059, 2.149999999999999911, 0.1000000000000000056 ) ;
#96128 = CARTESIAN_POINT ( 'NONE',  ( 6.262547730648324595, -1.248425448203832611, 1.254777848270997254 ) ) ;
#96130 = CIRCLE ( 'NONE', #16597, 0.4000000000000001332 ) ;
#96129 = CIRCLE ( 'NONE', #82169, 12.00000000000000178 ) ;
#96131 = CARTESIAN_POINT ( 'NONE',  ( 0.9367328597341374463, -1.586666764284098807, 1.244388658875786424 ) ) ;
#96133 = CARTESIAN_POINT ( 'NONE',  ( 3.281953686177707219, 1.336396692706752765, 1.627740544975244008 ) ) ;
#96132 = CARTESIAN_POINT ( 'NONE',  ( -8.292783513053063160, 12.82666453187061073, 0.7998128361456481317 ) ) ;
#96134 = EDGE_CURVE ( 'NONE', #92745, #108467, #114554, .T. ) ;
#96135 = CARTESIAN_POINT ( 'NONE',  ( 7.584896871841365851, 10.93646455286856956, -1.199719254218446718 ) ) ;
#96137 = CARTESIAN_POINT ( 'NONE',  ( -7.831806290188425557, 12.28885777186185990, -0.7998128361456281477 ) ) ;
#96136 = CARTESIAN_POINT ( 'NONE',  ( -1.500000000000013101, 0.1708333333333560411, 0.8660254037844403729 ) ) ;
#96138 = CARTESIAN_POINT ( 'NONE',  ( 4.764381983412778688E-15, 12.93749999999999645, -1.499999999999998446 ) ) ;
#96139 = CARTESIAN_POINT ( 'NONE',  ( 3.234633093136650928, 1.278207680322031026, -1.563912617747134970 ) ) ;
#96140 = CARTESIAN_POINT ( 'NONE',  ( 0.6823417656249899377, 2.842708333674753618, 1.181850606188765695 ) ) ;
#96141 = EDGE_CURVE ( 'NONE', #32206, #164712, #97938, .T. ) ;
#96142 = CARTESIAN_POINT ( 'NONE',  ( 3.440018289565364817, 5.036440642624797626, 1.599625672291267398 ) ) ;
#96143 = CARTESIAN_POINT ( 'NONE',  ( 3.761131992884462871, -1.904433681825665969, -1.022602951024270679 ) ) ;
#96144 = CARTESIAN_POINT ( 'NONE',  ( 5.826972158823246595, 10.02016096192762085, -0.7998128361456481317 ) ) ;
#96146 = DIRECTION ( 'NONE',  ( 1.276756478318932585E-15, -1.000000000000000000, 1.665334536937738262E-16 ) ) ;
#96145 = CARTESIAN_POINT ( 'NONE',  ( 7.666209513884374438, 7.908608952478760834, 0.7998128361456281477 ) ) ;
#96147 = CARTESIAN_POINT ( 'NONE',  ( 8.880227426826634129, 11.38335130276301754, 1.443375672974076540 ) ) ;
#96149 = CARTESIAN_POINT ( 'NONE',  ( 9.171693111243110152, 14.14829661376107772, -7.667865116287802429 ) ) ;
#96148 = CARTESIAN_POINT ( 'NONE',  ( 0.8894206616707257540, 0.1598827910747530057, 2.165323314709698632 ) ) ;
#96150 = CARTESIAN_POINT ( 'NONE',  ( -5.395781948558855845, 9.238903340053241209, 0.7216878364870458196 ) ) ;
#96151 = CARTESIAN_POINT ( 'NONE',  ( -0.6823417656250003738, 1.217708333674752286, -1.181850606188749264 ) ) ;
#96152 = CARTESIAN_POINT ( 'NONE',  ( 2.173600921376659834, 1.351110561487681716, 1.725424542402646422 ) ) ;
#96153 = CARTESIAN_POINT ( 'NONE',  ( 0.4210486379898482623, 7.995128625469308581, 1.998698746375270341 ) ) ;
#96154 = CARTESIAN_POINT ( 'NONE',  ( 2.553932558351139193, 0.6037834209405189556, -2.180390065951258283 ) ) ;
#96155 = CARTESIAN_POINT ( 'NONE',  ( -6.509886312855995172, 10.74661779830734254, -0.7998128361456291469 ) ) ;
#96156 = CARTESIAN_POINT ( 'NONE',  ( 4.399625206644591557, -1.976670321813909892, 0.3981083777728141038 ) ) ;
#96157 = CARTESIAN_POINT ( 'NONE',  ( -3.511198595814942980, 5.119484333249288532, 1.443375672974064550 ) ) ;
#96158 = CARTESIAN_POINT ( 'NONE',  ( 0.6823417656249882723, 2.988541667008084879, -1.181850606188754593 ) ) ;
#96159 = CARTESIAN_POINT ( 'NONE',  ( 6.003728048595398548, 7.077753126805482076, 1.059392881431284961 ) ) ;
#96160 = CARTESIAN_POINT ( 'NONE',  ( -1.500000000000001110, 10.77083333333333037, 0.8660254037844419273 ) ) ;
#96161 = CARTESIAN_POINT ( 'NONE',  ( 7.526184669361807522, 7.953172667109813077, 0.000000000000000000 ) ) ;
#96162 = EDGE_CURVE ( 'NONE', #69507, #2895, #45413, .T. ) ;
#96163 = CARTESIAN_POINT ( 'NONE',  ( 3.461912321176093599, 0.7928900474763724837, 1.582224000876080172 ) ) ;
#96164 = CIRCLE ( 'NONE', #102933, 11.09999999999999964 ) ;
#96165 = CARTESIAN_POINT ( 'NONE',  ( 9.921869487102386032, 10.46993591124128997, 0.000000000000000000 ) ) ;
#96166 = CARTESIAN_POINT ( 'NONE',  ( 6.001041448284401447, 1.807427358944500684, -1.265864663738118345 ) ) ;
#96167 = CARTESIAN_POINT ( 'NONE',  ( -8.012344526598182026E-15, 9.296875000341398021, -1.575800808251669460 ) ) ;
#96168 = CARTESIAN_POINT ( 'NONE',  ( -3.461074353238556167, 7.259946855412102273, 0.000000000000000000 ) ) ;
#96169 = CARTESIAN_POINT ( 'NONE',  ( 5.817982510940042040, 0.9913841921252890543, -1.755779027446252138 ) ) ;
#96170 = ORIENTED_EDGE ( 'NONE', *, *, #168698, .T. ) ;
#96171 = CIRCLE ( 'NONE', #68450, 11.54340198673881979 ) ;
#96172 = CARTESIAN_POINT ( 'NONE',  ( 3.485083742438867205, 1.691615344724434200, -0.7988839237506043522 ) ) ;
#96173 = CARTESIAN_POINT ( 'NONE',  ( 3.344645782512998267, -2.038826501179476391, -0.3585456059004287765 ) ) ;
#96174 = CARTESIAN_POINT ( 'NONE',  ( -5.736508391913536897, 9.706693867292189637, 0.7216878364870267237 ) ) ;
#96175 = DIRECTION ( 'NONE',  ( 0.000000000000000000, 0.000000000000000000, 1.000000000000000000 ) ) ;
#96176 = CARTESIAN_POINT ( 'NONE',  ( -1.546240757466864402, 8.694816975860053532, 2.507471980975723103 ) ) ;
#96177 = CARTESIAN_POINT ( 'NONE',  ( -4.790662068211312352, 6.933575286401571169, 1.250027526764455388 ) ) ;
#96178 = CARTESIAN_POINT ( 'NONE',  ( 0.6823417656249864960, -0.8239583329919114574, -1.181850606188749264 ) ) ;
#96179 = CARTESIAN_POINT ( 'NONE',  ( 2.611707774152134842, 0.5260268489151798121, -1.889944157703125072 ) ) ;
#96180 = CARTESIAN_POINT ( 'NONE',  ( 0.3860920070548681804, -0.1017387759476989784, 2.013677428805898728 ) ) ;
#96181 = CARTESIAN_POINT ( 'NONE',  ( -5.008811405605897882, 4.808311159487113073, 0.7998128361456281477 ) ) ;
#96183 = CARTESIAN_POINT ( 'NONE',  ( -11.97181073603049839, 13.88000000000000256, -0.8318477717169578955 ) ) ;
#96182 = CARTESIAN_POINT ( 'NONE',  ( 8.769426429940780920, 9.125419011219408461, 0.7998128361456462443 ) ) ;
#96184 = CARTESIAN_POINT ( 'NONE',  ( 0.8252170375972631700, -1.778153878779257901, 0.5809004490327505099 ) ) ;
#96185 = CARTESIAN_POINT ( 'NONE',  ( 0.6823417656249899377, 3.176041667008085323, -1.181850606188754593 ) ) ;
#96186 = CARTESIAN_POINT ( 'NONE',  ( 2.601816991827472947, 1.426658649466717943, 1.420685320369071025 ) ) ;
#96188 = CARTESIAN_POINT ( 'NONE',  ( 2.601287765717251510, -0.2046159961377100600, 2.107301599238825318 ) ) ;
#96187 = CARTESIAN_POINT ( 'NONE',  ( -7.537970219518089543, 8.857015346601659900, -1.082531754730543971 ) ) ;
#96189 = CARTESIAN_POINT ( 'NONE',  ( 1.440240048130367878, 7.355731858843415516, 4.317885097515409498 ) ) ;
#96190 = CARTESIAN_POINT ( 'NONE',  ( 3.736834853878097107, -1.994506513866915576, -0.5549897870569252545 ) ) ;
#96191 = CARTESIAN_POINT ( 'NONE',  ( 7.506374323821472849, 8.786466794993730289, -1.199719254218452047 ) ) ;
#96193 = FACE_OUTER_BOUND ( 'NONE', #201526, .T. ) ;
#96192 = CARTESIAN_POINT ( 'NONE',  ( 6.316366637557600860, 1.950215401406007354, 0.7537550503652605816 ) ) ;
#96195 = VERTEX_POINT ( 'NONE', #11642 ) ;
#96194 = CARTESIAN_POINT ( 'NONE',  ( 4.313378725478684395, -0.3118687524542098632, 1.798583714455632476 ) ) ;
#96196 = CARTESIAN_POINT ( 'NONE',  ( 8.703444544968814256, 12.24143683818393313, -1.199719254218446718 ) ) ;
#96197 = AXIS2_PLACEMENT_3D ( 'NONE', #17324, #37863, #101797 ) ;
#96198 = CARTESIAN_POINT ( 'NONE',  ( 0.000000000000000000, 9.719999999999998863, 0.000000000000000000 ) ) ;
#96199 = CARTESIAN_POINT ( 'NONE',  ( 11.86429981771095754, 8.354644167381561459, 1.610253852115079543 ) ) ;
#96200 = CARTESIAN_POINT ( 'NONE',  ( 6.405322867445039314, 1.831175526881479776, 1.231239259074583092 ) ) ;
#96201 = CARTESIAN_POINT ( 'NONE',  ( -1.364683531250014514, 11.15104166700806232, -0.7879004041258335089 ) ) ;
#96202 = CARTESIAN_POINT ( 'NONE',  ( 5.074826771331380826, -1.382354945563003312, 1.321565576914075502 ) ) ;
#96203 = CARTESIAN_POINT ( 'NONE',  ( -8.136864746495904299, 12.64475930422059768, -0.7998128361456281477 ) ) ;
#96204 = CARTESIAN_POINT ( 'NONE',  ( 7.446452682403650769, 9.710614100936176385, -1.599625672291262513 ) ) ;
#96205 = CARTESIAN_POINT ( 'NONE',  ( -6.960724307482170605E-14, 1.484375000341481288, 1.570758158831758289 ) ) ;
#96206 = CARTESIAN_POINT ( 'NONE',  ( 4.514501963226220660, 4.369266499959774563, -0.7216878364870197293 ) ) ;
#96207 = CARTESIAN_POINT ( 'NONE',  ( 0.9250624443557056154, -1.167992581197497604, -1.423340509374780405 ) ) ;
#96208 = ORIENTED_EDGE ( 'NONE', *, *, #79248, .F. ) ;
#96209 = AXIS2_PLACEMENT_3D ( 'NONE', #4064, #77359, #127271 ) ;
#96210 = SURFACE_SIDE_STYLE ('',( #30121 ) ) ;
#96211 = CARTESIAN_POINT ( 'NONE',  ( 4.305816765424046011, -1.865681898550693107, 0.1353468896250972775 ) ) ;
#96212 = CARTESIAN_POINT ( 'NONE',  ( -0.02319159430947542386, 1.394398620246390275, -2.068318759734718792 ) ) ;
#96213 = CARTESIAN_POINT ( 'NONE',  ( 5.830888582329017744, 8.960397891762626799, -1.199719254218452047 ) ) ;
#96214 = CARTESIAN_POINT ( 'NONE',  ( -0.05470795666946129399, -5.634700952767740745, 11.00000000000002487 ) ) ;
#96215 = CARTESIAN_POINT ( 'NONE',  ( -5.819752210671484960, 7.227523004248635807, 1.175121323085267289 ) ) ;
#96216 = CARTESIAN_POINT ( 'NONE',  ( -6.724481002698138532, 6.947575379343695623, -0.7216878364870278340 ) ) ;
#96217 = CARTESIAN_POINT ( 'NONE',  ( 3.225950485047770933, 5.851027101609320269, 1.199719254218450271 ) ) ;
#96218 = CARTESIAN_POINT ( 'NONE',  ( 0.9714669389824581724, -0.2943045352901324518, 1.947222615934702139 ) ) ;
#96219 = CARTESIAN_POINT ( 'NONE',  ( 2.355092412869797869, 0.09611577090188136441, -2.014234804981252847 ) ) ;
#96220 = CARTESIAN_POINT ( 'NONE',  ( -8.179646747746328828, 8.437342715325849341, -0.7998128361456291469 ) ) ;
#96221 = CARTESIAN_POINT ( 'NONE',  ( 6.201928923608456046, 6.200281597156833691, 0.7998128361456352531 ) ) ;
#96222 = CARTESIAN_POINT ( 'NONE',  ( 6.727182134110200273, -0.004969159814478123736, 2.189081792362323586 ) ) ;
#96223 = CARTESIAN_POINT ( 'NONE',  ( 2.994263412949605296, -0.6367403190770392074, -2.096898073876966251 ) ) ;
#96224 = CARTESIAN_POINT ( 'NONE',  ( -5.586581854188635177, 5.810800913040471194, -0.4357733342581562863 ) ) ;
#96225 = CARTESIAN_POINT ( 'NONE',  ( -8.286004436246233951, 12.81875560892930466, 1.040834085586084257E-14 ) ) ;
#96226 = CARTESIAN_POINT ( 'NONE',  ( -1.734723475976807094E-15, -6.134628647623513231, -10.91970695577494332 ) ) ;
#96227 = CARTESIAN_POINT ( 'NONE',  ( -3.929058411375401683, 6.499999999999999112, -0.7500000000000006661 ) ) ;
#96228 = CARTESIAN_POINT ( 'NONE',  ( 4.746763178560261309, 5.670883475476017566, 1.082531754730549078 ) ) ;
#96229 = CARTESIAN_POINT ( 'NONE',  ( 6.909851844459134362, 11.21324425184434936, -0.7998128361456291469 ) ) ;
#96230 =( BOUNDED_SURFACE ( )  B_SPLINE_SURFACE ( 1, 2, ( 
 ( #170261, #87954, #154028, #7752, #22925, #139935, #71675, #203808, #56528, #55453, #138856, #188651, #205962, #123752, #173502, #109620, #125878, #145284, #177749, #43500, #175625, #96522, #212349, #45626, #27212, #191837, #94383, #195054, #30436, #59719, #193978, #178824, #162570, #143155, #174570, #112811, #110676, #14143, #176676, #28288, #208091, #29364, #93318, #80236, #159354, #146335, #63990, #10951, #78100, #111743, #129083, #130142, #196131, #192904, #47771, #13089, #26146, #161508, #92260, #158306, #160423, #77025, #209149, #44560, #60788, #144227, #75974, #9897, #79168, #61857, #46693, #12029, #210221, #142077, #126947, #128024, #62914, #95459, #211290, #69281, #113884, #82356, #150581, #3213, #16271, #15218, #114931, #115993, #201416, #164688, #135394, #133284, #66080, #1085, #200354, #101811, #179879, #149502, #32550, #19479, #31504, #52004, #184115, #98627, #85554, #181982, #33613, #99684, #198231, #118130, #97578, #67149, #165753, #199291, #17339, #167879, #48814, #65033, #166822, #83421, #50936, #163635, #16, #151644, #49867, #197178, #2143, #81308, #148446, #35736, #132221, #147385, #180929, #117060, #183057, #34671, #100741, #18416, #84490, #213411, #131189, #68220, #134351, #4275, #57329, #36798, #107208, #172154, #56266, #168941, #55198, #72491, #203544, #171069, #70346, #138592, #123493, #122425, #120270, #22666, #103956, #88777, #188382, #102883, #71417, #54135, #20543, #139672, #74647, #153766, #137529, #24811, #87691, #187320, #86627, #7488, #38948, #204615, #119189, #121345, #23746, #41099, #40020, #105031, #169999, #189457, #90912, #6419, #154835, #37880, #89851, #155901, #106131, #21586, #73570, #5334, #202482, #205694, #185174, #152694, #173231, #156977, #8566, #186245, #136463, #140752, #53055, #190509, #9632, #44291, #191571, #93051, #175362, #176416, #174302, #178547, #59455, #77833, #10690, #45357, #46418, #125612, #28023, #62641, #26944, #159092, #193714, #158046, #111476, #141824, #75709, #177481, #209949, #207826, #43235, #128799, #30157, #143954, #109352, #76760, #126675, #12816, #194781, #91987, #11759, #211018, #112535, #142882, #206763, #145012, #208884, #96245, #60514, #192638, #25877, #61588, #110413, #162296, #94120, #13883, #79962, #160161, #127757, #29096, #161229, #58395, #124551, #95180, #42166, #78889, #108281, #133021, #134091, #167622, #131959, #14941, #114671, #164421, #196913, #115724, #47498, #51748, #199020, #33344, #100480, #82090, #197969, #195858, #117871, #81036, #34408, #113607, #16005, #101553, #146065, #180665, #182790, #35475, #148183, #214184, #50667, #181715, #166556, #179611, #212078, #98356, #183862, #49600, #31232, #97306, #147123, #19221, #116793, #163365, #65812, #32290, #18144, #84232, #150320, #213149, #64779, #63717, #130920, #1886, #99426, #129875, #48553, #165480, #17076, #83154, #67946, #149234, #808, #66876, #200099, #38695, #152442, #102628, #168684, #135143, #72230, #73305, #106952, #71159, #20288, #53877, #103700, #136205, #54943, #201159, #205441, #138337, #187062, #39761, #21339, #137276, #52798, #57077, #86373, #188130, #118937, #169751, #40843, #85299, #120010, #122163, #189206, #87446, #153515, #204353, #121095, #105866, #184917, #151385, #37620, #123241, #203296, #36541, #4021, #70090, #172975, #56011, #202223, #5084, #185986, #171892, #23489, #89596, #104773, #170822, #2955, #22413, #155645, #88522, #69026, #154584, #6161, #7229, #139407, #190259, #108028, #206510, #58141, #124300, #41917, #156723, #90661, #8314, #24554, #74399, #140500, #196097, #200320, #81267, #99647, #32514, #67110, #68182, #147346, #198194, #84456, #197139, #48778, #1047, #179841, #133246, #163597, #31464, #199251, #17303, #97539, #15180, #150544, #51971, #165714, #213373, #64996, #148412, #34636, #2108, #113846, #33575, #18378, #134313, #114893, #14108, #166784, #164651, #118096, #16235, #82318, #47729, #83382, #131150, #184081, #180892, #35699, #101775, #98589, #132187, #149464, #183020, #80196, #146300, #197476, #212313, #50898, #63948, #117024, #130103, #66043, #49830, #115955, #181945, #100707, #70310, #69245, #168903, #169965, #41062, #4240 ),
 ( #73532, #21551, #87661, #153730, #37842, #106094, #123457, #121308, #5299, #187283, #71380, #155864, #102846, #119152, #6384, #137493, #203509, #3174, #54097, #139634, #103920, #36761, #56228, #167843, #86591, #172117, #152658, #205657, #20506, #55161, #38910, #136427, #104994, #171034, #202442, #189419, #85520, #22630, #88740, #185135, #23711, #151606, #7454, #72455, #154797, #135363, #138554, #204578, #122389, #188346, #120234, #39985, #89819, #57293, #186208, #19440, #201378, #53019, #27984, #90877, #125573, #108243, #74609, #193674, #128765, #207789, #191534, #78849, #141781, #26906, #156939, #61548, #93012, #192599, #173194, #43198, #11720, #95139, #94080, #109312, #9597, #29056, #144970, #60476, #159055, #91948, #143915, #77796, #10649, #158009, #209910, #75674, #42131, #59417, #24776, #140714, #126634, #127715, #175322, #25841, #8530, #45317, #206729, #76724, #62602, #107169, #142840, #111437, #210975, #208845, #44252, #160119, #110374, #177440, #58357, #124512, #176379, #194741, #161189, #190470, #174266, #12776, #142602, #159885, #79696, #26677, #208612, #128544, #129607, #127482, #93847, #158824, #145809, #48291, #10420, #192362, #12549, #11491, #61322, #77564, #76492, #176152, #177209, #175089, #143686, #196651, #194510, #193453, #62380, #47226, #163099, #92779, #210760, #209678, #80776, #60245, #113344, #30971, #45097, #146864, #28823, #94909, #160959, #111206, #179349, #130661, #46158, #78624, #112271, #144748, #14679, #110140, #126402, #13623, #178285, #29894, #44021, #95980, #212885, #162032, #27752, #63453, #211816, #195592, #97046, #64516, #20005, #115461, #182506, #100205, #49342, #1608, #133811, #165210, #135915, #32021, #116516, #67667, #65549, #118653, #98106, #168408, #18935, #117590, #15743, #34136, #199825, #50396, #17863, #131694, #51466, #184639, #183581, #181452, #83946, #16800, #150037, #35188, #164158, #132746, #33082, #81828, #200876, #201933, #533, #198749, #86089, #148961, #166271, #101264, #167348, #152165, #99157, #85020, #36257, #82884, #66600, #151109, #197700, #2675, #68747, #134869, #52521, #102336, #3734, #69809, #114403, #180402, #147911, #213926, #4794, #187845, #74115, #124019, #153224, #73024, #57857, #189984, #22117, #53590, #206230, #204068, #41636, #55720, #121874, #87153, #56792, #54656, #107750, #120804, #173776, #25351, #186781, #171602, #139122, #8025, #91451, #157512, #71945, #9107, #106664, #75183, #40558, #141295, #119724, #39471, #136987, #88229, #138055, #104489, #23195, #169471, #185703, #172689, #155358, #140211, #105570, #89311, #103410, #37337, #203014, #156441, #21056, #6943, #70873, #38407, #154297, #90372, #170532, #205149, #122961, #24267, #188920, #5872, #108816, #207304, #159633, #30712, #110945, #174840, #92529, #208361, #59992, #192108, #143422, #96795, #27489, #13370, #161779, #145561, #126145, #42708, #162844, #43772, #194258, #11229, #125085, #191043, #58926, #26417, #14422, #211559, #80512, #176952, #144493, #62136, #160699, #109885, #10168, #76242, #158569, #175898, #28568, #142351, #179090, #93589, #78373, #193191, #77309, #94655, #12293, #209418, #61063, #127222, #44839, #210501, #128296, #63194, #45904, #46968, #112022, #178023, #29642, #95727, #79444, #129358, #195336, #113084, #166026, #2421, #149785, #213675, #116270, #197449, #182259, #67421, #130412, #164957, #147659, #114158, #18690, #168160, #32828, #16549, #118404, #181200, #66357, #196400, #101012, #132503, #17611, #212627, #82631, #51214, #134626, #133564, #148716, #49090, #68498, #184391, #99962, #198501, #131448, #183335, #117338, #50146, #115210, #286, #180151, #98905, #34939, #64269, #31777, #83697, #167103, #33884, #65300, #48045, #84772, #19758, #97849, #163912, #1359, #199570, #150859, #200630, #15488, #52278, #36011, #146609, #102090, #81576, #105314, #38161, #187596, #172434, #73858, #151917, #121627, #4551, #205977, #3490, #24023, #156191, #70624, #57612, #154047, #5614, #71696, #170280, #90124, #41383, #39223, #137808, #171352, #203827, #139952, #20812, #37080, #138876, #55472, #22945, #135670, #186532, #123770, #21868, #169220, #188671, #173520, #136737, #7767 ) ),
 .UNSPECIFIED., .F., .F., .T. ) 
 B_SPLINE_SURFACE_WITH_KNOTS ( ( 2, 2 ),
 ( 3, 2, 2, 2, 2, 2, 2, 2, 2, 2, 2, 2, 2, 2, 2, 2, 2, 2, 2, 2, 2, 2, 2, 2, 2, 2, 2, 2, 2, 2, 2, 2, 2, 2, 2, 2, 2, 2, 2, 2, 2, 2, 2, 2, 2, 2, 2, 2, 2, 2, 2, 2, 2, 2, 2, 2, 2, 2, 2, 2, 2, 2, 2, 2, 2, 2, 2, 2, 2, 2, 2, 2, 2, 2, 2, 2, 2, 2, 2, 2, 2, 2, 2, 2, 2, 2, 2, 2, 2, 2, 2, 2, 2, 2, 2, 2, 2, 2, 2, 2, 2, 2, 2, 2, 2, 2, 2, 2, 2, 2, 2, 2, 2, 2, 2, 2, 2, 2, 2, 2, 2, 2, 2, 2, 2, 2, 2, 2, 2, 2, 2, 2, 2, 2, 2, 2, 2, 2, 2, 2, 2, 2, 2, 2, 2, 2, 2, 2, 2, 2, 2, 2, 2, 2, 2, 2, 2, 2, 2, 2, 2, 2, 2, 2, 2, 2, 2, 2, 2, 2, 2, 2, 2, 2, 2, 2, 2, 2, 2, 2, 2, 2, 2, 2, 2, 2, 2, 2, 2, 2, 2, 2, 2, 2, 2, 2, 2, 2, 2, 2, 2, 2, 2, 2, 2, 2, 2, 2, 2, 2, 2, 2, 2, 2, 2, 2, 2, 2, 2, 2, 2, 2, 2, 2, 2, 2, 2, 2, 2, 2, 2, 2, 2, 2, 2, 2, 2, 2, 2, 2, 3 ),
 ( 0.000000000000000000, 1.000000000000000000 ),
 ( 0.000000000000000000, 0.004166666666666666609, 0.008333333333333333218, 0.01250000000000000069, 0.01666666666666666644, 0.02083333333333333218, 0.02500000000000000139, 0.02916666666666666713, 0.03333333333333333287, 0.03749999999999999861, 0.04166666666666666435, 0.04583333333333333010, 0.05000000000000000278, 0.05416666666666666852, 0.05833333333333333426, 0.06250000000000000000, 0.06666666666666666574, 0.07083333333333333148, 0.07499999999999999722, 0.07916666666666666297, 0.08333333333333332871, 0.08749999999999999445, 0.09166666666666666019, 0.09583333333333333981, 0.1000000000000000056, 0.1041666666666666713, 0.1083333333333333370, 0.1125000000000000028, 0.1166666666666666685, 0.1208333333333333343, 0.1250000000000000000, 0.1291666666666666796, 0.1333333333333333315, 0.1375000000000000111, 0.1416666666666666630, 0.1458333333333333426, 0.1499999999999999944, 0.1541666666666666741, 0.1583333333333333259, 0.1625000000000000056, 0.1666666666666666574, 0.1708333333333333370, 0.1749999999999999889, 0.1791666666666666685, 0.1833333333333333204, 0.1875000000000000000, 0.1916666666666666796, 0.1958333333333333315, 0.2000000000000000111, 0.2041666666666666630, 0.2083333333333333426, 0.2124999999999999944, 0.2166666666666666741, 0.2208333333333333259, 0.2250000000000000056, 0.2291666666666666574, 0.2333333333333333370, 0.2374999999999999889, 0.2416666666666666685, 0.2458333333333333204, 0.2500000000000000000, 0.2541666666666666519, 0.2583333333333333592, 0.2625000000000000111, 0.2666666666666666630, 0.2708333333333333148, 0.2750000000000000222, 0.2791666666666666741, 0.2833333333333333259, 0.2874999999999999778, 0.2916666666666666852, 0.2958333333333333370, 0.2999999999999999889, 0.3041666666666666408, 0.3083333333333333481, 0.3125000000000000000, 0.3166666666666666519, 0.3208333333333333592, 0.3250000000000000111, 0.3291666666666666630, 0.3333333333333333148, 0.3375000000000000222, 0.3416666666666666741, 0.3458333333333333259, 0.3499999999999999778, 0.3541666666666666852, 0.3583333333333333370, 0.3624999999999999889, 0.3666666666666666408, 0.3708333333333333481, 0.3750000000000000000, 0.3791666666666666519, 0.3833333333333333592, 0.3875000000000000111, 0.3916666666666666630, 0.3958333333333333148, 0.4000000000000000222, 0.4041666666666666741, 0.4083333333333333259, 0.4124999999999999778, 0.4166666666666666852, 0.4208333333333333370, 0.4249999999999999889, 0.4291666666666666408, 0.4333333333333333481, 0.4375000000000000000, 0.4416666666666666519, 0.4458333333333333592, 0.4500000000000000111, 0.4541666666666666630, 0.4583333333333333148, 0.4625000000000000222, 0.4666666666666666741, 0.4708333333333333259, 0.4749999999999999778, 0.4791666666666666852, 0.4833333333333333370, 0.4874999999999999889, 0.4916666666666666408, 0.4958333333333333481, 0.5000000000000000000, 0.5041666666666666519, 0.5083333333333333037, 0.5124999999999999556, 0.5166666666666667185, 0.5208333333333333703, 0.5250000000000000222, 0.5291666666666666741, 0.5333333333333333259, 0.5374999999999999778, 0.5416666666666666297, 0.5458333333333332815, 0.5500000000000000444, 0.5541666666666666963, 0.5583333333333333481, 0.5625000000000000000, 0.5666666666666666519, 0.5708333333333333037, 0.5749999999999999556, 0.5791666666666667185, 0.5833333333333333703, 0.5875000000000000222, 0.5916666666666666741, 0.5958333333333333259, 0.5999999999999999778, 0.6041666666666666297, 0.6083333333333332815, 0.6125000000000000444, 0.6166666666666666963, 0.6208333333333333481, 0.6250000000000000000, 0.6291666666666666519, 0.6333333333333333037, 0.6374999999999999556, 0.6416666666666667185, 0.6458333333333333703, 0.6500000000000000222, 0.6541666666666666741, 0.6583333333333333259, 0.6624999999999999778, 0.6666666666666666297, 0.6708333333333332815, 0.6750000000000000444, 0.6791666666666666963, 0.6833333333333333481, 0.6875000000000000000, 0.6916666666666666519, 0.6958333333333333037, 0.6999999999999999556, 0.7041666666666667185, 0.7083333333333333703, 0.7125000000000000222, 0.7166666666666666741, 0.7208333333333333259, 0.7249999999999999778, 0.7291666666666666297, 0.7333333333333332815, 0.7375000000000000444, 0.7416666666666666963, 0.7458333333333333481, 0.7500000000000000000, 0.7541666666666666519, 0.7583333333333333037, 0.7624999999999999556, 0.7666666666666667185, 0.7708333333333333703, 0.7750000000000000222, 0.7791666666666666741, 0.7833333333333333259, 0.7874999999999999778, 0.7916666666666666297, 0.7958333333333332815, 0.8000000000000000444, 0.8041666666666666963, 0.8083333333333333481, 0.8125000000000000000, 0.8166666666666666519, 0.8208333333333333037, 0.8249999999999999556, 0.8291666666666667185, 0.8333333333333333703, 0.8375000000000000222, 0.8416666666666666741, 0.8458333333333333259, 0.8499999999999999778, 0.8541666666666666297, 0.8583333333333332815, 0.8625000000000000444, 0.8666666666666666963, 0.8708333333333333481, 0.8750000000000000000, 0.8791666666666666519, 0.8833333333333333037, 0.8874999999999999556, 0.8916666666666667185, 0.8958333333333333703, 0.9000000000000000222, 0.9041666666666666741, 0.9083333333333333259, 0.9124999999999999778, 0.9166666666666666297, 0.9208333333333332815, 0.9250000000000000444, 0.9291666666666666963, 0.9333333333333333481, 0.9375000000000000000, 0.9416666666666666519, 0.9458333333333333037, 0.9499999999999999556, 0.9541666666666667185, 0.9583333333333333703, 0.9625000000000000222, 0.9666666666666666741, 0.9708333333333333259, 0.9749999999999999778, 0.9791666666666666297, 0.9833333333333332815, 0.9875000000000000444, 0.9916666666666666963, 0.9958333333333333481, 1.000000000000000000 ),
 .UNSPECIFIED. ) 
 GEOMETRIC_REPRESENTATION_ITEM ( )  RATIONAL_B_SPLINE_SURFACE ( (
 ( 1.000000000000000000, 0.8660254037844387076, 1.000000000000000000, 0.8660254037844387076, 1.000000000000000000, 0.8660254037844387076, 1.000000000000000000, 0.8660254037844387076, 1.000000000000000000, 0.8660254037844387076, 1.000000000000000000, 0.8660254037844387076, 1.000000000000000000, 0.8660254037844387076, 1.000000000000000000, 0.8660254037844387076, 1.000000000000000000, 0.8660254037844387076, 1.000000000000000000, 0.8660254037844387076, 1.000000000000000000, 0.8660254037844387076, 1.000000000000000000, 0.8660254037844387076, 1.000000000000000000, 0.8660254037844387076, 1.000000000000000000, 0.8660254037844387076, 1.000000000000000000, 0.8660254037844387076, 1.000000000000000000, 0.8660254037844387076, 1.000000000000000000, 0.8660254037844387076, 1.000000000000000000, 0.8660254037844387076, 1.000000000000000000, 0.8660254037844387076, 1.000000000000000000, 0.8660254037844387076, 1.000000000000000000, 0.8660254037844387076, 1.000000000000000000, 0.8660254037844387076, 1.000000000000000000, 0.8660254037844387076, 1.000000000000000000, 0.8660254037844387076, 1.000000000000000000, 0.8660254037844387076, 1.000000000000000000, 0.8660254037844387076, 1.000000000000000000, 0.8660254037844387076, 1.000000000000000000, 0.8660254037844387076, 1.000000000000000000, 0.8660254037844387076, 1.000000000000000000, 0.8660254037844387076, 1.000000000000000000, 0.8660254037844387076, 1.000000000000000000, 0.8660254037844387076, 1.000000000000000000, 0.8660254037844387076, 1.000000000000000000, 0.8660254037844387076, 1.000000000000000000, 0.8660254037844387076, 1.000000000000000000, 0.8660254037844387076, 1.000000000000000000, 0.8660254037844387076, 1.000000000000000000, 0.8660254037844387076, 1.000000000000000000, 0.8660254037844387076, 1.000000000000000000, 0.8660254037844387076, 1.000000000000000000, 0.8660254037844387076, 1.000000000000000000, 0.8660254037844387076, 1.000000000000000000, 0.8660254037844387076, 1.000000000000000000, 0.8660254037844387076, 1.000000000000000000, 0.8660254037844387076, 1.000000000000000000, 0.8660254037844387076, 1.000000000000000000, 0.8660254037844387076, 1.000000000000000000, 0.8660254037844387076, 1.000000000000000000, 0.8660254037844387076, 1.000000000000000000, 0.8660254037844387076, 1.000000000000000000, 0.8660254037844387076, 1.000000000000000000, 0.8660254037844387076, 1.000000000000000000, 0.8660254037844387076, 1.000000000000000000, 0.8660254037844387076, 1.000000000000000000, 0.8660254037844387076, 1.000000000000000000, 0.8660254037844387076, 1.000000000000000000, 0.8660254037844387076, 1.000000000000000000, 0.8660254037844387076, 1.000000000000000000, 0.8660254037844387076, 1.000000000000000000, 0.8660254037844387076, 1.000000000000000000, 0.8660254037844387076, 1.000000000000000000, 0.8660254037844387076, 1.000000000000000000, 0.8660254037844387076, 1.000000000000000000, 0.8660254037844387076, 1.000000000000000000, 0.8660254037844387076, 1.000000000000000000, 0.8660254037844387076, 1.000000000000000000, 0.8660254037844387076, 1.000000000000000000, 0.8660254037844387076, 1.000000000000000000, 0.8660254037844387076, 1.000000000000000000, 0.8660254037844387076, 1.000000000000000000, 0.8660254037844387076, 1.000000000000000000, 0.8660254037844387076, 1.000000000000000000, 0.8660254037844387076, 1.000000000000000000, 0.8660254037844387076, 1.000000000000000000, 0.8660254037844387076, 1.000000000000000000, 0.8660254037844387076, 1.000000000000000000, 0.8660254037844387076, 1.000000000000000000, 0.8660254037844387076, 1.000000000000000000, 0.8660254037844387076, 1.000000000000000000, 0.8660254037844387076, 1.000000000000000000, 0.8660254037844387076, 1.000000000000000000, 0.8660254037844387076, 1.000000000000000000, 0.8660254037844387076, 1.000000000000000000, 0.8660254037844387076, 1.000000000000000000, 0.8660254037844387076, 1.000000000000000000, 0.8660254037844387076, 1.000000000000000000, 0.8660254037844387076, 1.000000000000000000, 0.8660254037844387076, 1.000000000000000000, 0.8660254037844387076, 1.000000000000000000, 0.8660254037844387076, 1.000000000000000000, 0.8660254037844387076, 1.000000000000000000, 0.8660254037844387076, 1.000000000000000000, 0.8660254037844387076, 1.000000000000000000, 0.8660254037844387076, 1.000000000000000000, 0.8660254037844387076, 1.000000000000000000, 0.8660254037844387076, 1.000000000000000000, 0.8660254037844387076, 1.000000000000000000, 0.8660254037844387076, 1.000000000000000000, 0.8660254037844387076, 1.000000000000000000, 0.8660254037844387076, 1.000000000000000000, 0.8660254037844387076, 1.000000000000000000, 0.8660254037844387076, 1.000000000000000000, 0.8660254037844387076, 1.000000000000000000, 0.8660254037844387076, 1.000000000000000000, 0.8660254037844387076, 1.000000000000000000, 0.8660254037844387076, 1.000000000000000000, 0.8660254037844387076, 1.000000000000000000, 0.8660254037844387076, 1.000000000000000000, 0.8660254037844387076, 1.000000000000000000, 0.8660254037844387076, 1.000000000000000000, 0.8660254037844387076, 1.000000000000000000, 0.8660254037844387076, 1.000000000000000000, 0.8660254037844387076, 1.000000000000000000, 0.8660254037844387076, 1.000000000000000000, 0.8660254037844387076, 1.000000000000000000, 0.8660254037844387076, 1.000000000000000000, 0.8660254037844387076, 1.000000000000000000, 0.8660254037844387076, 1.000000000000000000, 0.8660254037844387076, 1.000000000000000000, 0.8660254037844387076, 1.000000000000000000, 0.8660254037844387076, 1.000000000000000000, 0.8660254037844387076, 1.000000000000000000, 0.8660254037844387076, 1.000000000000000000, 0.8660254037844387076, 1.000000000000000000, 0.8660254037844387076, 1.000000000000000000, 0.8660254037844387076, 1.000000000000000000, 0.8660254037844387076, 1.000000000000000000, 0.8660254037844387076, 1.000000000000000000, 0.8660254037844387076, 1.000000000000000000, 0.8660254037844387076, 1.000000000000000000, 0.8660254037844387076, 1.000000000000000000, 0.8660254037844387076, 1.000000000000000000, 0.8660254037844387076, 1.000000000000000000, 0.8660254037844387076, 1.000000000000000000, 0.8660254037844387076, 1.000000000000000000, 0.8660254037844387076, 1.000000000000000000, 0.8660254037844387076, 1.000000000000000000, 0.8660254037844387076, 1.000000000000000000, 0.8660254037844387076, 1.000000000000000000, 0.8660254037844387076, 1.000000000000000000, 0.8660254037844387076, 1.000000000000000000, 0.8660254037844387076, 1.000000000000000000, 0.8660254037844387076, 1.000000000000000000, 0.8660254037844387076, 1.000000000000000000, 0.8660254037844387076, 1.000000000000000000, 0.8660254037844387076, 1.000000000000000000, 0.8660254037844387076, 1.000000000000000000, 0.8660254037844387076, 1.000000000000000000, 0.8660254037844387076, 1.000000000000000000, 0.8660254037844387076, 1.000000000000000000, 0.8660254037844387076, 1.000000000000000000, 0.8660254037844387076, 1.000000000000000000, 0.8660254037844387076, 1.000000000000000000, 0.8660254037844387076, 1.000000000000000000, 0.8660254037844387076, 1.000000000000000000, 0.8660254037844387076, 1.000000000000000000, 0.8660254037844387076, 1.000000000000000000, 0.8660254037844387076, 1.000000000000000000, 0.8660254037844387076, 1.000000000000000000, 0.8660254037844387076, 1.000000000000000000, 0.8660254037844387076, 1.000000000000000000, 0.8660254037844387076, 1.000000000000000000, 0.8660254037844387076, 1.000000000000000000, 0.8660254037844387076, 1.000000000000000000, 0.8660254037844387076, 1.000000000000000000, 0.8660254037844387076, 1.000000000000000000, 0.8660254037844387076, 1.000000000000000000, 0.8660254037844387076, 1.000000000000000000, 0.8660254037844387076, 1.000000000000000000, 0.8660254037844387076, 1.000000000000000000, 0.8660254037844387076, 1.000000000000000000, 0.8660254037844387076, 1.000000000000000000, 0.8660254037844387076, 1.000000000000000000, 0.8660254037844387076, 1.000000000000000000, 0.8660254037844387076, 1.000000000000000000, 0.8660254037844387076, 1.000000000000000000, 0.8660254037844387076, 1.000000000000000000, 0.8660254037844387076, 1.000000000000000000, 0.8660254037844387076, 1.000000000000000000, 0.8660254037844387076, 1.000000000000000000, 0.8660254037844387076, 1.000000000000000000, 0.8660254037844387076, 1.000000000000000000, 0.8660254037844387076, 1.000000000000000000, 0.8660254037844387076, 1.000000000000000000, 0.8660254037844387076, 1.000000000000000000, 0.8660254037844387076, 1.000000000000000000, 0.8660254037844387076, 1.000000000000000000, 0.8660254037844387076, 1.000000000000000000, 0.8660254037844387076, 1.000000000000000000, 0.8660254037844387076, 1.000000000000000000, 0.8660254037844387076, 1.000000000000000000, 0.8660254037844387076, 1.000000000000000000, 0.8660254037844387076, 1.000000000000000000, 0.8660254037844387076, 1.000000000000000000, 0.8660254037844387076, 1.000000000000000000, 0.8660254037844387076, 1.000000000000000000, 0.8660254037844387076, 1.000000000000000000, 0.8660254037844387076, 1.000000000000000000, 0.8660254037844387076, 1.000000000000000000, 0.8660254037844387076, 1.000000000000000000, 0.8660254037844387076, 1.000000000000000000, 0.8660254037844387076, 1.000000000000000000, 0.8660254037844387076, 1.000000000000000000, 0.8660254037844387076, 1.000000000000000000, 0.8660254037844387076, 1.000000000000000000, 0.8660254037844387076, 1.000000000000000000, 0.8660254037844387076, 1.000000000000000000, 0.8660254037844387076, 1.000000000000000000, 0.8660254037844387076, 1.000000000000000000, 0.8660254037844387076, 1.000000000000000000, 0.8660254037844387076, 1.000000000000000000, 0.8660254037844387076, 1.000000000000000000, 0.8660254037844387076, 1.000000000000000000, 0.8660254037844387076, 1.000000000000000000, 0.8660254037844387076, 1.000000000000000000, 0.8660254037844387076, 1.000000000000000000, 0.8660254037844387076, 1.000000000000000000, 0.8660254037844387076, 1.000000000000000000, 0.8660254037844387076, 1.000000000000000000, 0.8660254037844387076, 1.000000000000000000, 0.8660254037844387076, 1.000000000000000000, 0.8660254037844387076, 1.000000000000000000, 0.8660254037844387076, 1.000000000000000000, 0.8660254037844387076, 1.000000000000000000, 0.8660254037844387076, 1.000000000000000000, 0.8660254037844387076, 1.000000000000000000, 0.8660254037844387076, 1.000000000000000000, 0.8660254037844387076, 1.000000000000000000, 0.8660254037844387076, 1.000000000000000000, 0.8660254037844387076, 1.000000000000000000, 0.8660254037844387076, 1.000000000000000000, 0.8660254037844387076, 1.000000000000000000, 0.8660254037844387076, 1.000000000000000000, 0.8660254037844387076, 1.000000000000000000, 0.8660254037844387076, 1.000000000000000000, 0.8660254037844387076, 1.000000000000000000, 0.8660254037844387076, 1.000000000000000000, 0.8660254037844387076, 1.000000000000000000, 0.8660254037844387076, 1.000000000000000000, 0.8660254037844387076, 1.000000000000000000),
 ( 1.000000000000000000, 0.8660254037844387076, 1.000000000000000000, 0.8660254037844387076, 1.000000000000000000, 0.8660254037844387076, 1.000000000000000000, 0.8660254037844387076, 1.000000000000000000, 0.8660254037844387076, 1.000000000000000000, 0.8660254037844387076, 1.000000000000000000, 0.8660254037844387076, 1.000000000000000000, 0.8660254037844387076, 1.000000000000000000, 0.8660254037844387076, 1.000000000000000000, 0.8660254037844387076, 1.000000000000000000, 0.8660254037844387076, 1.000000000000000000, 0.8660254037844387076, 1.000000000000000000, 0.8660254037844387076, 1.000000000000000000, 0.8660254037844387076, 1.000000000000000000, 0.8660254037844387076, 1.000000000000000000, 0.8660254037844387076, 1.000000000000000000, 0.8660254037844387076, 1.000000000000000000, 0.8660254037844387076, 1.000000000000000000, 0.8660254037844387076, 1.000000000000000000, 0.8660254037844387076, 1.000000000000000000, 0.8660254037844387076, 1.000000000000000000, 0.8660254037844387076, 1.000000000000000000, 0.8660254037844387076, 1.000000000000000000, 0.8660254037844387076, 1.000000000000000000, 0.8660254037844387076, 1.000000000000000000, 0.8660254037844387076, 1.000000000000000000, 0.8660254037844387076, 1.000000000000000000, 0.8660254037844387076, 1.000000000000000000, 0.8660254037844387076, 1.000000000000000000, 0.8660254037844387076, 1.000000000000000000, 0.8660254037844387076, 1.000000000000000000, 0.8660254037844387076, 1.000000000000000000, 0.8660254037844387076, 1.000000000000000000, 0.8660254037844387076, 1.000000000000000000, 0.8660254037844387076, 1.000000000000000000, 0.8660254037844387076, 1.000000000000000000, 0.8660254037844387076, 1.000000000000000000, 0.8660254037844387076, 1.000000000000000000, 0.8660254037844387076, 1.000000000000000000, 0.8660254037844387076, 1.000000000000000000, 0.8660254037844387076, 1.000000000000000000, 0.8660254037844387076, 1.000000000000000000, 0.8660254037844387076, 1.000000000000000000, 0.8660254037844387076, 1.000000000000000000, 0.8660254037844387076, 1.000000000000000000, 0.8660254037844387076, 1.000000000000000000, 0.8660254037844387076, 1.000000000000000000, 0.8660254037844387076, 1.000000000000000000, 0.8660254037844387076, 1.000000000000000000, 0.8660254037844387076, 1.000000000000000000, 0.8660254037844387076, 1.000000000000000000, 0.8660254037844387076, 1.000000000000000000, 0.8660254037844387076, 1.000000000000000000, 0.8660254037844387076, 1.000000000000000000, 0.8660254037844387076, 1.000000000000000000, 0.8660254037844387076, 1.000000000000000000, 0.8660254037844387076, 1.000000000000000000, 0.8660254037844387076, 1.000000000000000000, 0.8660254037844387076, 1.000000000000000000, 0.8660254037844387076, 1.000000000000000000, 0.8660254037844387076, 1.000000000000000000, 0.8660254037844387076, 1.000000000000000000, 0.8660254037844387076, 1.000000000000000000, 0.8660254037844387076, 1.000000000000000000, 0.8660254037844387076, 1.000000000000000000, 0.8660254037844387076, 1.000000000000000000, 0.8660254037844387076, 1.000000000000000000, 0.8660254037844387076, 1.000000000000000000, 0.8660254037844387076, 1.000000000000000000, 0.8660254037844387076, 1.000000000000000000, 0.8660254037844387076, 1.000000000000000000, 0.8660254037844387076, 1.000000000000000000, 0.8660254037844387076, 1.000000000000000000, 0.8660254037844387076, 1.000000000000000000, 0.8660254037844387076, 1.000000000000000000, 0.8660254037844387076, 1.000000000000000000, 0.8660254037844387076, 1.000000000000000000, 0.8660254037844387076, 1.000000000000000000, 0.8660254037844387076, 1.000000000000000000, 0.8660254037844387076, 1.000000000000000000, 0.8660254037844387076, 1.000000000000000000, 0.8660254037844387076, 1.000000000000000000, 0.8660254037844387076, 1.000000000000000000, 0.8660254037844387076, 1.000000000000000000, 0.8660254037844387076, 1.000000000000000000, 0.8660254037844387076, 1.000000000000000000, 0.8660254037844387076, 1.000000000000000000, 0.8660254037844387076, 1.000000000000000000, 0.8660254037844387076, 1.000000000000000000, 0.8660254037844387076, 1.000000000000000000, 0.8660254037844387076, 1.000000000000000000, 0.8660254037844387076, 1.000000000000000000, 0.8660254037844387076, 1.000000000000000000, 0.8660254037844387076, 1.000000000000000000, 0.8660254037844387076, 1.000000000000000000, 0.8660254037844387076, 1.000000000000000000, 0.8660254037844387076, 1.000000000000000000, 0.8660254037844387076, 1.000000000000000000, 0.8660254037844387076, 1.000000000000000000, 0.8660254037844387076, 1.000000000000000000, 0.8660254037844387076, 1.000000000000000000, 0.8660254037844387076, 1.000000000000000000, 0.8660254037844387076, 1.000000000000000000, 0.8660254037844387076, 1.000000000000000000, 0.8660254037844387076, 1.000000000000000000, 0.8660254037844387076, 1.000000000000000000, 0.8660254037844387076, 1.000000000000000000, 0.8660254037844387076, 1.000000000000000000, 0.8660254037844387076, 1.000000000000000000, 0.8660254037844387076, 1.000000000000000000, 0.8660254037844387076, 1.000000000000000000, 0.8660254037844387076, 1.000000000000000000, 0.8660254037844387076, 1.000000000000000000, 0.8660254037844387076, 1.000000000000000000, 0.8660254037844387076, 1.000000000000000000, 0.8660254037844387076, 1.000000000000000000, 0.8660254037844387076, 1.000000000000000000, 0.8660254037844387076, 1.000000000000000000, 0.8660254037844387076, 1.000000000000000000, 0.8660254037844387076, 1.000000000000000000, 0.8660254037844387076, 1.000000000000000000, 0.8660254037844387076, 1.000000000000000000, 0.8660254037844387076, 1.000000000000000000, 0.8660254037844387076, 1.000000000000000000, 0.8660254037844387076, 1.000000000000000000, 0.8660254037844387076, 1.000000000000000000, 0.8660254037844387076, 1.000000000000000000, 0.8660254037844387076, 1.000000000000000000, 0.8660254037844387076, 1.000000000000000000, 0.8660254037844387076, 1.000000000000000000, 0.8660254037844387076, 1.000000000000000000, 0.8660254037844387076, 1.000000000000000000, 0.8660254037844387076, 1.000000000000000000, 0.8660254037844387076, 1.000000000000000000, 0.8660254037844387076, 1.000000000000000000, 0.8660254037844387076, 1.000000000000000000, 0.8660254037844387076, 1.000000000000000000, 0.8660254037844387076, 1.000000000000000000, 0.8660254037844387076, 1.000000000000000000, 0.8660254037844387076, 1.000000000000000000, 0.8660254037844387076, 1.000000000000000000, 0.8660254037844387076, 1.000000000000000000, 0.8660254037844387076, 1.000000000000000000, 0.8660254037844387076, 1.000000000000000000, 0.8660254037844387076, 1.000000000000000000, 0.8660254037844387076, 1.000000000000000000, 0.8660254037844387076, 1.000000000000000000, 0.8660254037844387076, 1.000000000000000000, 0.8660254037844387076, 1.000000000000000000, 0.8660254037844387076, 1.000000000000000000, 0.8660254037844387076, 1.000000000000000000, 0.8660254037844387076, 1.000000000000000000, 0.8660254037844387076, 1.000000000000000000, 0.8660254037844387076, 1.000000000000000000, 0.8660254037844387076, 1.000000000000000000, 0.8660254037844387076, 1.000000000000000000, 0.8660254037844387076, 1.000000000000000000, 0.8660254037844387076, 1.000000000000000000, 0.8660254037844387076, 1.000000000000000000, 0.8660254037844387076, 1.000000000000000000, 0.8660254037844387076, 1.000000000000000000, 0.8660254037844387076, 1.000000000000000000, 0.8660254037844387076, 1.000000000000000000, 0.8660254037844387076, 1.000000000000000000, 0.8660254037844387076, 1.000000000000000000, 0.8660254037844387076, 1.000000000000000000, 0.8660254037844387076, 1.000000000000000000, 0.8660254037844387076, 1.000000000000000000, 0.8660254037844387076, 1.000000000000000000, 0.8660254037844387076, 1.000000000000000000, 0.8660254037844387076, 1.000000000000000000, 0.8660254037844387076, 1.000000000000000000, 0.8660254037844387076, 1.000000000000000000, 0.8660254037844387076, 1.000000000000000000, 0.8660254037844387076, 1.000000000000000000, 0.8660254037844387076, 1.000000000000000000, 0.8660254037844387076, 1.000000000000000000, 0.8660254037844387076, 1.000000000000000000, 0.8660254037844387076, 1.000000000000000000, 0.8660254037844387076, 1.000000000000000000, 0.8660254037844387076, 1.000000000000000000, 0.8660254037844387076, 1.000000000000000000, 0.8660254037844387076, 1.000000000000000000, 0.8660254037844387076, 1.000000000000000000, 0.8660254037844387076, 1.000000000000000000, 0.8660254037844387076, 1.000000000000000000, 0.8660254037844387076, 1.000000000000000000, 0.8660254037844387076, 1.000000000000000000, 0.8660254037844387076, 1.000000000000000000, 0.8660254037844387076, 1.000000000000000000, 0.8660254037844387076, 1.000000000000000000, 0.8660254037844387076, 1.000000000000000000, 0.8660254037844387076, 1.000000000000000000, 0.8660254037844387076, 1.000000000000000000, 0.8660254037844387076, 1.000000000000000000, 0.8660254037844387076, 1.000000000000000000, 0.8660254037844387076, 1.000000000000000000, 0.8660254037844387076, 1.000000000000000000, 0.8660254037844387076, 1.000000000000000000, 0.8660254037844387076, 1.000000000000000000, 0.8660254037844387076, 1.000000000000000000, 0.8660254037844387076, 1.000000000000000000, 0.8660254037844387076, 1.000000000000000000, 0.8660254037844387076, 1.000000000000000000, 0.8660254037844387076, 1.000000000000000000, 0.8660254037844387076, 1.000000000000000000, 0.8660254037844387076, 1.000000000000000000, 0.8660254037844387076, 1.000000000000000000, 0.8660254037844387076, 1.000000000000000000, 0.8660254037844387076, 1.000000000000000000, 0.8660254037844387076, 1.000000000000000000, 0.8660254037844387076, 1.000000000000000000, 0.8660254037844387076, 1.000000000000000000, 0.8660254037844387076, 1.000000000000000000, 0.8660254037844387076, 1.000000000000000000, 0.8660254037844387076, 1.000000000000000000, 0.8660254037844387076, 1.000000000000000000, 0.8660254037844387076, 1.000000000000000000, 0.8660254037844387076, 1.000000000000000000, 0.8660254037844387076, 1.000000000000000000, 0.8660254037844387076, 1.000000000000000000, 0.8660254037844387076, 1.000000000000000000, 0.8660254037844387076, 1.000000000000000000, 0.8660254037844387076, 1.000000000000000000, 0.8660254037844387076, 1.000000000000000000, 0.8660254037844387076, 1.000000000000000000, 0.8660254037844387076, 1.000000000000000000, 0.8660254037844387076, 1.000000000000000000, 0.8660254037844387076, 1.000000000000000000, 0.8660254037844387076, 1.000000000000000000, 0.8660254037844387076, 1.000000000000000000, 0.8660254037844387076, 1.000000000000000000, 0.8660254037844387076, 1.000000000000000000, 0.8660254037844387076, 1.000000000000000000, 0.8660254037844387076, 1.000000000000000000, 0.8660254037844387076, 1.000000000000000000, 0.8660254037844387076, 1.000000000000000000, 0.8660254037844387076, 1.000000000000000000, 0.8660254037844387076, 1.000000000000000000, 0.8660254037844387076, 1.000000000000000000) ) ) 
 REPRESENTATION_ITEM ( '' )  SURFACE ( )  );
#96231 = CARTESIAN_POINT ( 'NONE',  ( -1.598423149420354905, 8.713846000021355565, -2.499999999999995115 ) ) ;
#96232 = CARTESIAN_POINT ( 'NONE',  ( 7.377044979611483200, 7.779176362401098999, -0.7216878364870317197 ) ) ;
#96233 = ORIENTED_EDGE ( 'NONE', *, *, #59329, .F. ) ;
#96235 = CARTESIAN_POINT ( 'NONE',  ( 1.453772141523026251, -1.459646937795316068, -1.386592938616920678 ) ) ;
#96234 = CARTESIAN_POINT ( 'NONE',  ( 5.020983453748395497, -1.746657797055195305, 0.5827527221545365510 ) ) ;
#96236 = CARTESIAN_POINT ( 'NONE',  ( 3.937115517079175842, 1.273119805769900026, 1.913412639830965434 ) ) ;
#96238 = CARTESIAN_POINT ( 'NONE',  ( 2.570971337753673147, 1.659905555536644872, 0.8415416509589612737 ) ) ;
#96237 = CARTESIAN_POINT ( 'NONE',  ( -0.02900071798685523866, 4.082342745036794618, -2.728474045032194262 ) ) ;
#96239 = CARTESIAN_POINT ( 'NONE',  ( 3.285556943750000070, -2.734374999522042771, 0.000000000000000000 ) ) ;
#96240 = CARTESIAN_POINT ( 'NONE',  ( 6.047114369478562956, 0.1942372860762129894, 1.902532258075719351 ) ) ;
#96241 = CARTESIAN_POINT ( 'NONE',  ( -9.182950115157607840, 9.607863310639020327, 0.7998128361456462443 ) ) ;
#96242 = CARTESIAN_POINT ( 'NONE',  ( -6.807602527837528505, 7.114826835331461652, 0.7216878364870317197 ) ) ;
#96244 = CARTESIAN_POINT ( 'NONE',  ( 3.256579335763456040, -1.417408692332474462, 1.220890361658559575 ) ) ;
#96243 = CARTESIAN_POINT ( 'NONE',  ( 5.249593148720715696, 2.088313038247250120, -0.1037309089504182269 ) ) ;
#96245 = CARTESIAN_POINT ( 'NONE',  ( 7.456621297836082185, 7.801739057004660971, 0.7216878364870317197 ) ) ;
#96246 = CARTESIAN_POINT ( 'NONE',  ( 6.110883706712432861, -0.2185277653131960651, 1.828168259763853776 ) ) ;
#96247 = CARTESIAN_POINT ( 'NONE',  ( 4.681643115420508039, 4.356338477612361260, 0.7998128361456341429 ) ) ;
#96248 = DIRECTION ( 'NONE',  ( 5.578564026256490882E-16, 1.000000000000000000, 9.066213480720158442E-32 ) ) ;
#96249 = CARTESIAN_POINT ( 'NONE',  ( 5.391107817497476695, 1.518517088589757424, -0.8181074574388611520 ) ) ;
#96250 = CARTESIAN_POINT ( 'NONE',  ( -6.226218857173722476, 8.287007971501239467, 1.599625672291283607 ) ) ;
#96251 = CARTESIAN_POINT ( 'NONE',  ( 0.7911957196942709380, 1.314039333434241508, -1.131676627359794240 ) ) ;
#96252 = CARTESIAN_POINT ( 'NONE',  ( 1.836970198721030181E-16, 13.49999999999999822, 1.500000000000000222 ) ) ;
#96253 = CARTESIAN_POINT ( 'NONE',  ( 1.893304937267579202, 3.295344712542831900, 0.4038802767148412798 ) ) ;
#96254 = CARTESIAN_POINT ( 'NONE',  ( 4.750930541093643100, -0.4693155065514472701, -2.119606683777853995 ) ) ;
#96255 = CARTESIAN_POINT ( 'NONE',  ( 3.527797039230845311, -1.088449851438414218, -1.465592618984489670 ) ) ;
#96256 = CARTESIAN_POINT ( 'NONE',  ( 1.059338230090471011, 1.600537254139059673, 1.134074526779847769 ) ) ;
#96257 = CARTESIAN_POINT ( 'NONE',  ( 0.3689691111537584112, -0.2640367098126532031, -2.100658933187772526 ) ) ;
#96258 = ADVANCED_FACE ( 'NONE', ( #178433 ), #164643, .T. ) ;
#96260 = CARTESIAN_POINT ( 'NONE',  ( -1.364683531250012516, 4.301041667008089320, -0.7879004041258300672 ) ) ;
#96259 = CARTESIAN_POINT ( 'NONE',  ( 0.1469514510107531868, -1.837142584329341410, 1.370738489780512825 ) ) ;
#96261 = CARTESIAN_POINT ( 'NONE',  ( 10.36809559534897573, -7.321523296574929063, -0.4642244361878615222 ) ) ;
#96262 = CARTESIAN_POINT ( 'NONE',  ( 9.077347539549325717, 10.54899253668443393, -1.199719254218446718 ) ) ;
#96263 = CARTESIAN_POINT ( 'NONE',  ( 3.018346832952636394, -2.117961878424143407, 0.1061830045200745365 ) ) ;
#96264 = CARTESIAN_POINT ( 'NONE',  ( -4.799223189557577207, 4.701441264013013210, 0.7216878364870317197 ) ) ;
#96265 = EDGE_CURVE ( 'NONE', #201912, #200114, #136512, .T. ) ;
#96266 = CARTESIAN_POINT ( 'NONE',  ( 5.599506603007033512, 5.747200726622710754, 0.6510759304539673886 ) ) ;
#96267 = CARTESIAN_POINT ( 'NONE',  ( -5.219525951136862574, 5.191794485855519170, -0.7216878364870197293 ) ) ;
#96269 = AXIS2_PLACEMENT_3D ( 'NONE', #96404, #162454, #46575 ) ;
#96268 = VECTOR ( 'NONE', #114947, 1000.000000000000000 ) ;
#96270 = CARTESIAN_POINT ( 'NONE',  ( 0.7079804021624566124, 0.6528548590773940452, -1.964656565413371414 ) ) ;
#96272 = CARTESIAN_POINT ( 'NONE',  ( 1.500000000000001332, 13.65625000068279604, 0.000000000000000000 ) ) ;
#96271 = CARTESIAN_POINT ( 'NONE',  ( 6.983263157960363898, 2.958708369276577432, 2.506372104999963657 ) ) ;
#96274 = ORIENTED_EDGE ( 'NONE', *, *, #15120, .F. ) ;
#96273 = CARTESIAN_POINT ( 'NONE',  ( 2.508681548337174494, -2.215532678404589007, -0.1606611847707327678 ) ) ;
#96275 = CARTESIAN_POINT ( 'NONE',  ( 0.9679111143040418641, -2.244285626452859450, -0.4966636800145701747 ) ) ;
#96277 = CARTESIAN_POINT ( 'NONE',  ( 5.137578304370245874, 1.926469575665398448, -0.7373178810637993630 ) ) ;
#96276 = CARTESIAN_POINT ( 'NONE',  ( 2.171277156482887882, 5.684907115872006145, -0.7998128361456291469 ) ) ;
#96279 = CARTESIAN_POINT ( 'NONE',  ( 3.475000000000000533, -1.225000000000000311, 0.000000000000000000 ) ) ;
#96278 = CARTESIAN_POINT ( 'NONE',  ( 6.150558962454855561, 7.204682206732687000, 1.199719254218452047 ) ) ;
#96280 = CARTESIAN_POINT ( 'NONE',  ( 6.249382461256315580, 6.255644057745969988, -0.7998128361456481317 ) ) ;
#96281 = CARTESIAN_POINT ( 'NONE',  ( 0.1333542156527113831, 2.876250315000815405, -2.534448870308704915 ) ) ;
#96282 = CARTESIAN_POINT ( 'NONE',  ( 5.354971380013192395, 0.3533838956982695567, -1.806849549699687696 ) ) ;
#96283 = CARTESIAN_POINT ( 'NONE',  ( 3.520313441042647540, 7.258782781191745137, 0.7998128361456321445 ) ) ;
#96284 =( NAMED_UNIT ( * ) SI_UNIT ( $, .STERADIAN. ) SOLID_ANGLE_UNIT ( ) );
#96285 = CARTESIAN_POINT ( 'NONE',  ( 1.992754126006650806, 1.502677205460640764, -0.8464738358340985203 ) ) ;
#96286 = CARTESIAN_POINT ( 'NONE',  ( 0.9894706735516716201, -0.4852629857438545691, 1.957171443305204761 ) ) ;
#96287 = CARTESIAN_POINT ( 'NONE',  ( 1.793957786719975633, 1.699999873817940044, -1.547402956443538313 ) ) ;
#96288 = CARTESIAN_POINT ( 'NONE',  ( -1.364683531250012516, 3.801041667008087099, -0.7879004041258300672 ) ) ;
#96289 = CARTESIAN_POINT ( 'NONE',  ( 2.038691496156146865, 2.237626877524625524, 0.3332970034419027727 ) ) ;
#96290 = CARTESIAN_POINT ( 'NONE',  ( 4.547555978022395529, -1.627529793438415417, -1.336665591334128100 ) ) ;
#96291 = CARTESIAN_POINT ( 'NONE',  ( -2.986538976760251263, 6.706322249520737522, -0.7998128361456481317 ) ) ;
#96292 = CARTESIAN_POINT ( 'NONE',  ( 2.178617772012156006, -0.08127397458944020381, -1.767985329221566815 ) ) ;
#96293 = CARTESIAN_POINT ( 'NONE',  ( 6.257251587906815793, 7.258880593101466161, 1.199719254218462483 ) ) ;
#96295 = CARTESIAN_POINT ( 'NONE',  ( 5.337530604160453329, 0.9314408107504292822, -2.094771667654048208 ) ) ;
#96294 = CARTESIAN_POINT ( 'NONE',  ( 3.729901657090938460, 7.365652676665848553, 0.7216878364870257245 ) ) ;
#96296 = CARTESIAN_POINT ( 'NONE',  ( -4.466521540698216164, 7.298359999868178960, -1.199719254218452047 ) ) ;
#96297 = CARTESIAN_POINT ( 'NONE',  ( 1.499999999999987121, 2.295833333333350268, -0.8660254037844262731 ) ) ;
#96298 = CARTESIAN_POINT ( 'NONE',  ( 4.066501749483540706, -2.044453849244652233, -0.7895499924894524568 ) ) ;
#96299 = CARTESIAN_POINT ( 'NONE',  ( -3.948449050077848632, 5.629609863222681199, 1.599625672291267398 ) ) ;
#96300 = CARTESIAN_POINT ( 'NONE',  ( -0.006913841192830532355, 8.234242197375163386, -1.999988128101762186 ) ) ;
#96301 = CARTESIAN_POINT ( 'NONE',  ( 0.4638907948587486785, -7.079050064870604508, 10.61081979358357863 ) ) ;
#96302 = CARTESIAN_POINT ( 'NONE',  ( 1.364683531249986537, 2.655208333674754062, -0.7879004041258239610 ) ) ;
#96303 = CARTESIAN_POINT ( 'NONE',  ( 3.756402471274498112, 0.6942424141608801724, 1.797233106274237713 ) ) ;
#96304 = CARTESIAN_POINT ( 'NONE',  ( -8.012344526598182026E-15, 8.546875000341403350, -1.575800808251669460 ) ) ;
#96305 = CARTESIAN_POINT ( 'NONE',  ( -3.904385051055635270, 6.538571078664754843, 1.082531754730560403 ) ) ;
#96306 = CARTESIAN_POINT ( 'NONE',  ( 6.099870585610251084, 1.463495690422533579, 1.534846084132005961 ) ) ;
#96307 = CARTESIAN_POINT ( 'NONE',  ( -5.424670859243583720, 8.382514198209223721, 1.082531754730550855 ) ) ;
#96308 = ORIENTED_EDGE ( 'NONE', *, *, #16302, .T. ) ;
#96310 = DIRECTION ( 'NONE',  ( -0.000000000000000000, -1.000000000000000000, -0.000000000000000000 ) ) ;
#96309 = CARTESIAN_POINT ( 'NONE',  ( -5.072158865288277418, 7.010880990960010273, 1.443375672974058777 ) ) ;
#96311 = CARTESIAN_POINT ( 'NONE',  ( 4.273844736805816780, 6.009238164405336313, 1.599625672291267398 ) ) ;
#96312 = CARTESIAN_POINT ( 'NONE',  ( 6.216338285296751032, 1.720575329815833721, 0.6561210673821930017 ) ) ;
#96313 = FILL_AREA_STYLE ('',( #81102 ) ) ;
#96314 = CARTESIAN_POINT ( 'NONE',  ( 11.52463353791760348, 13.87999999999998479, 3.346594096177638367 ) ) ;
#96315 = CARTESIAN_POINT ( 'NONE',  ( 1.364683531249988535, 3.926041667008087543, 0.7879004041258500513 ) ) ;
#96316 = CARTESIAN_POINT ( 'NONE',  ( 1.803882474592255258, 1.289405681850508190, -1.169162514946599174 ) ) ;
#96317 = CARTESIAN_POINT ( 'NONE',  ( 6.776323704810607751, -7.189630408300039299, 6.777912011469599207 ) ) ;
#96319 = CARTESIAN_POINT ( 'NONE',  ( 0.1331565106231328843, 0.003911343561965873426, -1.946049565259087455 ) ) ;
#96318 = AXIS2_PLACEMENT_3D ( 'NONE', #3711, #200851, #168387 ) ;
#96320 = CARTESIAN_POINT ( 'NONE',  ( -1.364683531250014514, 0.05104166700808546175, -0.7879004041258359514 ) ) ;
#96321 = CARTESIAN_POINT ( 'NONE',  ( -4.278446361140257892, 7.376938836250866771, -1.009706106759753030 ) ) ;
#96322 = CARTESIAN_POINT ( 'NONE',  ( 6.543834100630380846, 0.8322713294773576020, -1.995267709627518427 ) ) ;
#96323 = CARTESIAN_POINT ( 'NONE',  ( -9.969323024750229578, 10.52529837183042716, -0.7998128361456291469 ) ) ;
#96324 = CARTESIAN_POINT ( 'NONE',  ( -7.009202228140764213, 7.279750142360097875, -0.7216878364870267237 ) ) ;
#96325 = CARTESIAN_POINT ( 'NONE',  ( 5.594645800149128156, -0.5210773734287167391, -2.097845705497362712 ) ) ;
#96327 = ORIENTED_EDGE ( 'NONE', *, *, #159688, .F. ) ;
#96326 = CARTESIAN_POINT ( 'NONE',  ( -4.496464221587651799, 5.274905009054215554, 1.199719254218452935 ) ) ;
#96328 = CARTESIAN_POINT ( 'NONE',  ( -1.364683531249997417, 5.009375000341425022, 1.214306433183764966E-14 ) ) ;
#96329 = CARTESIAN_POINT ( 'NONE',  ( 6.520779640719153392, 1.838571040693348646, 0.7116797190419403840 ) ) ;
#96330 = CARTESIAN_POINT ( 'NONE',  ( 5.870364492519208888, -0.4185229733149243292, 1.682389803524992011 ) ) ;
#96332 = CARTESIAN_POINT ( 'NONE',  ( 2.489988787850425656, -2.185901284972164405, -0.1580625509675498419 ) ) ;
#96331 = CARTESIAN_POINT ( 'NONE',  ( 1.360316468749983576, 0.5156250003414062366, -5.204170427930421283E-15 ) ) ;
#96333 = CARTESIAN_POINT ( 'NONE',  ( 3.241587113499379669, -2.035928198617407592, 1.086232460313860892 ) ) ;
#96334 = CARTESIAN_POINT ( 'NONE',  ( 5.887979924156289790, -0.9304241717780140641, 1.838884224927712419 ) ) ;
#96335 = CARTESIAN_POINT ( 'NONE',  ( 1.394366005188719893, 1.587816662021741543, -1.117778254020968420 ) ) ;
#96336 = CARTESIAN_POINT ( 'NONE',  ( -5.192409643909507544, 9.001635651295671892, 0.7216878364870458196 ) ) ;
#96337 = CARTESIAN_POINT ( 'NONE',  ( -4.842197138736131556, 5.678260079060780008, 1.199719254218452935 ) ) ;
#96338 = CARTESIAN_POINT ( 'NONE',  ( -9.523113341625002448, 14.62187147401989407, 7.301473412126905593 ) ) ;
#96339 = ADVANCED_FACE ( 'NONE', ( #179497 ), #143963, .T. ) ;
#96340 = CARTESIAN_POINT ( 'NONE',  ( 4.482752736079084421, -1.382999391253452615, 1.607682512923855445 ) ) ;
#96341 = CARTESIAN_POINT ( 'NONE',  ( -1.355252715606880543E-15, 4.021557182957054444, 11.93179687198411720 ) ) ;
#96342 = CARTESIAN_POINT ( 'NONE',  ( 2.461564753630896440, -1.930417925741171103, -0.5826551686555282439 ) ) ;
#96343 = CARTESIAN_POINT ( 'NONE',  ( -4.731432421044865499, 8.463828891286912182, -0.7216878364870257245 ) ) ;
#96344 = CARTESIAN_POINT ( 'NONE',  ( 4.050008041959299199, 0.7462531942188169731, -2.076888956485785975 ) ) ;
#96345 = FACE_OUTER_BOUND ( 'NONE', #125951, .T. ) ;
#96346 = CARTESIAN_POINT ( 'NONE',  ( -3.112320638501687053, -3.098081249360057132, -1.430203574381059495 ) ) ;
#96347 = CARTESIAN_POINT ( 'NONE',  ( 11.97181073603049306, 12.22000000000000064, -0.8318477717169578955 ) ) ;
#96348 = CARTESIAN_POINT ( 'NONE',  ( -8.100070429521727178, 8.414780020722290033, 0.7998128361456341429 ) ) ;
#96350 = CARTESIAN_POINT ( 'NONE',  ( 6.825078400183548055, -0.008500281443135982926, 2.244262395727573356 ) ) ;
#96349 = CARTESIAN_POINT ( 'NONE',  ( -5.535867093699859964, 7.544539992772745229, 1.349747212490030046 ) ) ;
#96351 = DIRECTION ( 'NONE',  ( 1.000000000000000000, -5.578564026256490882E-16, -5.570868214615546318E-48 ) ) ;
#96352 = VERTEX_POINT ( 'NONE', #65694 ) ;
#96353 = CARTESIAN_POINT ( 'NONE',  ( 4.082927109850850833, -0.2000173336921743650, -2.051146848037002979 ) ) ;
#96354 = LINE ( 'NONE', #144061, #203026 ) ;
#96355 = CARTESIAN_POINT ( 'NONE',  ( 0.1489494290324722969, -7.995840219786913394, 9.536979704252537715 ) ) ;
#96356 = CARTESIAN_POINT ( 'NONE',  ( -4.608882153641705059, 7.464447381635583412, -1.199719254218452047 ) ) ;
#96357 = CARTESIAN_POINT ( 'NONE',  ( -4.197131071882288289, 7.054347462908075350, -1.199719254218455378 ) ) ;
#96358 = CARTESIAN_POINT ( 'NONE',  ( 3.475264548829166689, -1.782285498782819610, -0.9499825727283210952 ) ) ;
#96359 = CARTESIAN_POINT ( 'NONE',  ( 0.7499999999999885647, 0.7333333333333567072, 1.299038105676657340 ) ) ;
#96360 = STYLED_ITEM ( 'NONE', ( #15380 ), #40567 ) ;
#96362 = CARTESIAN_POINT ( 'NONE',  ( 2.198393463710220264, 5.716542807637226886, 0.7998128361456462443 ) ) ;
#96361 = CARTESIAN_POINT ( 'NONE',  ( -3.318713740295064163, 7.093859473644694269, 0.000000000000000000 ) ) ;
#96363 = CARTESIAN_POINT ( 'NONE',  ( 6.120616281565444794, 9.228137197546649517, -1.199719254218440723 ) ) ;
#96364 = CARTESIAN_POINT ( 'NONE',  ( 3.186453599190769648, -2.030135695866011503, -0.3537577654625714274 ) ) ;
#96365 = CARTESIAN_POINT ( 'NONE',  ( 3.217422812353257555, 1.967887761762876941, 0.4390297752325384995 ) ) ;
#96366 = EDGE_CURVE ( 'NONE', #109852, #39789, #67506, .T. ) ;
#96367 = CARTESIAN_POINT ( 'NONE',  ( 0.000000000000000000, 0.000000000000000000, 0.000000000000000000 ) ) ;
#96368 = CARTESIAN_POINT ( 'NONE',  ( 3.981290663907289140, 7.796589541200495965, -0.7998128361456221525 ) ) ;
#96370 = VERTEX_POINT ( 'NONE', #85173 ) ;
#96369 = CARTESIAN_POINT ( 'NONE',  ( -11.52463353791760348, 9.719999999999982876, 3.346594096177640143 ) ) ;
#96371 = CARTESIAN_POINT ( 'NONE',  ( 1.693040327840355408, -0.6214066371539993527, 1.733238834403828754 ) ) ;
#96372 = CARTESIAN_POINT ( 'NONE',  ( 6.463508838306311510, 0.3818026259072569983, -2.173449913608487716 ) ) ;
#96373 = CARTESIAN_POINT ( 'NONE',  ( 6.412080304620304538, 6.445458208337293549, -0.7998128361456481317 ) ) ;
#96374 = CARTESIAN_POINT ( 'NONE',  ( 3.093221446634909721, 1.855696356685032633, -1.108285163885482039 ) ) ;
#96375 = CIRCLE ( 'NONE', #165609, 0.1000000000000000472 ) ;
#96376 = CARTESIAN_POINT ( 'NONE',  ( -4.284013352238265959, 5.060732334775157604, -1.082531754730544860 ) ) ;
#96377 = CARTESIAN_POINT ( 'NONE',  ( 4.153586450535729391, 2.052860580235102095, -0.5180077198428371110 ) ) ;
#96378 = DIRECTION ( 'NONE',  ( 0.000000000000000000, 0.000000000000000000, 1.000000000000000000 ) ) ;
#96379 = CARTESIAN_POINT ( 'NONE',  ( 1.709613803025863188, -1.856884215550944850, 0.2259493607114013147 ) ) ;
#96380 = CARTESIAN_POINT ( 'NONE',  ( 4.821144081919094049, -0.09777198692111942202, 1.969167557456591666 ) ) ;
#96381 = CARTESIAN_POINT ( 'NONE',  ( 4.575407832915947104, 1.497500392235491029, 1.350737390116145242 ) ) ;
#96383 = CARTESIAN_POINT ( 'NONE',  ( 9.205623113554612047, 12.72334881824701469, 1.082531754730546636 ) ) ;
#96382 = CARTESIAN_POINT ( 'NONE',  ( -1.364683531249997417, 2.759375000341422801, 1.214306433183764966E-14 ) ) ;
#96385 = CARTESIAN_POINT ( 'NONE',  ( 6.111965604441711442, -2.090389680133018846, 0.2559737671669787273 ) ) ;
#96384 = CARTESIAN_POINT ( 'NONE',  ( -5.703176172842872482, 9.805455968292021041, 0.000000000000000000 ) ) ;
#96386 = EDGE_CURVE ( 'NONE', #101960, #146443, #50534, .T. ) ;
#96387 = CARTESIAN_POINT ( 'NONE',  ( 5.073973250452978867, 4.884333311808733313, 0.1550835458496209185 ) ) ;
#96388 = CARTESIAN_POINT ( 'NONE',  ( 5.120175567455225618, 9.125288595339771547, -0.7998128361456281477 ) ) ;
#96389 = CARTESIAN_POINT ( 'NONE',  ( -7.576308911938196999, 7.733448573549685179, 0.7998128361456462443 ) ) ;
#96390 = CARTESIAN_POINT ( 'NONE',  ( 6.639320575229223031, 6.036153810275548537, 2.598155902862766542 ) ) ;
#96391 = CARTESIAN_POINT ( 'NONE',  ( 4.838727080925394830, 0.3361901323847040213, 1.942436603694275510 ) ) ;
#96392 = CARTESIAN_POINT ( 'NONE',  ( 6.064714679231743233, 0.6376439298158544933, 1.916535431269225098 ) ) ;
#96393 = CARTESIAN_POINT ( 'NONE',  ( 0.7499999999999902300, 1.014583334016154526, 1.299038105676657340 ) ) ;
#96394 = CARTESIAN_POINT ( 'NONE',  ( 4.758593218111947465, 0.8799714688421821362, 2.133523255312119726 ) ) ;
#96395 = ADVANCED_FACE ( 'NONE', ( #169627 ), #134004, .T. ) ;
#96396 = CARTESIAN_POINT ( 'NONE',  ( 2.166912933460037660, 1.531321095959611966, -1.381971985785889423 ) ) ;
#96397 = CARTESIAN_POINT ( 'NONE',  ( 6.426201623197458801, 9.480690412830290015, -1.082531754730537088 ) ) ;
#96398 = CARTESIAN_POINT ( 'NONE',  ( 6.717138760927786834, 6.801359740696030443, -0.7998128361456481317 ) ) ;
#96399 = CARTESIAN_POINT ( 'NONE',  ( 5.571474780572990504, 5.464751763615448787, 0.7998128361456352531 ) ) ;
#96400 = CARTESIAN_POINT ( 'NONE',  ( 1.364683531249988757, 1.696875000341414808, 0.000000000000000000 ) ) ;
#96401 = CARTESIAN_POINT ( 'NONE',  ( 4.927462483923885195, 4.713404084191450849, -0.7998128361456481317 ) ) ;
#96402 = CARTESIAN_POINT ( 'NONE',  ( 5.287316719205157334, 9.112360572473935605, 1.040834085586084257E-14 ) ) ;
#96403 = CARTESIAN_POINT ( 'NONE',  ( 4.088457082891777894, 1.164728776245987918, -1.832164736925721682 ) ) ;
#96404 = CARTESIAN_POINT ( 'NONE',  ( -7.065207446497166366, 9.336104335703744539, 0.000000000000000000 ) ) ;
#96406 = CARTESIAN_POINT ( 'NONE',  ( 3.192734241421916419, 1.453351889590439816, 1.130385295574042104 ) ) ;
#96405 = CARTESIAN_POINT ( 'NONE',  ( -2.928197990871687306, 5.399686175116803710, 1.082531754730560403 ) ) ;
#96408 = CARTESIAN_POINT ( 'NONE',  ( 6.620655732516642189, 0.6076529131340856482, 1.780684370158796881 ) ) ;
#96407 = CARTESIAN_POINT ( 'NONE',  ( -1.201851678989727383E-14, 4.196875000341417028, -1.575800808251660134 ) ) ;
#96409 = CARTESIAN_POINT ( 'NONE',  ( 5.671465802443460547, 1.304529079428708549, 1.760837017921567771 ) ) ;
#96410 = CARTESIAN_POINT ( 'NONE',  ( 7.885016188448159546, 14.36996334327324476, 9.048771281106397169 ) ) ;
#96411 = CARTESIAN_POINT ( 'NONE',  ( 6.420815857685610695, 2.108269355124866351, 0.8215519888849237562 ) ) ;
#96412 = B_SPLINE_CURVE_WITH_KNOTS ( 'NONE', 3,
 ( #140627, #161108, #79844, #12695, #213027, #93997, #97193 ),
 .UNSPECIFIED., .F., .F.,
 ( 4, 3, 4 ),
 ( 0.000000000000000000, 3.302246092615816574E-05, 4.223956139718768900E-05 ),
 .UNSPECIFIED. ) ;
#96413 = CARTESIAN_POINT ( 'NONE',  ( -5.461413243215608837, 6.444398994036877326, -1.303746704243381238 ) ) ;
#96414 = CARTESIAN_POINT ( 'NONE',  ( 4.617922728991994852, 8.461530327540957686, 0.3091873533234041904 ) ) ;
#96415 = CARTESIAN_POINT ( 'NONE',  ( -4.787437638956920871, 8.599444655509458357, -0.7216878364870338292 ) ) ;
#96416 = CARTESIAN_POINT ( 'NONE',  ( -3.147653791585727667, 8.920000000000001705, 2.499999999999999556 ) ) ;
#96417 = CARTESIAN_POINT ( 'NONE',  ( 0.9359865740741512008, 1.742660192269055663, 0.3080425777817352162 ) ) ;
#96419 = CARTESIAN_POINT ( 'NONE',  ( 4.705731023397805579, 1.493295645070455535, 1.350234862845017592 ) ) ;
#96418 = CIRCLE ( 'NONE', #23857, 0.1000000000000000472 ) ;
#96420 = CARTESIAN_POINT ( 'NONE',  ( 5.445571254183207088, 9.504916896522420444, -0.7998128361456281477 ) ) ;
#96421 = CARTESIAN_POINT ( 'NONE',  ( 2.924945619078959336, 1.982447918529605557, 0.7109604360746536456 ) ) ;
#96422 = CARTESIAN_POINT ( 'NONE',  ( 1.563933522115690922, -1.023182376180698849, 1.619245466209729756 ) ) ;
#96423 = CARTESIAN_POINT ( 'NONE',  ( 2.900554798319789906, 5.471398800426671372, 1.199719254218452047 ) ) ;
#96424 = CARTESIAN_POINT ( 'NONE',  ( 3.086336304319175383, 1.096367280595906601, -1.635968976963786847 ) ) ;
#96425 = CARTESIAN_POINT ( 'NONE',  ( 5.361584196017279424, -1.594725845915157647, -1.239436484511841519 ) ) ;
#96426 = CARTESIAN_POINT ( 'NONE',  ( 1.445950363956361340, 1.868363765441739099, 0.09516058986362013750 ) ) ;
#96427 = CARTESIAN_POINT ( 'NONE',  ( 1.715213470010600538, -1.680963409367957295, -1.011360081469035999 ) ) ;
#96430 = VERTEX_POINT ( 'NONE', #203171 ) ;
#96429 = CARTESIAN_POINT ( 'NONE',  ( 1.371198541116287917, -1.641758494746584418, -0.9804709962101465504 ) ) ;
#96428 = CARTESIAN_POINT ( 'NONE',  ( 3.791373243616827704, 1.250846937323921715, 1.187934608979845708 ) ) ;
#96432 = CARTESIAN_POINT ( 'NONE',  ( 6.005898861173831094, 6.109229547565340646, 1.040834085586084257E-14 ) ) ;
#96431 = CARTESIAN_POINT ( 'NONE',  ( 1.067327838873022516, -1.996528553209110379, -0.9406146916221403975 ) ) ;
#96433 = CARTESIAN_POINT ( 'NONE',  ( 1.364683531249986537, 1.467708333674748289, -0.7879004041258239610 ) ) ;
#96434 = CARTESIAN_POINT ( 'NONE',  ( 7.228468454380276853, 11.58496363008569574, 1.040834085586084257E-14 ) ) ;
#96435 = CARTESIAN_POINT ( 'NONE',  ( 6.807498166657679484, -0.4075194142965677391, 1.832415718333743282 ) ) ;
#96436 = CARTESIAN_POINT ( 'NONE',  ( 0.5625979714343026794, 6.581402773648894033, -3.408537031531792660 ) ) ;
#96437 = CARTESIAN_POINT ( 'NONE',  ( -3.730464822054482710, 7.503959392372201442, 1.040834085586084257E-14 ) ) ;
#96438 = B_SPLINE_CURVE_WITH_KNOTS ( 'NONE', 3,
 ( #155523, #190141, #8191, #156599, #7104, #203172, #189083, #38569 ),
 .UNSPECIFIED., .F., .F.,
 ( 4, 2, 2, 4 ),
 ( 1.065747948313845892E-15, 0.0004636157603174433485, 0.0006954236404756316495, 0.0009272315206338199505 ),
 .UNSPECIFIED. ) ;
#96439 = CARTESIAN_POINT ( 'NONE',  ( 6.578973861349465935, 1.929489650308688464, 0.7507879531711419974 ) ) ;
#96440 = VECTOR ( 'NONE', #126450, 1000.000000000000000 ) ;
#96441 = CARTESIAN_POINT ( 'NONE',  ( 0.5728211633247158874, 1.428863753495920763, -1.498466819491943269 ) ) ;
#96442 = CARTESIAN_POINT ( 'NONE',  ( -1.201851678989727383E-14, 1.462500000000018119, 1.732050807568877637 ) ) ;
#96443 = CARTESIAN_POINT ( 'NONE',  ( 6.317209508963599340, 9.457495962844502557, 1.199719254218462483 ) ) ;
#96444 = CARTESIAN_POINT ( 'NONE',  ( -7.004758919754800139, 11.32396917302262018, 0.000000000000000000 ) ) ;
#96445 = CARTESIAN_POINT ( 'NONE',  ( 4.203910148689107729, 7.062256385849379647, -1.199719254218448494 ) ) ;
#96446 = CARTESIAN_POINT ( 'NONE',  ( 5.690118541956746157, 1.263103799472656164, 1.703077153987264669 ) ) ;
#96447 = DIRECTION ( 'NONE',  ( -1.000000000000000000, 1.250471828332832423E-35, 1.561251128379126077E-17 ) ) ;
#96448 = CARTESIAN_POINT ( 'NONE',  ( 1.364683531249988535, 2.113541667008087099, 0.7879004041258500513 ) ) ;
#96449 = VERTEX_POINT ( 'NONE', #103568 ) ;
#96450 = CARTESIAN_POINT ( 'NONE',  ( 0.7499999999999902300, 4.066666666666690411, -1.299038105676658228 ) ) ;
#96452 = CARTESIAN_POINT ( 'NONE',  ( 2.510230996824538430, 6.080353262937265413, 0.000000000000000000 ) ) ;
#96451 = CARTESIAN_POINT ( 'NONE',  ( 6.584431417889404337, 1.130572321132311098, -1.603143135845342515 ) ) ;
#96453 = CARTESIAN_POINT ( 'NONE',  ( 4.429064430395744267, 0.9478954142983322395, 1.779353956671766657 ) ) ;
#96454 = CARTESIAN_POINT ( 'NONE',  ( 4.012823373000539817, 0.09967532595039167720, 1.913279002700827514 ) ) ;
#96455 = PLANE ( 'NONE',  #131309 ) ;
#96456 = CARTESIAN_POINT ( 'NONE',  ( 1.136565065649897344, 0.4323997850379874830, 2.148315308122191514 ) ) ;
#96457 = CARTESIAN_POINT ( 'NONE',  ( 0.1333692844072559003, 2.872395615372814515, -2.542035612928101873 ) ) ;
#96458 = CARTESIAN_POINT ( 'NONE',  ( 1.499999999999989120, 1.056250000682816603, 0.000000000000000000 ) ) ;
#96459 = CARTESIAN_POINT ( 'NONE',  ( 5.256112987848621465, 0.8120324739511315393, -1.842333132669704554 ) ) ;
#96460 = CARTESIAN_POINT ( 'NONE',  ( -6.344325816190970357, 9.489131654609717970, 1.199719254218452047 ) ) ;
#96462 = CARTESIAN_POINT ( 'NONE',  ( 5.589508065689547500, -0.5136281568550029597, 2.053882654316901313 ) ) ;
#96461 = CARTESIAN_POINT ( 'NONE',  ( -3.877268743828284681, 5.546566172598190292, 1.443375672974064550 ) ) ;
#96463 = CARTESIAN_POINT ( 'NONE',  ( -1.364683531250010295, 8.442708333674730170, 0.7879004041258445001 ) ) ;
#96465 = CARTESIAN_POINT ( 'NONE',  ( -8.106849506328558164, 8.422688943663599659, 0.000000000000000000 ) ) ;
#96464 = CARTESIAN_POINT ( 'NONE',  ( 2.788710525494293879, 1.791885054564039903, -1.076980376859866029 ) ) ;
#96467 = VERTEX_POINT ( 'NONE', #21210 ) ;
#96466 = CARTESIAN_POINT ( 'NONE',  ( 2.449869591326372387, 1.724352457016034457, 0.04528501180301596624 ) ) ;
#96468 = CARTESIAN_POINT ( 'NONE',  ( 7.450369105909416589, 8.650851030771185890, -1.199719254218441611 ) ) ;
#96469 = CARTESIAN_POINT ( 'NONE',  ( -1.301544632936721735, 13.25916247302991380, 0.7160067306521127328 ) ) ;
#96470 = CARTESIAN_POINT ( 'NONE',  ( 4.858757509019037357, 5.629766575900002401, 2.420000000000000373 ) ) ;
#96471 = AXIS2_PLACEMENT_3D ( 'NONE', #174163, #191428, #204466 ) ;
#96472 = DIRECTION ( 'NONE',  ( 0.000000000000000000, -1.000000000000000000, 0.000000000000000000 ) ) ;
#96474 = CARTESIAN_POINT ( 'NONE',  ( 7.904040366642684390, 11.20483561351640844, 1.082531754730558626 ) ) ;
#96473 = CARTESIAN_POINT ( 'NONE',  ( 7.145310649601935182, 8.294949498412453437, -1.199719254218446718 ) ) ;
#96475 = ORIENTED_EDGE ( 'NONE', *, *, #176945, .T. ) ;
#96476 = CARTESIAN_POINT ( 'NONE',  ( -1.500000000000001110, 9.520833333333333925, 0.8660254037844418162 ) ) ;
#96477 = ORIENTED_EDGE ( 'NONE', *, *, #169747, .T. ) ;
#96479 = CARTESIAN_POINT ( 'NONE',  ( 1.910541399130718743, -0.4838386274770510864, -1.745561575705076862 ) ) ;
#96478 = CARTESIAN_POINT ( 'NONE',  ( 4.830447868218803897, 8.857549289555754157, -0.7998128361456481317 ) ) ;
#96480 = CARTESIAN_POINT ( 'NONE',  ( -6.561256274009600986, 9.742217188731485678, -1.199719254218440723 ) ) ;
#96481 = CARTESIAN_POINT ( 'NONE',  ( 3.541704441667858472, 5.155074486744371853, -1.599625672291262513 ) ) ;
#96482 = VERTEX_POINT ( 'NONE', #117748 ) ;
#96483 = CARTESIAN_POINT ( 'NONE',  ( 4.701645408888975197, 8.707279753670952971, 0.000000000000000000 ) ) ;
#96484 = CARTESIAN_POINT ( 'NONE',  ( 2.455456329753392897, -1.343237331403211776, -1.215579648594692808 ) ) ;
#96485 = CARTESIAN_POINT ( 'NONE',  ( 6.639320575229256782, 2.986994467643698137, 2.250762793112503157 ) ) ;
#96486 = CARTESIAN_POINT ( 'NONE',  ( 4.038955833855768063, 7.541343398062151593, 0.4257906834902285276 ) ) ;
#96487 = ORIENTED_EDGE ( 'NONE', *, *, #114707, .F. ) ;
#96488 = CARTESIAN_POINT ( 'NONE',  ( 2.927998328727512867, 0.9930260268339460294, 1.573771836281928627 ) ) ;
#96489 = AXIS2_PLACEMENT_3D ( 'NONE', #163547, #214363, #116977 ) ;
#96490 = CARTESIAN_POINT ( 'NONE',  ( 0.1400564425528905699, 0.7337865575636399740, 1.769695213874568962 ) ) ;
#96491 = CARTESIAN_POINT ( 'NONE',  ( 0.1822601575737579360, -1.769359155225664226, -0.4491840103194589817 ) ) ;
#96492 = CARTESIAN_POINT ( 'NONE',  ( 0.000000000000000000, -3.517800438942085606, 0.000000000000000000 ) ) ;
#96493 = LINE ( 'NONE', #63955, #15739 ) ;
#96494 = CARTESIAN_POINT ( 'NONE',  ( 4.604167169973131912, 8.362045362587558373, -0.1994984680026238300 ) ) ;
#96495 = CARTESIAN_POINT ( 'NONE',  ( -4.609409038966253647, 4.479991421656468908, -0.7216878364870207285 ) ) ;
#96496 = CARTESIAN_POINT ( 'NONE',  ( 7.619319141200057821, 10.87266085050000974, 1.082531754730557072 ) ) ;
#96497 = CARTESIAN_POINT ( 'NONE',  ( 4.750814831274846384, -0.4274863908861815665, -1.922328355476431216 ) ) ;
#96498 = CARTESIAN_POINT ( 'NONE',  ( -5.440899717785814715, 5.242137847038546461, 0.7998128361456341429 ) ) ;
#96499 = DIRECTION ( 'NONE',  ( -5.578564026256490882E-16, -1.000000000000000000, -9.066213480720158442E-32 ) ) ;
#96500 = CARTESIAN_POINT ( 'NONE',  ( 0.1993191639408486426, -0.5556045495253292277, 2.015383906575985318 ) ) ;
#96501 = CARTESIAN_POINT ( 'NONE',  ( -0.7500000000000179856, 10.07291666734946922, 1.299038105676658228 ) ) ;
#96502 = CARTESIAN_POINT ( 'NONE',  ( 5.262690832784179484, -1.395389315813623909, 1.328347855495640273 ) ) ;
#96503 = CARTESIAN_POINT ( 'NONE',  ( -5.856232286098998152, 8.919689202835742847, 1.199719254218452047 ) ) ;
#96504 = DIRECTION ( 'NONE',  ( -0.5005768354468334014, 0.8656921114426502362, 1.887379141862767696E-15 ) ) ;
#96505 = CARTESIAN_POINT ( 'NONE',  ( 1.963769682107346037, 0.3752889857368996163, -2.174583152744386627 ) ) ;
#96506 = CARTESIAN_POINT ( 'NONE',  ( -6.118005967093342434, 7.012694018530115869, 0.9664715254068743100 ) ) ;
#96507 = CARTESIAN_POINT ( 'NONE',  ( -0.2049973002360427898, -0.1418364932926942379, -1.881151990943498387 ) ) ;
#96508 = VERTEX_POINT ( 'NONE', #67821 ) ;
#96509 = EDGE_LOOP ( 'NONE', ( #129732, #65135, #181172, #124800 ) ) ;
#96510 = CARTESIAN_POINT ( 'NONE',  ( 0.4495734683114894215, 1.456899865409568617, 1.325532655419828787 ) ) ;
#96511 = CARTESIAN_POINT ( 'NONE',  ( 1.856878829904203165, 0.3300924852138227283, -1.913646475244117795 ) ) ;
#96512 = ORIENTED_EDGE ( 'NONE', *, *, #19860, .T. ) ;
#96513 = CARTESIAN_POINT ( 'NONE',  ( 0.8607036144342284922, -0.7282710370301350711, 1.880145570116364073 ) ) ;
#96515 = CARTESIAN_POINT ( 'NONE',  ( 4.961672996587167539, -0.4989766864872626217, 1.792691909438326681 ) ) ;
#96514 = CARTESIAN_POINT ( 'NONE',  ( -6.479871072688648148, 6.524547437750345402, 0.000000000000000000 ) ) ;
#96516 = CARTESIAN_POINT ( 'NONE',  ( 6.723917837734620484, 6.809268663637336516, 0.000000000000000000 ) ) ;
#96517 = DIRECTION ( 'NONE',  ( -5.578564026256491869E-16, -1.000000000000000000, -9.066213480720160632E-32 ) ) ;
#96518 = CARTESIAN_POINT ( 'NONE',  ( 1.499999999999819256, 7.438721522839173872, -4.195160983902622043 ) ) ;
#96519 = CARTESIAN_POINT ( 'NONE',  ( -6.064574784014443942, 5.969758757638621738, -0.7998128361456291469 ) ) ;
#96520 = CARTESIAN_POINT ( 'NONE',  ( -5.887983850084758330, 10.09134126839936840, 0.7998128361456291469 ) ) ;
#96521 = CARTESIAN_POINT ( 'NONE',  ( 1.593588134247824639, -0.7342643958434189599, 2.065040727587868830 ) ) ;
#96522 = CARTESIAN_POINT ( 'NONE',  ( 3.389175213736297820, 4.977123720824209840, 1.443375672974062551 ) ) ;
#96523 = CIRCLE ( 'NONE', #207182, 6.329999999999995630 ) ;
#96524 = DIRECTION ( 'NONE',  ( -1.000000000000000000, -1.276756478318932585E-15, -3.330669073875474552E-16 ) ) ;
#96525 = CARTESIAN_POINT ( 'NONE',  ( 1.418276456094772708, 1.227529518603141190, -1.351586893430449576 ) ) ;
#96526 = CARTESIAN_POINT ( 'NONE',  ( -3.623053363349869382, 5.249981562040033189, 1.599625672291267398 ) ) ;
#96527 = CARTESIAN_POINT ( 'NONE',  ( -0.3583907109357110099, 2.793873605144960859, -2.035334756721693061 ) ) ;
#96528 = CARTESIAN_POINT ( 'NONE',  ( -1.777638883463106279, 0.9165151389911794233, 1.199999999999999734 ) ) ;
#96529 = CARTESIAN_POINT ( 'NONE',  ( 8.367353357928214663, 12.91366268422496688, 1.040834085586084257E-14 ) ) ;
#96530 = CARTESIAN_POINT ( 'NONE',  ( 1.559075672363739118, -1.651969382833524902, -0.9909376787137593734 ) ) ;
#96531 = CARTESIAN_POINT ( 'NONE',  ( 4.469553177461598636, -0.3394721387663233170, 1.932013773527321066 ) ) ;
#96532 = CIRCLE ( 'NONE', #65393, 0.05000000000000002359 ) ;
#96533 = ADVANCED_FACE ( 'NONE', ( #198897 ), #165601, .F. ) ;
#96534 = CARTESIAN_POINT ( 'NONE',  ( -7.153898609505128015, 11.49796547773133604, 0.7998128361456481317 ) ) ;
#96535 = CARTESIAN_POINT ( 'NONE',  ( 6.148786358997489820, 7.132337826040578754, -1.199719254218446718 ) ) ;
#96536 = CARTESIAN_POINT ( 'NONE',  ( 4.564136437409766600, -1.431273618155091576, 1.659743667367798103 ) ) ;
#96537 = EDGE_CURVE ( 'NONE', #136572, #35662, #124852, .T. ) ;
#96538 = CARTESIAN_POINT ( 'NONE',  ( 4.381733404717279790, -1.982624999272282862, 0.5960583376443123749 ) ) ;
#96540 = CARTESIAN_POINT ( 'NONE',  ( -0.6823417656250003738, 1.530208333674752730, -1.181850606188749264 ) ) ;
#96539 = CARTESIAN_POINT ( 'NONE',  ( 6.966220764712121927, 6.002124920821316323, 2.500000000000000444 ) ) ;
#96541 = VERTEX_POINT ( 'NONE', #63384 ) ;
#96542 = CARTESIAN_POINT ( 'NONE',  ( 4.078954460043759056, -0.8795263853869551562, 2.123946672719174700 ) ) ;
#96543 = CARTESIAN_POINT ( 'NONE',  ( 5.965224400332808763, 9.903252867122883885, -0.7216878364870267237 ) ) ;
#96545 = CARTESIAN_POINT ( 'NONE',  ( -2.440293211016301606E-15, 1.312499999999991118, 1.224999999999973888 ) ) ;
#96544 = CARTESIAN_POINT ( 'NONE',  ( 5.885648082108190238, 7.959951743916638733, 1.443375672974065660 ) ) ;
#96546 = CARTESIAN_POINT ( 'NONE',  ( -7.462104991928526054, -5.166862915010159263, -8.081892667527538876 ) ) ;
#96547 = CARTESIAN_POINT ( 'NONE',  ( -9.569358774130439116, 4.446955548196708463, -7.167287524826070566 ) ) ;
#96548 = CARTESIAN_POINT ( 'NONE',  ( 4.066302494797935374, -1.812431348068560988, -0.6977731361806001065 ) ) ;
#96549 = VERTEX_POINT ( 'NONE', #77491 ) ;
#96550 = CARTESIAN_POINT ( 'NONE',  ( -0.07406709734315156113, -9.431556885384965838, 9.500634193481339196 ) ) ;
#96551 = ADVANCED_FACE ( 'NONE', ( #65482 ), #164332, .T. ) ;
#96552 = CARTESIAN_POINT ( 'NONE',  ( 5.080287894202283105, 0.9478536798121822704, 1.660923459347658282 ) ) ;
#96553 = CARTESIAN_POINT ( 'NONE',  ( 5.192313411850084215, -1.712133481052197093, -0.2078965086465163203 ) ) ;
#96554 = CARTESIAN_POINT ( 'NONE',  ( 4.329314735043091389, -1.561880650076686861, -1.275557594027726394 ) ) ;
#96555 = CARTESIAN_POINT ( 'NONE',  ( 5.028124288008245735, -1.972403190421234687, 1.180361310613570414 ) ) ;
#96556 = CARTESIAN_POINT ( 'NONE',  ( -2.487170525094696938, 8.243531156566643148, 2.499999999999999112 ) ) ;
#96557 = CARTESIAN_POINT ( 'NONE',  ( 0.6806489137391663613, -1.222764829241920648, 1.836970590647703627 ) ) ;
#96559 = CARTESIAN_POINT ( 'NONE',  ( -5.167065940583949413, 5.200867483535597913, 0.000000000000000000 ) ) ;
#96558 = CARTESIAN_POINT ( 'NONE',  ( -8.482597663644387609, 13.04811437422715414, -0.7998128361456281477 ) ) ;
#96560 = CARTESIAN_POINT ( 'NONE',  ( 6.081276588353502710, 1.634447734625959825, -0.6791225938206167934 ) ) ;
#96561 = CARTESIAN_POINT ( 'NONE',  ( 5.045546153961558922, -1.458558117013383892, 1.392544180963309230 ) ) ;
#96563 = CARTESIAN_POINT ( 'NONE',  ( 2.344040366607359704, 2.291775683190785173, 0.05432913299479279201 ) ) ;
#96562 = CARTESIAN_POINT ( 'NONE',  ( 3.576318658954677598, 7.394398545414291313, 0.7998128361456281477 ) ) ;
#96564 = CARTESIAN_POINT ( 'NONE',  ( 1.323703871734905890, 1.676395044522845712, 0.4671252976603932350 ) ) ;
#96565 = CARTESIAN_POINT ( 'NONE',  ( 11.84668730067608244, 10.90000000000000036, -1.400000000000001688 ) ) ;
#96566 = CARTESIAN_POINT ( 'NONE',  ( 1.159081676615776990, -0.4145447896758222561, -1.683414020171439818 ) ) ;
#96567 = CARTESIAN_POINT ( 'NONE',  ( -1.360316468750032870, 0.9427083336747503761, 0.7853790794158641564 ) ) ;
#96568 = CARTESIAN_POINT ( 'NONE',  ( -11.33772467203841572, 12.59267152018143854, 3.599999999999999201 ) ) ;
#96569 = CARTESIAN_POINT ( 'NONE',  ( 1.223348113247175961, -1.962646724111057672, -0.9287667758015824004 ) ) ;
#96570 = CARTESIAN_POINT ( 'NONE',  ( 2.290250256651988892, -0.7762311197250795214, -1.861343989391924358 ) ) ;
#96571 = VECTOR ( 'NONE', #112840, 1000.000000000000000 ) ;
#96572 = CARTESIAN_POINT ( 'NONE',  ( -0.7500000000000215383, 1.222916667349485564, 1.299038105676659116 ) ) ;
#96573 = CARTESIAN_POINT ( 'NONE',  ( 6.059198490463121090, -1.653572398999035853, -0.9882694798356050914 ) ) ;
#96574 = CARTESIAN_POINT ( 'NONE',  ( -1.402160292154681736E-14, 12.67187500034139802, 1.575800808251682339 ) ) ;
#96575 = CARTESIAN_POINT ( 'NONE',  ( 2.338390812749164827, -1.283062462031187456, -1.813217020134863411 ) ) ;
#96576 = VERTEX_POINT ( 'NONE', #99091 ) ;
#96577 = CARTESIAN_POINT ( 'NONE',  ( 6.608557002163613525, -8.105676417795780964, 6.825099317097805596 ) ) ;
#96578 = CARTESIAN_POINT ( 'NONE',  ( -1.402160292154681736E-14, -0.2874999999999741096, 1.732050807568877637 ) ) ;
#96579 = CARTESIAN_POINT ( 'NONE',  ( 8.697719238366680372, 10.10609285197134533, 1.199719254218462483 ) ) ;
#96580 = CARTESIAN_POINT ( 'NONE',  ( 6.251718229232841928, 8.387033582228703210, -1.443375672974078761 ) ) ;
#96581 = CARTESIAN_POINT ( 'NONE',  ( 5.179165720741062628, 1.174484231026547976, 1.284593650646998375 ) ) ;
#96582 = CARTESIAN_POINT ( 'NONE',  ( 4.070719198475009293, 1.388998261151509039, -1.385754695631277844 ) ) ;
#96584 = CARTESIAN_POINT ( 'NONE',  ( -7.863365906246074566, 8.276274433482971205, -0.7216878364870278340 ) ) ;
#96583 = CARTESIAN_POINT ( 'NONE',  ( 4.871457266011829823, 4.577788319968905562, -0.7998128361456221525 ) ) ;
#96585 = CARTESIAN_POINT ( 'NONE',  ( 6.966220764712121927, 6.002124920821316323, 2.420000000000000373 ) ) ;
#96586 = CARTESIAN_POINT ( 'NONE',  ( 4.429186382639688446, 0.1052742795825665628, 2.260063922926962121 ) ) ;
#96587 = CARTESIAN_POINT ( 'NONE',  ( 1.574752048370867907, 1.386759265612296455, -1.527078818449955966 ) ) ;
#96588 = CARTESIAN_POINT ( 'NONE',  ( -6.398558430645608475, 9.552403038140164782, -1.199719254218440723 ) ) ;
#96589 = CARTESIAN_POINT ( 'NONE',  ( 2.290224401178039049, -0.9674489778378884131, 2.045383877150886320 ) ) ;
#96590 = ORIENTED_EDGE ( 'NONE', *, *, #204859, .F. ) ;
#96591 = CARTESIAN_POINT ( 'NONE',  ( -1.500000000000013101, 0.7020833340161545255, 0.8660254037844403729 ) ) ;
#96592 = CARTESIAN_POINT ( 'NONE',  ( 3.989402248074361612, 1.353031944225962624, 1.291829963354161892 ) ) ;
#96593 = CARTESIAN_POINT ( 'NONE',  ( 3.041388834704723099, -1.310848641452688979, 1.135385315042459542 ) ) ;
#96594 = CARTESIAN_POINT ( 'NONE',  ( 6.427279137517246888, -1.429865906218323435, -1.660902671979214595 ) ) ;
#96595 = CARTESIAN_POINT ( 'NONE',  ( 0.4115098346569624477, 1.921242953230850148, 1.085561749797583797 ) ) ;
#96596 = CARTESIAN_POINT ( 'NONE',  ( 3.713887418366210280, -2.130098009959373151, 0.3673708613747132534 ) ) ;
#96597 = CARTESIAN_POINT ( 'NONE',  ( 5.033120997586177481, -1.374529083251808892, -1.372050024763036280 ) ) ;
#96598 = CARTESIAN_POINT ( 'NONE',  ( -3.050221372950322252, 5.542046787541873520, 1.082531754730560403 ) ) ;
#96599 = CARTESIAN_POINT ( 'NONE',  ( 6.292256349370360269, -1.861554482619768525, -0.1834065582871149958 ) ) ;
#96600 = CARTESIAN_POINT ( 'NONE',  ( 4.753338833179075351, 6.783512570024928579, 1.242321799368527380 ) ) ;
#96601 = CYLINDRICAL_SURFACE ( 'NONE', #200626, 0.08000000000000020983 ) ;
#96602 = EDGE_CURVE ( 'NONE', #84740, #84121, #102269, .T. ) ;
#96603 = CARTESIAN_POINT ( 'NONE',  ( -5.608633734226008194, 5.643391804966442216, 0.4859901473732997079 ) ) ;
#96604 = CARTESIAN_POINT ( 'NONE',  ( 5.660779783930850684, 1.203351582566011047, 1.617819807990819481 ) ) ;
#96605 = CARTESIAN_POINT ( 'NONE',  ( -4.243338890952916387, 4.052909582307567149, -0.7216878364870207285 ) ) ;
#96606 = CARTESIAN_POINT ( 'NONE',  ( 7.259501185113382604, 10.55683625168592243, -1.199719254218441611 ) ) ;
#96607 = CARTESIAN_POINT ( 'NONE',  ( 11.97929049433705373, 12.22000000000000064, 0.7046979865771783036 ) ) ;
#96609 = FACE_OUTER_BOUND ( 'NONE', #76209, .T. ) ;
#96608 = CARTESIAN_POINT ( 'NONE',  ( 3.228933428962964758, 0.04559371896543929631, 1.825288036790246204 ) ) ;
#96610 = CARTESIAN_POINT ( 'NONE',  ( 11.88168509644349058, 9.719999999999998863, -1.685788023084331400 ) ) ;
#96611 = ORIENTED_EDGE ( 'NONE', *, *, #99741, .T. ) ;
#96612 = CARTESIAN_POINT ( 'NONE',  ( -3.472296738431328134, 7.065113604896248845, 0.000000000000000000 ) ) ;
#96613 = CARTESIAN_POINT ( 'NONE',  ( 4.597436146581902250, 8.478756905425443691, -0.3710115925776128476 ) ) ;
#96614 = CARTESIAN_POINT ( 'NONE',  ( -8.507905087775398556, 9.884643009614800135, 1.199719254218462483 ) ) ;
#96615 = CARTESIAN_POINT ( 'NONE',  ( 6.287761640583830136, 1.932026593981367002, -0.5884565063561957299 ) ) ;
#96616 = CARTESIAN_POINT ( 'NONE',  ( 0.6805317496583452863, 1.048634805427307359, 1.842989218901350812 ) ) ;
#96617 = EDGE_LOOP ( 'NONE', ( #164031, #95666, #39746, #144857 ) ) ;
#96618 = CARTESIAN_POINT ( 'NONE',  ( -6.459533842268148973, 6.500820668926428958, 0.000000000000000000 ) ) ;
#96619 = CARTESIAN_POINT ( 'NONE',  ( 1.920531177235841103, -1.320465346956477992, 1.311572250416197960 ) ) ;
#96620 = CARTESIAN_POINT ( 'NONE',  ( 4.878236342818665250, 4.585697242910212523, 1.040834085586084257E-14 ) ) ;
#96621 = CARTESIAN_POINT ( 'NONE',  ( 6.772340629568521564, -1.270048932776141726, 1.623522132280514896 ) ) ;
#96622 = CARTESIAN_POINT ( 'NONE',  ( 6.311172677262812059, 1.158691452862798954, -1.650079838712660063 ) ) ;
#96623 = VERTEX_POINT ( 'NONE', #184573 ) ;
#96624 = FACE_OUTER_BOUND ( 'NONE', #26104, .T. ) ;
#96625 = CARTESIAN_POINT ( 'NONE',  ( 6.966220764712146796, 6.002124920821316323, -2.420000000000000373 ) ) ;
#96628 = ORIENTED_EDGE ( 'NONE', *, *, #39143, .F. ) ;
#96627 = CARTESIAN_POINT ( 'NONE',  ( 0.07680821025391955381, 1.395885924038504644, -2.068540888291516833 ) ) ;
#96626 = CARTESIAN_POINT ( 'NONE',  ( -5.438755897737433287, 6.374245297895642537, -1.199719254218453823 ) ) ;
#96629 = CARTESIAN_POINT ( 'NONE',  ( 5.917965873332177829, 7.245500866451762612, 1.242176317587460943 ) ) ;
#96630 = CARTESIAN_POINT ( 'NONE',  ( 6.766953912288387940, -2.015720078709513086, 0.04667315333419658208 ) ) ;
#96631 = CARTESIAN_POINT ( 'NONE',  ( 4.189278935350455590, -0.7026162016144417155, 1.701997885059022497 ) ) ;
#96632 = CARTESIAN_POINT ( 'NONE',  ( -10.99934730582667797, -5.294005300192715424, 0.1376907581457726126 ) ) ;
#96633 = CARTESIAN_POINT ( 'NONE',  ( 3.739178398684524396, 0.3374720328367666888, 2.282779155512550062 ) ) ;
#96634 = CARTESIAN_POINT ( 'NONE',  ( 6.717138760927786834, 6.801359740696030443, -0.7998128361456481317 ) ) ;
#96635 = CARTESIAN_POINT ( 'NONE',  ( 5.448557382023540896, 0.6217387762853660016, 2.070273951448368788 ) ) ;
#96636 = CARTESIAN_POINT ( 'NONE',  ( 7.039708073993665494, 9.236078724457858158, 1.599625672291281386 ) ) ;
#96637 = CARTESIAN_POINT ( 'NONE',  ( 0.7142757748631656245, 1.794906310038762109, 0.7420174003010558961 ) ) ;
#96638 = CARTESIAN_POINT ( 'NONE',  ( -4.973143418114339021, 4.696422164088486895, 0.7998128361456341429 ) ) ;
#96639 = ORIENTED_EDGE ( 'NONE', *, *, #63612, .T. ) ;
#96640 = CIRCLE ( 'NONE', #114007, 0.6500000000000000222 ) ;
#96641 = CARTESIAN_POINT ( 'NONE',  ( 5.149944687579217195, -0.2746161857135383522, -2.281865060072391760 ) ) ;
#96642 = DIRECTION ( 'NONE',  ( 0.000000000000000000, 8.546850786086437571E-32, 1.000000000000000000 ) ) ;
#96643 = CARTESIAN_POINT ( 'NONE',  ( -5.143339171537843590, 7.093924681584509173, 1.599625672291263179 ) ) ;
#96644 = CARTESIAN_POINT ( 'NONE',  ( 4.698043743269282757, -1.870269067358639958, -0.04562963166049315705 ) ) ;
#96645 =( BOUNDED_SURFACE ( )  B_SPLINE_SURFACE ( 3, 2, ( 
 ( #100331, #198872, #32142 ),
 ( #98222, #117720, #116642 ),
 ( #151231, #182637, #84079 ),
 ( #34259, #166398, #17989 ) ),
 .UNSPECIFIED., .F., .F., .T. ) 
 B_SPLINE_SURFACE_WITH_KNOTS ( ( 4, 4 ),
 ( 3, 3 ),
 ( 0.000000000000000000, 9.170893477967426329E-05 ),
 ( 0.000000000000000000, 1.000000000000000000 ),
 .UNSPECIFIED. ) 
 GEOMETRIC_REPRESENTATION_ITEM ( )  RATIONAL_B_SPLINE_SURFACE ( (
 ( 1.000000000000000000, 0.6787756258918243857, 1.000000000000000000),
 ( 1.000000000000000000, 0.6894756946173453693, 1.000000000000000000),
 ( 1.000000000000000000, 0.6998898451713360114, 1.000000000000000000),
 ( 1.000000000000000000, 0.7100530722072171397, 1.000000000000000000) ) ) 
 REPRESENTATION_ITEM ( '' )  SURFACE ( )  );
#96648 = CARTESIAN_POINT ( 'NONE',  ( -5.448397627845328550, 7.449826213943242514, 1.599625672291263179 ) ) ;
#96647 = CARTESIAN_POINT ( 'NONE',  ( 1.499999999999987121, 0.7854166673494828999, 0.8660254037844524744 ) ) ;
#96646 = CARTESIAN_POINT ( 'NONE',  ( 1.406358598101828283, -1.903450966454448334, -0.1843715739238485363 ) ) ;
#96649 = CARTESIAN_POINT ( 'NONE',  ( 3.299657469156279888, 1.739734091921738557, 1.357710657151039779 ) ) ;
#96650 = ADVANCED_FACE ( 'NONE', ( #167284 ), #19939, .T. ) ;
#96651 = CARTESIAN_POINT ( 'NONE',  ( -1.499999999999997558, 8.627523663848661428, -2.579999999999989857 ) ) ;
#96652 = CARTESIAN_POINT ( 'NONE',  ( 4.161989969270895706, 5.878740935614592544, 1.443375672974062551 ) ) ;
#96653 = CARTESIAN_POINT ( 'NONE',  ( 6.414416072596830887, 8.576847732820027659, -1.443375672974078761 ) ) ;
#96654 = CARTESIAN_POINT ( 'NONE',  ( -2.286521462199063492, 5.819358805874190743, 1.040834085586084257E-14 ) ) ;
#96655 = CARTESIAN_POINT ( 'NONE',  ( -6.590672069574513792, 6.861741300691274859, 0.000000000000000000 ) ) ;
#96656 = CARTESIAN_POINT ( 'NONE',  ( 1.352734582195244561, -1.556726207391207817, 1.209420702486432297 ) ) ;
#96657 = CARTESIAN_POINT ( 'NONE',  ( 0.7632353006940760798, -1.668858575275869116, 1.593938313602519363 ) ) ;
#96658 = CARTESIAN_POINT ( 'NONE',  ( 2.541395235131336694, 1.794889867694851260, -0.7924082849640816661 ) ) ;
#96659 = CARTESIAN_POINT ( 'NONE',  ( 5.489153638472886954, 0.1464082308396240373, 2.057405090433866324 ) ) ;
#96660 = CARTESIAN_POINT ( 'NONE',  ( 3.985733972737593778, 6.633478153960411738, -1.082531754730548412 ) ) ;
#96661 = CARTESIAN_POINT ( 'NONE',  ( 5.448397627845284141, 7.449826213943242514, 1.599625672291268286 ) ) ;
#96662 = ORIENTED_EDGE ( 'NONE', *, *, #118355, .F. ) ;
#96663 = CARTESIAN_POINT ( 'NONE',  ( -1.364683531250010295, 5.551041667008087543, -0.7879004041258300672 ) ) ;
#96664 =( BOUNDED_SURFACE ( )  B_SPLINE_SURFACE ( 1, 2, ( 
 ( #109658, #208127, #92298, #28326, #175660, #111783, #209186, #59756, #210261, #77065, #94422, #61899, #158342, #143195, #44598, #123792, #91218, #160461, #194016, #95497, #139975, #189750, #41402, #25115, #42469, #108579, #157279, #8868, #141058, #197213, #96559, #97616, #130176, #1126, #53, #33647, #65069, #146373, #148484, #50974, #164721, #162606, #16310, #161544, #112847, #46735, #165793, #196168, #49909, #66116, #117096, #163673, #212388, #132259, #47809, #133325, #98666, #34708, #211327, #13131, #198266, #180967, #83460, #183096, #114967, #99721, #116030, #199328, #182016, #17376, #62952, #14182, #149540, #79208, #67188, #145326, #129121, #147422, #195098, #80275, #31540, #178863, #213447, #48853, #30474, #64030, #15256, #113922, #179918, #81343, #131225, #32589, #82395, #54171, #71458, #2182, #37922, #153808, #70385, #3253, #101852, #69321, #200394, #188427, #204657, #184154, #134391, #137571, #5379, #201453, #100777, #18455, #120310, #186285, #105075, #102920, #53096, #20581, #68258, #84532, #103996, #170040, #21626, #38990, #122468, #88819, #6459, #35777, #203588, #4314, #187360, #150621, #135431, #55240, #56306, #87734, #171114, #121387, #85595, #52042, #151683, #22706, #185213, #138634, #154876, #168981, #118168, #72536, #166859, #167921, #136501, #19518, #202522, #119230, #36837, #86665, #152732, #127799, #155944, #42206, #75751, #40062, #106172, #43274, #108323, #10733, #59493, #76803, #89893, #174343, #141861, #23787, #94160, #142924, #74689, #126718, #7530, #208924, #176455, #58437, #123533, #124590, #25921, #172198, #73613, #60559, #192678, #11802, #206804, #158086, #139712, #190550, #92029, #9674, #207869, #44332, #110454, #24853, #28067, #41142, #125650, #191612, #205736, #109394, #175399, #107252, #26984, #160199, #173273, #90955, #93091, #159132, #57370, #157020, #77877, #140790, #143999, #209991, #61633, #189498, #8606, #132009, #95223, #211059, #12859, #31279, #178594, #148229, #14987, #198019, #80006, #129920, #78934, #99471, #45401, #165530, #161273, #196960, #146111, #97354, #47542 ),
 ( #164467, #145056, #179659, #115770, #46460, #63760, #62684, #163411, #81081, #111517, #49647, #195906, #82137, #96291, #17122, #212122, #214231, #113655, #147168, #16053, #128843, #130968, #32334, #213195, #162343, #194824, #13926, #112582, #66928, #83199, #30203, #64822, #65859, #98402, #48598, #193754, #177523, #114716, #180711, #181759, #33393, #149281, #862, #29135, #116840, #136251, #70139, #4069, #71206, #154628, #121143, #38740, #1936, #37670, #36587, #5131, #182841, #167666, #103746, #88570, #202271, #137322, #152487, #117917, #186034, #101598, #86420, #187106, #100530, #169797, #18194, #199068, #166605, #19267, #203338, #102674, #53922, #120059, #21386, #50714, #87495, #153560, #135192, #6208, #34458, #54991, #104822, #170868, #85349, #168732, #84279, #151430, #118982, #52847, #3003, #22458, #133070, #183910, #150366, #134138, #20334, #201208, #67996, #184961, #69072, #200145, #51799, #35521, #139455, #123288, #90710, #8358, #105916, #205487, #43032, #106995, #124344, #206558, #110206, #89640, #173020, #10486, #188176, #155692, #171941, #190302, #57121, #26743, #108071, #76560, #24601, #74442, #23532, #192432, #138386, #44087, #39810, #75503, #156772, #41959, #140544, #58186, #175157, #174099, #176216, #59242, #25672, #208681, #91779, #92846, #60310, #157836, #9433, #141614, #7275, #73352, #191365, #207624, #125400, #109144, #158890, #189251, #142670, #40890, #126469, #27818, #93915, #159956, #72277, #204404, #56057, #122214, #65609, #64584, #98172, #129676, #210823, #212947, #115521, #14748, #12618, #80840, #11560, #177277, #111274, #15807, #46224, #114468, #130725, #181516, #13689, #162100, #28893, #131759, #77630, #197764, #193519, #146930, #112341, #195661, #79759, #96047, #180469, #47295, #49402, #196716, #145875, #147979, #211883, #32084, #213989, #29961, #113410, #48357, #127548, #94977, #164220, #179416, #31037, #97111, #163163, #45160, #81893, #62448, #178353, #33145, #99225, #161023, #143752, #78691, #63524, #194578, #209747, #61389, #144816, #128611, #150105, #152228, #54722, #168470, #166338 ) ),
 .UNSPECIFIED., .F., .F., .F. ) 
 B_SPLINE_SURFACE_WITH_KNOTS ( ( 2, 2 ),
 ( 3, 2, 2, 2, 2, 2, 2, 2, 2, 2, 2, 2, 2, 2, 2, 2, 2, 2, 2, 2, 2, 2, 2, 2, 2, 2, 2, 2, 2, 2, 2, 2, 2, 2, 2, 2, 2, 2, 2, 2, 2, 2, 2, 2, 2, 2, 2, 2, 2, 2, 2, 2, 2, 2, 2, 2, 2, 2, 2, 2, 2, 2, 2, 2, 2, 2, 2, 2, 2, 2, 2, 2, 2, 2, 2, 2, 2, 2, 2, 2, 2, 2, 2, 2, 2, 2, 2, 2, 2, 2, 2, 2, 2, 2, 2, 2, 2, 2, 2, 2, 2, 2, 2, 2, 2, 2, 2, 2, 2, 2, 2, 2, 2, 2, 2, 2, 2, 2, 2, 2, 3 ),
 ( 0.000000000000000000, 1.000000000000000000 ),
 ( 0.000000000000000000, 0.008333333333333333218, 0.01666666666666666644, 0.02500000000000000139, 0.03333333333333333287, 0.04166666666666666435, 0.05000000000000000278, 0.05833333333333333426, 0.06666666666666666574, 0.07499999999999999722, 0.08333333333333332871, 0.09166666666666666019, 0.1000000000000000056, 0.1083333333333333370, 0.1166666666666666685, 0.1250000000000000000, 0.1333333333333333315, 0.1416666666666666630, 0.1499999999999999944, 0.1583333333333333259, 0.1666666666666666574, 0.1749999999999999889, 0.1833333333333333204, 0.1916666666666666796, 0.2000000000000000111, 0.2083333333333333426, 0.2166666666666666741, 0.2250000000000000056, 0.2333333333333333370, 0.2416666666666666685, 0.2500000000000000000, 0.2583333333333333592, 0.2666666666666666630, 0.2750000000000000222, 0.2833333333333333259, 0.2916666666666666852, 0.2999999999999999889, 0.3083333333333333481, 0.3166666666666666519, 0.3250000000000000111, 0.3333333333333333148, 0.3416666666666666741, 0.3499999999999999778, 0.3583333333333333370, 0.3666666666666666408, 0.3750000000000000000, 0.3833333333333333592, 0.3916666666666666630, 0.4000000000000000222, 0.4083333333333333259, 0.4166666666666666852, 0.4249999999999999889, 0.4333333333333333481, 0.4416666666666666519, 0.4500000000000000111, 0.4583333333333333148, 0.4666666666666666741, 0.4749999999999999778, 0.4833333333333333370, 0.4916666666666666408, 0.5000000000000000000, 0.5083333333333333037, 0.5166666666666667185, 0.5250000000000000222, 0.5333333333333333259, 0.5416666666666666297, 0.5500000000000000444, 0.5583333333333333481, 0.5666666666666666519, 0.5749999999999999556, 0.5833333333333333703, 0.5916666666666666741, 0.5999999999999999778, 0.6083333333333332815, 0.6166666666666666963, 0.6250000000000000000, 0.6333333333333333037, 0.6416666666666667185, 0.6500000000000000222, 0.6583333333333333259, 0.6666666666666666297, 0.6750000000000000444, 0.6833333333333333481, 0.6916666666666666519, 0.6999999999999999556, 0.7083333333333333703, 0.7166666666666666741, 0.7249999999999999778, 0.7333333333333332815, 0.7416666666666666963, 0.7500000000000000000, 0.7583333333333333037, 0.7666666666666667185, 0.7750000000000000222, 0.7833333333333333259, 0.7916666666666666297, 0.8000000000000000444, 0.8083333333333333481, 0.8166666666666666519, 0.8249999999999999556, 0.8333333333333333703, 0.8416666666666666741, 0.8499999999999999778, 0.8583333333333332815, 0.8666666666666666963, 0.8750000000000000000, 0.8833333333333333037, 0.8916666666666667185, 0.9000000000000000222, 0.9083333333333333259, 0.9166666666666666297, 0.9250000000000000444, 0.9333333333333333481, 0.9416666666666666519, 0.9499999999999999556, 0.9583333333333333703, 0.9666666666666666741, 0.9749999999999999778, 0.9833333333333332815, 0.9916666666666666963, 1.000000000000000000 ),
 .UNSPECIFIED. ) 
 GEOMETRIC_REPRESENTATION_ITEM ( )  RATIONAL_B_SPLINE_SURFACE ( (
 ( 1.000000000000000000, 0.8660254037844387076, 1.000000000000000000, 0.8660254037844387076, 1.000000000000000000, 0.8660254037844387076, 1.000000000000000000, 0.8660254037844387076, 1.000000000000000000, 0.8660254037844387076, 1.000000000000000000, 0.8660254037844387076, 1.000000000000000000, 0.8660254037844387076, 1.000000000000000000, 0.8660254037844387076, 1.000000000000000000, 0.8660254037844387076, 1.000000000000000000, 0.8660254037844387076, 1.000000000000000000, 0.8660254037844387076, 1.000000000000000000, 0.8660254037844387076, 1.000000000000000000, 0.8660254037844387076, 1.000000000000000000, 0.8660254037844387076, 1.000000000000000000, 0.8660254037844387076, 1.000000000000000000, 0.8660254037844387076, 1.000000000000000000, 0.8660254037844387076, 1.000000000000000000, 0.8660254037844387076, 1.000000000000000000, 0.8660254037844387076, 1.000000000000000000, 0.8660254037844387076, 1.000000000000000000, 0.8660254037844387076, 1.000000000000000000, 0.8660254037844387076, 1.000000000000000000, 0.8660254037844387076, 1.000000000000000000, 0.8660254037844387076, 1.000000000000000000, 0.8660254037844387076, 1.000000000000000000, 0.8660254037844387076, 1.000000000000000000, 0.8660254037844387076, 1.000000000000000000, 0.8660254037844387076, 1.000000000000000000, 0.8660254037844387076, 1.000000000000000000, 0.8660254037844387076, 1.000000000000000000, 0.8660254037844387076, 1.000000000000000000, 0.8660254037844387076, 1.000000000000000000, 0.8660254037844387076, 1.000000000000000000, 0.8660254037844387076, 1.000000000000000000, 0.8660254037844387076, 1.000000000000000000, 0.8660254037844387076, 1.000000000000000000, 0.8660254037844387076, 1.000000000000000000, 0.8660254037844387076, 1.000000000000000000, 0.8660254037844387076, 1.000000000000000000, 0.8660254037844387076, 1.000000000000000000, 0.8660254037844387076, 1.000000000000000000, 0.8660254037844387076, 1.000000000000000000, 0.8660254037844387076, 1.000000000000000000, 0.8660254037844387076, 1.000000000000000000, 0.8660254037844387076, 1.000000000000000000, 0.8660254037844387076, 1.000000000000000000, 0.8660254037844387076, 1.000000000000000000, 0.8660254037844387076, 1.000000000000000000, 0.8660254037844387076, 1.000000000000000000, 0.8660254037844387076, 1.000000000000000000, 0.8660254037844387076, 1.000000000000000000, 0.8660254037844387076, 1.000000000000000000, 0.8660254037844387076, 1.000000000000000000, 0.8660254037844387076, 1.000000000000000000, 0.8660254037844387076, 1.000000000000000000, 0.8660254037844387076, 1.000000000000000000, 0.8660254037844387076, 1.000000000000000000, 0.8660254037844387076, 1.000000000000000000, 0.8660254037844387076, 1.000000000000000000, 0.8660254037844387076, 1.000000000000000000, 0.8660254037844387076, 1.000000000000000000, 0.8660254037844387076, 1.000000000000000000, 0.8660254037844387076, 1.000000000000000000, 0.8660254037844387076, 1.000000000000000000, 0.8660254037844387076, 1.000000000000000000, 0.8660254037844387076, 1.000000000000000000, 0.8660254037844387076, 1.000000000000000000, 0.8660254037844387076, 1.000000000000000000, 0.8660254037844387076, 1.000000000000000000, 0.8660254037844387076, 1.000000000000000000, 0.8660254037844387076, 1.000000000000000000, 0.8660254037844387076, 1.000000000000000000, 0.8660254037844387076, 1.000000000000000000, 0.8660254037844387076, 1.000000000000000000, 0.8660254037844387076, 1.000000000000000000, 0.8660254037844387076, 1.000000000000000000, 0.8660254037844387076, 1.000000000000000000, 0.8660254037844387076, 1.000000000000000000, 0.8660254037844387076, 1.000000000000000000, 0.8660254037844387076, 1.000000000000000000, 0.8660254037844387076, 1.000000000000000000, 0.8660254037844387076, 1.000000000000000000, 0.8660254037844387076, 1.000000000000000000, 0.8660254037844387076, 1.000000000000000000, 0.8660254037844387076, 1.000000000000000000, 0.8660254037844387076, 1.000000000000000000, 0.8660254037844387076, 1.000000000000000000, 0.8660254037844387076, 1.000000000000000000, 0.8660254037844387076, 1.000000000000000000, 0.8660254037844387076, 1.000000000000000000, 0.8660254037844387076, 1.000000000000000000, 0.8660254037844387076, 1.000000000000000000, 0.8660254037844387076, 1.000000000000000000, 0.8660254037844387076, 1.000000000000000000, 0.8660254037844387076, 1.000000000000000000, 0.8660254037844387076, 1.000000000000000000, 0.8660254037844387076, 1.000000000000000000, 0.8660254037844387076, 1.000000000000000000, 0.8660254037844387076, 1.000000000000000000, 0.8660254037844387076, 1.000000000000000000, 0.8660254037844387076, 1.000000000000000000, 0.8660254037844387076, 1.000000000000000000, 0.8660254037844387076, 1.000000000000000000, 0.8660254037844387076, 1.000000000000000000, 0.8660254037844387076, 1.000000000000000000, 0.8660254037844387076, 1.000000000000000000, 0.8660254037844387076, 1.000000000000000000, 0.8660254037844387076, 1.000000000000000000, 0.8660254037844387076, 1.000000000000000000, 0.8660254037844387076, 1.000000000000000000, 0.8660254037844387076, 1.000000000000000000, 0.8660254037844387076, 1.000000000000000000, 0.8660254037844387076, 1.000000000000000000, 0.8660254037844387076, 1.000000000000000000, 0.8660254037844387076, 1.000000000000000000, 0.8660254037844387076, 1.000000000000000000, 0.8660254037844387076, 1.000000000000000000, 0.8660254037844387076, 1.000000000000000000, 0.8660254037844387076, 1.000000000000000000, 0.8660254037844387076, 1.000000000000000000),
 ( 1.000000000000000000, 0.8660254037844387076, 1.000000000000000000, 0.8660254037844387076, 1.000000000000000000, 0.8660254037844387076, 1.000000000000000000, 0.8660254037844387076, 1.000000000000000000, 0.8660254037844387076, 1.000000000000000000, 0.8660254037844387076, 1.000000000000000000, 0.8660254037844387076, 1.000000000000000000, 0.8660254037844387076, 1.000000000000000000, 0.8660254037844387076, 1.000000000000000000, 0.8660254037844387076, 1.000000000000000000, 0.8660254037844387076, 1.000000000000000000, 0.8660254037844387076, 1.000000000000000000, 0.8660254037844387076, 1.000000000000000000, 0.8660254037844387076, 1.000000000000000000, 0.8660254037844387076, 1.000000000000000000, 0.8660254037844387076, 1.000000000000000000, 0.8660254037844387076, 1.000000000000000000, 0.8660254037844387076, 1.000000000000000000, 0.8660254037844387076, 1.000000000000000000, 0.8660254037844387076, 1.000000000000000000, 0.8660254037844387076, 1.000000000000000000, 0.8660254037844387076, 1.000000000000000000, 0.8660254037844387076, 1.000000000000000000, 0.8660254037844387076, 1.000000000000000000, 0.8660254037844387076, 1.000000000000000000, 0.8660254037844387076, 1.000000000000000000, 0.8660254037844387076, 1.000000000000000000, 0.8660254037844387076, 1.000000000000000000, 0.8660254037844387076, 1.000000000000000000, 0.8660254037844387076, 1.000000000000000000, 0.8660254037844387076, 1.000000000000000000, 0.8660254037844387076, 1.000000000000000000, 0.8660254037844387076, 1.000000000000000000, 0.8660254037844387076, 1.000000000000000000, 0.8660254037844387076, 1.000000000000000000, 0.8660254037844387076, 1.000000000000000000, 0.8660254037844387076, 1.000000000000000000, 0.8660254037844387076, 1.000000000000000000, 0.8660254037844387076, 1.000000000000000000, 0.8660254037844387076, 1.000000000000000000, 0.8660254037844387076, 1.000000000000000000, 0.8660254037844387076, 1.000000000000000000, 0.8660254037844387076, 1.000000000000000000, 0.8660254037844387076, 1.000000000000000000, 0.8660254037844387076, 1.000000000000000000, 0.8660254037844387076, 1.000000000000000000, 0.8660254037844387076, 1.000000000000000000, 0.8660254037844387076, 1.000000000000000000, 0.8660254037844387076, 1.000000000000000000, 0.8660254037844387076, 1.000000000000000000, 0.8660254037844387076, 1.000000000000000000, 0.8660254037844387076, 1.000000000000000000, 0.8660254037844387076, 1.000000000000000000, 0.8660254037844387076, 1.000000000000000000, 0.8660254037844387076, 1.000000000000000000, 0.8660254037844387076, 1.000000000000000000, 0.8660254037844387076, 1.000000000000000000, 0.8660254037844387076, 1.000000000000000000, 0.8660254037844387076, 1.000000000000000000, 0.8660254037844387076, 1.000000000000000000, 0.8660254037844387076, 1.000000000000000000, 0.8660254037844387076, 1.000000000000000000, 0.8660254037844387076, 1.000000000000000000, 0.8660254037844387076, 1.000000000000000000, 0.8660254037844387076, 1.000000000000000000, 0.8660254037844387076, 1.000000000000000000, 0.8660254037844387076, 1.000000000000000000, 0.8660254037844387076, 1.000000000000000000, 0.8660254037844387076, 1.000000000000000000, 0.8660254037844387076, 1.000000000000000000, 0.8660254037844387076, 1.000000000000000000, 0.8660254037844387076, 1.000000000000000000, 0.8660254037844387076, 1.000000000000000000, 0.8660254037844387076, 1.000000000000000000, 0.8660254037844387076, 1.000000000000000000, 0.8660254037844387076, 1.000000000000000000, 0.8660254037844387076, 1.000000000000000000, 0.8660254037844387076, 1.000000000000000000, 0.8660254037844387076, 1.000000000000000000, 0.8660254037844387076, 1.000000000000000000, 0.8660254037844387076, 1.000000000000000000, 0.8660254037844387076, 1.000000000000000000, 0.8660254037844387076, 1.000000000000000000, 0.8660254037844387076, 1.000000000000000000, 0.8660254037844387076, 1.000000000000000000, 0.8660254037844387076, 1.000000000000000000, 0.8660254037844387076, 1.000000000000000000, 0.8660254037844387076, 1.000000000000000000, 0.8660254037844387076, 1.000000000000000000, 0.8660254037844387076, 1.000000000000000000, 0.8660254037844387076, 1.000000000000000000, 0.8660254037844387076, 1.000000000000000000, 0.8660254037844387076, 1.000000000000000000, 0.8660254037844387076, 1.000000000000000000, 0.8660254037844387076, 1.000000000000000000, 0.8660254037844387076, 1.000000000000000000, 0.8660254037844387076, 1.000000000000000000, 0.8660254037844387076, 1.000000000000000000, 0.8660254037844387076, 1.000000000000000000, 0.8660254037844387076, 1.000000000000000000, 0.8660254037844387076, 1.000000000000000000, 0.8660254037844387076, 1.000000000000000000, 0.8660254037844387076, 1.000000000000000000, 0.8660254037844387076, 1.000000000000000000, 0.8660254037844387076, 1.000000000000000000, 0.8660254037844387076, 1.000000000000000000, 0.8660254037844387076, 1.000000000000000000, 0.8660254037844387076, 1.000000000000000000, 0.8660254037844387076, 1.000000000000000000, 0.8660254037844387076, 1.000000000000000000, 0.8660254037844387076, 1.000000000000000000, 0.8660254037844387076, 1.000000000000000000, 0.8660254037844387076, 1.000000000000000000, 0.8660254037844387076, 1.000000000000000000, 0.8660254037844387076, 1.000000000000000000, 0.8660254037844387076, 1.000000000000000000, 0.8660254037844387076, 1.000000000000000000, 0.8660254037844387076, 1.000000000000000000, 0.8660254037844387076, 1.000000000000000000, 0.8660254037844387076, 1.000000000000000000) ) ) 
 REPRESENTATION_ITEM ( '' )  SURFACE ( )  );
#96665 = CARTESIAN_POINT ( 'NONE',  ( 6.688963559358025002, -6.732807188596389381, 6.903494779225465727 ) ) ;
#96666 = CARTESIAN_POINT ( 'NONE',  ( 3.429849674132933846, 5.024577257953626308, -1.443375672974058777 ) ) ;
#96667 = CARTESIAN_POINT ( 'NONE',  ( 1.217902493145516463, 0.4257177869225349243, -2.128761017034991543 ) ) ;
#96668 = B_SPLINE_CURVE_WITH_KNOTS ( 'NONE', 3,
 ( #58987, #5933, #156502, #171661, #188977, #125144, #191101, #108876, #57917, #174900, #73079, #121936, #23257, #139180 ),
 .UNSPECIFIED., .F., .F.,
 ( 4, 2, 2, 2, 2, 2, 4 ),
 ( 0.000000000000000000, 0.2499999999999998890, 0.3750000000000000000, 0.5000000000000000000, 0.6250000000000000000, 0.7499999999999998890, 1.000000000000000000 ),
 .UNSPECIFIED. ) ;
#96670 = CARTESIAN_POINT ( 'NONE',  ( 5.825163275726873202, 6.825053905550038991, 1.199719254218452047 ) ) ;
#96669 = CARTESIAN_POINT ( 'NONE',  ( -11.97181042169641074, 11.37999999999999901, 0.8318531151397159373 ) ) ;
#96671 = EDGE_CURVE ( 'NONE', #70986, #148656, #103343, .T. ) ;
#96672 = CARTESIAN_POINT ( 'NONE',  ( 11.48784849554592924, 11.33049527181923111, -3.469614872287849927 ) ) ;
#96673 = DIRECTION ( 'NONE',  ( 0.000000000000000000, 0.5005768354468290715, -0.8656921114426525676 ) ) ;
#96674 = CARTESIAN_POINT ( 'NONE',  ( 2.864352374448192240, -1.292745417840787781, 1.352161534859085412 ) ) ;
#96675 = CIRCLE ( 'NONE', #183058, 0.8300000000000008482 ) ;
#96676 = CARTESIAN_POINT ( 'NONE',  ( 6.345025448074324892, -1.829860219143174982, 1.150409744987097804 ) ) ;
#96677 = CARTESIAN_POINT ( 'NONE',  ( -5.687563394514326909, 6.287294490948974968, 1.127084646392717548 ) ) ;
#96679 = CARTESIAN_POINT ( 'NONE',  ( 6.727182134110201162, 0.6069527724139511804, 1.765151538780465712 ) ) ;
#96678 = FILL_AREA_STYLE ('',( #32705 ) ) ;
#96680 = CARTESIAN_POINT ( 'NONE',  ( -1.602468905319636405E-14, -1.053124999658583638, -1.575800808251665908 ) ) ;
#96681 =( BOUNDED_CURVE ( )  B_SPLINE_CURVE ( 3, ( #184741, #85126, #119831, #103520 ),
 .UNSPECIFIED., .F., .T. ) 
 B_SPLINE_CURVE_WITH_KNOTS ( ( 4, 4 ),
 ( 1.683648326080136037, 1.706346174174820041 ),
 .UNSPECIFIED. ) 
 CURVE ( )  GEOMETRIC_REPRESENTATION_ITEM ( )  RATIONAL_B_SPLINE_CURVE ( ( 1.000000000000000000, 0.9999570677684579412, 0.9999570677684579412, 1.000000000000000000 ) ) 
 REPRESENTATION_ITEM ( '' )  );
#96682 = CARTESIAN_POINT ( 'NONE',  ( 2.314975094136799694, 1.534822137071165438, -1.140449143091977646 ) ) ;
#96683 = CARTESIAN_POINT ( 'NONE',  ( 3.643183530381717716, -1.339777920602200467, -1.156514101391445948 ) ) ;
#96684 = CARTESIAN_POINT ( 'NONE',  ( 2.244649938279310142, 1.855272219182309668, 0.4629769397326845004 ) ) ;
#96685 = CARTESIAN_POINT ( 'NONE',  ( -5.416646063859567484, 6.278174148379618735, 1.199719254218450271 ) ) ;
#96687 = CARTESIAN_POINT ( 'NONE',  ( 5.026915340915774522, -1.640707562863060520, 0.9885212758144015233 ) ) ;
#96686 = CARTESIAN_POINT ( 'NONE',  ( 7.834948825496932834, -6.134628647623485698, 7.720982897393586342 ) ) ;
#96688 = VECTOR ( 'NONE', #88760, 1000.000000000000000 ) ;
#96689 = CARTESIAN_POINT ( 'NONE',  ( 0.5445930744353514319, 3.250057683544645304, -0.4000000000000409339 ) ) ;
#96690 = CARTESIAN_POINT ( 'NONE',  ( 6.549268392505379843, 1.714383406945050980, -0.9693629108104614422 ) ) ;
#96691 = CARTESIAN_POINT ( 'NONE',  ( 1.499999999999987121, 4.545833333333352932, -0.8660254037844323793 ) ) ;
#96692 = CARTESIAN_POINT ( 'NONE',  ( 1.828540510153942922, -1.004066958311781832, -1.867862179375394005 ) ) ;
#96693 = CARTESIAN_POINT ( 'NONE',  ( 4.926551758443064699, 1.790249073151507497, 0.5424879929923772659 ) ) ;
#96695 = VERTEX_POINT ( 'NONE', #151042 ) ;
#96694 = CARTESIAN_POINT ( 'NONE',  ( 0.7326872660318053398, 0.1314506862302306234, 1.821024990000128518 ) ) ;
#96697 = CARTESIAN_POINT ( 'NONE',  ( 4.700249516990034238, 8.244041944096728969, -0.6212051699984559860 ) ) ;
#96696 = CARTESIAN_POINT ( 'NONE',  ( 4.424592250794217030, 1.359014646446855767, -1.738718759629574118 ) ) ;
#96698 = PRESENTATION_LAYER_ASSIGNMENT (  '', '', ( #68940 ) ) ;
#96699 = CARTESIAN_POINT ( 'NONE',  ( 0.6823417656249882723, -0.4072916663252490466, 1.181850606188755259 ) ) ;
#96700 = CARTESIAN_POINT ( 'NONE',  ( 2.365751517750969146, -0.4541778970535991777, 2.011898661289913903 ) ) ;
#96701 = CARTESIAN_POINT ( 'NONE',  ( 6.810273232766058449, 6.839740281182199233, 1.040834085586084257E-14 ) ) ;
#96702 = CARTESIAN_POINT ( 'NONE',  ( -8.148614017013223076, 9.465470093725620870, -1.199719254218446718 ) ) ;
#96703 = CARTESIAN_POINT ( 'NONE',  ( 1.378881877344207085, 3.612814789603054688, 0.5904953584336758432 ) ) ;
#96704 = EDGE_CURVE ( 'NONE', #38441, #176198, #70809, .T. ) ;
#96705 = CARTESIAN_POINT ( 'NONE',  ( -1.000000000000017097, 9.200000000000018829, -0.3999999999999961919 ) ) ;
#96706 = CARTESIAN_POINT ( 'NONE',  ( 8.005163354226054295, 8.304055099544019214, 0.000000000000000000 ) ) ;
#96707 = EDGE_LOOP ( 'NONE', ( #175127, #156407, #25001, #207125, #183097, #167991 ) ) ;
#96708 = CARTESIAN_POINT ( 'NONE',  ( 3.789561645344252661, -1.914057400617325433, 0.7896510022299551013 ) ) ;
#96709 = CARTESIAN_POINT ( 'NONE',  ( -1.499999999999997780, 5.400000000000022560, 1.214306433183764966E-14 ) ) ;
#96710 = CARTESIAN_POINT ( 'NONE',  ( 2.724079341238437646, -1.242159841233332562, -1.768869243570107885 ) ) ;
#96711 = CARTESIAN_POINT ( 'NONE',  ( -6.357087581413799704, 6.851358791993434671, -0.6307199548913413611 ) ) ;
#96712 = CARTESIAN_POINT ( 'NONE',  ( 2.121745675717867652, -0.4403476065239861903, 1.970919799026500607 ) ) ;
#96713 = CARTESIAN_POINT ( 'NONE',  ( 0.000000000000000000, 4.500000000000003553, 0.000000000000000000 ) ) ;
#96714 = ORIENTED_EDGE ( 'NONE', *, *, #117140, .T. ) ;
#96715 = CARTESIAN_POINT ( 'NONE',  ( 7.076992996653421741, 10.23994701519558781, -1.082531754730537976 ) ) ;
#96716 = CARTESIAN_POINT ( 'NONE',  ( -3.757017964318317471, 6.436919154129725484, 1.082531754730549967 ) ) ;
#96717 = CARTESIAN_POINT ( 'NONE',  ( -0.1179535434602772825, -2.016182236903838465, -0.04464881524945257807 ) ) ;
#96718 = CARTESIAN_POINT ( 'NONE',  ( 4.493798347139664529, -2.191065130646638437, -0.05333993539427539510 ) ) ;
#96719 = CARTESIAN_POINT ( 'NONE',  ( 1.499999999999990896, 5.306250000682820378, 1.214306433183764966E-14 ) ) ;
#96720 = CARTESIAN_POINT ( 'NONE',  ( 4.166199421025417848, 1.911861072351704882, -0.05224187775455800542 ) ) ;
#96721 = CARTESIAN_POINT ( 'NONE',  ( -2.442440228756222353, 6.001264033524212671, -0.7998128361456281477 ) ) ;
#96722 = CARTESIAN_POINT ( 'NONE',  ( 6.277061933002785032, 7.385955679000473673, 1.082531754730558626 ) ) ;
#96724 = CARTESIAN_POINT ( 'NONE',  ( 2.355092412869797869, 0.09611577090188136441, -2.014234804981252847 ) ) ;
#96723 = CARTESIAN_POINT ( 'NONE',  ( -8.798878505144649864, 11.28844422746735532, -1.443375672974058777 ) ) ;
#96725 = CARTESIAN_POINT ( 'NONE',  ( 0.6823417656249969321, 12.58854166700806942, -1.181850606188757036 ) ) ;
#96726 = CARTESIAN_POINT ( 'NONE',  ( -3.709037541790315640, 6.484905011134099340, -1.199719254218450271 ) ) ;
#96727 = CARTESIAN_POINT ( 'NONE',  ( 5.209832820053398983, -1.716139821054706749, 0.1720855783484842860 ) ) ;
#96728 = CARTESIAN_POINT ( 'NONE',  ( 0.1405533004714800693, 1.287645162063441928, -2.525240623925705474 ) ) ;
#96729 = CARTESIAN_POINT ( 'NONE',  ( 8.270110514656016321, 12.59228666716665401, 0.7216878364870438212 ) ) ;
#96730 = DIRECTION ( 'NONE',  ( -0.6483454320283800199, 0.000000000000000000, 0.7613463080411787542 ) ) ;
#96731 = DIRECTION ( 'NONE',  ( 0.3502638921866460531, -1.953969548649011959E-16, -0.9366510587354619499 ) ) ;
#96732 = ORIENTED_EDGE ( 'NONE', *, *, #211523, .T. ) ;
#96734 =( BOUNDED_CURVE ( )  B_SPLINE_CURVE ( 2, ( #81577, #96796, #144494 ),
 .UNSPECIFIED., .F., .T. ) 
 B_SPLINE_CURVE_WITH_KNOTS ( ( 3, 3 ),
 ( 0.2943294064411632327, 0.2999999999999999889 ),
 .UNSPECIFIED. ) 
 CURVE ( )  GEOMETRIC_REPRESENTATION_ITEM ( )  RATIONAL_B_SPLINE_CURVE ( ( 0.9417397705941343844, 0.9088341421182736246, 1.000000000000000000 ) ) 
 REPRESENTATION_ITEM ( '' )  );
#96733 = CARTESIAN_POINT ( 'NONE',  ( 0.7079804021624566124, 0.6528548590773939342, -1.964656565413371414 ) ) ;
#96735 =( GEOMETRIC_REPRESENTATION_CONTEXT ( 3 ) GLOBAL_UNCERTAINTY_ASSIGNED_CONTEXT ( ( #39835 ) ) GLOBAL_UNIT_ASSIGNED_CONTEXT ( ( #53915, #5124, #71199 ) ) REPRESENTATION_CONTEXT ( 'NONE', 'WORKASPACE' ) );
#96736 = ORIENTED_EDGE ( 'NONE', *, *, #99699, .T. ) ;
#96737 = CARTESIAN_POINT ( 'NONE',  ( 5.022017691244989201, -1.802217576119311770, 0.1829344734397136685 ) ) ;
#96738 = CARTESIAN_POINT ( 'NONE',  ( 4.030516805012513082, 7.924296382481737844, 0.000000000000000000 ) ) ;
#96739 = CARTESIAN_POINT ( 'NONE',  ( 5.689503332392597201, 5.810377773979076288, 0.3369718469911698322 ) ) ;
#96740 = CARTESIAN_POINT ( 'NONE',  ( 6.428355384240774129, -0.8606449381524762243, -1.593976378398887173 ) ) ;
#96741 = CARTESIAN_POINT ( 'NONE',  ( 5.411112705185558092, 6.445957923205511086, -1.082531754730548412 ) ) ;
#96742 = CARTESIAN_POINT ( 'NONE',  ( 7.968844136639799736, -5.196967604326696133, -7.583016927391841300 ) ) ;
#96743 = CARTESIAN_POINT ( 'NONE',  ( 3.574349206294104242, -2.111947977397998777, -0.5846811180381800144 ) ) ;
#96745 = CARTESIAN_POINT ( 'NONE',  ( 7.781490099239519509, 11.16582331816642260, 1.199719254218460707 ) ) ;
#96744 = CARTESIAN_POINT ( 'NONE',  ( 0.5023040531197673353, 1.956348610274569744, 0.1481081594910879096 ) ) ;
#96746 = CARTESIAN_POINT ( 'NONE',  ( 5.466386403393696192, -1.869944189333021090, -0.4150143681153609654 ) ) ;
#96747 = CARTESIAN_POINT ( 'NONE',  ( -10.50000000000000000, 10.19999999999998153, 3.599999999999999201 ) ) ;
#96748 = DIRECTION ( 'NONE',  ( 0.000000000000000000, 0.000000000000000000, -1.000000000000000000 ) ) ;
#96749 = CARTESIAN_POINT ( 'NONE',  ( -0.6823417656250003738, -0.2822916663252489355, -1.181850606188749264 ) ) ;
#96750 = CARTESIAN_POINT ( 'NONE',  ( 4.934804725694211136, 6.780358151441803649, -1.443375672974051449 ) ) ;
#96751 = CARTESIAN_POINT ( 'NONE',  ( -9.829298180227631576, 10.56986208646148384, 1.040834085586084257E-14 ) ) ;
#96752 = CARTESIAN_POINT ( 'NONE',  ( 1.885829143180400624, 1.490600019384461294, 1.565824011241300440 ) ) ;
#96753 = CARTESIAN_POINT ( 'NONE',  ( -5.204350862799341115, 7.165104988056252289, -1.599625672291271394 ) ) ;
#96754 = CARTESIAN_POINT ( 'NONE',  ( 4.420840606507738357, 7.315341919971147355, 1.199719254218451159 ) ) ;
#96755 = CARTESIAN_POINT ( 'NONE',  ( 1.430379662499326354, 1.758314708518812663, 0.4907259477668829972 ) ) ;
#96756 = CARTESIAN_POINT ( 'NONE',  ( -3.741160322367112379, 6.452105245148518797, 1.199719254218464037 ) ) ;
#96757 = CARTESIAN_POINT ( 'NONE',  ( 4.612205747861584548, -0.7811881352849485705, -1.650120847746315622 ) ) ;
#96758 = CARTESIAN_POINT ( 'NONE',  ( 11.40264643788129639, 9.090283821728826652, -6.596144476283479996 ) ) ;
#96759 = CARTESIAN_POINT ( 'NONE',  ( 2.619282413590624525, 1.617716081779559278, 1.019604094833974628 ) ) ;
#96760 = ORIENTED_EDGE ( 'NONE', *, *, #164952, .T. ) ;
#96761 = CARTESIAN_POINT ( 'NONE',  ( 3.701571259021796845, -1.489687541828330852, -1.288469680017936048 ) ) ;
#96762 = ORIENTED_EDGE ( 'NONE', *, *, #118406, .F. ) ;
#96763 = CARTESIAN_POINT ( 'NONE',  ( 5.425317942119275649, -1.235012148030777412, -1.498765763798795891 ) ) ;
#96764 = ORIENTED_EDGE ( 'NONE', *, *, #149705, .T. ) ;
#96765 = CARTESIAN_POINT ( 'NONE',  ( -5.586841817283045408, 8.675676665875643678, 1.199719254218454489 ) ) ;
#96767 = CARTESIAN_POINT ( 'NONE',  ( 5.590118541908202232, 1.264772504208915072, 1.701965355810124203 ) ) ;
#96766 = CARTESIAN_POINT ( 'NONE',  ( 7.367930134383754215, 7.560616343061329125, -0.7998128361456341429 ) ) ;
#96768 = CARTESIAN_POINT ( 'NONE',  ( -3.809456170543688458, 8.470288933811595200, -2.500000000000000444 ) ) ;
#96770 = VERTEX_POINT ( 'NONE', #117522 ) ;
#96769 = CARTESIAN_POINT ( 'NONE',  ( 2.648957786072099641, 0.2360777847093403214, 1.897596177352772306 ) ) ;
#96771 = CARTESIAN_POINT ( 'NONE',  ( 5.406339766261963220, 6.489514674222595758, -1.307707983115678152 ) ) ;
#96772 = CARTESIAN_POINT ( 'NONE',  ( -9.497255425109827343, -6.896119493545144863, 0.09872732973945987089 ) ) ;
#96773 = CARTESIAN_POINT ( 'NONE',  ( 3.984117037569365305, 5.741498858621315371, 1.599625672291261402 ) ) ;
#96774 = CIRCLE ( 'NONE', #93363, 3.150000000000000799 ) ;
#96775 = CARTESIAN_POINT ( 'NONE',  ( 5.250644345176154637, 1.983683461502975254, 0.3419521592970317103 ) ) ;
#96776 = DIRECTION ( 'NONE',  ( 3.330669073875478989E-16, -3.540251991789410786E-16, -1.000000000000000000 ) ) ;
#96777 = CARTESIAN_POINT ( 'NONE',  ( 4.740742070742828496, 0.3150700179065483719, 1.798135100120237251 ) ) ;
#96778 = CARTESIAN_POINT ( 'NONE',  ( 0.7837444799244470683, -1.966470238067185905, 0.6478734989143406509 ) ) ;
#96779 = CARTESIAN_POINT ( 'NONE',  ( -8.405692050792730186, 9.869357483088723626, 1.082531754730558626 ) ) ;
#96780 = CARTESIAN_POINT ( 'NONE',  ( -6.292453103784333202, 6.974073686386621951, 0.9489479220791104952 ) ) ;
#96781 = DIRECTION ( 'NONE',  ( 0.000000000000000000, 1.000000000000000000, 0.000000000000000000 ) ) ;
#96782 = CARTESIAN_POINT ( 'NONE',  ( 5.629731426258720361, -1.187751674602673058, -1.445209747047627946 ) ) ;
#96783 = CARTESIAN_POINT ( 'NONE',  ( 7.610204295972345712, 7.772993188256215547, 0.7998128361456341429 ) ) ;
#96784 = CARTESIAN_POINT ( 'NONE',  ( -3.737243898861318137, 7.511868315313509292, 0.7998128361456341429 ) ) ;
#96785 = EDGE_CURVE ( 'NONE', #178469, #169262, #31506, .T. ) ;
#96786 = CARTESIAN_POINT ( 'NONE',  ( 3.029357257649615054, 5.621668336311468117, -1.199719254218446718 ) ) ;
#96787 = CARTESIAN_POINT ( 'NONE',  ( -0.6823417656250039265, 10.63020833367472839, -1.181850606188755259 ) ) ;
#96788 = CARTESIAN_POINT ( 'NONE',  ( -6.087774667736030487, 7.061157519568837415, 1.199719254218450271 ) ) ;
#96790 = CARTESIAN_POINT ( 'NONE',  ( -6.071018923869249129, 10.30488218781460574, 0.7998128361456291469 ) ) ;
#96789 = CARTESIAN_POINT ( 'NONE',  ( -11.96209379583854293, 11.32792940594236519, -0.9572398070798617820 ) ) ;
#96791 = AXIS2_PLACEMENT_3D ( 'NONE', #154116, #71763, #50214 ) ;
#96792 = CARTESIAN_POINT ( 'NONE',  ( -6.175902666224832416, 7.163973517805802160, -1.199719254218446718 ) ) ;
#96793 = CARTESIAN_POINT ( 'NONE',  ( 1.059532578591013463, 1.690300726139557952, 1.195051122980017144 ) ) ;
#96794 = CARTESIAN_POINT ( 'NONE',  ( 2.179462045401040715, 1.638881033884627803, 1.340452329455198210 ) ) ;
#96795 = CARTESIAN_POINT ( 'NONE',  ( 8.613507663383630941, 8.943513783569379427, -0.7998128361456221525 ) ) ;
#96796 = CARTESIAN_POINT ( 'NONE',  ( 5.727717027299726205, 5.854960418037383540, 0.4679561398535265204 ) ) ;
#96797 = CARTESIAN_POINT ( 'NONE',  ( 0.2331713839410576583, 0.005725554726919174046, -1.953566683266183102 ) ) ;
#96798 = CARTESIAN_POINT ( 'NONE',  ( 4.867170269011318773, 6.911508770089412224, 1.419371323323643130 ) ) ;
#96799 = CARTESIAN_POINT ( 'NONE',  ( 5.843201017809841247, 5.919415396974013532, 1.040834085586084257E-14 ) ) ;
#96801 = FACE_OUTER_BOUND ( 'NONE', #189045, .T. ) ;
#96800 = CARTESIAN_POINT ( 'NONE',  ( -3.474999999999998312, -3.820833333333332416, 2.006292185433951047 ) ) ;
#96802 = CARTESIAN_POINT ( 'NONE',  ( 2.765910322896072859, 1.227222833649963540, 1.935908780871216761 ) ) ;
#96803 = CARTESIAN_POINT ( 'NONE',  ( 0.7678472254676466102, 0.8974085622692473674, 1.589837017038860045 ) ) ;
#96804 = CARTESIAN_POINT ( 'NONE',  ( 1.986440140746603911, -1.173720106059353396, 1.509789020923378189 ) ) ;
#96806 = ORIENTED_EDGE ( 'NONE', *, *, #77903, .T. ) ;
#96805 = CARTESIAN_POINT ( 'NONE',  ( 5.182959862174088883, 9.268813282503625572, 0.7998128361456331437 ) ) ;
#96807 = CARTESIAN_POINT ( 'NONE',  ( 7.917598520256366790, 8.339545816494993602, 1.040834085586084257E-14 ) ) ;
#96808 = CARTESIAN_POINT ( 'NONE',  ( 1.441653692521651653, -1.894234556111865420, 0.6821031695033189513 ) ) ;
#96809 = CARTESIAN_POINT ( 'NONE',  ( 0.5319879461419263489, 1.124744735265088780, 1.607134405190835391 ) ) ;
#96810 = CARTESIAN_POINT ( 'NONE',  ( -9.755255220232635693, 11.33988483081495957, -1.199719254218441611 ) ) ;
#96811 = CARTESIAN_POINT ( 'NONE',  ( -8.199983978166823562, 8.461069484149769337, -0.7998128361456291469 ) ) ;
#96812 = LINE ( 'NONE', #134642, #50636 ) ;
#96814 = CARTESIAN_POINT ( 'NONE',  ( 3.238855601640895809, -1.561498447111120402, 0.8330696194922878606 ) ) ;
#96813 = CARTESIAN_POINT ( 'NONE',  ( 3.503930302474305591, -0.8474990640115993568, -1.911341529346534118 ) ) ;
#96815 = CARTESIAN_POINT ( 'NONE',  ( -9.898321827459618305, 15.00000000000623857, 7.924999999990495425 ) ) ;
#96816 = CARTESIAN_POINT ( 'NONE',  ( 0.1643758432304382178, -1.428106194732338352, 1.662303017507735792 ) ) ;
#96817 = CARTESIAN_POINT ( 'NONE',  ( 5.015436155323918399, -0.9350583589616268121, -1.467585299639478702 ) ) ;
#96818 = CARTESIAN_POINT ( 'NONE',  ( 8.890396042259068210, 11.39521468743417998, -1.599625672291257406 ) ) ;
#96819 = DIRECTION ( 'NONE',  ( 0.000000000000000000, 1.000000000000000000, 0.000000000000000000 ) ) ;
#96820 = CARTESIAN_POINT ( 'NONE',  ( 4.833154173618329885, -1.132187431169606739, 1.313192701189482614 ) ) ;
#96821 = CARTESIAN_POINT ( 'NONE',  ( 4.334556721604589491, -1.253389318223859350, 1.772677672673736771 ) ) ;
#96822 = CARTESIAN_POINT ( 'NONE',  ( 3.009020027229115879, 5.597941567487558778, -1.199719254218446718 ) ) ;
#96823 = CARTESIAN_POINT ( 'NONE',  ( 5.700407750362016301, 1.350738941191354625, -1.497498989668680114 ) ) ;
#96824 = CARTESIAN_POINT ( 'NONE',  ( 6.406249999940950346, 1.895863741710943406, -0.7852924748303196090 ) ) ;
#96825 = CARTESIAN_POINT ( 'NONE',  ( -0.7500000000000215383, 4.972916667349482012, 1.299038105676671107 ) ) ;
#96826 = CARTESIAN_POINT ( 'NONE',  ( 3.205993170255555302, -1.924248618553949353, 0.09317337220685062427 ) ) ;
#96827 = CARTESIAN_POINT ( 'NONE',  ( -0.7500000000000179856, 9.822916667349467446, 1.299038105676658228 ) ) ;
#96828 = CARTESIAN_POINT ( 'NONE',  ( 6.328415579541645464, -1.046111920768664660, -1.959710881125435789 ) ) ;
#96829 = VERTEX_POINT ( 'NONE', #35124 ) ;
#96830 = CARTESIAN_POINT ( 'NONE',  ( 6.983263157960393208, 0.5798717822590447879, 1.998431770337566027 ) ) ;
#96831 = CARTESIAN_POINT ( 'NONE',  ( -1.201851678989727383E-14, 2.712500000000023892, 1.732050807568877637 ) ) ;
#96832 = CARTESIAN_POINT ( 'NONE',  ( 5.286789834324991055, 8.255339675766103724, -1.199719254218452935 ) ) ;
#96833 = CARTESIAN_POINT ( 'NONE',  ( 1.366231352279376310, 0.6402347118669349246, -2.127050378772620487 ) ) ;
#96834 = SPHERICAL_SURFACE ( 'NONE', #42734, 0.08000000000000000167 ) ;
#96835 = CARTESIAN_POINT ( 'NONE',  ( 6.588899466561449536, 9.670504563421618016, -1.082531754730537088 ) ) ;
#96836 = CARTESIAN_POINT ( 'NONE',  ( 0.5031024701319273262, 7.721748688246023562, 1.994341720826588782 ) ) ;
#96837 = CARTESIAN_POINT ( 'NONE',  ( 4.472210567661338843, 6.310941310395290493, 1.599625672291261402 ) ) ;
#96838 = B_SPLINE_CURVE_WITH_KNOTS ( 'NONE', 3,
 ( #52452, #50322, #3661, #169397, #70800, #104409, #170458, #36185, #182434, #69738, #100132 ),
 .UNSPECIFIED., .F., .F.,
 ( 4, 1, 1, 1, 1, 1, 1, 1, 4 ),
 ( 0.000000000000000000, 0.2257091236145174484, 0.3979912149639216468, 0.5260416812932605657, 0.6190739408849097458, 0.6862087210430605211, 0.7361363507675404705, 0.7768852254246026989, 0.9999999999999998890 ),
 .UNSPECIFIED. ) ;
#96839 = CARTESIAN_POINT ( 'NONE',  ( 0.08851783505585240908, -0.5350849913869708541, 1.944072358963434555 ) ) ;
#96841 = CARTESIAN_POINT ( 'NONE',  ( 6.004357462130720080, 2.060136995665005522, 0.1050117271170700056 ) ) ;
#96840 = CARTESIAN_POINT ( 'NONE',  ( 8.353795204314554468, 12.89784483834236184, -0.7998128361456352531 ) ) ;
#96842 = CARTESIAN_POINT ( 'NONE',  ( -3.469997250093771246, 6.135748327496311383, -1.199719254218452935 ) ) ;
#96843 = B_SPLINE_CURVE_WITH_KNOTS ( 'NONE', 3,
 ( #149613, #182086, #165861, #67259, #17447, #98735, #133395, #198338, #68332, #86739 ),
 .UNSPECIFIED., .F., .F.,
 ( 4, 3, 3, 4 ),
 ( 1.091119002910726144E-17, 3.125232789889730939E-05, 6.250428833270779022E-05, 0.0001046311988174829390 ),
 .UNSPECIFIED. ) ;
#96844 = CARTESIAN_POINT ( 'NONE',  ( -1.499999999999997780, 4.931250000682820378, 1.214306433183764966E-14 ) ) ;
#96845 = CARTESIAN_POINT ( 'NONE',  ( 1.364683531249988757, -0.6156249996585803075, 0.000000000000000000 ) ) ;
#96846 = CARTESIAN_POINT ( 'NONE',  ( 6.591075523649926993, 1.627300515804396941, -0.9222108319836411772 ) ) ;
#96847 = CARTESIAN_POINT ( 'NONE',  ( 5.695915039874445362, 1.533740007788013449, 0.8092579662780824412 ) ) ;
#96848 = CARTESIAN_POINT ( 'NONE',  ( 4.370479661831958573, -0.005723030808118654937, -1.740626722379432501 ) ) ;
#96849 = CARTESIAN_POINT ( 'NONE',  ( 3.846762897975340767, 5.510976019103107859, -1.599625672291256295 ) ) ;
#96850 = CARTESIAN_POINT ( 'NONE',  ( 2.859215333236740264, 0.3337469566037793989, -2.267824818490314254 ) ) ;
#96851 = CARTESIAN_POINT ( 'NONE',  ( -0.6823417656250212460, 5.113541667008086655, 1.181850606188767472 ) ) ;
#96852 = CARTESIAN_POINT ( 'NONE',  ( 1.675478281319711549, -0.9859397310463119402, 1.554705294492392254 ) ) ;
#96853 = CARTESIAN_POINT ( 'NONE',  ( 0.000000000000000000, -2.000000000000001776, 0.000000000000000000 ) ) ;
#96854 = CARTESIAN_POINT ( 'NONE',  ( -10.47807565189556911, 4.462864196998284960, -5.860964803283929214 ) ) ;
#96855 = CARTESIAN_POINT ( 'NONE',  ( 1.869861807837460921, 0.9356042063937075604, 1.567457579366556386 ) ) ;
#96856 = CARTESIAN_POINT ( 'NONE',  ( 2.320935597664942396, 0.9480396085976348086, -1.779626998253575509 ) ) ;
#96857 = CARTESIAN_POINT ( 'NONE',  ( 1.324469081069843623, 2.112754910877081560, 0.5817525768514880680 ) ) ;
#96858 = CARTESIAN_POINT ( 'NONE',  ( 9.645118626927368766, 13.59280469987849216, -8.209452448563446580 ) ) ;
#96859 = CARTESIAN_POINT ( 'NONE',  ( 3.962026973360888604, 2.090321222856437178, -0.2555144258320155015 ) ) ;
#96860 = CARTESIAN_POINT ( 'NONE',  ( -5.703176172842872482, 9.805455968292021041, 0.000000000000000000 ) ) ;
#96861 = CARTESIAN_POINT ( 'NONE',  ( 9.211430769240257277, 13.21586787862255363, 9.027972232310341738 ) ) ;
#96862 = CARTESIAN_POINT ( 'NONE',  ( 1.539598694730393680, 1.913698299121506352, -0.7905179490511196061 ) ) ;
#96863 = CARTESIAN_POINT ( 'NONE',  ( 4.547870462380197765, 7.393267075163835855, 1.199719254218462483 ) ) ;
#96864 = CARTESIAN_POINT ( 'NONE',  ( 1.360316468749973140, -0.2031249996586187434, -5.030698080332740574E-14 ) ) ;
#96865 = CARTESIAN_POINT ( 'NONE',  ( 3.791739704763209318, 1.996120715041304061, -0.7158466834289514136 ) ) ;
#96866 = CARTESIAN_POINT ( 'NONE',  ( 6.111906964637446649, -1.811269838261083232, 0.2284818145076653595 ) ) ;
#96867 = VERTEX_POINT ( 'NONE', #1541 ) ;
#96868 = CARTESIAN_POINT ( 'NONE',  ( -4.457598643843001973, 8.422558527783969851, 0.000000000000000000 ) ) ;
#96869 = CARTESIAN_POINT ( 'NONE',  ( 10.09812548408005384, 10.67556790771522124, -0.7998128361456281477 ) ) ;
#96870 = CARTESIAN_POINT ( 'NONE',  ( 5.844973620822835336, 7.912498205750389424, 1.443375672974064550 ) ) ;
#96871 = CARTESIAN_POINT ( 'NONE',  ( 3.475000000000000533, -2.902083332377417779, -2.006292185433951047 ) ) ;
#96872 = CARTESIAN_POINT ( 'NONE',  ( -5.392392409933270514, 7.314210449720692786, 1.599625672291269396 ) ) ;
#96873 = CARTESIAN_POINT ( 'NONE',  ( 3.427994306938833002, -1.989183439576122758, 0.3493681432537446563 ) ) ;
#96874 = CARTESIAN_POINT ( 'NONE',  ( 0.9914056592630847708, 1.857388527897243291, -0.9925227068504693939 ) ) ;
#96875 = CARTESIAN_POINT ( 'NONE',  ( -5.981082042284069367, 7.006959133200059142, 1.199719254218452935 ) ) ;
#96876 = CARTESIAN_POINT ( 'NONE',  ( 8.971744963941056028, 11.49012176272984931, 1.599625672291281386 ) ) ;
#96877 = CARTESIAN_POINT ( 'NONE',  ( 5.172628746253565168, 1.285086882066178937, -1.346197146212588347 ) ) ;
#96878 = CARTESIAN_POINT ( 'NONE',  ( 8.263858322729371153, 9.599921783727809910, -1.199719254218446718 ) ) ;
#96879 = CARTESIAN_POINT ( 'NONE',  ( -0.4841688312534676575, 4.104470248636722829, -0.4351271339794008930 ) ) ;
#96880 = CARTESIAN_POINT ( 'NONE',  ( -3.949167883330528372, 7.829389307186077396, 1.214306433183764966E-14 ) ) ;
#96881 = CARTESIAN_POINT ( 'NONE',  ( -9.842856333841300653, 10.58567993234409421, 0.7216878364870438212 ) ) ;
#96882 = COLOUR_RGB ( '', 0.08235294, 0.09019608, 0.10196078) ;
#96884 = CARTESIAN_POINT ( 'NONE',  ( 1.873419974815058842, -0.2433403713097622156, 1.946663811685337420 ) ) ;
#96883 = CARTESIAN_POINT ( 'NONE',  ( -5.343885102080728977, 9.386283052402845328, 0.7998128361456481317 ) ) ;
#96885 = CARTESIAN_POINT ( 'NONE',  ( 0.6378455412261313517, -1.529572671500577297, -1.527792216034072670 ) ) ;
#96887 = CARTESIAN_POINT ( 'NONE',  ( -5.687563394514326909, 6.287294490948974968, 1.127084646392717548 ) ) ;
#96886 = CARTESIAN_POINT ( 'NONE',  ( -4.911796789900812144, 8.952456364851418158, 0.7998128361456291469 ) ) ;
#96888 = CARTESIAN_POINT ( 'NONE',  ( -1.364683531250012516, 1.030208333674754062, 0.7879004041258379498 ) ) ;
#96889 = CARTESIAN_POINT ( 'NONE',  ( 2.635775109972549490, 0.08874582706053059378, -1.731711113058966633 ) ) ;
#96890 = CARTESIAN_POINT ( 'NONE',  ( 2.853125853291237579, 1.731928873650347311, -0.1707260732264591074 ) ) ;
#96892 = CARTESIAN_POINT ( 'NONE',  ( 7.375272376154084597, 9.627570410311676596, -1.443375672974057666 ) ) ;
#96891 = CARTESIAN_POINT ( 'NONE',  ( 6.305331169356420240, 1.914788864002760160, 1.287784001537124468 ) ) ;
#96893 = CARTESIAN_POINT ( 'NONE',  ( -10.47476631618627252, 5.237304525980054137, 5.169966676860812349 ) ) ;
#96894 = CARTESIAN_POINT ( 'NONE',  ( 2.636070936407476584, 0.9742463255392861399, -1.815968889038493073 ) ) ;
#96895 = CARTESIAN_POINT ( 'NONE',  ( 5.518332215962025167, 6.396807992499198292, -1.199719254218445830 ) ) ;
#96896 = CARTESIAN_POINT ( 'NONE',  ( 1.300157425512000087, -1.823841169980220167, 0.8594962466553013325 ) ) ;
#96897 = CARTESIAN_POINT ( 'NONE',  ( 6.925078400183569904, 6.033938712579569597, 2.739235483740619426 ) ) ;
#96898 = CARTESIAN_POINT ( 'NONE',  ( -3.122120512896910505, 6.864500708346841229, 0.7998128361456352531 ) ) ;
#96899 = CARTESIAN_POINT ( 'NONE',  ( 0.8308620510419548744, 0.1428995296039961560, 1.966335887032538032 ) ) ;
#96901 = CARTESIAN_POINT ( 'NONE',  ( -6.644904684473536882, 6.925012684740138980, 0.7216878364870317197 ) ) ;
#96900 = CARTESIAN_POINT ( 'NONE',  ( 4.236511230858605259, 1.172298487584079396, -1.510895503047122945 ) ) ;
#96902 = CARTESIAN_POINT ( 'NONE',  ( -5.600926855776882540, 8.588146194164741232, -1.082531754730549967 ) ) ;
#96903 = CARTESIAN_POINT ( 'NONE',  ( 7.526711554241970248, 8.810193563817646734, -1.199719254218452047 ) ) ;
#96904 = CARTESIAN_POINT ( 'NONE',  ( -7.605197822622922210, 7.837428646007010613, -0.7998128361456362523 ) ) ;
#96905 = CARTESIAN_POINT ( 'NONE',  ( 1.682291859507994092, 1.040098842697153136, 1.731126528333865933 ) ) ;
#96906 = CARTESIAN_POINT ( 'NONE',  ( 4.964078638949532163, 2.283327717301757431, -0.3329734184051634238 ) ) ;
#96907 = CARTESIAN_POINT ( 'NONE',  ( 6.461383593301071926, 1.630371061775518271, 1.090930979547571456 ) ) ;
#96908 = CARTESIAN_POINT ( 'NONE',  ( 2.289831844592318255, -1.277571413231039399, -1.488851726829776068 ) ) ;
#96909 = CARTESIAN_POINT ( 'NONE',  ( 9.694243528971124846, 11.26870452434320491, 1.199719254218450271 ) ) ;
#96910 = CARTESIAN_POINT ( 'NONE',  ( 1.491410138560286924, 1.333748936243118077, 1.500000000000000888 ) ) ;
#96911 = ORIENTED_EDGE ( 'NONE', *, *, #4772, .F. ) ;
#96912 = CARTESIAN_POINT ( 'NONE',  ( 1.341172884435502866, -1.819006327537198153, -1.083427034744638862 ) ) ;
#96913 =( BOUNDED_CURVE ( )  B_SPLINE_CURVE ( 2, ( #63814, #11853, #210047, #164521, #214282 ),
 .UNSPECIFIED., .F., .T. ) 
 B_SPLINE_CURVE_WITH_KNOTS ( ( 3, 2, 3 ),
 ( 0.2229596301642877976, 0.2250000000000000056, 0.2273783041757627965 ),
 .UNSPECIFIED. ) 
 CURVE ( )  GEOMETRIC_REPRESENTATION_ITEM ( )  RATIONAL_B_SPLINE_CURVE ( ( 0.9504573706892978091, 0.9671970730156055351, 1.000000000000000000, 0.9617641190049276423, 0.9453530113141472846 ) ) 
 REPRESENTATION_ITEM ( '' )  );
#96915 = CARTESIAN_POINT ( 'NONE',  ( -7.531718027591449705, 8.745758106066849891, 1.199719254218462483 ) ) ;
#96914 = CARTESIAN_POINT ( 'NONE',  ( -3.764360206088648297, 7.543504007078730922, -0.7998128361456281477 ) ) ;
#96916 = CARTESIAN_POINT ( 'NONE',  ( 0.6734667703603390843, -1.024904740748554532, 1.529287851792550335 ) ) ;
#96917 = ORIENTED_EDGE ( 'NONE', *, *, #114330, .F. ) ;
#96918 = CARTESIAN_POINT ( 'NONE',  ( 3.959984535978885667, -0.6353779353734061441, 2.075986281735443750 ) ) ;
#96919 = CARTESIAN_POINT ( 'NONE',  ( 11.81165604110238299, 7.954580463409317126, -2.158456547454505881 ) ) ;
#96921 = EDGE_CURVE ( 'NONE', #45318, #96984, #213018, .T. ) ;
#96920 = CARTESIAN_POINT ( 'NONE',  ( 1.600013431492643745, 1.466117565985028515, 1.532352819790145482 ) ) ;
#96922 = CARTESIAN_POINT ( 'NONE',  ( 0.7499999999999902300, 2.514583334016148974, 1.299038105676669330 ) ) ;
#96923 = CARTESIAN_POINT ( 'NONE',  ( 9.250740883225924804, 9.686952540052077509, 1.040834085586084257E-14 ) ) ;
#96924 = CARTESIAN_POINT ( 'NONE',  ( -0.3282377607281344867, 0.5513354503153581332, 1.224999999999968114 ) ) ;
#96925 = CARTESIAN_POINT ( 'NONE',  ( 2.934896792925650644, 0.2487164785463981398, 2.045624280402899231 ) ) ;
#96927 = CARTESIAN_POINT ( 'NONE',  ( 0.5031362391596030381, -1.832460416942282011, 0.1798594046882526221 ) ) ;
#96926 = CARTESIAN_POINT ( 'NONE',  ( -7.506410603460441422, 11.90922947067921278, -0.7998128361456291469 ) ) ;
#96928 = CARTESIAN_POINT ( 'NONE',  ( 0.6823417656249899377, 3.426041667008085323, -1.181850606188754593 ) ) ;
#96929 = CARTESIAN_POINT ( 'NONE',  ( -0.02244404828160087226, 6.946777552644228138, -2.784171975256703124 ) ) ;
#96930 = CARTESIAN_POINT ( 'NONE',  ( 1.425171720896451832, 3.733877413282800095, 0.4907744223921421955 ) ) ;
#96931 = CARTESIAN_POINT ( 'NONE',  ( -4.370663978927107785, 5.060324124126027279, -2.420000000000000373 ) ) ;
#96932 = CARTESIAN_POINT ( 'NONE',  ( 1.265308524177723326, -2.045349560253268084, -0.9672931750909097293 ) ) ;
#96933 = CARTESIAN_POINT ( 'NONE',  ( -10.14113571334194930, 10.93367254176152059, -0.7216878364870267237 ) ) ;
#96934 = CARTESIAN_POINT ( 'NONE',  ( 2.513665319321151337, -0.5648568745635518251, 1.721363734954905356 ) ) ;
#96935 = CARTESIAN_POINT ( 'NONE',  ( 1.780357001937494799, -0.5149467098792412934, -1.845104466984174962 ) ) ;
#96936 = CARTESIAN_POINT ( 'NONE',  ( 3.191909353267761151, -1.388477207968623839, -1.535938721777901472 ) ) ;
#96937 = CARTESIAN_POINT ( 'NONE',  ( -0.6823417656250003738, 1.030208333674752286, -1.181850606188749264 ) ) ;
#96938 = CARTESIAN_POINT ( 'NONE',  ( 1.287891803077842345, -0.8884654817012342942, 1.759997859036799284 ) ) ;
#96939 = CARTESIAN_POINT ( 'NONE',  ( 0.4988883441144418840, 1.603466095971857852, -1.067369714357151222 ) ) ;
#96940 = CARTESIAN_POINT ( 'NONE',  ( 3.151090109352538082, -1.528452604574185525, -1.078222621661927061 ) ) ;
#96941 = AXIS2_PLACEMENT_3D ( 'NONE', #47854, #64076, #192990 ) ;
#96943 = CARTESIAN_POINT ( 'NONE',  ( 4.653539691347775786, 8.417882268172059312, -0.4891605808478947104 ) ) ;
#96942 = CARTESIAN_POINT ( 'NONE',  ( 0.8214423835279326402, 2.134246884609458661, 0.8782244701446385582 ) ) ;
#96944 = CARTESIAN_POINT ( 'NONE',  ( 2.242426168690789368, -1.824373289281261634, -0.3667376154973446267 ) ) ;
#96945 = CARTESIAN_POINT ( 'NONE',  ( -1.364683531250012516, 3.280208333674756727, 0.7879004041258379498 ) ) ;
#96946 = CARTESIAN_POINT ( 'NONE',  ( 5.424308963177657539, 1.013736099364664911, 1.796294033555500658 ) ) ;
#96947 = CARTESIAN_POINT ( 'NONE',  ( -4.076197739202962467, 7.907314462378773001, 1.040834085586084257E-14 ) ) ;
#96948 = CARTESIAN_POINT ( 'NONE',  ( 7.019370843573166319, 9.212351955633947043, 1.599625672291281386 ) ) ;
#96949 = CARTESIAN_POINT ( 'NONE',  ( 11.01135777277262306, 13.50632581993708570, 1.399999999999998579 ) ) ;
#96950 = EDGE_CURVE ( 'NONE', #170253, #140850, #116448, .T. ) ;
#96951 = CARTESIAN_POINT ( 'NONE',  ( 6.317421145955757211, -0.2613792861649695265, 2.089613723330654427 ) ) ;
#96952 = CARTESIAN_POINT ( 'NONE',  ( -1.201851678989727383E-14, 2.759375000341417916, -1.575800808251660134 ) ) ;
#96953 = CARTESIAN_POINT ( 'NONE',  ( 5.729794944320468097, -1.366427417996706417, -1.674954217032841974 ) ) ;
#96954 = CARTESIAN_POINT ( 'NONE',  ( 1.188719773494644860, 1.394467456127197025, 1.202481090285527632 ) ) ;
#96955 = CARTESIAN_POINT ( 'NONE',  ( 5.215492487644303843, 1.652332223238074604, 1.161132580238199541 ) ) ;
#96956 = CARTESIAN_POINT ( 'NONE',  ( 0.6823417656249882723, 0.09270833367475139752, 1.181850606188755259 ) ) ;
#96957 = CARTESIAN_POINT ( 'NONE',  ( -4.934804725694220906, 7.740727365743146571, -1.082531754730549967 ) ) ;
#96960 = CARTESIAN_POINT ( 'NONE',  ( 5.178851490740205676, 6.104710163027444736, 1.082531754730558626 ) ) ;
#96959 = CARTESIAN_POINT ( 'NONE',  ( 6.925078400183553029, 7.053346220238264408, 2.353806654540433030 ) ) ;
#96958 = CARTESIAN_POINT ( 'NONE',  ( 8.188198428010544205, 8.517596018959260107, 0.000000000000000000 ) ) ;
#96961 = CARTESIAN_POINT ( 'NONE',  ( -5.143339171537843590, 7.093924681584509173, 1.599625672291263179 ) ) ;
#96962 = CARTESIAN_POINT ( 'NONE',  ( 4.874232570624013050, -2.001857581374043349, -0.2420344392276354561 ) ) ;
#96963 = CARTESIAN_POINT ( 'NONE',  ( -8.864333505236459132, 9.236143932397675727, 1.040834085586084257E-14 ) ) ;
#96965 = CARTESIAN_POINT ( 'NONE',  ( -6.902509602688818191, 9.146290184594002781, -1.443375672974066548 ) ) ;
#96964 = CARTESIAN_POINT ( 'NONE',  ( -3.144601563365788444, 5.756120026313656268, -1.199719254218452935 ) ) ;
#96966 = CARTESIAN_POINT ( 'NONE',  ( 1.364683531249988535, 4.905208333674756283, -0.7879004041258300672 ) ) ;
#96968 = CARTESIAN_POINT ( 'NONE',  ( -1.364683531250014514, 9.088541667008060543, -0.7879004041258335089 ) ) ;
#96967 = CARTESIAN_POINT ( 'NONE',  ( 6.174726448494309849, -2.051094451480539149, -0.6828207641706719455 ) ) ;
#96969 = CARTESIAN_POINT ( 'NONE',  ( 0.000000000000000000, 15.50000000000019362, 0.000000000000000000 ) ) ;
#96970 = CARTESIAN_POINT ( 'NONE',  ( -11.82276436367499883, 7.680992254652674767, -2.069180822227531635 ) ) ;
#96972 = CARTESIAN_POINT ( 'NONE',  ( 5.220327442464319567, 1.987051044970666647, 0.3419161450798278157 ) ) ;
#96971 = CARTESIAN_POINT ( 'NONE',  ( -6.683806541412768532, 8.820860269780128604, -1.443375672974058777 ) ) ;
#96973 = CARTESIAN_POINT ( 'NONE',  ( 1.364683531249988757, -0.05312499965857975237, 0.000000000000000000 ) ) ;
#96974 = CARTESIAN_POINT ( 'NONE',  ( 1.857592325351750118, 1.720440678145126467, -0.1246472719800949674 ) ) ;
#96975 = CARTESIAN_POINT ( 'NONE',  ( 4.329849954717849947, 6.144853928627882489, 1.599625672291262513 ) ) ;
#96977 = CARTESIAN_POINT ( 'NONE',  ( 6.994027139803230320, 9.253060644560830994, -1.599625672291267398 ) ) ;
#96976 = CARTESIAN_POINT ( 'NONE',  ( 7.470179451449751262, 7.817556902887268677, 1.040834085586084257E-14 ) ) ;
#96978 = CARTESIAN_POINT ( 'NONE',  ( -11.63550830110499135, 8.311017141679082343, -2.948455737676608290 ) ) ;
#96979 = CARTESIAN_POINT ( 'NONE',  ( 6.802024559211160337, -1.870114703409443857, 0.04643648283486622591 ) ) ;
#96980 = CARTESIAN_POINT ( 'NONE',  ( 0.8209481077818219230, 1.523044454047136176, -1.316462280350006342 ) ) ;
#96981 = DIRECTION ( 'NONE',  ( 0.000000000000000000, 0.000000000000000000, 1.000000000000000000 ) ) ;
#96982 = CARTESIAN_POINT ( 'NONE',  ( 3.382038520680182181, 1.398480293485371284, 1.707083182650385389 ) ) ;
#96983 = CARTESIAN_POINT ( 'NONE',  ( 5.559503684912662003, 1.770657277210012204, 1.256059096652543783 ) ) ;
#96984 = VERTEX_POINT ( 'NONE', #17793 ) ;
#96985 = CARTESIAN_POINT ( 'NONE',  ( 4.248501033035879004, 6.049946853332221153, -1.599625672291273171 ) ) ;
#96986 = CARTESIAN_POINT ( 'NONE',  ( 9.259855728009286580, 10.86588177317476855, -1.082531754730543083 ) ) ;
#96988 = CARTESIAN_POINT ( 'NONE',  ( 1.933220473845993492, -1.621196910160098925, -1.198842755339262212 ) ) ;
#96987 = CARTESIAN_POINT ( 'NONE',  ( 2.666775373343560407, 0.7166976873529752323, 1.995817185486338019 ) ) ;
#96990 = VERTEX_POINT ( 'NONE', #173709 ) ;
#96989 = CARTESIAN_POINT ( 'NONE',  ( 2.162115752888054576, 1.811270999727595976, 0.04120172278379052866 ) ) ;
#96991 = CARTESIAN_POINT ( 'NONE',  ( 4.715203562502613188, 8.723097599553565118, 0.7998128361456341429 ) ) ;
#96992 = VECTOR ( 'NONE', #200865, 1000.000000000000000 ) ;
#96993 = CARTESIAN_POINT ( 'NONE',  ( 5.124091990960999432, 8.065525525174782828, -1.199719254218452047 ) ) ;
#96995 = CARTESIAN_POINT ( 'NONE',  ( 0.8486862992652006721, -1.733348825135153648, -0.8160025691017428473 ) ) ;
#96994 = CARTESIAN_POINT ( 'NONE',  ( -5.115504031057831469, 4.862509545855891346, 0.7998128361456341429 ) ) ;
#96996 = DIRECTION ( 'NONE',  ( -0.6483454320283789096, 0.000000000000000000, 0.7613463080411795314 ) ) ;
#96997 = CARTESIAN_POINT ( 'NONE',  ( 9.611344009005486910, -6.731960136058449784, -0.1523027874134945669 ) ) ;
#96998 = CARTESIAN_POINT ( 'NONE',  ( 5.382223794500827552, 7.302347065049529462, -1.443375672974051449 ) ) ;
#96999 = CARTESIAN_POINT ( 'NONE',  ( -0.6823417656250246877, -0.1364583329919108468, 1.181850606188755259 ) ) ;
#97000 = FACE_OUTER_BOUND ( 'NONE', #83362, .T. ) ;
#97001 = CARTESIAN_POINT ( 'NONE',  ( -9.215791728987058562, 11.77484298861683598, -1.599625672291263179 ) ) ;
#97002 = CARTESIAN_POINT ( 'NONE',  ( 5.489210439962995736, 1.908424935776025455, -1.015307555102950010 ) ) ;
#97003 = CARTESIAN_POINT ( 'NONE',  ( -6.156811154381562012, 6.355570232966157640, 0.7216878364870257245 ) ) ;
#97004 = CARTESIAN_POINT ( 'NONE',  ( 4.909461021924244051, 6.821066840368686712, 1.443375672974065660 ) ) ;
#97005 = CARTESIAN_POINT ( 'NONE',  ( 2.092179824929023102, 1.308410154019133076, 1.668721082780571408 ) ) ;
#97007 = CARTESIAN_POINT ( 'NONE',  ( -11.82198925196379946, 4.889592154110854239, -4.884635108899213485 ) ) ;
#97006 = CARTESIAN_POINT ( 'NONE',  ( -4.791166081694341550, 4.882818525799564213, 0.4357780244859492669 ) ) ;
#97008 = CARTESIAN_POINT ( 'NONE',  ( 3.479716606839049930, 1.247861786229450543, 1.526166498753677825 ) ) ;
#97009 = CARTESIAN_POINT ( 'NONE',  ( 5.203337695038355193, 1.683698669361912259, -0.9069238330124268499 ) ) ;
#97010 = ORIENTED_EDGE ( 'NONE', *, *, #142740, .F. ) ;
#97011 = CARTESIAN_POINT ( 'NONE',  ( -15.75000000000000000, 11.29999999999999893, -1.800000000000001155 ) ) ;
#97012 = CARTESIAN_POINT ( 'NONE',  ( 0.6431357727456864515, -0.2518013131528433757, -2.054909676291870380 ) ) ;
#97013 = CARTESIAN_POINT ( 'NONE',  ( 1.904143259493733309, 1.439083257011425587, -1.304092337848123062 ) ) ;
#97014 = EDGE_LOOP ( 'NONE', ( #138020, #87095, #5452, #153618, #79661 ) ) ;
#97016 = CARTESIAN_POINT ( 'NONE',  ( 0.4637852190931108232, -7.024005807102823518, 10.66594404249596728 ) ) ;
#97015 = CARTESIAN_POINT ( 'NONE',  ( -7.770231434407805615, 8.237893892996801526, 0.000000000000000000 ) ) ;
#97018 = CARTESIAN_POINT ( 'NONE',  ( 6.470265622219697477, 8.571729197388226140, -1.599625672291262513 ) ) ;
#97017 = CARTESIAN_POINT ( 'NONE',  ( 2.414113337891873101, 1.364997783657854846, -1.583610807417460631 ) ) ;
#97019 = CARTESIAN_POINT ( 'NONE',  ( 5.194182247366869731, 7.153241603385088965, 1.443375672974064550 ) ) ;
#97021 = ORIENTED_EDGE ( 'NONE', *, *, #154979, .F. ) ;
#97020 = CARTESIAN_POINT ( 'NONE',  ( 6.481121912432155519, -1.750430003815309998, -0.7703581994758443852 ) ) ;
#97022 = CARTESIAN_POINT ( 'NONE',  ( 4.477303810882872881, 0.001702072213635372200, -2.207063162522747479 ) ) ;
#97023 = CARTESIAN_POINT ( 'NONE',  ( 3.206306947805489305, -2.204311952916749640, 0.1065802224688369715 ) ) ;
#97024 = CARTESIAN_POINT ( 'NONE',  ( 6.909851844459134362, 11.21324425184434936, -0.7998128361456291469 ) ) ;
#97025 = CARTESIAN_POINT ( 'NONE',  ( -11.84668729410370602, 12.59379487675469278, 1.399999999999998357 ) ) ;
#97026 = CARTESIAN_POINT ( 'NONE',  ( 1.488763880571321030, -1.816176428755595706, -0.5988469716494760897 ) ) ;
#97028 = CARTESIAN_POINT ( 'NONE',  ( -2.535011536075375105, 5.133042487381368701, 1.000000000000011324 ) ) ;
#97027 = MECHANICAL_DESIGN_GEOMETRIC_PRESENTATION_REPRESENTATION (  '', ( #79679 ), #24294 ) ;
#97029 = DIRECTION ( 'NONE',  ( 0.2684563758389248433, 0.000000000000000000, 0.9632918427306597087 ) ) ;
#97030 = CARTESIAN_POINT ( 'NONE',  ( 4.352052382902608763, -0.7952921280917917279, 1.911720769834826195 ) ) ;
#97032 = CARTESIAN_POINT ( 'NONE',  ( 2.272554088390315030, -1.330374092946192688, 1.703740541667747133 ) ) ;
#97031 = CARTESIAN_POINT ( 'NONE',  ( 4.197870329852989357, 3.573279226090490646, 2.499999999999999112 ) ) ;
#97033 = CARTESIAN_POINT ( 'NONE',  ( 4.142245973918059043, 0.5854081421233224836, 2.111838497463234710 ) ) ;
#97034 = CARTESIAN_POINT ( 'NONE',  ( 7.065207446497155708, 9.336104335703744539, 0.000000000000000000 ) ) ;
#97035 = SURFACE_SIDE_STYLE ('',( #65540 ) ) ;
#97036 = CARTESIAN_POINT ( 'NONE',  ( 0.006768871532348800547, 8.210909518262138107, 2.038649385027043959 ) ) ;
#97037 = ADVANCED_FACE ( 'NONE', ( #123953 ), #201628, .F. ) ;
#97038 = CARTESIAN_POINT ( 'NONE',  ( 6.547661840756936691, 6.603636667163397256, 0.7998128361456352531 ) ) ;
#97039 = CARTESIAN_POINT ( 'NONE',  ( -8.012344526598182026E-15, 14.35937500034139802, -1.575800808251669460 ) ) ;
#97040 = CARTESIAN_POINT ( 'NONE',  ( -3.305155586681401303, 7.078041627762083898, 0.7998128361456352531 ) ) ;
#97041 = CARTESIAN_POINT ( 'NONE',  ( -0.08726289061519039436, -1.242903867559573161, -1.588418431006669351 ) ) ;
#97042 = CARTESIAN_POINT ( 'NONE',  ( -9.869972641068651242, 11.57768483841065787, 1.082531754730558626 ) ) ;
#97043 = CARTESIAN_POINT ( 'NONE',  ( 4.575093719746353038, 1.890691655113156289, 0.8438020912069632562 ) ) ;
#97044 = CARTESIAN_POINT ( 'NONE',  ( 3.246621724073412096, 0.4685524532376301177, 1.868535087029847386 ) ) ;
#97045 = CARTESIAN_POINT ( 'NONE',  ( 6.081681791882147969, -0.7128978460711818954, 1.993742607474026984 ) ) ;
#97046 = CARTESIAN_POINT ( 'NONE',  ( 5.124091990960999432, 8.065525525174782828, -1.199719254218452047 ) ) ;
#97047 = CARTESIAN_POINT ( 'NONE',  ( 0.6823417656249899377, 5.676041667008087543, -1.181850606188754593 ) ) ;
#97048 = CARTESIAN_POINT ( 'NONE',  ( 3.994935505748583360, 0.2844874371618256736, 1.948636269439333546 ) ) ;
#97049 = CARTESIAN_POINT ( 'NONE',  ( 5.525394443818422374, -1.450416979558573072, -1.775029086184358507 ) ) ;
#97050 = CARTESIAN_POINT ( 'NONE',  ( 4.213378774425760476, -0.3099129147984269195, 1.799030153321119263 ) ) ;
#97051 = CARTESIAN_POINT ( 'NONE',  ( 5.709392085130549077, 9.675058176045386205, 0.000000000000000000 ) ) ;
#97052 = CARTESIAN_POINT ( 'NONE',  ( 3.646780131951580461, 7.198401220678078971, -0.7216878364870267237 ) ) ;
#97053 = CARTESIAN_POINT ( 'NONE',  ( -6.903036488013351679, 8.082572653217566128, -1.199719254218452047 ) ) ;
#97054 = CARTESIAN_POINT ( 'NONE',  ( 6.378184920586140727, 6.405913593630768510, 0.000000000000000000 ) ) ;
#97055 = ORIENTED_EDGE ( 'NONE', *, *, #73345, .T. ) ;
#97057 = CARTESIAN_POINT ( 'NONE',  ( 5.361592829351686795, -1.589796019859390563, -1.235070861824426824 ) ) ;
#97056 = CARTESIAN_POINT ( 'NONE',  ( 1.751249726499287673, 1.836263021919124050, -0.1365115386888632321 ) ) ;
#97058 = CARTESIAN_POINT ( 'NONE',  ( 5.818996626390088522, 1.136386364665368687, -1.998068361519554248 ) ) ;
#97059 = CARTESIAN_POINT ( 'NONE',  ( 5.541838416980684023, 1.314774629379747539, 1.456173869884537675 ) ) ;
#97060 = CARTESIAN_POINT ( 'NONE',  ( -7.152089726408780379, 8.302858421353754181, -1.199719254218446718 ) ) ;
#97061 = CARTESIAN_POINT ( 'NONE',  ( -5.922214171070950606, 5.803671375871217286, -0.7998128361456291469 ) ) ;
#97062 = CARTESIAN_POINT ( 'NONE',  ( -10.10343170205618968, 2.974000657016934390, -5.833219012919392377 ) ) ;
#97063 = CARTESIAN_POINT ( 'NONE',  ( -5.285699784481336927, 7.260012063351913625, 1.599625672291263179 ) ) ;
#97065 = CARTESIAN_POINT ( 'NONE',  ( 0.2681426532152464959, -1.225442487749365483, 1.413462724991432218 ) ) ;
#97064 = CARTESIAN_POINT ( 'NONE',  ( 1.944979630195432074, -1.681012947115037015, -1.242954243213564292 ) ) ;
#97066 = DIRECTION ( 'NONE',  ( -0.000000000000000000, -1.000000000000000000, -0.000000000000000000 ) ) ;
#97067 = CARTESIAN_POINT ( 'NONE',  ( 5.525317926099265087, -1.233401178653690033, -1.499961942869533438 ) ) ;
#97068 = CARTESIAN_POINT ( 'NONE',  ( -0.6823417656250212460, 3.363541667008085323, 1.181850606188767472 ) ) ;
#97069 = CARTESIAN_POINT ( 'NONE',  ( 1.241335265265028687, 1.738410175110545852, 0.08621907427421551806 ) ) ;
#97070 = CARTESIAN_POINT ( 'NONE',  ( 6.972971076130050072, 7.029554431773520129, 1.040834085586084257E-14 ) ) ;
#97071 = DIRECTION ( 'NONE',  ( 0.000000000000000000, 3.330669073875420317E-16, 1.000000000000000000 ) ) ;
#97072 = CARTESIAN_POINT ( 'NONE',  ( 1.330204427372463138, 1.661418051098985327, 0.4633224975721556005 ) ) ;
#97073 = CARTESIAN_POINT ( 'NONE',  ( 1.611130907606239004, -0.2639259086049255965, 2.175532687872412829 ) ) ;
#97074 = CARTESIAN_POINT ( 'NONE',  ( 4.108205984530819421, -2.201057848371779535, 0.1611738814469021175 ) ) ;
#97075 = CARTESIAN_POINT ( 'NONE',  ( -10.49139461985735977, 3.038394114823554482, -7.128631142076787164 ) ) ;
#97076 = CARTESIAN_POINT ( 'NONE',  ( 1.745237678848761576, -0.3157848129633227807, -2.147843386395100751 ) ) ;
#97077 = CARTESIAN_POINT ( 'NONE',  ( 1.203907071533380613, 3.118479746939697872, -0.7749999999999910294 ) ) ;
#97078 = CARTESIAN_POINT ( 'NONE',  ( 2.448581487809509571, -1.456371601587917120, 1.537162028231451538 ) ) ;
#97079 = CARTESIAN_POINT ( 'NONE',  ( 6.639320575229252341, 0.005161017367553630275, 1.896863882003448021 ) ) ;
#97080 = ADVANCED_FACE ( 'NONE', ( #207235 ), #208590, .T. ) ;
#97081 = ORIENTED_EDGE ( 'NONE', *, *, #68964, .F. ) ;
#97083 = CARTESIAN_POINT ( 'NONE',  ( -1.364683531250014514, 0.3010416670080866552, -0.7879004041258359514 ) ) ;
#97082 = CARTESIAN_POINT ( 'NONE',  ( 2.964700083287651999, -2.118976988643240578, -0.8750470330559836363 ) ) ;
#97084 = CARTESIAN_POINT ( 'NONE',  ( -11.84668730067608777, 12.59365272245204892, -1.400000000000002132 ) ) ;
#97085 = CARTESIAN_POINT ( 'NONE',  ( 5.138703914779377158, 5.953908307786102583, 1.199719254218462483 ) ) ;
#97086 = CARTESIAN_POINT ( 'NONE',  ( 5.356174596383207032, 0.9017655805138939940, -2.030186355573161627 ) ) ;
#97087 = CARTESIAN_POINT ( 'NONE',  ( -7.537970219518091319, 7.896646132300314314, -0.7216878364870278340 ) ) ;
#97088 = CARTESIAN_POINT ( 'NONE',  ( 4.636525346193557162, 7.392734756325715750, -1.082531754730549078 ) ) ;
#97089 = CARTESIAN_POINT ( 'NONE',  ( -6.683806541412762314, 9.781229484081471526, -1.082531754730537976 ) ) ;
#97090 = CARTESIAN_POINT ( 'NONE',  ( 4.584065335196261692, 7.401807753487379848, 1.082531754730549078 ) ) ;
#97091 = ORIENTED_EDGE ( 'NONE', *, *, #91598, .F. ) ;
#97092 = CARTESIAN_POINT ( 'NONE',  ( 2.988907892087853568, -2.013985899409028946, 0.1017507309580278629 ) ) ;
#97094 = CARTESIAN_POINT ( 'NONE',  ( 1.920832408274443903, -1.461550516301242775, 1.455605961035913776 ) ) ;
#97093 = CARTESIAN_POINT ( 'NONE',  ( 6.531277313481192337, 8.642909503859968368, 1.599625672291281386 ) ) ;
#97095 = CARTESIAN_POINT ( 'NONE',  ( -3.009396220815599321, 6.452359640394901952, 0.6004564335717228474 ) ) ;
#97096 = ADVANCED_FACE ( 'NONE', ( #71880 ), #42639, .T. ) ;
#97097 = CARTESIAN_POINT ( 'NONE',  ( 3.567203813726949058, 7.175838526074521440, 0.7216878364870257245 ) ) ;
#97098 = VERTEX_POINT ( 'NONE', #121811 ) ;
#97099 = CYLINDRICAL_SURFACE ( 'NONE', #40303, 4.000000000000000000 ) ;
#97100 = CARTESIAN_POINT ( 'NONE',  ( 1.364683531249988535, 5.155208333674749177, -0.7879004041258300672 ) ) ;
#97101 = CARTESIAN_POINT ( 'NONE',  ( 4.980524279605372584, -0.2661484459187679064, -2.175167798947100994 ) ) ;
#97102 = CARTESIAN_POINT ( 'NONE',  ( 2.285779929129946098, 1.617817622347239803, -1.203354541732377658 ) ) ;
#97103 = CARTESIAN_POINT ( 'NONE',  ( 2.735704033801298785, 1.827604811068459956, 0.2230458208379028362 ) ) ;
#97104 = CARTESIAN_POINT ( 'NONE',  ( 8.067265095331215718, 9.370563018429956870, 1.199719254218462483 ) ) ;
#97105 = CARTESIAN_POINT ( 'NONE',  ( 4.928627555176230857, 1.747287423663802075, 0.5288322122747670662 ) ) ;
#97106 = CARTESIAN_POINT ( 'NONE',  ( 5.977185442992979603, -2.006959616289708315, -0.1948445219252663840 ) ) ;
#97107 = CARTESIAN_POINT ( 'NONE',  ( -8.389798128758148010, 8.682519326506312751, 0.7998128361456462443 ) ) ;
#97109 = CARTESIAN_POINT ( 'NONE',  ( -4.444040490229335560, 8.406740681901359480, 0.7998128361456352531 ) ) ;
#97108 = CARTESIAN_POINT ( 'NONE',  ( 5.700151306344448443, -2.262689076517818254, -0.006432940626173094985 ) ) ;
#97110 = CARTESIAN_POINT ( 'NONE',  ( 1.032015147355441309, -1.337601665653989302, -1.626754097558680057 ) ) ;
#97111 = CARTESIAN_POINT ( 'NONE',  ( -6.831329296439251131, 9.063246493969506545, -1.599625672291271394 ) ) ;
#97112 = CARTESIAN_POINT ( 'NONE',  ( 4.264170421968140445, -2.065031762457261610, 0.1491743435546449281 ) ) ;
#97113 = CARTESIAN_POINT ( 'NONE',  ( 9.134442807305049428, 11.67993591332117376, 1.599625672291281386 ) ) ;
#97114 = FACE_OUTER_BOUND ( 'NONE', #93897, .T. ) ;
#97115 = DIRECTION ( 'NONE',  ( 0.000000000000000000, 1.000000000000000000, 0.000000000000000000 ) ) ;
#97116 = CARTESIAN_POINT ( 'NONE',  ( -7.479294296233107708, 11.87759377891399204, 0.7998128361456481317 ) ) ;
#97117 = UNCERTAINTY_MEASURE_WITH_UNIT (LENGTH_MEASURE( 1.000000000000000082E-05 ), #74601, 'distance_accuracy_value', 'NONE');
#97118 = DIRECTION ( 'NONE',  ( 3.330669073875478989E-16, -3.540251991789410786E-16, -1.000000000000000000 ) ) ;
#97119 = CARTESIAN_POINT ( 'NONE',  ( 7.523848900940885542, 7.742521570711348389, 0.7998128361456291469 ) ) ;
#97120 = CARTESIAN_POINT ( 'NONE',  ( 4.904330715672160501, 6.657863961833647259, -1.249385787368818113 ) ) ;
#97121 = CARTESIAN_POINT ( 'NONE',  ( -8.920901888112002354, 11.43080484092926241, 1.443375672974064550 ) ) ;
#97122 = CARTESIAN_POINT ( 'NONE',  ( 2.689914112924804090, 2.107969469017998421, -0.7009301692152307695 ) ) ;
#97123 = DIRECTION ( 'NONE',  ( 1.000000000000000000, 0.000000000000000000, 0.000000000000000000 ) ) ;
#97125 = CARTESIAN_POINT ( 'NONE',  ( -4.437261413422502798, 8.398831758960053406, 0.000000000000000000 ) ) ;
#97124 = AXIS2_PLACEMENT_3D ( 'NONE', #50386, #100197, #103400 ) ;
#97126 = CARTESIAN_POINT ( 'NONE',  ( 6.043183783389218355, 8.073467052085995022, 1.599625672291267398 ) ) ;
#97127 = CARTESIAN_POINT ( 'NONE',  ( 3.297265573180406584, -1.731424309613574852, 0.9225008839797432802 ) ) ;
#97128 = CARTESIAN_POINT ( 'NONE',  ( 6.308621549060418054, 6.254479983525607523, 0.7998128361456341429 ) ) ;
#97129 = CARTESIAN_POINT ( 'NONE',  ( -4.145235801320589886, 7.447099624555288067, -0.7035710955675591460 ) ) ;
#97130 = CARTESIAN_POINT ( 'NONE',  ( 3.358669367883368118, 4.941533567329135401, -1.599625672291262513 ) ) ;
#97131 = CARTESIAN_POINT ( 'NONE',  ( -5.072158865288277418, 7.010880990960010273, 1.443375672974058777 ) ) ;
#97132 = CARTESIAN_POINT ( 'NONE',  ( -6.046573322014817897, 9.998159942418544333, 0.7216878364870458196 ) ) ;
#97133 = CARTESIAN_POINT ( 'NONE',  ( 2.514065211524143084, -0.6609878990531635745, 2.015050547854141172 ) ) ;
#97134 = CARTESIAN_POINT ( 'NONE',  ( -5.822300622425855110, 5.757381912443740646, 0.7998128361456281477 ) ) ;
#97135 = CARTESIAN_POINT ( 'NONE',  ( 3.854492016355787420, 0.7758605394001509836, 2.017853709245204463 ) ) ;
#97136 = CARTESIAN_POINT ( 'NONE',  ( 3.122423488780329048, 0.04808623196613135559, 1.840796284283818363 ) ) ;
#97137 = CARTESIAN_POINT ( 'NONE',  ( -4.264599663924041550, 7.301641052403419430, 0.9184948912712449509 ) ) ;
#97138 = CARTESIAN_POINT ( 'NONE',  ( 1.364683531249986537, -0.2822916663252520997, -0.7879004041258309554 ) ) ;
#97139 = CARTESIAN_POINT ( 'NONE',  ( 5.894438200647534210, 1.418812651433436933, -1.007543873543685020 ) ) ;
#97140 = CARTESIAN_POINT ( 'NONE',  ( 6.727182134110231360, 2.105158487175392334, 2.022197281440795358 ) ) ;
#97141 = CARTESIAN_POINT ( 'NONE',  ( 5.680503174445848735, 5.729601246382692636, 1.040834085586084257E-14 ) ) ;
#97142 = CARTESIAN_POINT ( 'NONE',  ( 10.97031310326519282, 9.799999999999998934, -1.695146482106562269 ) ) ;
#97143 = CIRCLE ( 'NONE', #110934, 4.899999999999999467 ) ;
#97144 = CARTESIAN_POINT ( 'NONE',  ( 2.571340117545738657, 0.1069729528509130723, -2.159185227005658181 ) ) ;
#97145 = CARTESIAN_POINT ( 'NONE',  ( 4.059922587279920947, 1.704677108394496043, -1.076152822228809480 ) ) ;
#97146 = CARTESIAN_POINT ( 'NONE',  ( -9.951321562306267410, 10.71222269888655987, 1.040834085586084257E-14 ) ) ;
#97147 = CARTESIAN_POINT ( 'NONE',  ( 2.571340117545738657, 0.1069729528509130723, -2.159185227005658181 ) ) ;
#97148 = CARTESIAN_POINT ( 'NONE',  ( 2.811746400649973499, -1.950408978035414354, 0.2857507918755904930 ) ) ;
#97149 = CARTESIAN_POINT ( 'NONE',  ( 6.509000000000015440, 0.001920477310516938412, 2.100274754360692331 ) ) ;
#97150 = CARTESIAN_POINT ( 'NONE',  ( 4.405766152992893758, -0.8336290453338083273, -1.754189941349618920 ) ) ;
#97153 = ORIENTED_EDGE ( 'NONE', *, *, #195936, .T. ) ;
#97152 = DIRECTION ( 'NONE',  ( -0.4243160830846685605, -0.9055141421511231359, 0.000000000000000000 ) ) ;
#97151 = CARTESIAN_POINT ( 'NONE',  ( -9.476786185827959841, 10.15859809299519334, 0.7216878364870438212 ) ) ;
#97154 = CARTESIAN_POINT ( 'NONE',  ( -3.309598895067336510, 6.875299454304925284, 0.000000000000000000 ) ) ;
#97155 = CARTESIAN_POINT ( 'NONE',  ( 0.000000000000000000, 0.5000000000000000000, 10.75000000000000000 ) ) ;
#97157 = EDGE_LOOP ( 'NONE', ( #206117, #150568, #210240, #201106 ) ) ;
#97156 = CARTESIAN_POINT ( 'NONE',  ( -5.224688093219839402, 7.188831756880171397, -1.599625672291271394 ) ) ;
#97158 = CARTESIAN_POINT ( 'NONE',  ( -9.178506806327330736, 10.77097469787910455, 1.082531754730558626 ) ) ;
#97159 = CARTESIAN_POINT ( 'NONE',  ( 1.624349867039249329, -1.226448341774049267, -1.834376716147153363 ) ) ;
#97160 = CARTESIAN_POINT ( 'NONE',  ( 1.001543065824772753E-15, -1.421874999522042327, 3.793834371823811669 ) ) ;
#97161 = CARTESIAN_POINT ( 'NONE',  ( 5.453941704850034711, -0.7095916301838971485, 1.829088932523432964 ) ) ;
#97162 = CARTESIAN_POINT ( 'NONE',  ( -1.364683531250010295, 5.592708333674750953, 0.7879004041258379498 ) ) ;
#97163 = CARTESIAN_POINT ( 'NONE',  ( -1.500000000000013101, 2.910416667349485120, -0.8660254037844313801 ) ) ;
#97164 = CARTESIAN_POINT ( 'NONE',  ( 5.943008360174058424, 6.124345481070006869, -0.7360307644482602107 ) ) ;
#97165 = CARTESIAN_POINT ( 'NONE',  ( 0.07499057489260964326, 4.092262291754148684, -2.510514182268712702 ) ) ;
#97166 = CARTESIAN_POINT ( 'NONE',  ( 4.804558796598876746, 1.603369264058150279, 0.9048477820690554729 ) ) ;
#97167 = ORIENTED_EDGE ( 'NONE', *, *, #186498, .F. ) ;
#97168 = CARTESIAN_POINT ( 'NONE',  ( -3.355169270512988773E-14, 2.500000000682816026, -1.414508159514599628 ) ) ;
#97169 = CARTESIAN_POINT ( 'NONE',  ( -8.342344591110322227, 8.627156865917170236, -0.7998128361456291469 ) ) ;
#97170 = DIRECTION ( 'NONE',  ( 0.000000000000000000, 0.000000000000000000, -1.000000000000000000 ) ) ;
#97172 = EDGE_CURVE ( 'NONE', #105253, #72492, #188759, .T. ) ;
#97171 = CARTESIAN_POINT ( 'NONE',  ( 5.572555445586866441, 0.8612648569810870125, 1.938019255899057658 ) ) ;
#97173 = CARTESIAN_POINT ( 'NONE',  ( -9.488641820551102057, -8.233137084989836652, 0.4644097342743139234 ) ) ;
#97174 = CARTESIAN_POINT ( 'NONE',  ( 6.661133543015731462, 6.665743976473484267, -0.7998128361456281477 ) ) ;
#97175 = CARTESIAN_POINT ( 'NONE',  ( 6.309851081105539272, -2.045767358615140807, 0.2475669877257078710 ) ) ;
#97178 = CARTESIAN_POINT ( 'NONE',  ( 3.175182228840720988, 1.170341537027960843, 1.421418621496411516 ) ) ;
#97177 = CARTESIAN_POINT ( 'NONE',  ( 1.873285555135986824, -0.2318667498520594894, 1.846494694648516788 ) ) ;
#97176 = CARTESIAN_POINT ( 'NONE',  ( 10.50000000000000178, 12.69999999999998153, 3.599999999999999201 ) ) ;
#97179 = CARTESIAN_POINT ( 'NONE',  ( 7.259501185113382604, 10.55683625168592243, -1.199719254218441611 ) ) ;
#97180 = CARTESIAN_POINT ( 'NONE',  ( -6.257970421159510188, 9.458660037064859694, 1.199719254218452047 ) ) ;
#97182 = ORIENTED_EDGE ( 'NONE', *, *, #3914, .F. ) ;
#97181 = CARTESIAN_POINT ( 'NONE',  ( 0.6124999999999707345, 2.145833334016141070, 1.060881119635899816 ) ) ;
#97183 = CARTESIAN_POINT ( 'NONE',  ( 3.774219598512587037, 1.225428716765289749, 1.835190637982798023 ) ) ;
#97184 = CARTESIAN_POINT ( 'NONE',  ( 5.466221857368295467, 1.108383815247836690, 1.972225493889906867 ) ) ;
#97185 = AXIS2_PLACEMENT_3D ( 'NONE', #36689, #136354, #4169 ) ;
#97186 = CARTESIAN_POINT ( 'NONE',  ( -6.778713617152821058, 7.971215977175476475, 1.082531754730549967 ) ) ;
#97187 = CARTESIAN_POINT ( 'NONE',  ( 6.187769672300552415, 1.730736780639136496, -0.5351268960485565662 ) ) ;
#97188 = CARTESIAN_POINT ( 'NONE',  ( 5.630082600720735186, 1.913861949906026538, 0.08686293782892740012 ) ) ;
#97189 = CARTESIAN_POINT ( 'NONE',  ( -2.440293211016301606E-15, 1.187499999999993117, -1.225000000000025624 ) ) ;
#97190 = CARTESIAN_POINT ( 'NONE',  ( 6.719622092096638966, -1.813896567892055112, 0.4569536213836836169 ) ) ;
#97191 = ADVANCED_FACE ( 'NONE', ( #189922 ), #89710, .T. ) ;
#97192 = CARTESIAN_POINT ( 'NONE',  ( 5.670303652858919463, -0.8369403475225531963, -1.662290214344812833 ) ) ;
#97193 = CARTESIAN_POINT ( 'NONE',  ( 1.734723475976807094E-15, 15.42733875946000133, 11.91973154060105955 ) ) ;
#97194 = CARTESIAN_POINT ( 'NONE',  ( 6.508682224664005922, 1.308065493886721775, -1.192407281889706905 ) ) ;
#97195 = CARTESIAN_POINT ( 'NONE',  ( 1.464077725791514517, -1.074659653367866952, 1.706114136832518779 ) ) ;
#97197 = CARTESIAN_POINT ( 'NONE',  ( 2.508543264270487683, -0.8067718606631252287, -1.945620686511064790 ) ) ;
#97196 = CARTESIAN_POINT ( 'NONE',  ( -9.938290294017125603, 11.55342575023019691, -1.199719254218441611 ) ) ;
#97198 = CARTESIAN_POINT ( 'NONE',  ( 8.880754312151170282, 10.31963377138658089, 1.199719254218453823 ) ) ;
#97200 = CARTESIAN_POINT ( 'NONE',  ( -10.15235809853472126, 10.73883929124566983, -0.7998128361456291469 ) ) ;
#97199 = CYLINDRICAL_SURFACE ( 'NONE', #18051, 10.25000000000000000 ) ;
#97201 =( LENGTH_UNIT ( ) NAMED_UNIT ( * ) SI_UNIT ( .MILLI., .METRE. ) );
#97202 = CARTESIAN_POINT ( 'NONE',  ( 2.777608160125254688, 0.2920557517631214295, -1.998411540393054020 ) ) ;
#97203 = CARTESIAN_POINT ( 'NONE',  ( 1.364683531249990311, 3.884375000341417028, 1.214306433183764966E-14 ) ) ;
#97204 = ADVANCED_FACE ( 'NONE', ( #6880 ), #120126, .T. ) ;
#97205 = CARTESIAN_POINT ( 'NONE',  ( 3.684065054611349144, 5.321161868511784299, -1.599625672291262513 ) ) ;
#97206 = CARTESIAN_POINT ( 'NONE',  ( 2.987745815084281276, 1.526290923294726820, 1.530918043534036599 ) ) ;
#97207 = CARTESIAN_POINT ( 'NONE',  ( 6.610000000000026077, 2.442988107647511509, 2.382821027452782570 ) ) ;
#97209 = CARTESIAN_POINT ( 'NONE',  ( 7.777967379493318845, -9.999999999999994671, 7.744830294503448620 ) ) ;
#97208 = CARTESIAN_POINT ( 'NONE',  ( 5.671053392266061977, 9.838255734277600695, 0.7998128361456331437 ) ) ;
#97210 = CARTESIAN_POINT ( 'NONE',  ( 9.585251414737269826, 11.24551007435741568, -1.082531754730537088 ) ) ;
#97211 = CARTESIAN_POINT ( 'NONE',  ( 9.398454900782844845, 13.71746517427355627, -7.461324637964940720 ) ) ;
#97212 = CARTESIAN_POINT ( 'NONE',  ( -6.371969008742801144, 10.37778824360119145, 0.7216878364870458196 ) ) ;
#97213 = CARTESIAN_POINT ( 'NONE',  ( -0.6823417656250003738, 0.9677083336747521747, -1.181850606188749264 ) ) ;
#97214 = CARTESIAN_POINT ( 'NONE',  ( 2.208753784402537335, 1.959192758111829136, 0.9821998110004714899 ) ) ;
#97215 = CARTESIAN_POINT ( 'NONE',  ( -3.023105066167323329, 5.702484939155337607, -2.420000000000000373 ) ) ;
#97216 = CARTESIAN_POINT ( 'NONE',  ( 2.255063695347800934, -1.748954272965432155, 1.435335380440343256 ) ) ;
#97217 = CARTESIAN_POINT ( 'NONE',  ( -8.830438121202295321, 9.196599317691152464, -0.7998128361456291469 ) ) ;
#97218 = CARTESIAN_POINT ( 'NONE',  ( -3.592547517496941900, 5.214391408544949869, -1.443375672974051449 ) ) ;
#97219 = CARTESIAN_POINT ( 'NONE',  ( -1.364683531249997417, 3.571875000341423245, 1.214306433183764966E-14 ) ) ;
#97220 = CARTESIAN_POINT ( 'NONE',  ( 6.233692552841108458, 6.917895963632635592, 0.8214459722771473293 ) ) ;
#97221 = CARTESIAN_POINT ( 'NONE',  ( 1.499999999999993117, 11.10416666666666785, 0.8660254037844409281 ) ) ;
#97222 = CARTESIAN_POINT ( 'NONE',  ( 5.872089928494542477, 9.864872326636710653, 0.000000000000000000 ) ) ;
#97223 = CARTESIAN_POINT ( 'NONE',  ( 3.303702144000867591, -1.767878013958000150, 0.08340844992380143375 ) ) ;
#97224 = CARTESIAN_POINT ( 'NONE',  ( 6.440462174652990868, 2.181831651002089423, 0.3301269925025315799 ) ) ;
#97225 = CARTESIAN_POINT ( 'NONE',  ( -1.364683531250010295, 9.630208333674735499, 0.7879004041258445001 ) ) ;
#97226 = CARTESIAN_POINT ( 'NONE',  ( -4.437261413422502798, 8.398831758960053406, 0.000000000000000000 ) ) ;
#97227 = CARTESIAN_POINT ( 'NONE',  ( 4.675407748274028386, 1.496063595514389721, 1.352143027241403450 ) ) ;
#97228 = ORIENTED_EDGE ( 'NONE', *, *, #32740, .F. ) ;
#97229 = CARTESIAN_POINT ( 'NONE',  ( 3.397188523315307407, 1.473948685399184111, 1.151750840393983344 ) ) ;
#97230 = CARTESIAN_POINT ( 'NONE',  ( 3.204029340230400091, 0.7494766052340908757, -1.929994576353490032 ) ) ;
#97231 = CIRCLE ( 'NONE', #20963, 0.5000000000000015543 ) ;
#97232 = CARTESIAN_POINT ( 'NONE',  ( -7.729556973122450714, 8.190440354830551328, 0.000000000000000000 ) ) ;
#97233 = FACE_BOUND ( 'NONE', #144787, .T. ) ;
#97234 = CARTESIAN_POINT ( 'NONE',  ( -9.348561386899501002, 3.999985931113709814, -7.001914024221969512 ) ) ;
#97235 =( NAMED_UNIT ( * ) SI_UNIT ( $, .STERADIAN. ) SOLID_ANGLE_UNIT ( ) );
#97236 = CARTESIAN_POINT ( 'NONE',  ( 1.364683531249990311, 4.446875000341417028, 1.214306433183764966E-14 ) ) ;
#97237 = CARTESIAN_POINT ( 'NONE',  ( 1.318461241437279607, -0.6911404020932455650, -1.783297644634279200 ) ) ;
#97238 = CARTESIAN_POINT ( 'NONE',  ( 3.086327779807009009, 1.092107249913790712, -1.629585102321646328 ) ) ;
#97239 = CARTESIAN_POINT ( 'NONE',  ( 1.194685229111978497, -1.276845315561925931, -1.560263297373874813 ) ) ;
#97240 = CARTESIAN_POINT ( 'NONE',  ( -3.786470039966538970, 7.639575156594750283, 0.000000000000000000 ) ) ;
#97242 = CARTESIAN_POINT ( 'NONE',  ( -1.264911064067355984, 3.850000000000006306, -0.5000000000000004441 ) ) ;
#97241 = CARTESIAN_POINT ( 'NONE',  ( 8.932124273304774320, 9.315233161810734686, 0.7998128361456462443 ) ) ;
#97243 = CARTESIAN_POINT ( 'NONE',  ( 6.503199639966785739, 1.637674054957323433, 1.097108698291071827 ) ) ;
#97244 = CARTESIAN_POINT ( 'NONE',  ( -0.6823417656250003738, 2.967708333674754062, -1.181850606188749264 ) ) ;
#97245 = CARTESIAN_POINT ( 'NONE',  ( 2.408449855729302591, -2.008082631278225616, -0.1440398445633188362 ) ) ;
#97247 = CARTESIAN_POINT ( 'NONE',  ( 2.021262997689095897, -1.889599275135231071, 0.9552078933684378104 ) ) ;
#97246 = CARTESIAN_POINT ( 'NONE',  ( -5.585596099150174965, 9.460353182409786399, -0.7216878364870207285 ) ) ;
#97248 = CARTESIAN_POINT ( 'NONE',  ( 8.360103901485762989, 14.02891420676280987, -8.609295381564869842 ) ) ;
#97249 = CARTESIAN_POINT ( 'NONE',  ( 3.297389726143421740, -1.827171938055579536, 0.9735347560282039403 ) ) ;
#97250 = CARTESIAN_POINT ( 'NONE',  ( 3.711900195091365262, 7.552577004240394132, -0.7998128361456362523 ) ) ;
#97252 = CARTESIAN_POINT ( 'NONE',  ( 2.706824224222692088, 6.309712028235118453, 0.7998128361456362523 ) ) ;
#97251 = CARTESIAN_POINT ( 'NONE',  ( 5.806606243248950250, 1.843357943042901459, 0.9862787698241348711 ) ) ;
#97254 = ORIENTED_EDGE ( 'NONE', *, *, #127848, .T. ) ;
#97253 = CARTESIAN_POINT ( 'NONE',  ( 4.119992258926360229, -0.9384382104282267267, -1.565754920925747973 ) ) ;
#97255 = CARTESIAN_POINT ( 'NONE',  ( 10.53876547652418338, 11.18964789890005918, 0.7998128361456462443 ) ) ;
#97256 = FILL_AREA_STYLE ('',( #195807 ) ) ;
#97257 = CARTESIAN_POINT ( 'NONE',  ( 9.898415338264832997, 12.56653357618227318, -7.886274193477667893 ) ) ;
#97258 = CARTESIAN_POINT ( 'NONE',  ( 6.124089168553260798, -1.220954261165616783, -1.838047742986161026 ) ) ;
#97259 = CARTESIAN_POINT ( 'NONE',  ( 0.6823417656249969321, 10.58854166700806587, -1.181850606188757036 ) ) ;
#97260 = EDGE_LOOP ( 'NONE', ( #119416, #135212, #127701, #67498, #123164 ) ) ;
#97261 = CARTESIAN_POINT ( 'NONE',  ( 5.408822929737922003, -0.4686924282312036061, -1.853821656156897646 ) ) ;
#97262 = CARTESIAN_POINT ( 'NONE',  ( -10.13202086811422475, 10.71511252242175161, -0.7998128361456291469 ) ) ;
#97263 = CARTESIAN_POINT ( 'NONE',  ( 7.253775878511261155, 8.421492265473332850, 1.199719254218462483 ) ) ;
#97264 = CARTESIAN_POINT ( 'NONE',  ( -0.6801582343750420812, 1.880208333674727950, -1.178068619123883165 ) ) ;
#97265 = CARTESIAN_POINT ( 'NONE',  ( 2.684151225381301575, 6.075334163012737321, 0.000000000000000000 ) ) ;
#97266 = CARTESIAN_POINT ( 'NONE',  ( 9.500232605408204023, -7.619382996155577459, 0.01181297548900739694 ) ) ;
#97268 = EDGE_CURVE ( 'NONE', #13166, #128202, #14358, .T. ) ;
#97267 = CARTESIAN_POINT ( 'NONE',  ( 8.223666246221556619, 14.19229986755559558, -8.739774625693256027 ) ) ;
#97269 = CARTESIAN_POINT ( 'NONE',  ( 0.6261898170028465938, 0.1349980957352381883, 1.836376839866371569 ) ) ;
#97270 = EDGE_LOOP ( 'NONE', ( #167324, #83529, #59960, #124882 ) ) ;
#97271 = CIRCLE ( 'NONE', #83482, 4.000000000000000000 ) ;
#97272 = CARTESIAN_POINT ( 'NONE',  ( -6.129167961829681488, 9.308390501180058507, -1.199719254218452047 ) ) ;
#97273 = CARTESIAN_POINT ( 'NONE',  ( 4.692568346783878575, -0.4079999995015987091, -1.825350503840660110 ) ) ;
#97274 = CARTESIAN_POINT ( 'NONE',  ( -11.06297021485807797, 13.75669301487472218, 0.9089447062504983910 ) ) ;
#97275 = CARTESIAN_POINT ( 'NONE',  ( 11.84668730067608777, 11.00634727754795250, -1.400000000000001910 ) ) ;
#97276 = CARTESIAN_POINT ( 'NONE',  ( 0.04160618626039885859, 14.52029232702615325, 11.99061297704356299 ) ) ;
#97277 = CARTESIAN_POINT ( 'NONE',  ( -5.012700657095048307, 7.921469694614043711, 1.075264880722737182 ) ) ;
#97278 = CARTESIAN_POINT ( 'NONE',  ( -5.205967797967562483, 8.057084283395347768, 1.082531754730548412 ) ) ;
#97279 = CARTESIAN_POINT ( 'NONE',  ( 5.148345644887269756, 7.029489223833707001, -1.599625672291256295 ) ) ;
#97280 = CARTESIAN_POINT ( 'NONE',  ( 1.797640638355556320, -1.422838571669628127, -1.361938172677351400 ) ) ;
#97281 = CARTESIAN_POINT ( 'NONE',  ( 2.126577575561945821, 0.4445254776237593242, 1.966640697269490312 ) ) ;
#97282 = CARTESIAN_POINT ( 'NONE',  ( -8.290974629956718189, 9.631557475493025322, -1.199719254218446718 ) ) ;
#97283 = CARTESIAN_POINT ( 'NONE',  ( 6.039231080244466199, 6.010467446565510130, 0.7998128361456352531 ) ) ;
#97284 = CARTESIAN_POINT ( 'NONE',  ( 6.938893903907228378E-15, 10.64264068711930733, 1.214306433183764966E-14 ) ) ;
#97285 = CARTESIAN_POINT ( 'NONE',  ( 3.029421956395737858, -1.472182739719897215, -1.623467934892895759 ) ) ;
#97286 = CARTESIAN_POINT ( 'NONE',  ( -9.646789991323334590, 11.21334206375407305, 1.199719254218462483 ) ) ;
#97287 = CARTESIAN_POINT ( 'NONE',  ( 1.313174662617483834, 8.310476012147658409, 10.86148356754323885 ) ) ;
#97288 = EDGE_CURVE ( 'NONE', #76748, #135683, #95412, .T. ) ;
#97289 = CARTESIAN_POINT ( 'NONE',  ( 4.421367491832282504, 5.291255174293369556, 1.082531754730549078 ) ) ;
#97290 = CARTESIAN_POINT ( 'NONE',  ( 7.262363838414439776, 11.62450824479221900, 0.7998128361456462443 ) ) ;
#97291 = CARTESIAN_POINT ( 'NONE',  ( -2.493739017041110895, 8.265916556960572592, -2.456386464945111481 ) ) ;
#97292 = CARTESIAN_POINT ( 'NONE',  ( 6.888951449519509218, 7.209733910627123876, -0.7216878364870317197 ) ) ;
#97293 = ORIENTED_EDGE ( 'NONE', *, *, #76293, .F. ) ;
#97295 = CARTESIAN_POINT ( 'NONE',  ( 1.963540897105001459, -1.618223010570983611, -1.197281337589267247 ) ) ;
#97294 = CARTESIAN_POINT ( 'NONE',  ( 4.827609030688454261, 0.9420861819694618111, -1.581835861328761528 ) ) ;
#97296 = CARTESIAN_POINT ( 'NONE',  ( 2.812212034788389214, -1.912053501320301718, 1.275153900055803646 ) ) ;
#97298 = CARTESIAN_POINT ( 'NONE',  ( 1.656853885927531689, 1.525116498273047405, -1.066097284832379755 ) ) ;
#97297 = FACE_OUTER_BOUND ( 'NONE', #5828, .T. ) ;
#97299 = CARTESIAN_POINT ( 'NONE',  ( 1.642778471875000035, -2.676041666188708756, -2.845375778867859751 ) ) ;
#97300 = CARTESIAN_POINT ( 'NONE',  ( -9.523113340799540083, 15.37812852751596004, -7.301473413204503160 ) ) ;
#97301 = CARTESIAN_POINT ( 'NONE',  ( 5.607647405131535479, 1.452367144367059826, 1.244281684088064166 ) ) ;
#97302 = CARTESIAN_POINT ( 'NONE',  ( -7.621654909176601045, 12.04368116068139472, 0.7998128361456481317 ) ) ;
#97303 = CARTESIAN_POINT ( 'NONE',  ( -5.858531774880906262, 6.967946837850073294, 1.082531754730549078 ) ) ;
#97305 = CARTESIAN_POINT ( 'NONE',  ( 3.977312496258199825, 1.761605600429091201, -0.6297503393934977822 ) ) ;
#97304 = CARTESIAN_POINT ( 'NONE',  ( 5.355056023315875713, 0.4066876561409601964, -2.050628154503638889 ) ) ;
#97306 = CARTESIAN_POINT ( 'NONE',  ( 7.293923454472080792, 9.532663335016016148, 1.443375672974076540 ) ) ;
#97307 = CARTESIAN_POINT ( 'NONE',  ( 5.899929530298204661, -0.6689130865737795695, -1.715630562827724637 ) ) ;
#97308 = CARTESIAN_POINT ( 'NONE',  ( 4.844340958784499662, 4.546152628203684820, 0.7998128361456341429 ) ) ;
#97310 = CARTESIAN_POINT ( 'NONE',  ( 3.669453130792974971, 7.432779085900453886, 1.040834085586084257E-14 ) ) ;
#97309 = CARTESIAN_POINT ( 'NONE',  ( 0.1172869779874900348, -7.889939693150851419, -10.99948653685772726 ) ) ;
#97311 = CARTESIAN_POINT ( 'NONE',  ( 4.916472993244619616, 1.186103633638861288, -1.252587755385982771 ) ) ;
#97312 = CARTESIAN_POINT ( 'NONE',  ( -5.442708600882160574, 8.437244903416123876, -1.199719254218446718 ) ) ;
#97313 =( BOUNDED_SURFACE ( )  B_SPLINE_SURFACE ( 3, 3, ( 
 ( #138412, #174129, #90736, #139487, #38766, #91810, #158920, #60339, #142702, #208711, #105946 ),
 ( #74468, #9461, #171970, #206586, #23561, #22485, #89669, #6235, #40916, #109173, #154653 ),
 ( #187137, #76591, #104847, #72307, #10516, #190331, #41992, #204433, #58215, #108100, #56086 ),
 ( #122244, #189277, #8386, #188202, #39839, #92874, #155720, #7305, #205515, #25702, #75533 ),
 ( #57147, #141644, #170893, #24629, #123313, #107022, #207653, #173046, #59274, #156799, #140573 ),
 ( #125430, #191395, #43060, #175186, #194606, #98200, #63549, #97140, #12648, #159985, #13716 ),
 ( #15836, #193547, #129705, #31065, #161052, #11587, #64614, #163194, #48388, #176245, #112368 ) ),
 .UNSPECIFIED., .T., .F., .T. ) 
 B_SPLINE_SURFACE_WITH_KNOTS ( ( 4, 3, 4 ),
 ( 4, 1, 1, 1, 1, 1, 1, 1, 4 ),
 ( 0.000000000000000000, 0.5000000000000000000, 1.000000000000000000 ),
 ( 0.000000000000000000, 0.2254101072112788262, 0.3970395454107691902, 0.5239558410346354389, 0.6152342776129972046, 0.6800502191696807808, 0.7279184599320936977, 0.7685697607527866015, 1.000000000000000000 ),
 .UNSPECIFIED. ) 
 GEOMETRIC_REPRESENTATION_ITEM ( )  RATIONAL_B_SPLINE_SURFACE ( (
 ( 1.000000000000000000, 1.000000000000000000, 1.000000000000000222, 1.000000000000000222, 0.9999999999999996669, 1.000000000000000222, 0.9999999999999994449, 1.000000000000000222, 0.9999999999999992228, 1.000000000000000000, 1.000000000000000000),
 ( 0.3333333333333333703, 0.3333333333333333703, 0.3333333333333334259, 0.3333333333333333703, 0.3333333333333333148, 0.3333333333333334814, 0.3333333333333332593, 0.3333333333333334259, 0.3333333333333330928, 0.3333333333333333703, 0.3333333333333333703),
 ( 0.3333333333333333703, 0.3333333333333333703, 0.3333333333333334259, 0.3333333333333333703, 0.3333333333333333148, 0.3333333333333334814, 0.3333333333333332593, 0.3333333333333334259, 0.3333333333333330928, 0.3333333333333333703, 0.3333333333333333703),
 ( 1.000000000000000000, 1.000000000000000000, 1.000000000000000222, 1.000000000000000222, 0.9999999999999996669, 1.000000000000000222, 0.9999999999999994449, 1.000000000000000222, 0.9999999999999992228, 1.000000000000000000, 1.000000000000000000),
 ( 0.3333333333333333703, 0.3333333333333333703, 0.3333333333333334259, 0.3333333333333333703, 0.3333333333333333148, 0.3333333333333334814, 0.3333333333333332593, 0.3333333333333334259, 0.3333333333333330928, 0.3333333333333333703, 0.3333333333333333703),
 ( 0.3333333333333333703, 0.3333333333333333703, 0.3333333333333334259, 0.3333333333333333703, 0.3333333333333333148, 0.3333333333333334814, 0.3333333333333332593, 0.3333333333333334259, 0.3333333333333330928, 0.3333333333333333703, 0.3333333333333333703),
 ( 1.000000000000000000, 1.000000000000000000, 1.000000000000000222, 1.000000000000000222, 0.9999999999999996669, 1.000000000000000222, 0.9999999999999994449, 1.000000000000000222, 0.9999999999999992228, 1.000000000000000000, 1.000000000000000000) ) ) 
 REPRESENTATION_ITEM ( '' )  SURFACE ( )  );
#97314 = PRODUCT_DEFINITION_FORMATION_WITH_SPECIFIED_SOURCE ( 'ANY', '', #207916, .NOT_KNOWN. ) ;
#97315 = DIRECTION ( 'NONE',  ( 0.000000000000000000, -1.000000000000000000, 0.000000000000000000 ) ) ;
#97316 = DIRECTION ( 'NONE',  ( 0.000000000000000000, 0.000000000000000000, 1.000000000000000000 ) ) ;
#97317 = VECTOR ( 'NONE', #142999, 1000.000000000000000 ) ;
#97318 = PLANE ( 'NONE',  #196990 ) ;
#97319 = CARTESIAN_POINT ( 'NONE',  ( 4.223599041728074432, 0.2716450895321539383, -2.153977947863388476 ) ) ;
#97320 = CARTESIAN_POINT ( 'NONE',  ( 3.809063337113669068, 1.566667275063510445, 0.9371452329686791316 ) ) ;
#97321 = CARTESIAN_POINT ( 'NONE',  ( 0.9011314981347726683, -1.685442764318560771, 1.003610994683441948 ) ) ;
#97322 = CARTESIAN_POINT ( 'NONE',  ( 5.471900407082693540, -0.9496530807377671080, 1.892462605218522720 ) ) ;
#97323 = AXIS2_PLACEMENT_3D ( 'NONE', #13323, #143369, #115163 ) ;
#97325 = CARTESIAN_POINT ( 'NONE',  ( -1.364683531249997417, 4.571875000341417028, 1.214306433183764966E-14 ) ) ;
#97324 = CARTESIAN_POINT ( 'NONE',  ( 6.409759596795807646, -1.076414324555999391, -2.023967322820482639 ) ) ;
#97326 = CARTESIAN_POINT ( 'NONE',  ( 3.325722479477248861, 7.699077257575519972, 2.499999999999998224 ) ) ;
#97327 = CARTESIAN_POINT ( 'NONE',  ( 8.052653171512838881, 11.48218023581863001, -1.199719254218446718 ) ) ;
#97328 = CARTESIAN_POINT ( 'NONE',  ( 2.104293207771616991, -0.9040658786637757460, 1.918231223523607865 ) ) ;
#97329 = CARTESIAN_POINT ( 'NONE',  ( -4.636525346193588248, 4.511627113421689650, 0.7216878364870317197 ) ) ;
#97330 = CARTESIAN_POINT ( 'NONE',  ( -5.111060722227552588, 6.025620933095978238, 1.082531754730546636 ) ) ;
#97331 = CARTESIAN_POINT ( 'NONE',  ( 6.034065736706932803, 1.286768452391522377, 1.748546487445822750 ) ) ;
#97333 = CARTESIAN_POINT ( 'NONE',  ( 1.499999999999997113, 13.42708333401613174, -0.8660254037844378194 ) ) ;
#97332 = CARTESIAN_POINT ( 'NONE',  ( 6.883263157960364254, 2.038911835798001171, 2.358809022084580764 ) ) ;
#97335 = EDGE_LOOP ( 'NONE', ( #60810, #183818, #184861, #77651 ) ) ;
#97334 = CARTESIAN_POINT ( 'NONE',  ( 2.877807283724475251, 0.3237236903097116536, -2.197462771414046223 ) ) ;
#97336 = CARTESIAN_POINT ( 'NONE',  ( -0.1394461523061351904, -0.009327122704730000241, -2.280146446826665230 ) ) ;
#97338 = CARTESIAN_POINT ( 'NONE',  ( 5.594603800059450904, 2.031116569408123240, 0.3580809986778245024 ) ) ;
#97337 = CARTESIAN_POINT ( 'NONE',  ( 4.334856428067313416, 6.080418470877079429, -1.599625672291256295 ) ) ;
#97340 = CARTESIAN_POINT ( 'NONE',  ( 1.737499999999999378, -1.516666666666666163, -3.009438278150925683 ) ) ;
#97339 = CARTESIAN_POINT ( 'NONE',  ( 4.529305835417093640, 7.441884687032027657, -1.199719254218450271 ) ) ;
#97341 = EDGE_CURVE ( 'NONE', #23962, #169987, #2358, .T. ) ;
#97342 = CARTESIAN_POINT ( 'NONE',  ( 5.737035277238070385, 6.722237907313067140, -1.199719254218452047 ) ) ;
#97343 = CARTESIAN_POINT ( 'NONE',  ( 3.285556943750000514, -0.3135416661887098777, 1.896917185911906500 ) ) ;
#97344 = CARTESIAN_POINT ( 'NONE',  ( 0.2333540202161792088, 2.022347194651296753, -2.461825824937914575 ) ) ;
#97345 = CARTESIAN_POINT ( 'NONE',  ( 5.548353751603532835, -1.447698842669535413, 1.137588655622793876 ) ) ;
#97346 = EDGE_CURVE ( 'NONE', #183546, #6442, #57339, .T. ) ;
#97347 = CARTESIAN_POINT ( 'NONE',  ( 4.436542580169809291, 6.199052314996659874, 1.599625672291267398 ) ) ;
#97348 = CARTESIAN_POINT ( 'NONE',  ( 1.500562974171329333, 1.412943827846969702, -0.9888553570028703055 ) ) ;
#97349 = CARTESIAN_POINT ( 'NONE',  ( 0.1105650446291406575, 1.931126588553159884, 0.5807481968119407867 ) ) ;
#97350 = CARTESIAN_POINT ( 'NONE',  ( 1.495234749544295250, -2.280609600776092094, 0.2875172478875551163 ) ) ;
#97351 = CARTESIAN_POINT ( 'NONE',  ( -1.201851678989727383E-14, 3.884375000341423689, 1.575800808251672791 ) ) ;
#97352 = CARTESIAN_POINT ( 'NONE',  ( 1.915646641569005659, -0.2780824042511415017, 2.245213254143724413 ) ) ;
#97353 = CARTESIAN_POINT ( 'NONE',  ( 4.143269384990833970, -1.832638288540566318, 1.037631460274644812 ) ) ;
#97354 = CARTESIAN_POINT ( 'NONE',  ( -6.102578539926875933, 10.13377570664109051, 0.7216878364870267237 ) ) ;
#97355 = CARTESIAN_POINT ( 'NONE',  ( 2.969704930451398717, 0.9433242808821461489, 1.497149023046380423 ) ) ;
#97356 = CARTESIAN_POINT ( 'NONE',  ( 6.745345117998789775, 7.828323044875442172, 1.199719254218462483 ) ) ;
#97357 = CARTESIAN_POINT ( 'NONE',  ( 5.858531774436539052, 6.007577623030311287, 0.000000000000000000 ) ) ;
#97358 = CARTESIAN_POINT ( 'NONE',  ( -5.545448523189368650, 6.428443684264421698, -1.199719254218446718 ) ) ;
#97359 = UNCERTAINTY_MEASURE_WITH_UNIT (LENGTH_MEASURE( 1.000000000000000082E-05 ), #56717, 'distance_accuracy_value', 'NONE');
#97360 = CARTESIAN_POINT ( 'NONE',  ( -1.402160292154681736E-14, 2.587500000000023892, -1.732050807568863648 ) ) ;
#97361 = CARTESIAN_POINT ( 'NONE',  ( 5.853820293109783357, -1.608621682386938589, -1.532244055152881312 ) ) ;
#97362 = CARTESIAN_POINT ( 'NONE',  ( 3.134921595499224445, -1.932508288125428741, 1.033376004005027715 ) ) ;
#97363 = CARTESIAN_POINT ( 'NONE',  ( -3.425406365747000859, 7.148057860013469877, 1.040834085586084257E-14 ) ) ;
#97364 = DIRECTION ( 'NONE',  ( -5.551115123125758667E-17, 0.000000000000000000, 1.000000000000000000 ) ) ;
#97365 = CARTESIAN_POINT ( 'NONE',  ( 6.463548717370299457, -1.702720583769131490, -1.263627255760652046 ) ) ;
#97366 = CARTESIAN_POINT ( 'NONE',  ( -1.364683531250012516, 3.530208333674758059, 0.7879004041258379498 ) ) ;
#97367 = CARTESIAN_POINT ( 'NONE',  ( -1.364683531250014514, 8.588541667008067648, -0.7879004041258335089 ) ) ;
#97368 = CARTESIAN_POINT ( 'NONE',  ( -3.131570295076647525, 6.597323077657299528, 1.040834085586084257E-14 ) ) ;
#97369 = CARTESIAN_POINT ( 'NONE',  ( 6.170199167347634628, 2.114832956739281400, -0.1575216572810705096 ) ) ;
#97370 = CARTESIAN_POINT ( 'NONE',  ( -6.455090533882206216, 7.663932056684933158, -1.082531754730549967 ) ) ;
#97371 = VERTEX_POINT ( 'NONE', #193122 ) ;
#97373 = FILL_AREA_STYLE_COLOUR ( '', #146715 ) ;
#97372 = CARTESIAN_POINT ( 'NONE',  ( -4.665414256878293031, 7.496714828783040296, -1.082531754730549967 ) ) ;
#97374 = CARTESIAN_POINT ( 'NONE',  ( 4.330940004561544043, 7.140181541042074365, -1.199719254218452047 ) ) ;
#97375 = CARTESIAN_POINT ( 'NONE',  ( 5.899929530298204661, -0.6689130865737795695, -1.715630562827724637 ) ) ;
#97376 = DIRECTION ( 'NONE',  ( -0.000000000000000000, 1.000000000000000000, -0.000000000000000000 ) ) ;
#97377 = CARTESIAN_POINT ( 'NONE',  ( -2.428612866367529932E-14, 2.999999999999999112, 7.500000000000000000 ) ) ;
#97378 = CARTESIAN_POINT ( 'NONE',  ( 1.364683531249990311, 3.446875000341416584, 1.214306433183764966E-14 ) ) ;
#97379 = CARTESIAN_POINT ( 'NONE',  ( 2.225747907193951214, 1.688420964825324555, 0.4218146122960535482 ) ) ;
#97380 = CARTESIAN_POINT ( 'NONE',  ( -5.188547179131282938, 7.398091417871301978, -1.250000002070928096 ) ) ;
#97381 = CARTESIAN_POINT ( 'NONE',  ( 0.6605093422152423788, -0.6574743052488278838, -1.848563176889833626 ) ) ;
#97382 = CARTESIAN_POINT ( 'NONE',  ( 0.6823417656249882723, -0.3447916663252489911, 1.181850606188755259 ) ) ;
#97383 = LINE ( 'NONE', #164496, #146252 ) ;
#97384 = CARTESIAN_POINT ( 'NONE',  ( 6.350466702034289312, 0.6732396885240909956, 2.054270918568662729 ) ) ;
#97385 = CARTESIAN_POINT ( 'NONE',  ( -8.435144125996554720, 12.99275191363802229, 0.7998128361456341429 ) ) ;
#97386 = AXIS2_PLACEMENT_3D ( 'NONE', #18565, #83570, #84641 ) ;
#97387 = CARTESIAN_POINT ( 'NONE',  ( -5.382223794500827552, 9.223085493652217082, -0.7216878364870207285 ) ) ;
#97388 = CARTESIAN_POINT ( 'NONE',  ( 6.315313271410192719, -0.2696487299426887363, 2.144762774094311375 ) ) ;
#97390 = EDGE_LOOP ( 'NONE', ( #92360, #71911 ) ) ;
#97389 = DIRECTION ( 'NONE',  ( 0.000000000000000000, 0.000000000000000000, 1.000000000000000000 ) ) ;
#97391 = CARTESIAN_POINT ( 'NONE',  ( -0.6823417656249969321, 3.967708333674754950, -1.181850606188749264 ) ) ;
#97392 = CARTESIAN_POINT ( 'NONE',  ( 5.923112194766430250, -0.05102361969991364710, 1.970867320657720301 ) ) ;
#97393 = CARTESIAN_POINT ( 'NONE',  ( 5.149590220011600827, -0.2133714078210862675, -1.720544222028724146 ) ) ;
#97395 = CARTESIAN_POINT ( 'NONE',  ( 2.437293137456029157, -1.626093413141915134, -1.469474007205706645 ) ) ;
#97394 = CARTESIAN_POINT ( 'NONE',  ( 1.360316468749957597, -0.5052083329919204724, 0.7853790794159082322 ) ) ;
#97396 = CARTESIAN_POINT ( 'NONE',  ( 3.065757340968386035, 0.3400709678853690021, -2.282286004074239649 ) ) ;
#97397 = CARTESIAN_POINT ( 'NONE',  ( 6.415316853601439995, -0.2566941480561866773, 2.044681889290477894 ) ) ;
#97398 = CARTESIAN_POINT ( 'NONE',  ( 1.411946100005515126, 1.304364503314077162, -1.438846909250802053 ) ) ;
#97399 = CARTESIAN_POINT ( 'NONE',  ( -6.521108698048783126, 7.670676904887464786, -1.082531754730543083 ) ) ;
#97400 = PRODUCT_DEFINITION_SHAPE ( 'NONE', 'NONE',  #214429 ) ;
#97401 = CARTESIAN_POINT ( 'NONE',  ( -3.156015896931072540, 6.904045323053366268, 0.000000000000000000 ) ) ;
#97402 = CARTESIAN_POINT ( 'NONE',  ( -5.608481899782703728, 5.650097288974007981, -0.3354201317723095599 ) ) ;
#97403 = CARTESIAN_POINT ( 'NONE',  ( 4.096021571020786567, 1.387573888390711385, 1.603661410755026440 ) ) ;
#97404 =( NAMED_UNIT ( * ) SI_UNIT ( $, .STERADIAN. ) SOLID_ANGLE_UNIT ( ) );
#97405 = CARTESIAN_POINT ( 'NONE',  ( 1.828750219146151323, 0.7691198443132395424, -1.864169014999479623 ) ) ;
#97406 = CARTESIAN_POINT ( 'NONE',  ( -6.195713011320807873, 6.330679389403470303, -0.7216878364870267237 ) ) ;
#97407 = CARTESIAN_POINT ( 'NONE',  ( 4.577303723630254062, 0.003709267837189236805, -2.206952907291927168 ) ) ;
#97408 = CARTESIAN_POINT ( 'NONE',  ( -1.642778471874998480, -0.8385416661887100664, 2.845375778867863303 ) ) ;
#97409 = CARTESIAN_POINT ( 'NONE',  ( -2.123823618835070537, 5.629544655282869847, 1.040834085586084257E-14 ) ) ;
#97410 = CARTESIAN_POINT ( 'NONE',  ( -4.792515913634093623E-13, -7.868798029037626485, 9.500000000000001776 ) ) ;
#97411 = CARTESIAN_POINT ( 'NONE',  ( -6.749980374757255319, 8.968339418673846097, 1.599625672291269396 ) ) ;
#97413 = CARTESIAN_POINT ( 'NONE',  ( -9.836090041150098884, -8.872041098393765424, 0.1716895903079178054 ) ) ;
#97412 = CARTESIAN_POINT ( 'NONE',  ( -5.519007765018521638, 7.558588572879005874, 1.349693927849420438 ) ) ;
#97414 = CARTESIAN_POINT ( 'NONE',  ( 0.000000000000000000, 2.999999999999999112, -2.420000000000000373 ) ) ;
#97415 = VERTEX_POINT ( 'NONE', #194190 ) ;
#97416 = CARTESIAN_POINT ( 'NONE',  ( 4.838775396685393915, 0.3501730741383273782, 2.030750449888196751 ) ) ;
#97417 = CARTESIAN_POINT ( 'NONE',  ( 1.499999999999987566, 2.244000000000016648, 2.508000000000020435 ) ) ;
#97418 = FACE_OUTER_BOUND ( 'NONE', #45062, .T. ) ;
#97419 = CARTESIAN_POINT ( 'NONE',  ( -4.120788623549732854, 6.895004929861607401, -1.199719254218452047 ) ) ;
#97420 = CARTESIAN_POINT ( 'NONE',  ( 3.229170203573806130, 1.826861024573895653, 0.8614713780644381869 ) ) ;
#97421 = CARTESIAN_POINT ( 'NONE',  ( -1.500000000000013101, 0.6708333333333583726, 0.8660254037844403729 ) ) ;
#97422 = CARTESIAN_POINT ( 'NONE',  ( 8.568389894156670294, 12.94027927658408217, -0.7216878364870257245 ) ) ;
#97423 = CARTESIAN_POINT ( 'NONE',  ( 7.633404179693907388, 8.864391950186421454, -1.199719254218441611 ) ) ;
#97424 = VECTOR ( 'NONE', #120757, 1000.000000000000000 ) ;
#97425 = CARTESIAN_POINT ( 'NONE',  ( 3.397389285588784169, 1.623555618760182062, 1.269252347208242870 ) ) ;
#97426 = LINE ( 'NONE', #15061, #17645 ) ;
#97427 = CARTESIAN_POINT ( 'NONE',  ( 4.656335691289526402, 7.519809842224722374, -1.199719254218452047 ) ) ;
#97428 = CARTESIAN_POINT ( 'NONE',  ( -0.2408018239684330541, 4.084923768815020395, -2.655285172934387372 ) ) ;
#97429 = CARTESIAN_POINT ( 'NONE',  ( 1.095364067855080448, -1.841320589428995236, -0.001981933617903330457 ) ) ;
#97430 = CARTESIAN_POINT ( 'NONE',  ( -0.01646294620048001714, -0.1635519927996042511, -2.271437254364586877 ) ) ;
#97431 = CARTESIAN_POINT ( 'NONE',  ( 5.525830126021535449, 8.604496359403894346, -1.199719254218452047 ) ) ;
#97432 = CARTESIAN_POINT ( 'NONE',  ( 2.724079341238437646, -1.242159841233332562, -1.768869243570107885 ) ) ;
#97433 = CARTESIAN_POINT ( 'NONE',  ( -5.124618876285560454, 5.081069565195661220, 0.7216878364870317197 ) ) ;
#97434 = CARTESIAN_POINT ( 'NONE',  ( 1.411342602523330214, -1.897109289313268166, 0.6839406069230756779 ) ) ;
#97435 = MECHANICAL_DESIGN_GEOMETRIC_PRESENTATION_REPRESENTATION (  '', ( #176897 ), #194204 ) ;
#97436 = CARTESIAN_POINT ( 'NONE',  ( 2.777091360721035240, -2.273647235919952880, 0.3355521655935486125 ) ) ;
#97437 = LINE ( 'NONE', #213276, #132193 ) ;
#97438 = CARTESIAN_POINT ( 'NONE',  ( -0.02103505235494400674, 7.063943641280277852, 3.970081552354725485 ) ) ;
#97439 = CARTESIAN_POINT ( 'NONE',  ( 4.311372413323046437, -0.3381597629931332172, 1.942102657548309796 ) ) ;
#97440 = CARTESIAN_POINT ( 'NONE',  ( 4.997279897388729353, -0.2910847460899004258, 1.995267753224789997 ) ) ;
#97442 = CARTESIAN_POINT ( 'NONE',  ( 8.053180056393003383, 12.33920113252646367, 1.040834085586084257E-14 ) ) ;
#97441 = CARTESIAN_POINT ( 'NONE',  ( -1.364683531250012516, 2.988541667008091096, -0.7879004041258289570 ) ) ;
#97444 = CARTESIAN_POINT ( 'NONE',  ( 6.129533150132032482, -1.983608965904083421, 0.7080540597134558078 ) ) ;
#97443 = CARTESIAN_POINT ( 'NONE',  ( -5.215082642750900277, 9.236013516518044142, 0.000000000000000000 ) ) ;
#97445 = CARTESIAN_POINT ( 'NONE',  ( 6.877413708759195998, -0.1538780216673047430, 2.036608477593480959 ) ) ;
#97446 = CARTESIAN_POINT ( 'NONE',  ( 6.006425746053997372, 6.966250444273174303, -1.199719254218445830 ) ) ;
#97447 = CARTESIAN_POINT ( 'NONE',  ( -5.713871673155502151, 8.753601821068331290, 1.199719254218452047 ) ) ;
#97448 = CARTESIAN_POINT ( 'NONE',  ( -1.482143263342189154, 8.748906972890436506, 2.523193690251313459 ) ) ;
#97449 = CARTESIAN_POINT ( 'NONE',  ( 4.399269495383588691, 1.582840427583383613, 1.175083439883710890 ) ) ;
#97450 = CARTESIAN_POINT ( 'NONE',  ( 5.888927314555610693, -1.919185580196127283, -0.6297945592430991280 ) ) ;
#97451 = CARTESIAN_POINT ( 'NONE',  ( 1.499999999999987121, 0.03541666734948738238, 0.8660254037844524744 ) ) ;
#97452 = CARTESIAN_POINT ( 'NONE',  ( 4.371882800840491967, 2.239072524489620353, -0.5581132647194796403 ) ) ;
#97453 = CARTESIAN_POINT ( 'NONE',  ( 1.815356060102671698, -1.766853000457936806, -1.063981086615989113 ) ) ;
#97454 = CARTESIAN_POINT ( 'NONE',  ( 6.480434237652121787, 9.543961796360731498, 1.082531754730558626 ) ) ;
#97455 = CARTESIAN_POINT ( 'NONE',  ( 5.825163275726873202, 6.825053905550038991, 1.199719254218452047 ) ) ;
#97456 = CARTESIAN_POINT ( 'NONE',  ( 5.273195401072370281, 5.116759154198018855, -0.7998128361456481317 ) ) ;
#97457 = CARTESIAN_POINT ( 'NONE',  ( -1.364683531250014514, 0.09270833367475767028, 0.7879004041258379498 ) ) ;
#97458 = CARTESIAN_POINT ( 'NONE',  ( 3.393283585170187688, 7.180857625999046867, 0.7998128361456271485 ) ) ;
#97459 = CARTESIAN_POINT ( 'NONE',  ( 6.114364089638786304, 8.156510742710487705, 1.443375672974076540 ) ) ;
#97460 = CARTESIAN_POINT ( 'NONE',  ( 4.334556721604589491, -1.253389318223859350, 1.772677672673736771 ) ) ;
#97462 = CARTESIAN_POINT ( 'NONE',  ( 3.104851637799400876, -0.3563606998662186554, 1.806257425991746546 ) ) ;
#97461 = CARTESIAN_POINT ( 'NONE',  ( -2.643476764984671767, 6.027880625883323518, 1.040834085586084257E-14 ) ) ;
#97463 = CARTESIAN_POINT ( 'NONE',  ( 1.364683531249988535, 4.113541667008088432, 0.7879004041258500513 ) ) ;
#97464 = CARTESIAN_POINT ( 'NONE',  ( 5.583573808894983337, -0.9862700065477579825, 1.957137920222583372 ) ) ;
#97465 = CARTESIAN_POINT ( 'NONE',  ( 7.695957533950816831, 14.38956844792682688, 9.210281496461904638 ) ) ;
#97466 = CARTESIAN_POINT ( 'NONE',  ( 6.491137613139088991, 1.972399245366265985, -1.108330356262598126 ) ) ;
#97467 = CARTESIAN_POINT ( 'NONE',  ( -5.435328143874127882, 6.463069452080541843, -1.319038057358821403 ) ) ;
#97468 = CARTESIAN_POINT ( 'NONE',  ( 4.641000714467984345, 8.433135692799648808, 0.4354600853693716411 ) ) ;
#97469 = CARTESIAN_POINT ( 'NONE',  ( -5.275531169048901958, 8.208517892982092334, -1.082531754730549967 ) ) ;
#97470 = CARTESIAN_POINT ( 'NONE',  ( 2.957086901556340575, 6.464035461875470290, 0.7216878364870257245 ) ) ;
#97471 = CARTESIAN_POINT ( 'NONE',  ( 6.819637456808122167, -1.715783256332433115, 0.4333192982870024967 ) ) ;
#97472 = CARTESIAN_POINT ( 'NONE',  ( -8.012344526598182026E-15, 12.29687500034140513, -1.575800808251669460 ) ) ;
#97473 = VECTOR ( 'NONE', #189425, 1000.000000000000000 ) ;
#97474 = CARTESIAN_POINT ( 'NONE',  ( 3.967443207080887380, -1.674941000623398457, -1.116458483097344301 ) ) ;
#97475 = CARTESIAN_POINT ( 'NONE',  ( 6.012151052656117933, 9.101594430485762999, 1.199719254218460707 ) ) ;
#97476 = CARTESIAN_POINT ( 'NONE',  ( 2.485502531088045419, 1.925919180164997746, -0.8524081271456557252 ) ) ;
#97477 = CARTESIAN_POINT ( 'NONE',  ( 2.284663151613754550, 1.537047112958013440, -1.143011353438025957 ) ) ;
#97478 = CARTESIAN_POINT ( 'NONE',  ( 3.521367211247359741, 5.131347717920458962, -1.599625672291262513 ) ) ;
#97479 = CARTESIAN_POINT ( 'NONE',  ( 3.068762047175084717, 1.428394590129605346, -1.356294421569247177 ) ) ;
#97480 = CARTESIAN_POINT ( 'NONE',  ( 1.815107966846595255, -0.2319292346777863389, 1.856160199827073587 ) ) ;
#97481 = CARTESIAN_POINT ( 'NONE',  ( 1.064813361795993618, 1.487921858168140377, -1.278797858372302088 ) ) ;
#97484 = EDGE_LOOP ( 'NONE', ( #29216, #104355, #187889, #132691, #69211 ) ) ;
#97483 = CARTESIAN_POINT ( 'NONE',  ( 0.5449873876890098945, 0.1430962203496731200, 1.907122450762772647 ) ) ;
#97482 = CARTESIAN_POINT ( 'NONE',  ( 4.090264520950432470, -1.706510830129988499, -0.2501320830878352997 ) ) ;
#97486 = CARTESIAN_POINT ( 'NONE',  ( 5.666945020832177882, 6.674152614801420746, 1.082531754730558626 ) ) ;
#97485 = CARTESIAN_POINT ( 'NONE',  ( 1.295869073816724226, 1.673045085319382119, 1.439284050222865652 ) ) ;
#97487 = CARTESIAN_POINT ( 'NONE',  ( 1.364683531249986537, 0.7177083336747527298, -0.7879004041258239610 ) ) ;
#97488 = EDGE_CURVE ( 'NONE', #176917, #99973, #85004, .T. ) ;
#97489 = CARTESIAN_POINT ( 'NONE',  ( 6.561405567229332547, 0.3174558530528899247, -1.843364171016811603 ) ) ;
#97490 = CARTESIAN_POINT ( 'NONE',  ( 0.000000000000000000, 2.999999999999999112, 0.000000000000000000 ) ) ;
#97491 = CARTESIAN_POINT ( 'NONE',  ( 0.000000000000000000, 0.000000000000000000, 6.123233995736775897E-17 ) ) ;
#97492 = EDGE_LOOP ( 'NONE', ( #68934, #44809, #26612, #21881 ) ) ;
#97493 = CARTESIAN_POINT ( 'NONE',  ( 6.385608392048681026, -1.951384585020640383, 0.6918703269920487564 ) ) ;
#97494 = CARTESIAN_POINT ( 'NONE',  ( 1.223191768902037957, -1.870915810643185795, -0.8869332102946840823 ) ) ;
#97495 = CARTESIAN_POINT ( 'NONE',  ( 0.7499999999999902300, 1.983333333333357817, 1.299038105676669330 ) ) ;
#97496 = CARTESIAN_POINT ( 'NONE',  ( 6.799577732453452761, 7.891594428405881878, -1.199719254218446718 ) ) ;
#97497 = CARTESIAN_POINT ( 'NONE',  ( -7.609150525767646833, 9.900428251527500834, -1.599625672291263179 ) ) ;
#97498 = CARTESIAN_POINT ( 'NONE',  ( 4.716257332707354699, 6.595662536282280719, -1.599625672291269396 ) ) ;
#97499 = CARTESIAN_POINT ( 'NONE',  ( 5.865915527372128402, 0.6157079936559420874, -2.029145397309819021 ) ) ;
#97500 = CARTESIAN_POINT ( 'NONE',  ( 4.167152111353856547, 5.955039778036558040, 1.599625672291262513 ) ) ;
#97501 = B_SPLINE_CURVE_WITH_KNOTS ( 'NONE', 3,
 ( #172873, #74294, #140390, #24444, #125256, #107928 ),
 .UNSPECIFIED., .F., .F.,
 ( 4, 2, 4 ),
 ( 1.997645371451378118E-16, 3.619701867389574191E-05, 7.239403734759171957E-05 ),
 .UNSPECIFIED. ) ;
#97502 = CARTESIAN_POINT ( 'NONE',  ( -1.402160292154681736E-14, 1.446875000341420137, -1.575800808251659024 ) ) ;
#97503 = ORIENTED_EDGE ( 'NONE', *, *, #204577, .F. ) ;
#97504 = CARTESIAN_POINT ( 'NONE',  ( -1.201851678989727383E-14, 2.712500000000023892, 1.732050807568877637 ) ) ;
#97506 = CARTESIAN_POINT ( 'NONE',  ( 3.846762897975340767, 5.510976019103107859, -1.599625672291256295 ) ) ;
#97505 = CARTESIAN_POINT ( 'NONE',  ( 6.496542546517183325, 1.940334402339534581, 0.2891159199209930031 ) ) ;
#97507 = CARTESIAN_POINT ( 'NONE',  ( 4.112657547701242144, 0.6818919214185631406, -1.897407125352356339 ) ) ;
#97508 = CARTESIAN_POINT ( 'NONE',  ( 3.714002460163209562, 1.020071527678518164, -1.621341143276352703 ) ) ;
#97509 = CARTESIAN_POINT ( 'NONE',  ( -1.907862554904992569, 3.236716050607336914, -0.4606469147255816132 ) ) ;
#97510 = CARTESIAN_POINT ( 'NONE',  ( 1.365048776756357940, 0.1565470504056795942, -2.186014887712848243 ) ) ;
#97511 =( BOUNDED_SURFACE ( )  B_SPLINE_SURFACE ( 3, 2, ( 
 ( #136424, #152656, #6381 ),
 ( #202440, #4238, #135361 ),
 ( #56225, #3172, #19438 ),
 ( #54095, #37840, #118094 ),
 ( #39983, #103917, #151604 ),
 ( #155862, #201376, #72452 ),
 ( #137491, #85518, #169963 ),
 ( #36759, #153728, #5297 ) ),
 .UNSPECIFIED., .F., .F., .T. ) 
 B_SPLINE_SURFACE_WITH_KNOTS ( ( 4, 2, 2, 4 ),
 ( 3, 3 ),
 ( 0.000000000000000000, 0.0005109843281227174992, 0.0007664764921840762487, 0.001021968656245434998 ),
 ( 0.000000000000000000, 1.000000000000000000 ),
 .UNSPECIFIED. ) 
 GEOMETRIC_REPRESENTATION_ITEM ( )  RATIONAL_B_SPLINE_SURFACE ( (
 ( 1.000000000000000000, 0.7045118851637607316, 1.000000000000000000),
 ( 1.000000000000000000, 0.6478559580225851100, 1.000000000000000000),
 ( 1.000000000000000000, 0.5832506164441697560, 1.000000000000000000),
 ( 1.000000000000000000, 0.4879709628492566731, 1.000000000000000000),
 ( 1.000000000000000000, 0.4561823831825915221, 1.000000000000000000),
 ( 1.000000000000000000, 0.4039565156456190742, 1.000000000000000000),
 ( 1.000000000000000000, 0.3848936348729956602, 1.000000000000000000),
 ( 1.000000000000000000, 0.3826834323650904479, 1.000000000000000000) ) ) 
 REPRESENTATION_ITEM ( '' )  SURFACE ( )  );
#97512 = CARTESIAN_POINT ( 'NONE',  ( 0.1333692844072802142, 2.017199222642913625, -2.468757726274827036 ) ) ;
#97513 = CARTESIAN_POINT ( 'NONE',  ( 3.215925951850879816, -0.9189154559356220719, -1.629173103855706906 ) ) ;
#97514 = CARTESIAN_POINT ( 'NONE',  ( 0.7499999999999885647, 0.8479166673494853423, -1.299038105676652899 ) ) ;
#97515 = APPLICATION_CONTEXT ( 'automotive_design' ) ;
#97516 = CARTESIAN_POINT ( 'NONE',  ( -6.938021921891187382, 9.117444880338284818, -1.599625672291263179 ) ) ;
#97518 = CARTESIAN_POINT ( 'NONE',  ( 5.202788454032899246, 1.956619031766251737, 0.8093448757829673212 ) ) ;
#97517 = CARTESIAN_POINT ( 'NONE',  ( -5.111060722671894929, 5.065251719313053513, 0.000000000000000000 ) ) ;
#97519 = CARTESIAN_POINT ( 'NONE',  ( -0.6823417656250003738, 8.463541667008064096, 1.181850606188754593 ) ) ;
#97521 = CARTESIAN_POINT ( 'NONE',  ( -7.095713291905736853, 9.371694488680407886, 1.599625672291269396 ) ) ;
#97520 = CARTESIAN_POINT ( 'NONE',  ( 2.489882245090881963, -2.085347646507927699, -0.1508444384941027561 ) ) ;
#97523 = VERTEX_POINT ( 'NONE', #97784 ) ;
#97522 = CARTESIAN_POINT ( 'NONE',  ( 1.324769809204975557, -0.04781147349866912699, 1.724288685672677568 ) ) ;
#97524 = CARTESIAN_POINT ( 'NONE',  ( 5.666418135507635512, 8.698239360479199433, 1.199719254218462483 ) ) ;
#97525 = CARTESIAN_POINT ( 'NONE',  ( -1.022621712794113735, 13.26710252192129502, 1.066516380167074507 ) ) ;
#97526 = CARTESIAN_POINT ( 'NONE',  ( 0.005636796283160772081, -9.933099634201859374, 9.579656484007951889 ) ) ;
#97527 = CARTESIAN_POINT ( 'NONE',  ( 6.764644832403535979, -7.632775601084324180, -6.764644832400978025 ) ) ;
#97529 = CARTESIAN_POINT ( 'NONE',  ( 8.337901282279995385, 11.71100668175994386, -1.082531754730543083 ) ) ;
#97528 = CARTESIAN_POINT ( 'NONE',  ( 7.305145839664861640, 7.417091655897478653, 0.7998128361456341429 ) ) ;
#97530 = EDGE_LOOP ( 'NONE', ( #110265, #212988, #178534, #79228 ) ) ;
#97531 = CARTESIAN_POINT ( 'NONE',  ( -1.886017674307096437, 3.298060805577381238, 0.4014564593430944850 ) ) ;
#97533 = CARTESIAN_POINT ( 'NONE',  ( 2.121461778293322276, -0.3959642608444019496, 1.767488790605805438 ) ) ;
#97532 = CARTESIAN_POINT ( 'NONE',  ( 4.746236293235721604, 7.694970221153795364, 1.199719254218451159 ) ) ;
#97534 = CARTESIAN_POINT ( 'NONE',  ( -7.555971681517696936, 7.709721804725773175, 0.7998128361456462443 ) ) ;
#97535 = CARTESIAN_POINT ( 'NONE',  ( 3.344057444064992168, 7.053150784717805877, 1.040834085586084257E-14 ) ) ;
#97536 = CARTESIAN_POINT ( 'NONE',  ( 4.850785098639300408, 8.881276058379668825, -0.7998128361456481317 ) ) ;
#97537 = CARTESIAN_POINT ( 'NONE',  ( 6.639320575229278099, 1.279659970127836388, 2.012538313910294807 ) ) ;
#97538 = CARTESIAN_POINT ( 'NONE',  ( 4.047743032765107607, 7.529339606631276105, 0.4638284745723305624 ) ) ;
#97539 = CARTESIAN_POINT ( 'NONE',  ( 9.408995418203971894, 11.03987807840189816, 1.082531754730549967 ) ) ;
#97540 = ORIENTED_EDGE ( 'NONE', *, *, #153308, .F. ) ;
#97541 = CARTESIAN_POINT ( 'NONE',  ( 3.174093412877276865, -0.9148440431442562693, -1.620569831483926082 ) ) ;
#97542 = CARTESIAN_POINT ( 'NONE',  ( 0.6849900193761117029, 1.566649212177973149, 1.102054418794357948 ) ) ;
#97543 = CARTESIAN_POINT ( 'NONE',  ( 6.528350403681292491, 1.108413491673976736, -1.575378176345716419 ) ) ;
#97544 = CARTESIAN_POINT ( 'NONE',  ( 1.355148357678327420, 3.769637942705310163, 0.6430964159811484171 ) ) ;
#97545 = SURFACE_SIDE_STYLE ('',( #199257 ) ) ;
#97546 = VECTOR ( 'NONE', #186694, 1000.000000000000000 ) ;
#97547 = CARTESIAN_POINT ( 'NONE',  ( 4.684024595049480766, 8.263433789595206136, 0.5754648794667740486 ) ) ;
#97548 = CARTESIAN_POINT ( 'NONE',  ( -11.55950211276791428, 11.37999999999998302, 3.221476510067114329 ) ) ;
#97549 = CARTESIAN_POINT ( 'NONE',  ( -3.633221978782304351, 4.301475732409860697, -1.082531754730549967 ) ) ;
#97550 = CARTESIAN_POINT ( 'NONE',  ( 8.188761592974039161, 10.57664116326830595, -1.443375672974063439 ) ) ;
#97551 = CARTESIAN_POINT ( 'NONE',  ( 5.084792200464717915, 1.883391756629303471, 0.5756752826196751549 ) ) ;
#97552 = CARTESIAN_POINT ( 'NONE',  ( 1.489100733002651333, -2.014586327357254181, -0.6619970261998938676 ) ) ;
#97553 = CARTESIAN_POINT ( 'NONE',  ( -4.381256195510448315, 8.263215994737505454, 1.040834085586084257E-14 ) ) ;
#97554 = CARTESIAN_POINT ( 'NONE',  ( -11.94105721839855327, 10.07301656658874833, -1.187919402540362768 ) ) ;
#97555 = DIRECTION ( 'NONE',  ( -4.440892098500624683E-16, 6.661338147750949103E-16, -1.000000000000000000 ) ) ;
#97556 = CARTESIAN_POINT ( 'NONE',  ( 6.210891007176935652, -0.2719346519345893776, 2.174439262769362280 ) ) ;
#97557 = CARTESIAN_POINT ( 'NONE',  ( 5.052517032109132167, 6.451495319389863425, 1.297790489534809355 ) ) ;
#97558 = CARTESIAN_POINT ( 'NONE',  ( 4.682597122082689189, -1.868462817326870473, -0.4683620393717678465 ) ) ;
#97559 = CARTESIAN_POINT ( 'NONE',  ( -7.705111371268023923, 7.883718109434487253, 1.040834085586084257E-14 ) ) ;
#97560 = LINE ( 'NONE', #131170, #193594 ) ;
#97561 = CARTESIAN_POINT ( 'NONE',  ( 0.6630615684519860498, -1.595754342771567025, 1.524677653706180802 ) ) ;
#97562 = EDGE_CURVE ( 'NONE', #194213, #29472, #60996, .T. ) ;
#97563 = CARTESIAN_POINT ( 'NONE',  ( -0.4000000000000243916, 2.999999999999999112, 2.420000000000000373 ) ) ;
#97564 = CARTESIAN_POINT ( 'NONE',  ( 0.2461629937395051204, 0.9812432698282257393, -1.641294572782559413 ) ) ;
#97565 = EDGE_LOOP ( 'NONE', ( #61099, #122273, #40939, #39123 ) ) ;
#97566 = CARTESIAN_POINT ( 'NONE',  ( 3.119784744920330422, 6.653849612466795627, 0.7216878364870257245 ) ) ;
#97567 = ORIENTED_EDGE ( 'NONE', *, *, #37467, .F. ) ;
#97568 = CARTESIAN_POINT ( 'NONE',  ( 6.350452388456855779, -1.959648489363738699, -0.1964464578135850514 ) ) ;
#97569 = CARTESIAN_POINT ( 'NONE',  ( 1.364679817366498904, 0.1413127912619481230, -1.936958241114185020 ) ) ;
#97570 = CARTESIAN_POINT ( 'NONE',  ( 6.573571087534610058, 1.710132712828818402, -1.535791079811721360 ) ) ;
#97572 = CARTESIAN_POINT ( 'NONE',  ( 5.295690652966449363, -1.314428334581790203, -1.317609258728233756 ) ) ;
#97571 = CARTESIAN_POINT ( 'NONE',  ( -7.293360289508603600, 7.473618190706972086, 0.000000000000000000 ) ) ;
#97573 = CARTESIAN_POINT ( 'NONE',  ( 6.387826650694035990, 7.481494509678370264, -1.199719254218452047 ) ) ;
#97574 = CARTESIAN_POINT ( 'NONE',  ( -4.889337272013151825, 4.909234758358784312, -0.4031905389056227307 ) ) ;
#97575 = CARTESIAN_POINT ( 'NONE',  ( -5.585069213825653023, 8.603332285183535433, -1.199719254218440723 ) ) ;
#97576 = CARTESIAN_POINT ( 'NONE',  ( -6.912678218121246942, 9.158153569265168770, 1.599625672291269396 ) ) ;
#97577 = CARTESIAN_POINT ( 'NONE',  ( 1.118978350340808614, -0.04878210919301298465, 2.191179638975069732 ) ) ;
#97578 = CARTESIAN_POINT ( 'NONE',  ( 5.070386261830877928, 5.978167395966564435, -1.082531754730548412 ) ) ;
#97579 = CARTESIAN_POINT ( 'NONE',  ( 10.99740610014205267, -6.654245765634905219, -0.2680151545361366128 ) ) ;
#97580 = CARTESIAN_POINT ( 'NONE',  ( 1.734723475976807094E-15, -3.469446951953614189E-15, 0.9487424039605132364 ) ) ;
#97582 = EDGE_CURVE ( 'NONE', #42744, #211199, #112767, .T. ) ;
#97581 = CARTESIAN_POINT ( 'NONE',  ( 1.646812808029130215, -1.543121136568927243, 0.9753659028155501343 ) ) ;
#97583 = CARTESIAN_POINT ( 'NONE',  ( -2.785310492603665367, 5.336947110424484109, 1.199719254218462483 ) ) ;
#97584 = CARTESIAN_POINT ( 'NONE',  ( -0.2066541192881463374, 3.358188146985714884, -2.068744351199750753 ) ) ;
#97585 = CARTESIAN_POINT ( 'NONE',  ( -1.999999999999988232, 0.1960773996332039470, 0.6000000000000017542 ) ) ;
#97586 = CARTESIAN_POINT ( 'NONE',  ( 10.55232363013785246, 11.20546574478267132, 0.000000000000000000 ) ) ;
#97587 = CARTESIAN_POINT ( 'NONE',  ( 0.1000542341482368452, -1.926035175483146400, -0.04890095678477742597 ) ) ;
#97588 = CARTESIAN_POINT ( 'NONE',  ( 4.241029431094700541, -0.1880360549168894613, -1.952691919460777026 ) ) ;
#97589 = CARTESIAN_POINT ( 'NONE',  ( -6.692921386640485082, 10.96015871772258521, -0.7998128361456291469 ) ) ;
#97590 = CARTESIAN_POINT ( 'NONE',  ( 6.419949431270806528, 7.448694743692793274, 1.199719254218462483 ) ) ;
#97591 = CARTESIAN_POINT ( 'NONE',  ( 3.843468145482428877, 0.7371271433744167600, -2.064019554291535830 ) ) ;
#97592 = CARTESIAN_POINT ( 'NONE',  ( -0.4019237886467001974, 9.832585450998172050, 1.500000000000001998 ) ) ;
#97593 = CARTESIAN_POINT ( 'NONE',  ( 3.643477671580112709, 1.873648065284461817, -0.8808079623299628347 ) ) ;
#97595 = CARTESIAN_POINT ( 'NONE',  ( -1.402160292154681736E-14, 1.259375000341419248, -1.575800808251659024 ) ) ;
#97594 = PRESENTATION_STYLE_ASSIGNMENT (( #80255 ) ) ;
#97596 = ORIENTED_EDGE ( 'NONE', *, *, #163875, .T. ) ;
#97597 = CARTESIAN_POINT ( 'NONE',  ( 4.184446765594143081, 1.846410498051667348, 1.369081834291352218 ) ) ;
#97598 = CARTESIAN_POINT ( 'NONE',  ( 7.212574532790092974, 9.437756259720353924, -1.443375672974057666 ) ) ;
#97600 = CARTESIAN_POINT ( 'NONE',  ( -3.285556943750000070, -0.4593749995220435256, 0.000000000000000000 ) ) ;
#97599 = CARTESIAN_POINT ( 'NONE',  ( 5.207740401424913124, 9.089797878388800711, -0.7216878364870458196 ) ) ;
#97602 = ADVANCED_FACE ( 'NONE', ( #146548 ), #46905, .T. ) ;
#97601 = CARTESIAN_POINT ( 'NONE',  ( -1.500000000000008216, 8.281250000682797818, 3.469446951953614189E-15 ) ) ;
#97603 = LINE ( 'NONE', #12057, #47473 ) ;
#97604 = CARTESIAN_POINT ( 'NONE',  ( 3.468632250064273670, 0.04687378517908299957, -1.941542025766171298 ) ) ;
#97605 = VERTEX_POINT ( 'NONE', #147592 ) ;
#97606 = CARTESIAN_POINT ( 'NONE',  ( 9.449669878600614581, 12.04770082983265844, -1.443375672974058777 ) ) ;
#97607 = EDGE_CURVE ( 'NONE', #159704, #126491, #150434, .T. ) ;
#97608 = CARTESIAN_POINT ( 'NONE',  ( 4.377155534175989793, -1.710687068321177007, -0.8549628122409487219 ) ) ;
#97609 = FACE_OUTER_BOUND ( 'NONE', #149725, .T. ) ;
#97610 = CARTESIAN_POINT ( 'NONE',  ( 5.086778385480665854, -0.2138867007538784171, -1.711364050844576434 ) ) ;
#97611 = CARTESIAN_POINT ( 'NONE',  ( 4.909388789075159742, -1.913262893431907141, 0.6371506334161003426 ) ) ;
#97612 = CARTESIAN_POINT ( 'NONE',  ( 4.957821946367388932, -2.163970343481158132, -0.7757635736431248707 ) ) ;
#97613 = CARTESIAN_POINT ( 'NONE',  ( 0.7500000000000006661, 11.16666666666666430, -1.299038105676657340 ) ) ;
#97614 = CARTESIAN_POINT ( 'NONE',  ( 1.014635385311330795, -0.9952708415592588231, -1.969785480804244315 ) ) ;
#97616 = CARTESIAN_POINT ( 'NONE',  ( -5.180624094197616714, 5.216685329418210948, 0.7216878364870257245 ) ) ;
#97615 = CARTESIAN_POINT ( 'NONE',  ( -3.838459892414017194, 7.492294413340791159, -0.004696343102253854214 ) ) ;
#97617 = CARTESIAN_POINT ( 'NONE',  ( 6.063686852112752490, 1.743171776219472280, -0.3043750889455443254 ) ) ;
#97619 = CARTESIAN_POINT ( 'NONE',  ( 1.816774867096879964, 2.139948438195220071, 0.8220829075690959664 ) ) ;
#97618 = CARTESIAN_POINT ( 'NONE',  ( 4.376249722160992839, 8.327651452488305850, 0.000000000000000000 ) ) ;
#97620 = CARTESIAN_POINT ( 'NONE',  ( 0.9018503542332901857, 1.320273433284512521, -1.133937880871397796 ) ) ;
#97621 = DIRECTION ( 'NONE',  ( -7.387867266669436732E-31, -1.000000000000000000, 8.546850786086437571E-32 ) ) ;
#97622 = CARTESIAN_POINT ( 'NONE',  ( 1.229404279783296694, -1.564619330878062931, -0.7474530596254543857 ) ) ;
#97623 = CARTESIAN_POINT ( 'NONE',  ( -5.558564015327489343E-14, 0.6093750003414449834, -1.570758158831798257 ) ) ;
#97624 = CARTESIAN_POINT ( 'NONE',  ( -11.96209379583854293, 13.82792940594236519, -0.9572398070798617820 ) ) ;
#97625 = CARTESIAN_POINT ( 'NONE',  ( 0.9069515603133030401, 0.6301693757862131262, 2.077734764916533639 ) ) ;
#97626 = CARTESIAN_POINT ( 'NONE',  ( 2.132046339962359038, 2.016188815772378629, 0.04465230659478347519 ) ) ;
#97627 = AXIS2_PLACEMENT_3D ( 'NONE', #54194, #87758, #199351 ) ;
#97628 = CARTESIAN_POINT ( 'NONE',  ( -0.7500000000000006661, 0.6395833340161540814, -1.299038105676652011 ) ) ;
#97629 = CARTESIAN_POINT ( 'NONE',  ( 5.566998737003931552, -1.742544991934717125, -0.8218319283359241112 ) ) ;
#97630 = CARTESIAN_POINT ( 'NONE',  ( -0.6823417656250039265, 13.06770833367473017, -1.181850606188755259 ) ) ;
#97631 = CARTESIAN_POINT ( 'NONE',  ( 2.760263405638745393, 0.7954514732361592788, -2.074294698012415505 ) ) ;
#97632 = VERTEX_POINT ( 'NONE', #47979 ) ;
#97634 = AXIS2_PLACEMENT_3D ( 'NONE', #160583, #108702, #127108 ) ;
#97633 = CARTESIAN_POINT ( 'NONE',  ( 6.381095703207959602, -8.200000000000001066, 7.037870247915979149 ) ) ;
#97635 = CARTESIAN_POINT ( 'NONE',  ( 8.055515824813896941, 12.54985222892493368, 0.7998128361456462443 ) ) ;
#97636 = CARTESIAN_POINT ( 'NONE',  ( 8.136301581532414673, 8.664975731308866003, 0.000000000000000000 ) ) ;
#97637 = CARTESIAN_POINT ( 'NONE',  ( -10.50000000000000355, 10.09281572507203606, 3.599999999999998312 ) ) ;
#97638 = CARTESIAN_POINT ( 'NONE',  ( 5.794438198198100132, 1.417746085458403638, -1.009241466377588603 ) ) ;
#97639 = CARTESIAN_POINT ( 'NONE',  ( 3.051168888765115828, 1.684027830550902882, -1.006202029777767848 ) ) ;
#97641 = CARTESIAN_POINT ( 'NONE',  ( -7.375272376154101472, 7.706831981708990753, -0.7216878364870278340 ) ) ;
#97640 = CARTESIAN_POINT ( 'NONE',  ( 3.499976210622149253, 7.235056012367825140, 0.7998128361456321445 ) ) ;
#97642 = CARTESIAN_POINT ( 'NONE',  ( 5.741471521233657782, 5.663081294386209663, 0.3692415420062719611 ) ) ;
#97643 = CARTESIAN_POINT ( 'NONE',  ( 4.815850035042070765, -2.220064692501269477, 0.4349022163744782343 ) ) ;
#97644 = CARTESIAN_POINT ( 'NONE',  ( 1.311062339077714078, -1.627386490012251663, 1.267307609633941956 ) ) ;
#97645 = CARTESIAN_POINT ( 'NONE',  ( -5.696397096036042385, 9.797547045350714967, -0.7998128361456231517 ) ) ;
#97646 = CARTESIAN_POINT ( 'NONE',  ( 1.956323303678444425, 2.256377666735286169, -0.1672192238599319314 ) ) ;
#97647 = ORIENTED_EDGE ( 'NONE', *, *, #71255, .T. ) ;
#97648 = CARTESIAN_POINT ( 'NONE',  ( -0.7500000000000006661, 0.6395833340161540814, -1.299038105676652011 ) ) ;
#97649 = CARTESIAN_POINT ( 'NONE',  ( 2.002991962376502233, 1.552455721610061179, 1.043161660468715279 ) ) ;
#97650 = CARTESIAN_POINT ( 'NONE',  ( 1.476802972400652170, -1.725769044224190196, -0.1698483453264828802 ) ) ;
#97651 = CARTESIAN_POINT ( 'NONE',  ( 5.864808805604324604, 0.1626094438406736342, -2.185560445749204828 ) ) ;
#97652 = CARTESIAN_POINT ( 'NONE',  ( 6.756845507909216231, -1.789895876690169585, 1.456048205946461005 ) ) ;
#97653 = CARTESIAN_POINT ( 'NONE',  ( 4.153314892778156242, -1.795761387672462961, -1.203114871582221079 ) ) ;
#97654 = CARTESIAN_POINT ( 'NONE',  ( 4.663973314478016441, -1.267186161278991419, 1.471619509450792229 ) ) ;
#97655 = CARTESIAN_POINT ( 'NONE',  ( -2.616360457312984167, 5.996244933599686355, -0.7216878364870257245 ) ) ;
#97657 = ORIENTED_EDGE ( 'NONE', *, *, #198303, .T. ) ;
#97656 = CARTESIAN_POINT ( 'NONE',  ( 6.661405586796749212, 0.3194099797865917467, -1.842918054787326065 ) ) ;
#97658 = CARTESIAN_POINT ( 'NONE',  ( 2.093750000000001332, -1.895863743164132531, -0.7852924748298759638 ) ) ;
#97659 = CARTESIAN_POINT ( 'NONE',  ( 3.997610708356745146, 7.599328567695712522, -0.1184163795967980992 ) ) ;
#97660 = DIRECTION ( 'NONE',  ( 1.000000000000000000, 0.000000000000000000, 0.000000000000000000 ) ) ;
#97661 = CARTESIAN_POINT ( 'NONE',  ( 3.933273961740298752, 5.682181936820735579, 1.443375672974058777 ) ) ;
#97662 = CARTESIAN_POINT ( 'NONE',  ( 1.360316468750000896, 2.515625000341401130, -3.469446951953614189E-15 ) ) ;
#97663 = CARTESIAN_POINT ( 'NONE',  ( 6.188124994278807023, 1.678003296889327034, 1.117835524071027598 ) ) ;
#97664 = CARTESIAN_POINT ( 'NONE',  ( -3.348500752450953577, 4.929670182657964084, 1.443375672974062551 ) ) ;
#97665 = CARTESIAN_POINT ( 'NONE',  ( 7.904567251967224095, 9.180748867838630645, 1.199719254218462483 ) ) ;
#97666 = CARTESIAN_POINT ( 'NONE',  ( 2.891631901464575272, 6.595597328342462262, 0.000000000000000000 ) ) ;
#97668 =( NAMED_UNIT ( * ) SI_UNIT ( $, .STERADIAN. ) SOLID_ANGLE_UNIT ( ) );
#97667 = CARTESIAN_POINT ( 'NONE',  ( 3.334410585898534674, 1.781380905032422746, 0.3990451814587444024 ) ) ;
#97669 = DIRECTION ( 'NONE',  ( -5.578564026256490882E-16, -1.000000000000000000, -9.066213480720158442E-32 ) ) ;
#97670 = ORIENTED_EDGE ( 'NONE', *, *, #8812, .F. ) ;
#97671 = CARTESIAN_POINT ( 'NONE',  ( -3.973948422136970748, 6.690004688251493192, -1.082531754730546636 ) ) ;
#97672 = CARTESIAN_POINT ( 'NONE',  ( 4.161989969715272686, 4.726297878971393196, 2.420000000000010587 ) ) ;
#97673 = CARTESIAN_POINT ( 'NONE',  ( -9.053093885623068715, 11.58502883802551153, -1.599625672291263179 ) ) ;
#97674 = CARTESIAN_POINT ( 'NONE',  ( 0.2463608477257169804, 1.034524919618844407, -1.734561685378380957 ) ) ;
#97675 = CARTESIAN_POINT ( 'NONE',  ( 1.137531110418067204, -0.04838959064331486287, 2.120096749846810624 ) ) ;
#97676 = EDGE_LOOP ( 'NONE', ( #100437, #17831, #75413, #104179 ) ) ;
#97677 = CARTESIAN_POINT ( 'NONE',  ( -6.608673532018475960, 6.674816973635147477, -0.7998128361456362523 ) ) ;
#97678 = CARTESIAN_POINT ( 'NONE',  ( 3.167801447087334576, 6.847518788243868393, -0.7998128361456291469 ) ) ;
#97679 = CARTESIAN_POINT ( 'NONE',  ( 6.368051766976638994, 1.057089778920755840, 1.768976859881221442 ) ) ;
#97680 = CARTESIAN_POINT ( 'NONE',  ( 6.416638760586134360, -1.319225726833603840, -1.525046029381103452 ) ) ;
#97681 = ORIENTED_EDGE ( 'NONE', *, *, #114638, .F. ) ;
#97682 = ORIENTED_EDGE ( 'NONE', *, *, #25088, .T. ) ;
#97683 = CARTESIAN_POINT ( 'NONE',  ( -8.136864746495904299, 12.64475930422059768, -0.7998128361456281477 ) ) ;
#97685 = EDGE_CURVE ( 'NONE', #149147, #40830, #31710, .T. ) ;
#97684 = CARTESIAN_POINT ( 'NONE',  ( 3.475000000000000533, -1.152083332377417335, -2.006292185433951047 ) ) ;
#97688 = ORIENTED_EDGE ( 'NONE', *, *, #101820, .T. ) ;
#97687 = CARTESIAN_POINT ( 'NONE',  ( -1.580000000000022276, 8.674529973577531194, 2.500000000000011102 ) ) ;
#97686 = CARTESIAN_POINT ( 'NONE',  ( -4.142898457427624415, 6.991076079377632091, 1.199719254218452935 ) ) ;
#97689 = CARTESIAN_POINT ( 'NONE',  ( 6.231590709102786008, 7.018523052454695765, 1.002697108273574500 ) ) ;
#97690 = CARTESIAN_POINT ( 'NONE',  ( 5.694685421800770087, -1.276849089899323886, -1.560260200769040706 ) ) ;
#97691 = CARTESIAN_POINT ( 'NONE',  ( 5.138538782746885580, -1.577291412575715812, 0.9494700402261007088 ) ) ;
#97692 = CARTESIAN_POINT ( 'NONE',  ( 2.973738742942335200, 6.527870343122186725, 0.4765911511174560911 ) ) ;
#97693 = CARTESIAN_POINT ( 'NONE',  ( 2.895503172138352177, 1.978892393434032559, -1.186989842046539234 ) ) ;
#97694 = CARTESIAN_POINT ( 'NONE',  ( 5.342795052237045539, 8.390955439988655229, -1.199719254218450271 ) ) ;
#97695 = CARTESIAN_POINT ( 'NONE',  ( 6.046190728430958394, 2.158797838069245412, 0.1127497994189360364 ) ) ;
#97696 = CARTESIAN_POINT ( 'NONE',  ( 7.983053520348166288, 8.207983950027992748, -0.7998128361456281477 ) ) ;
#97697 = CARTESIAN_POINT ( 'NONE',  ( 1.065847985493496797, -1.230715344637549391, 1.502334450403658206 ) ) ;
#97698 = CARTESIAN_POINT ( 'NONE',  ( -3.436101866059630527, 6.096203712789787232, 1.199719254218462483 ) ) ;
#97699 = ORIENTED_EDGE ( 'NONE', *, *, #209026, .T. ) ;
#97700 = CARTESIAN_POINT ( 'NONE',  ( 4.411641467711771014, 0.6073606466481770161, 2.216650271500276492 ) ) ;
#97701 = FACE_OUTER_BOUND ( 'NONE', #90780, .T. ) ;
#97702 = CARTESIAN_POINT ( 'NONE',  ( -5.503684012504701961, 5.385662534202396934, 0.000000000000000000 ) ) ;
#97703 = AXIS2_PLACEMENT_3D ( 'NONE', #49726, #77964, #33476 ) ;
#97704 = CARTESIAN_POINT ( 'NONE',  ( 4.891396039733495016, 1.386484060982313249, 1.255958711209571810 ) ) ;
#97705 = AXIS2_PLACEMENT_3D ( 'NONE', #160636, #157454, #12237 ) ;
#97708 = CARTESIAN_POINT ( 'NONE',  ( -5.641074431737709283, 8.738948049406083385, -1.199719254218452047 ) ) ;
#97707 = CARTESIAN_POINT ( 'NONE',  ( 1.499999999999987121, 0.5770833340161539704, -0.8660254037844253849 ) ) ;
#97706 = CARTESIAN_POINT ( 'NONE',  ( 1.810667312839256304, -0.5133170510521027907, -1.842115474350584980 ) ) ;
#97709 = CARTESIAN_POINT ( 'NONE',  ( 2.983271218942393332, -0.1628219013674602478, -2.200934326520533446 ) ) ;
#97710 = CARTESIAN_POINT ( 'NONE',  ( -1.519204386771931148, 8.761797318405523782, -2.483775294098344411 ) ) ;
#97711 = CARTESIAN_POINT ( 'NONE',  ( 3.216308754939877446, 4.775446185561722956, -1.599625672291262513 ) ) ;
#97712 = CARTESIAN_POINT ( 'NONE',  ( 5.844973620822835336, 7.912498205750389424, 1.443375672974064550 ) ) ;
#97713 = CARTESIAN_POINT ( 'NONE',  ( -3.785751206713858785, 5.439795712631356750, 1.599625672291267398 ) ) ;
#97714 = CARTESIAN_POINT ( 'NONE',  ( -6.089020385868850305, 10.11795786024005572, -0.7216878364870338292 ) ) ;
#97715 = CARTESIAN_POINT ( 'NONE',  ( 1.967984887604894206, 1.010138386605848426, 1.692741100060575210 ) ) ;
#97716 = CARTESIAN_POINT ( 'NONE',  ( 0.6754003219355340093, -2.174137316696134636, -0.7736760779102586083 ) ) ;
#97717 = CARTESIAN_POINT ( 'NONE',  ( 1.680054527999317759, -1.087118939145682583, -1.632918184844594611 ) ) ;
#97718 = CARTESIAN_POINT ( 'NONE',  ( 5.014538805069497229, 0.7844730879308317029, 1.907755517398136647 ) ) ;
#97719 = CARTESIAN_POINT ( 'NONE',  ( 5.192409644353875642, 5.160158794608717514, 1.040834085586084257E-14 ) ) ;
#97720 = CARTESIAN_POINT ( 'NONE',  ( 5.017399365509065845, 8.011327138806002779, -1.199719254218450271 ) ) ;
#97721 = VERTEX_POINT ( 'NONE', #28495 ) ;
#97722 = CARTESIAN_POINT ( 'NONE',  ( 1.364683531249990311, 5.426041667008086655, 0.7879004041258500513 ) ) ;
#97723 = DIRECTION ( 'NONE',  ( 0.000000000000000000, 0.000000000000000000, -1.000000000000000000 ) ) ;
#97724 = CARTESIAN_POINT ( 'NONE',  ( 4.663641652976547647, 4.543262804668490418, 1.214306433183764966E-14 ) ) ;
#97725 = CARTESIAN_POINT ( 'NONE',  ( 0.5675212215028536678, 1.888217155380923939, 1.071465276393630539 ) ) ;
#97727 = CARTESIAN_POINT ( 'NONE',  ( 5.776868925826902590, 1.698781319366513998, -0.7106697882480541573 ) ) ;
#97726 = LINE ( 'NONE', #75318, #83896 ) ;
#97728 = CARTESIAN_POINT ( 'NONE',  ( -0.1000000000000028644, -9.999999999999994671, 0.000000000000000000 ) ) ;
#97729 = CARTESIAN_POINT ( 'NONE',  ( -6.966220764712169000, 6.002124920821316323, -2.500000000000000444 ) ) ;
#97730 = CARTESIAN_POINT ( 'NONE',  ( 1.387741975113141013, -0.8460221195879283895, 1.668388151239764028 ) ) ;
#97731 = CARTESIAN_POINT ( 'NONE',  ( 5.360679719606757487, -1.569739296358707570, 1.486333574453831297 ) ) ;
#97734 = ADVANCED_FACE ( 'NONE', ( #12230 ), #15423, .F. ) ;
#97733 = CARTESIAN_POINT ( 'NONE',  ( -5.732528328060045197, 6.256990841418501148, 1.080875701640615638 ) ) ;
#97732 = AXIS2_PLACEMENT_3D ( 'NONE', #205761, #186309, #21650 ) ;
#97735 = CARTESIAN_POINT ( 'NONE',  ( 0.07735805125222076917, 2.865712030211249761, -2.577262785371988496 ) ) ;
#97736 = CARTESIAN_POINT ( 'NONE',  ( 1.364683531249988757, -0.3656249996585800299, 0.000000000000000000 ) ) ;
#97737 = CARTESIAN_POINT ( 'NONE',  ( 1.875505643822904300, 0.3255412885708880433, -1.884197853084010443 ) ) ;
#97738 = CARTESIAN_POINT ( 'NONE',  ( 2.834531330521594228, 0.2145198750864007742, 1.756709382032408451 ) ) ;
#97739 = CARTESIAN_POINT ( 'NONE',  ( 0.7504700684401002242, 1.884043224930329385, 0.3264296256808990049 ) ) ;
#97741 = CARTESIAN_POINT ( 'NONE',  ( 5.694928174475800908, 1.691819642972839599, 0.8984594094828317612 ) ) ;
#97740 = CARTESIAN_POINT ( 'NONE',  ( 3.183171797643657097, -3.183434840866198545, -1.009552839968071325 ) ) ;
#97742 = CARTESIAN_POINT ( 'NONE',  ( 6.478958751509338754, 1.837172605331442332, 0.7103315708588151534 ) ) ;
#97743 = CARTESIAN_POINT ( 'NONE',  ( 1.499999999999989120, 5.004166666666691299, 0.8660254037844524744 ) ) ;
#97745 = EDGE_CURVE ( 'NONE', #144610, #13289, #43756, .T. ) ;
#97744 = CARTESIAN_POINT ( 'NONE',  ( 0.4926326669930108371, -1.172979896111199904, 1.766458537607276114 ) ) ;
#97746 = CARTESIAN_POINT ( 'NONE',  ( 4.504681594071535677, 1.446009304718363087, -1.186774495104812699 ) ) ;
#97748 = ORIENTED_EDGE ( 'NONE', *, *, #71283, .T. ) ;
#97747 = CARTESIAN_POINT ( 'NONE',  ( 1.013953575274041619, -0.8186894766500467657, -1.631917417583013341 ) ) ;
#97750 = CARTESIAN_POINT ( 'NONE',  ( 6.882015208740354772, 15.51845925587262798, -9.732639244658484401 ) ) ;
#97749 = CARTESIAN_POINT ( 'NONE',  ( 4.196070124731249074, -0.8457972711899945928, 2.038567251995755836 ) ) ;
#97751 = CARTESIAN_POINT ( 'NONE',  ( 1.364683531249988535, 4.967708333674756283, -0.7879004041258300672 ) ) ;
#97752 = CARTESIAN_POINT ( 'NONE',  ( 2.400897505987206415, 0.4495084874868838232, 2.012960725780033489 ) ) ;
#97754 = ADVANCED_FACE ( 'NONE', ( #132436 ), #12638, .T. ) ;
#97753 = CARTESIAN_POINT ( 'NONE',  ( 6.094553744542824170, 7.069066442510145265, 1.199719254218462483 ) ) ;
#97755 = CARTESIAN_POINT ( 'NONE',  ( -7.178152263431422320, 10.46192917639026554, 1.199719254218453823 ) ) ;
#97756 = DIRECTION ( 'NONE',  ( 0.5265943820992835533, 0.4485553919786932076, -0.7221470882502503130 ) ) ;
#97757 = FACE_OUTER_BOUND ( 'NONE', #28476, .T. ) ;
#97758 = CARTESIAN_POINT ( 'NONE',  ( 6.912678218121202534, 9.158153569265168770, 1.599625672291268286 ) ) ;
#97759 = VERTEX_POINT ( 'NONE', #3431 ) ;
#97760 = CARTESIAN_POINT ( 'NONE',  ( 3.719242722441223226, -1.824546119899137731, -0.9785211796824041519 ) ) ;
#97761 = CARTESIAN_POINT ( 'NONE',  ( -1.201851678989727383E-14, 5.587500000000021672, -1.732050807568863648 ) ) ;
#97762 = CARTESIAN_POINT ( 'NONE',  ( 1.282749207608822495, -2.108609127331688260, -0.4749100009155197699 ) ) ;
#97763 = CARTESIAN_POINT ( 'NONE',  ( -5.095330737579740976, 7.839774693193753308, -1.136590250493845877 ) ) ;
#97764 = CARTESIAN_POINT ( 'NONE',  ( 1.840495965525708932, 1.161060486998789942, -1.652382956570614736 ) ) ;
#97765 = LINE ( 'NONE', #132415, #66630 ) ;
#97766 = ORIENTED_EDGE ( 'NONE', *, *, #127956, .T. ) ;
#97768 = CARTESIAN_POINT ( 'NONE',  ( 6.968527767744098433, 9.153035033833367251, 1.443375672974076540 ) ) ;
#97767 = CARTESIAN_POINT ( 'NONE',  ( -3.474999999999998312, -3.120833333333331350, 2.006292185433951047 ) ) ;
#97769 = DIRECTION ( 'NONE',  ( 0.000000000000000000, -1.000000000000000000, 0.000000000000000000 ) ) ;
#97770 = CARTESIAN_POINT ( 'NONE',  ( 0.5500180045474002410, 0.9981291480291035745, 1.752136972055001518 ) ) ;
#97771 = CARTESIAN_POINT ( 'NONE',  ( 4.546525781634036534, -1.759932548463913671, 1.305750774140898685 ) ) ;
#97772 = CARTESIAN_POINT ( 'NONE',  ( -1.500000000000011324, 4.410416667349484676, -0.8660254037844313801 ) ) ;
#97773 = CARTESIAN_POINT ( 'NONE',  ( 3.779479514802902340, 0.2291398179169491789, -1.898525689255560422 ) ) ;
#97774 = CARTESIAN_POINT ( 'NONE',  ( -5.264643720808155791, 5.036505850564608089, 0.000000000000000000 ) ) ;
#97775 = CARTESIAN_POINT ( 'NONE',  ( 5.626270559546810546, 8.547437505237857280, 1.082531754730558626 ) ) ;
#97777 = CARTESIAN_POINT ( 'NONE',  ( 2.109000121467627498, 0.002830143620808495131, 2.016598147190066914 ) ) ;
#97776 = CARTESIAN_POINT ( 'NONE',  ( 0.3999999999999567235, 3.251480759208385862, 0.4649507210924435086 ) ) ;
#97778 = CARTESIAN_POINT ( 'NONE',  ( -1.364683531250010295, 11.94270833367473017, 0.7879004041258445001 ) ) ;
#97780 = CARTESIAN_POINT ( 'NONE',  ( -8.086512275908061653, 8.398962174839683215, 0.000000000000000000 ) ) ;
#97779 = CARTESIAN_POINT ( 'NONE',  ( 0.5215107003284430442, -2.174349661526672417, 0.7262685697029276355 ) ) ;
#97781 = CARTESIAN_POINT ( 'NONE',  ( 4.032037319687285404, 0.9221689259152658913, -1.457338292308225869 ) ) ;
#97782 = CARTESIAN_POINT ( 'NONE',  ( -0.1399997263889663501, 0.2375346743129815030, -2.034463206964792548 ) ) ;
#97783 = CARTESIAN_POINT ( 'NONE',  ( 2.496672843210871129, 6.064535417054653266, -0.7998128361456291469 ) ) ;
#97784 = CARTESIAN_POINT ( 'NONE',  ( 3.621833129746810265, 4.096114899008192367, -2.499999999999995115 ) ) ;
#97785 = CARTESIAN_POINT ( 'NONE',  ( 0.07536363704235825300, -0.001874865094115065866, -2.144269471569634433 ) ) ;
#97787 = AXIS2_PLACEMENT_3D ( 'NONE', #153682, #42083, #57246 ) ;
#97786 = CARTESIAN_POINT ( 'NONE',  ( 0.4618902312403839194, -0.5555351291045197426, 1.994226918997483500 ) ) ;
#97788 = ORIENTED_EDGE ( 'NONE', *, *, #72346, .T. ) ;
#97789 = CARTESIAN_POINT ( 'NONE',  ( 4.969312858920484466, -1.533218896822113653, -0.9643851972171797460 ) ) ;
#97790 = ORIENTED_EDGE ( 'NONE', *, *, #50048, .F. ) ;
#97792 = CARTESIAN_POINT ( 'NONE',  ( 4.908934136599710563, 7.884784371745123366, 1.199719254218451159 ) ) ;
#97791 = COLOUR_RGB ( '', 0.66274510, 0.83137255, 0.94901961) ;
#97793 = CARTESIAN_POINT ( 'NONE',  ( 6.773846765317306229, -7.246166700180828535, -6.773846765317331986 ) ) ;
#97794 = CARTESIAN_POINT ( 'NONE',  ( 6.129554203544218538, -0.2143803907406968412, 1.798669436738309368 ) ) ;
#97795 = CARTESIAN_POINT ( 'NONE',  ( 6.170369307550815030, 8.292126506933040986, 1.443375672974064550 ) ) ;
#97796 = CARTESIAN_POINT ( 'NONE',  ( -11.89321938400731860, 9.837447216393279348, -1.599605898944130189 ) ) ;
#97797 = CARTESIAN_POINT ( 'NONE',  ( 2.660326705311684581, -1.510451929809487170, 1.587989696798755013 ) ) ;
#97798 = VERTEX_POINT ( 'NONE', #102028 ) ;
#97800 = CARTESIAN_POINT ( 'NONE',  ( 8.378048858240820351, 11.86180853700128601, -1.199719254218446718 ) ) ;
#97799 = CARTESIAN_POINT ( 'NONE',  ( 5.986726177563552298, 1.793701560725208699, 0.4957798874403050449 ) ) ;
#97801 = CARTESIAN_POINT ( 'NONE',  ( 3.515159831171112970, -1.768693170575957874, 0.7362056930131228860 ) ) ;
#97802 = CARTESIAN_POINT ( 'NONE',  ( 0.4999999999999900080, 3.950000000000009059, -0.5000000000000160982 ) ) ;
#97803 = DIRECTION ( 'NONE',  ( 1.039099362110107450E-15, 1.000000000000000000, -4.583713267641621330E-32 ) ) ;
#97804 = CARTESIAN_POINT ( 'NONE',  ( 1.364683531249986537, -0.1364583329919154264, 0.7879004041258500513 ) ) ;
#97805 = CARTESIAN_POINT ( 'NONE',  ( 5.097502569058200983, 6.970172302033127210, -1.443375672974051449 ) ) ;
#97806 = CARTESIAN_POINT ( 'NONE',  ( -10.14113571334194930, 10.93367254176152059, -0.7216878364870267237 ) ) ;
#97807 = CARTESIAN_POINT ( 'NONE',  ( 0.5851287433712646369, -0.2658872486876809327, -2.145209338178376335 ) ) ;
#97808 = CARTESIAN_POINT ( 'NONE',  ( -5.798046968499580345, 6.793418213784815585, 1.199719254218452935 ) ) ;
#97809 = CARTESIAN_POINT ( 'NONE',  ( 4.472210567661338843, 6.310941310395290493, 1.599625672291261402 ) ) ;
#97810 = CARTESIAN_POINT ( 'NONE',  ( 1.799542586263824795, -0.6183211656001773582, 1.717807299235304619 ) ) ;
#97811 = CARTESIAN_POINT ( 'NONE',  ( -4.334856428067329404, 6.080418470877079429, -1.599625672291256295 ) ) ;
#97812 = CARTESIAN_POINT ( 'NONE',  ( 3.364083894888194592, 0.8197913233371354469, 1.631220078658943695 ) ) ;
#97813 = EDGE_CURVE ( 'NONE', #53173, #76973, #53614, .T. ) ;
#97814 = CARTESIAN_POINT ( 'NONE',  ( 9.692997807120237397, 13.38204337665774624, -8.150562841249751500 ) ) ;
#97815 = CARTESIAN_POINT ( 'NONE',  ( 2.548957913124219044, 0.2380835140640499836, 1.897471792728817386 ) ) ;
#97816 = ORIENTED_EDGE ( 'NONE', *, *, #127956, .F. ) ;
#97817 = CARTESIAN_POINT ( 'NONE',  ( 2.752355523121536862, -1.964097686037095336, -0.1475717908260633926 ) ) ;
#97818 = EDGE_LOOP ( 'NONE', ( #42022, #57436 ) ) ;
#97819 = CARTESIAN_POINT ( 'NONE',  ( 4.476081132534933893, -1.884639481945263872, -0.4683437986269470277 ) ) ;
#97820 = CARTESIAN_POINT ( 'NONE',  ( -6.129167961829681488, 9.308390501180058507, -1.199719254218452047 ) ) ;
#97822 = CARTESIAN_POINT ( 'NONE',  ( 5.607717026683647354, 1.607092460389969446, 1.383685132418293495 ) ) ;
#97821 = CARTESIAN_POINT ( 'NONE',  ( 7.517069824134078537, 7.734612647770044092, 0.000000000000000000 ) ) ;
#97823 = FACE_OUTER_BOUND ( 'NONE', #102558, .T. ) ;
#97824 = CARTESIAN_POINT ( 'NONE',  ( 2.473184984502617478, -1.664690511387197702, -0.9409074295685518896 ) ) ;
#97825 = CARTESIAN_POINT ( 'NONE',  ( 5.354985324346148268, 6.526937442883553153, -1.333766491515418817 ) ) ;
#97826 = CARTESIAN_POINT ( 'NONE',  ( 6.983263157960370116, 7.052597238847845063, 2.544342084569085838 ) ) ;
#97827 = CARTESIAN_POINT ( 'NONE',  ( 4.740510986633625024, 5.559626234941203116, -1.199719254218450271 ) ) ;
#97828 = CIRCLE ( 'NONE', #94282, 11.09999999999999964 ) ;
#97829 = CARTESIAN_POINT ( 'NONE',  ( 3.791655721365494891, 1.894798488814054327, -0.6802303536831488806 ) ) ;
#97830 = CARTESIAN_POINT ( 'NONE',  ( 0.08044988649997392161, -9.906619926850268598, 9.499659352616927066 ) ) ;
#97831 = CARTESIAN_POINT ( 'NONE',  ( 5.408770660633122063, 1.379882519126625295, -1.195542987486551301 ) ) ;
#97832 = CARTESIAN_POINT ( 'NONE',  ( 0.2739938332866619364, -2.030697503880642518, 0.4024348779970430834 ) ) ;
#97833 = CARTESIAN_POINT ( 'NONE',  ( -7.646435448427427062, 10.90429654226522693, 1.082531754730549967 ) ) ;
#97834 = CARTESIAN_POINT ( 'NONE',  ( -6.533345026022147728, 6.811601368426168257, 0.5105341503897353750 ) ) ;
#97835 = CARTESIAN_POINT ( 'NONE',  ( -0.4000000000000357714, 3.949999999999981526, -0.5000000000000299760 ) ) ;
#97836 = CARTESIAN_POINT ( 'NONE',  ( 5.278141497218024725, -1.038406966791558528, 1.555765341417144842 ) ) ;
#97837 = CARTESIAN_POINT ( 'NONE',  ( 5.615048174354031474, 9.702639970055050966, 0.7998128361456462443 ) ) ;
#97838 = CARTESIAN_POINT ( 'NONE',  ( -5.447678794592645701, 5.250046769979851646, 0.000000000000000000 ) ) ;
#97839 = CARTESIAN_POINT ( 'NONE',  ( 1.364683531249996529, 10.27604166700806765, 0.7879004041258405033 ) ) ;
#97840 = CARTESIAN_POINT ( 'NONE',  ( -5.250031796989778066, 7.148123067953287446, 1.599625672291267398 ) ) ;
#97842 = CARTESIAN_POINT ( 'NONE',  ( -4.217995187182965289, 6.014356699837137832, 1.443375672974065660 ) ) ;
#97841 = CARTESIAN_POINT ( 'NONE',  ( 2.510230996824538430, 6.080353262937265413, 0.000000000000000000 ) ) ;
#97843 = CARTESIAN_POINT ( 'NONE',  ( -5.302647476276252547, 5.359045941843285199, 0.7216878364870257245 ) ) ;
#97844 = AXIS2_PLACEMENT_3D ( 'NONE', #122296, #123364, #186115 ) ;
#97845 = CARTESIAN_POINT ( 'NONE',  ( -6.013204822860843457, 6.974159367214481264, -1.199719254218446718 ) ) ;
#97846 = CIRCLE ( 'NONE', #11382, 9.523431457505067144 ) ;
#97847 = CARTESIAN_POINT ( 'NONE',  ( 0.8134373588399683719, -1.746984811521329339, -1.110588058507409936 ) ) ;
#97848 = CARTESIAN_POINT ( 'NONE',  ( 1.827892122045454260, 0.8069190765337170834, -1.957623834376254646 ) ) ;
#97849 = CARTESIAN_POINT ( 'NONE',  ( 9.511208455186636712, 11.05516360492796935, 1.199719254218453823 ) ) ;
#97850 = CARTESIAN_POINT ( 'NONE',  ( 1.378728738066221871, 4.086408449757453099, -0.5908528300941785494 ) ) ;
#97851 = CARTESIAN_POINT ( 'NONE',  ( 0.8484201349984072937, -1.953920032193863232, -0.2464512992164570593 ) ) ;
#97852 = CARTESIAN_POINT ( 'NONE',  ( 4.247106804623488330, 7.517614509530361033, 0.9983198370346995087 ) ) ;
#97853 = CARTESIAN_POINT ( 'NONE',  ( 5.992340707560163793, 6.093411701682730275, 0.7216878364870317197 ) ) ;
#97855 = DIRECTION ( 'NONE',  ( 6.873509095275333662E-09, -1.000000000000000000, 0.000000000000000000 ) ) ;
#97854 = FACE_OUTER_BOUND ( 'NONE', #99412, .T. ) ;
#97856 = CARTESIAN_POINT ( 'NONE',  ( 2.203457528917366570, -0.4999491416500188579, 2.236933425931705521 ) ) ;
#97858 = EDGE_CURVE ( 'NONE', #71477, #42744, #200565, .T. ) ;
#97857 = CARTESIAN_POINT ( 'NONE',  ( -9.500102690074733403, -7.891095720666440272, 0.004933703209202861852 ) ) ;
#97859 = CARTESIAN_POINT ( 'NONE',  ( 2.302860652515530848, -0.3306829512400177862, -1.883434002855538081 ) ) ;
#97860 = VERTEX_POINT ( 'NONE', #164891 ) ;
#97861 = CARTESIAN_POINT ( 'NONE',  ( 6.927853306458739979, 10.06595070996845642, 1.082531754730558626 ) ) ;
#97862 = EDGE_CURVE ( 'NONE', #171541, #10112, #50676, .T. ) ;
#97863 = CIRCLE ( 'NONE', #122208, 11.99999999999999112 ) ;
#97864 = CARTESIAN_POINT ( 'NONE',  ( 0.8088407350804104334, -0.4930801656862683346, -1.951752914270672212 ) ) ;
#97865 = CARTESIAN_POINT ( 'NONE',  ( 1.340592890135338555, -1.912720961655197893, -0.4351338972534216087 ) ) ;
#97866 = CARTESIAN_POINT ( 'NONE',  ( -8.299562589859897699, 12.83457345481192036, -0.7998128361456281477 ) ) ;
#97867 = CARTESIAN_POINT ( 'NONE',  ( -6.714312387265696458, 8.856450423275211037, 1.599625672291283607 ) ) ;
#97869 = EDGE_CURVE ( 'NONE', #91680, #6715, #185491, .T. ) ;
#97868 = CARTESIAN_POINT ( 'NONE',  ( -7.724608556409207516, -5.759585062615365736, -7.735357998705601368 ) ) ;
#97871 = CARTESIAN_POINT ( 'NONE',  ( 2.518099203671141595, 1.158133694123581359, -1.338384833553945663 ) ) ;
#97870 = CARTESIAN_POINT ( 'NONE',  ( 3.960945476642624641, 0.2557261242597759776, -2.074860007841982767 ) ) ;
#97872 = SPHERICAL_SURFACE ( 'NONE', #209478, 0.08000000000000000167 ) ;
#97874 = CARTESIAN_POINT ( 'NONE',  ( 5.472717818731657857, -0.05164252020756903566, -2.291847404020570966 ) ) ;
#97873 = DIRECTION ( 'NONE',  ( 0.01240427322300429423, 0.9999230640433337536, 0.000000000000000000 ) ) ;
#97875 = CARTESIAN_POINT ( 'NONE',  ( 4.575936575705426890, -1.688975870839603655, -0.4190883748532001629 ) ) ;
#97876 = AXIS2_PLACEMENT_3D ( 'NONE', #40282, #42434, #90106 ) ;
#97877 = CARTESIAN_POINT ( 'NONE',  ( 8.269583629331492602, 11.73526576994040482, 1.199719254218450271 ) ) ;
#97878 = FACE_OUTER_BOUND ( 'NONE', #196698, .T. ) ;
#97879 = CARTESIAN_POINT ( 'NONE',  ( 3.936634314383654853, 0.9622043370151998065, 1.442083020896669954 ) ) ;
#97880 = CARTESIAN_POINT ( 'NONE',  ( 4.686072593652621521, -1.332121122860012052, -1.714431229949509250 ) ) ;
#97881 = CARTESIAN_POINT ( 'NONE',  ( 3.358669367883368118, 4.941533567329135401, -1.599625672291262513 ) ) ;
#97882 = CARTESIAN_POINT ( 'NONE',  ( 5.735564631760892595, 0.5807582108038509272, -1.931123567068816493 ) ) ;
#97883 = CARTESIAN_POINT ( 'NONE',  ( 0.5624999999999944489, -1.451031289061000207, -1.451031289061098795 ) ) ;
#97884 = CARTESIAN_POINT ( 'NONE',  ( 1.499999999999989120, 3.535416667349488229, 0.8660254037844524744 ) ) ;
#97885 = CARTESIAN_POINT ( 'NONE',  ( 3.082943253306829057, -0.1403151614269258773, -1.921328324580730440 ) ) ;
#97886 = CARTESIAN_POINT ( 'NONE',  ( 1.500000000000001332, 9.656250000682799595, 0.000000000000000000 ) ) ;
#97887 = CARTESIAN_POINT ( 'NONE',  ( 5.713180276867825924, 1.816287534895771216, -1.278698279616990563 ) ) ;
#97888 = EDGE_LOOP ( 'NONE', ( #125324, #181026, #75928, #203661 ) ) ;
#97889 = CARTESIAN_POINT ( 'NONE',  ( 6.883263157960373135, 0.5713788194823016253, 2.097868537683903245 ) ) ;
#97890 = CARTESIAN_POINT ( 'NONE',  ( -1.500000000000011324, 3.670833333333356485, 0.8660254037844403729 ) ) ;
#97891 = CARTESIAN_POINT ( 'NONE',  ( 6.308621549060418054, 6.254479983525607523, 0.7998128361456341429 ) ) ;
#97892 = CARTESIAN_POINT ( 'NONE',  ( 1.243189324034719823, 2.142110494306264101, 0.5876511989056328877 ) ) ;
#97893 = CARTESIAN_POINT ( 'NONE',  ( 10.41509302999109110, 1.813436143228260855, -5.960384690635902594 ) ) ;
#97894 = CARTESIAN_POINT ( 'NONE',  ( 8.297226821883377568, 8.782445501726501291, -0.7216878364870267237 ) ) ;
#97895 = CARTESIAN_POINT ( 'NONE',  ( -2.788906526875773208E-15, 10.21875000068279782, -1.499999999999998446 ) ) ;
#97896 = EDGE_CURVE ( 'NONE', #205873, #156566, #218, .T. ) ;
#97897 = CARTESIAN_POINT ( 'NONE',  ( 6.943184063974162434, 9.193743722760251202, -1.443375672974064550 ) ) ;
#97898 = CARTESIAN_POINT ( 'NONE',  ( 0.1060925565549031974, -0.09613213100253051313, 2.014232862735332308 ) ) ;
#97900 = CARTESIAN_POINT ( 'NONE',  ( 4.844214494511547286, -0.9753611933653669741, 1.817521503207474076 ) ) ;
#97899 = CARTESIAN_POINT ( 'NONE',  ( 10.24048609702354717, 10.84165528948263457, -0.7998128361456281477 ) ) ;
#97901 = CARTESIAN_POINT ( 'NONE',  ( -3.093231602212184850, 6.760520635889515795, -0.7998128361456281477 ) ) ;
#97902 = CARTESIAN_POINT ( 'NONE',  ( -1.402160292154681736E-14, -0.05312499965857903073, -1.575800808251665908 ) ) ;
#97903 = CARTESIAN_POINT ( 'NONE',  ( 5.606678975738343951, 1.416997745663551633, -1.221222563005261774 ) ) ;
#97904 = CARTESIAN_POINT ( 'NONE',  ( 4.957493672250036454, -1.635265592371325960, -0.5776676170772595542 ) ) ;
#97905 = CARTESIAN_POINT ( 'NONE',  ( 4.933026880143430049, -1.235701381803285148, -1.225916536586797667 ) ) ;
#97906 = CARTESIAN_POINT ( 'NONE',  ( 4.196412238629597447, 4.854568018944682706, -1.199719254218452047 ) ) ;
#97907 = B_SPLINE_CURVE_WITH_KNOTS ( 'NONE', 3,
 ( #107211, #123495, #90915, #145014 ),
 .UNSPECIFIED., .F., .F.,
 ( 4, 4 ),
 ( 0.000000000000000000, 0.0001589223950334678857 ),
 .UNSPECIFIED. ) ;
#97908 = CARTESIAN_POINT ( 'NONE',  ( 2.121020962670455923, 0.004254578539099414594, 2.292545472008022056 ) ) ;
#97909 = CARTESIAN_POINT ( 'NONE',  ( 1.364683531249988535, 5.217708333674750065, -0.7879004041258300672 ) ) ;
#97910 = CARTESIAN_POINT ( 'NONE',  ( 0.9020086522944226193, 1.395640307904035593, -1.200911154268270664 ) ) ;
#97911 = DIRECTION ( 'NONE',  ( -1.000000000000000000, 7.109522442527899011E-16, 0.000000000000000000 ) ) ;
#97912 = SURFACE_STYLE_FILL_AREA ( #149854 ) ;
#97913 = CARTESIAN_POINT ( 'NONE',  ( 2.133574855335911291, -1.190200692204022470, -1.384352166806518625 ) ) ;
#97914 = CARTESIAN_POINT ( 'NONE',  ( 2.496720397819631732, -1.994071314890283553, 0.2986276487200872354 ) ) ;
#97915 = CARTESIAN_POINT ( 'NONE',  ( 1.306853331985533107, 1.934050699793531836, 1.030479497498619557 ) ) ;
#97916 = CARTESIAN_POINT ( 'NONE',  ( 10.11376083457019526, 13.81646513174396951, -7.343696251440634093 ) ) ;
#97917 = CARTESIAN_POINT ( 'NONE',  ( 4.014754730066903754, 1.490810813664491974, -1.487730979428596223 ) ) ;
#97918 = CARTESIAN_POINT ( 'NONE',  ( -6.042130013184518589, 10.20090211535728031, -0.7998128361456291469 ) ) ;
#97919 =( BOUNDED_CURVE ( )  B_SPLINE_CURVE ( 2, ( #64274, #181206, #44845, #197455, #210507, #61069, #32834 ),
 .UNSPECIFIED., .F., .T. ) 
 B_SPLINE_CURVE_WITH_KNOTS ( ( 3, 2, 2, 3 ),
 ( 0.2125000000000001055, 0.2166666666666668128, 0.2208333333333334925, 0.2250000000000001998 ),
 .UNSPECIFIED. ) 
 CURVE ( )  GEOMETRIC_REPRESENTATION_ITEM ( )  RATIONAL_B_SPLINE_CURVE ( ( 0.9999999999999964473, 0.8660254037844422603, 1.000000000000000000, 0.8660254037844387076, 1.000000000000000000, 0.8660254037844324904, 1.000000000000006217 ) ) 
 REPRESENTATION_ITEM ( '' )  );
#97920 = CARTESIAN_POINT ( 'NONE',  ( 1.715371797147913435, -1.774658612622433296, -1.066089629202723765 ) ) ;
#97921 = CARTESIAN_POINT ( 'NONE',  ( 6.356075086708249167, 6.309842444114747373, -0.7998128361456281477 ) ) ;
#97922 = CARTESIAN_POINT ( 'NONE',  ( 1.360316468750003782, -0.1822916663252708847, -0.7853790794158961308 ) ) ;
#97923 = CARTESIAN_POINT ( 'NONE',  ( 3.317144061745095129, 1.670432841370917298, -1.306055464808851818 ) ) ;
#97924 = CARTESIAN_POINT ( 'NONE',  ( -1.364683531250000748, 1.259375000341421469, 0.000000000000000000 ) ) ;
#97925 = CARTESIAN_POINT ( 'NONE',  ( 6.234959169399230561, 0.1841439077357870380, 1.816378869960999509 ) ) ;
#97926 = VERTEX_POINT ( 'NONE', #165959 ) ;
#97927 = CARTESIAN_POINT ( 'NONE',  ( -5.601453741101424022, 6.564059448486966986, -1.199719254218453823 ) ) ;
#97928 = CARTESIAN_POINT ( 'NONE',  ( 8.615316546479974136, 12.13862083994696839, 1.199719254218450271 ) ) ;
#97929 = CARTESIAN_POINT ( 'NONE',  ( 5.506019780481205217, 9.437790487287811558, 0.000000000000000000 ) ) ;
#97930 = CARTESIAN_POINT ( 'NONE',  ( 0.000000000000000000, -2.843749999044084653, -4.012584370867899430 ) ) ;
#97931 = CARTESIAN_POINT ( 'NONE',  ( -6.368579470117215813, 8.453095353268645695, 1.599625672291283607 ) ) ;
#97932 = CARTESIAN_POINT ( 'NONE',  ( 3.498311158119755682, -0.9917195014866404534, 1.759444004082431068 ) ) ;
#97933 = CARTESIAN_POINT ( 'NONE',  ( 0.6574224672675427206, -1.779203033188281990, -1.126420244723020270 ) ) ;
#97934 = CARTESIAN_POINT ( 'NONE',  ( -5.769876891067536206, 8.889217585290882795, 1.199719254218454489 ) ) ;
#97935 = CARTESIAN_POINT ( 'NONE',  ( 7.553864141108259211, 11.96459193126834464, 1.040834085586084257E-14 ) ) ;
#97936 = CARTESIAN_POINT ( 'NONE',  ( 4.996841193152741667, 0.3155067605547862142, 1.833815385591957448 ) ) ;
#97937 = CARTESIAN_POINT ( 'NONE',  ( 8.320953590485093088, 10.73086516036454618, 1.599625672291281386 ) ) ;
#97938 =( BOUNDED_CURVE ( )  B_SPLINE_CURVE ( 3, ( #95059, #64661, #80919, #32168 ),
 .UNSPECIFIED., .F., .T. ) 
 B_SPLINE_CURVE_WITH_KNOTS ( ( 4, 4 ),
 ( 3.059570999471132424, 3.223614307708552840 ),
 .UNSPECIFIED. ) 
 CURVE ( )  GEOMETRIC_REPRESENTATION_ITEM ( )  RATIONAL_B_SPLINE_CURVE ( ( 1.000000000000000000, 0.9977587396908786932, 0.9977587396908786932, 1.000000000000000000 ) ) 
 REPRESENTATION_ITEM ( '' )  );
#97939 = DIRECTION ( 'NONE',  ( -0.9782075119097819460, 0.1245777785625464124, 0.1661037047500602826 ) ) ;
#97940 = CARTESIAN_POINT ( 'NONE',  ( -8.500599126088349777, 12.86119004717103209, 1.040834085586084257E-14 ) ) ;
#97941 = AXIS2_PLACEMENT_3D ( 'NONE', #138624, #204648, #188418 ) ;
#97942 = CARTESIAN_POINT ( 'NONE',  ( -6.368579470117215813, 8.453095353268645695, 1.599625672291283607 ) ) ;
#97943 = CARTESIAN_POINT ( 'NONE',  ( 0.1808504484964272296, -2.097240537080494516, -0.5235256853268267507 ) ) ;
#97944 = CARTESIAN_POINT ( 'NONE',  ( 3.274625289317079524, -0.3981104328964027994, -1.976669913042613747 ) ) ;
#97945 = AXIS2_PLACEMENT_3D ( 'NONE', #56932, #120949, #7085 ) ;
#97947 = CARTESIAN_POINT ( 'NONE',  ( -5.139172151939493283, 6.684247474441955106, 1.432371535143169394 ) ) ;
#97946 = CARTESIAN_POINT ( 'NONE',  ( -5.798046968499580345, 6.793418213784815585, 1.199719254218452935 ) ) ;
#97948 = CARTESIAN_POINT ( 'NONE',  ( 1.364683531249986537, 0.1552083336747499542, -0.7879004041258309554 ) ) ;
#97949 = CARTESIAN_POINT ( 'NONE',  ( 2.354500945691032410, -0.7452406562851380256, 1.565668601905329638 ) ) ;
#97950 = CARTESIAN_POINT ( 'NONE',  ( 1.147962396684144792, -1.373903031218721926, 1.068100470705938276 ) ) ;
#97952 = CARTESIAN_POINT ( 'NONE',  ( 7.944714827928050838, 9.331550723079971021, 1.082531754730558626 ) ) ;
#97951 = CARTESIAN_POINT ( 'NONE',  ( 6.129535273836777876, -2.175136813519952916, 0.7712226964542520102 ) ) ;
#97953 = CARTESIAN_POINT ( 'NONE',  ( -11.13230441903222534, 5.430351611223322550, 4.009938051813186632 ) ) ;
#97954 = CARTESIAN_POINT ( 'NONE',  ( 2.653650601580277879, 0.5529494111683015412, -1.985115717065755847 ) ) ;
#97955 = CARTESIAN_POINT ( 'NONE',  ( 1.598982282203027516, 0.9961506480390787122, -1.752761228829378126 ) ) ;
#97956 = CARTESIAN_POINT ( 'NONE',  ( 6.825078400183550720, 4.691998341648846882, 2.606919129228836507 ) ) ;
#97957 = CARTESIAN_POINT ( 'NONE',  ( -6.120580001926503755, 6.105374521861167914, -0.7998128361456362523 ) ) ;
#97958 = CARTESIAN_POINT ( 'NONE',  ( 0.6550726410136185063, -1.664185259661060234, -1.056694852926373773 ) ) ;
#97960 = CARTESIAN_POINT ( 'NONE',  ( -7.160114521792834807, 8.486460042580672436, 1.082531754730549078 ) ) ;
#97959 = CARTESIAN_POINT ( 'NONE',  ( 4.570513122935188299, 0.7371126809179430195, 1.764830652192488580 ) ) ;
#97961 = CARTESIAN_POINT ( 'NONE',  ( 5.901041445831936016, 1.806360628843254768, -1.267562117129708232 ) ) ;
#97962 = CARTESIAN_POINT ( 'NONE',  ( -7.566859129758459979, 8.000626204239226880, 0.000000000000000000 ) ) ;
#97963 = CARTESIAN_POINT ( 'NONE',  ( 5.365994935958575240, 9.482354201918870018, 0.7998128361456341429 ) ) ;
#97964 = CARTESIAN_POINT ( 'NONE',  ( -7.781453819600577582, 8.043060642480948985, 0.000000000000000000 ) ) ;
#97965 = CARTESIAN_POINT ( 'NONE',  ( 6.305353446217972113, 1.845220813986702124, -1.044706065825385943 ) ) ;
#97966 = CARTESIAN_POINT ( 'NONE',  ( 0.000000000000000000, 0.000000000000000000, 0.000000000000000000 ) ) ;
#97967 = CARTESIAN_POINT ( 'NONE',  ( 4.999205796216253717, 1.921780780153565793, -1.277121366954391934 ) ) ;
#97968 = CARTESIAN_POINT ( 'NONE',  ( 5.002378505967388200, 1.956489882415031190, 0.1462272935644214900 ) ) ;
#97969 = CARTESIAN_POINT ( 'NONE',  ( 1.428482823135175606, -1.248714028858177283, 1.512975372890807524 ) ) ;
#97970 = CARTESIAN_POINT ( 'NONE',  ( 9.154780037725547714, 11.70366268214508487, 1.599625672291279388 ) ) ;
#97971 = CARTESIAN_POINT ( 'NONE',  ( 0.01820432788856435335, -1.842448466851685840, 0.8197770699841927522 ) ) ;
#97972 = VERTEX_POINT ( 'NONE', #34871 ) ;
#97973 = CARTESIAN_POINT ( 'NONE',  ( -0.2232446489705899595, -0.4745787333681207865, -2.071451665377940010 ) ) ;
#97975 = CARTESIAN_POINT ( 'NONE',  ( -7.049349804101573191, 10.31165964050546258, -1.199719254218440723 ) ) ;
#97974 = CARTESIAN_POINT ( 'NONE',  ( -4.303823697334223652, 7.108545849276850959, -1.199719254218452047 ) ) ;
#97976 = CARTESIAN_POINT ( 'NONE',  ( 1.235996726672627943, 0.3573974351761283752, 1.805938768738392319 ) ) ;
#97977 = ORIENTED_EDGE ( 'NONE', *, *, #61570, .T. ) ;
#97978 = CARTESIAN_POINT ( 'NONE',  ( 4.047858276791187038, 1.568658707867241819, 1.501164901757213288 ) ) ;
#97979 = CARTESIAN_POINT ( 'NONE',  ( 9.528027380766250332, 12.67459186834941320, -7.221597964460605645 ) ) ;
#97980 = CARTESIAN_POINT ( 'NONE',  ( 1.389100911873580646, -2.015333191458138273, -0.6601287711371638389 ) ) ;
#97981 = CARTESIAN_POINT ( 'NONE',  ( -1.500000000000013101, 2.910416667349485120, -0.8660254037844313801 ) ) ;
#97982 = CARTESIAN_POINT ( 'NONE',  ( 9.752392566931574081, 10.27221283770866300, -0.7998128361456281477 ) ) ;
#97983 = CARTESIAN_POINT ( 'NONE',  ( -1.225000000000028066, 0.5000000000000143219, -5.030698080332740574E-14 ) ) ;
#97984 = CARTESIAN_POINT ( 'NONE',  ( 6.590809034589254267, 6.776089313701147532, -0.2235409772415736240 ) ) ;
#97985 = CARTESIAN_POINT ( 'NONE',  ( 1.950533276942335137, 0.6436621796281314367, 1.957774297735858759 ) ) ;
#97987 = CARTESIAN_POINT ( 'NONE',  ( -0.1237769027084348328, -0.1346504581853508187, -1.811164470923332104 ) ) ;
#97986 = CARTESIAN_POINT ( 'NONE',  ( -9.501566725078754772, 9.979582688880366703, -0.7998128361456291469 ) ) ;
#97988 = CARTESIAN_POINT ( 'NONE',  ( -1.364683531250012516, 3.988541667008088876, -0.7879004041258300672 ) ) ;
#97989 = CARTESIAN_POINT ( 'NONE',  ( -1.115562610750309283E-14, 9.312500000000001776, 1.500000000000001554 ) ) ;
#97990 = CARTESIAN_POINT ( 'NONE',  ( 5.671814582574529418, 7.426500967315623036, -1.373566114539000793 ) ) ;
#97991 =( BOUNDED_SURFACE ( )  B_SPLINE_SURFACE ( 3, 3, ( 
 ( #97785, #163846, #76175, #15425, #133502, #115145, #51149, #33822, #34875, #199506 ),
 ( #148655, #37016, #84710, #100949, #182195, #99902, #16488, #3435, #69502, #102031 ),
 ( #167036, #103099, #18631, #1298, #53278, #131389, #201630, #65238, #197385, #66294 ),
 ( #149719, #81515, #2361, #132440, #150797, #183271, #83635, #181142, #198441, #165963 ),
 ( #185399, #82568, #168101, #68437, #117273, #49027, #222, #50086, #134566, #151859 ),
 ( #164894, #147593, #116209, #98844, #200568, #32764, #17548, #119410, #213611, #52214 ),
 ( #118344, #67357, #184328, #135610, #35953, #19700, #85778, #86846, #55411, #152912 ) ),
 .UNSPECIFIED., .T., .F., .T. ) 
 B_SPLINE_SURFACE_WITH_KNOTS ( ( 4, 3, 4 ),
 ( 4, 1, 1, 1, 1, 1, 1, 4 ),
 ( 0.000000000000000000, 0.5000000000000000000, 1.000000000000000000 ),
 ( 0.000000000000000000, 0.09183773654504942541, 0.1838067853904964410, 0.2558923657893393822, 0.3606054339151033017, 0.5206678126786191685, 0.7335446035554463728, 1.000000000000000000 ),
 .UNSPECIFIED. ) 
 GEOMETRIC_REPRESENTATION_ITEM ( )  RATIONAL_B_SPLINE_SURFACE ( (
 ( 1.000000000000000222, 1.000000000000000222, 0.9999999999999997780, 1.000000000000000000, 1.000000000000000222, 0.9999999999999996669, 1.000000000000000222, 1.000000000000000444, 1.000000000000000000, 1.000000000000000000),
 ( 0.3333333333333334259, 0.3333333333333334814, 0.3333333333333333703, 0.3333333333333333703, 0.3333333333333333703, 0.3333333333333332593, 0.3333333333333334814, 0.3333333333333334814, 0.3333333333333333703, 0.3333333333333333703),
 ( 0.3333333333333334259, 0.3333333333333334814, 0.3333333333333333703, 0.3333333333333333703, 0.3333333333333333703, 0.3333333333333332593, 0.3333333333333334814, 0.3333333333333334814, 0.3333333333333333703, 0.3333333333333333703),
 ( 1.000000000000000222, 1.000000000000000222, 0.9999999999999997780, 1.000000000000000000, 1.000000000000000222, 0.9999999999999996669, 1.000000000000000222, 1.000000000000000444, 1.000000000000000000, 1.000000000000000000),
 ( 0.3333333333333334259, 0.3333333333333334814, 0.3333333333333333703, 0.3333333333333333703, 0.3333333333333333703, 0.3333333333333332593, 0.3333333333333334814, 0.3333333333333334814, 0.3333333333333333703, 0.3333333333333333703),
 ( 0.3333333333333334259, 0.3333333333333334814, 0.3333333333333333703, 0.3333333333333333703, 0.3333333333333333703, 0.3333333333333332593, 0.3333333333333334814, 0.3333333333333334814, 0.3333333333333333703, 0.3333333333333333703),
 ( 1.000000000000000222, 1.000000000000000222, 0.9999999999999997780, 1.000000000000000000, 1.000000000000000222, 0.9999999999999996669, 1.000000000000000222, 1.000000000000000444, 1.000000000000000000, 1.000000000000000000) ) ) 
 REPRESENTATION_ITEM ( '' )  SURFACE ( )  );
#97992 = CARTESIAN_POINT ( 'NONE',  ( 11.84100621633422179, 9.989584257766640718, -1.444132586618106728 ) ) ;
#97993 = CARTESIAN_POINT ( 'NONE',  ( 1.880510708721146118, -1.211181421480477693, 1.910737325309288304 ) ) ;
#97994 = CARTESIAN_POINT ( 'NONE',  ( -9.490344339885977476, 11.13478515369756217, -1.082531754730539753 ) ) ;
#97995 = CARTESIAN_POINT ( 'NONE',  ( 1.371055822538247870, -1.554752094505476467, -0.9295159999406394924 ) ) ;
#97996 = CARTESIAN_POINT ( 'NONE',  ( 2.079167605185348044, 1.483516914179264790, 1.212129443301296128 ) ) ;
#97997 = CARTESIAN_POINT ( 'NONE',  ( 2.787621587699981696, -1.932700977737045633, 0.7428295258242522126 ) ) ;
#97998 = CARTESIAN_POINT ( 'NONE',  ( 1.364683531249988535, 1.676041667008085101, 0.7879004041258500513 ) ) ;
#97999 = EDGE_CURVE ( 'NONE', #163825, #145411, #114476, .T. ) ;
#98000 = CARTESIAN_POINT ( 'NONE',  ( 1.674623549722221716, -1.871433754200592992, -0.6201854899473575600 ) ) ;
#98001 = CARTESIAN_POINT ( 'NONE',  ( 5.707627890916790570, -0.4656921374228146226, 1.869253615786143685 ) ) ;
#98003 = CARTESIAN_POINT ( 'NONE',  ( 6.490673131624099312, 6.748652840683030618, -0.08655830178419705867 ) ) ;
#98002 = CARTESIAN_POINT ( 'NONE',  ( 0.9620547613307988133, 0.4452262838200848893, -2.264189643979396482 ) ) ;
#98004 = CARTESIAN_POINT ( 'NONE',  ( -1.364683531250012516, 2.738541667008090208, -0.7879004041258289570 ) ) ;
#98005 = CARTESIAN_POINT ( 'NONE',  ( 5.353991443295786468, -0.7455691153513328562, 1.923382134945450295 ) ) ;
#98006 = AXIS2_PLACEMENT_3D ( 'NONE', #69693, #155244, #23077 ) ;
#98008 = CARTESIAN_POINT ( 'NONE',  ( -6.749261541504576911, 6.768559974710451677, 1.040834085586084257E-14 ) ) ;
#98007 = MECHANICAL_DESIGN_GEOMETRIC_PRESENTATION_REPRESENTATION (  '', ( #163702 ), #149782 ) ;
#98009 = CARTESIAN_POINT ( 'NONE',  ( 6.856673000209174695, 9.022537805042615489, 1.599625672291281386 ) ) ;
#98010 = CARTESIAN_POINT ( 'NONE',  ( 2.535011536075338689, 5.133042487381368701, -0.9999999999999956701 ) ) ;
#98011 = CARTESIAN_POINT ( 'NONE',  ( 0.03009625396771432870, -1.297761387203050232, -1.659265549802463546 ) ) ;
#98012 = CARTESIAN_POINT ( 'NONE',  ( 1.364683531249988757, 2.446875000341415696, 1.214306433183764966E-14 ) ) ;
#98013 = CARTESIAN_POINT ( 'NONE',  ( 4.675171183009182663, 0.005162144975975196948, -2.161773191939574179 ) ) ;
#98014 = CARTESIAN_POINT ( 'NONE',  ( 4.846356044401274765, 1.036295046036241674, -1.733382803446526621 ) ) ;
#98015 = DIRECTION ( 'NONE',  ( -1.000000000000000000, 0.000000000000000000, 0.000000000000000000 ) ) ;
#98016 = CARTESIAN_POINT ( 'NONE',  ( -6.399085315970155285, 6.567947078161039620, -0.7216878364870278340 ) ) ;
#98017 = EDGE_CURVE ( 'NONE', #96449, #116214, #173908, .T. ) ;
#98018 = CIRCLE ( 'NONE', #111987, 0.07999999999999993228 ) ;
#98021 = CARTESIAN_POINT ( 'NONE',  ( 5.558479791922850133, 6.547609847740540445, -1.082531754730542195 ) ) ;
#98020 = CARTESIAN_POINT ( 'NONE',  ( -3.285556943750000070, -1.159374999522042815, 0.000000000000000000 ) ) ;
#98019 = CARTESIAN_POINT ( 'NONE',  ( 5.664274315459256748, 9.830346811336296398, -0.7998128361456481317 ) ) ;
#98022 = CARTESIAN_POINT ( 'NONE',  ( -3.630551273409382329, 7.457669928944732796, 0.7998128361456352531 ) ) ;
#98023 = CARTESIAN_POINT ( 'NONE',  ( 4.153529959351897283, 1.954779968807466295, -0.4946301968136583849 ) ) ;
#98024 = CARTESIAN_POINT ( 'NONE',  ( -8.213542131780492639, 8.476887330032372603, 1.040834085586084257E-14 ) ) ;
#98026 = SURFACE_STYLE_FILL_AREA ( #114324 ) ;
#98025 = CARTESIAN_POINT ( 'NONE',  ( -3.898132859128961236, 4.506575409527250997, -1.199719254218452047 ) ) ;
#98027 = CARTESIAN_POINT ( 'NONE',  ( -0.6823417656250212460, 5.301041667008086655, 1.181850606188767472 ) ) ;
#98029 = CARTESIAN_POINT ( 'NONE',  ( -1.364683531250000748, 8.859375000341396245, 0.000000000000000000 ) ) ;
#98028 = CARTESIAN_POINT ( 'NONE',  ( 4.926735330553584369, 2.067573386176469796, 0.6309256262674377558 ) ) ;
#98030 = SURFACE_STYLE_FILL_AREA ( #180324 ) ;
#98031 = CARTESIAN_POINT ( 'NONE',  ( -11.86531349175653105, 7.722710556319649200, 1.810764415104959779 ) ) ;
#98033 = CARTESIAN_POINT ( 'NONE',  ( 5.026970340808907700, -1.727993218758390404, 1.039010492973009514 ) ) ;
#98032 = CARTESIAN_POINT ( 'NONE',  ( -7.876924059415400414, 9.252461493148505411, 1.082531754730558626 ) ) ;
#98034 = CARTESIAN_POINT ( 'NONE',  ( 0.6823417656249882723, -1.094791666325249713, 1.181850606188755259 ) ) ;
#98035 = AXIS2_PLACEMENT_3D ( 'NONE', #139423, #25640, #175126 ) ;
#98036 = CARTESIAN_POINT ( 'NONE',  ( 0.1172359533097135365, -1.692718506494130359, 0.3305547394890032686 ) ) ;
#98037 = CARTESIAN_POINT ( 'NONE',  ( 3.576318658954677598, 7.394398545414291313, 0.7998128361456281477 ) ) ;
#98039 = CARTESIAN_POINT ( 'NONE',  ( 5.657495238652423097, 9.822437888394988548, 0.000000000000000000 ) ) ;
#98038 = CARTESIAN_POINT ( 'NONE',  ( 7.266807147244743526, 11.42176607185347414, -0.7216878364870267237 ) ) ;
#98040 = CARTESIAN_POINT ( 'NONE',  ( -11.81671913857781853, 8.671847271708829297, 2.110070278039765768 ) ) ;
#98041 = CARTESIAN_POINT ( 'NONE',  ( 6.415307259278708152, -0.2288938695442776505, 1.856442058181500654 ) ) ;
#98042 = CARTESIAN_POINT ( 'NONE',  ( 1.084635982312625924, -1.275300252541565538, 1.557628696486039077 ) ) ;
#98043 = CARTESIAN_POINT ( 'NONE',  ( 3.083271082906696048, -0.1608111237268796401, -2.200959079826501075 ) ) ;
#98044 = CARTESIAN_POINT ( 'NONE',  ( -7.241463443030476732, 7.620997903056574430, 0.000000000000000000 ) ) ;
#98045 = ORIENTED_EDGE ( 'NONE', *, *, #207616, .F. ) ;
#98046 = CARTESIAN_POINT ( 'NONE',  ( 9.869972640624258275, 10.61731562359089587, 0.000000000000000000 ) ) ;
#98048 = CARTESIAN_POINT ( 'NONE',  ( 1.898064762488653079, -0.9530305783747442527, -1.777002450075705120 ) ) ;
#98047 = CARTESIAN_POINT ( 'NONE',  ( 1.805496089173063812, 1.843435535509674317, -1.047849062051921853 ) ) ;
#98050 = ORIENTED_EDGE ( 'NONE', *, *, #58273, .F. ) ;
#98049 = CARTESIAN_POINT ( 'NONE',  ( 2.144508837627901343, 1.757922920557394519, 0.4371675498636724000 ) ) ;
#98051 = CARTESIAN_POINT ( 'NONE',  ( 7.849244587668864348, 8.122149871893999062, 0.7998128361456291469 ) ) ;
#98052 = CARTESIAN_POINT ( 'NONE',  ( 6.986529229743720926, 7.045372277656132276, -0.7998128361456281477 ) ) ;
#98054 = CARTESIAN_POINT ( 'NONE',  ( -0.1708952380198276444, -1.482394133889615828, -1.213259445456981167 ) ) ;
#98053 = CARTESIAN_POINT ( 'NONE',  ( -2.930533758848195447, 6.570706485298192234, -0.7998128361456281477 ) ) ;
#98055 = CARTESIAN_POINT ( 'NONE',  ( 0.000000000000000000, 13.49999999999999822, -1.500000000000000222 ) ) ;
#98056 = CARTESIAN_POINT ( 'NONE',  ( -11.94105721237522921, 12.57259215598210744, -1.187919463087249605 ) ) ;
#98057 = CARTESIAN_POINT ( 'NONE',  ( 5.300874872818828187, 8.167809204055208383, 1.082531754730558626 ) ) ;
#98058 = CARTESIAN_POINT ( 'NONE',  ( 1.364683531249986537, 0.7177083336747527298, -0.7879004041258239610 ) ) ;
#98059 = FACE_OUTER_BOUND ( 'NONE', #157898, .T. ) ;
#98060 = CARTESIAN_POINT ( 'NONE',  ( -9.378489572351046633, 11.96465713920816043, -1.599625672291263179 ) ) ;
#98061 = CARTESIAN_POINT ( 'NONE',  ( 5.577088068215094729, -0.04877400797019536272, -2.161318155665878038 ) ) ;
#98062 = CARTESIAN_POINT ( 'NONE',  ( -5.560252395380252288, 7.580323442733986283, 1.443375672974058777 ) ) ;
#98063 = CARTESIAN_POINT ( 'NONE',  ( 6.211043768836185031, 6.418841616496599123, 0.7216878364870328300 ) ) ;
#98064 = CARTESIAN_POINT ( 'NONE',  ( 2.250376613284802207, 0.9954810856505690309, -1.872389709364124188 ) ) ;
#98065 = CARTESIAN_POINT ( 'NONE',  ( 6.616225513087798049, -0.8637638766970030524, -1.608286988965562214 ) ) ;
#98066 = EDGE_CURVE ( 'NONE', #176773, #205805, #186914, .T. ) ;
#98067 = CARTESIAN_POINT ( 'NONE',  ( 3.093000238167437743, 1.692540756771460764, -1.010471881233595104 ) ) ;
#98068 = CARTESIAN_POINT ( 'NONE',  ( 5.994389040191065554, -1.017321598621454548, 1.619163160827830517 ) ) ;
#98069 = ORIENTED_EDGE ( 'NONE', *, *, #25801, .T. ) ;
#98070 = DIRECTION ( 'NONE',  ( 0.000000000000000000, 0.000000000000000000, 1.000000000000000000 ) ) ;
#98071 = CARTESIAN_POINT ( 'NONE',  ( 0.2212536527127808295, -1.848710500310095872, -0.9322282823912150240 ) ) ;
#98072 = CARTESIAN_POINT ( 'NONE',  ( 1.956878712445113244, 0.3320500349934927820, -1.913199751371328361 ) ) ;
#98073 = VERTEX_POINT ( 'NONE', #69498 ) ;
#98074 = CARTESIAN_POINT ( 'NONE',  ( -4.454990830682073799, 7.094613310480975876, -1.116242305992283690 ) ) ;
#98076 = CARTESIAN_POINT ( 'NONE',  ( 7.364013710877980401, 8.620379413226322285, -1.199719254218452047 ) ) ;
#98075 = CARTESIAN_POINT ( 'NONE',  ( -5.451787166470911217, 9.374519104275787384, 0.7216878364870267237 ) ) ;
#98078 = CARTESIAN_POINT ( 'NONE',  ( 6.446011968293428041, 9.607765498729298415, -1.199719254218440723 ) ) ;
#98077 = CARTESIAN_POINT ( 'NONE',  ( 2.185595087713845697, -0.8928614526015861141, 1.890522631819052002 ) ) ;
#98080 = CARTESIAN_POINT ( 'NONE',  ( 5.248414861821569133, 6.256143772614186638, -1.082531754730548412 ) ) ;
#98079 = CARTESIAN_POINT ( 'NONE',  ( 5.795220594837462436, 8.848508896363995291, -1.199719254218440723 ) ) ;
#98082 = EDGE_LOOP ( 'NONE', ( #37121, #141930, #163949, #44129, #123603 ) ) ;
#98081 = CARTESIAN_POINT ( 'NONE',  ( 5.725241913846256914, 1.688569718951500986, 0.8975008795490189151 ) ) ;
#98083 = CARTESIAN_POINT ( 'NONE',  ( 4.073040751519330094, -2.058760688187323495, -0.7953439701907026871 ) ) ;
#98084 = CARTESIAN_POINT ( 'NONE',  ( 1.887996149947854807, 1.521953097117642706, 1.598203399828190152 ) ) ;
#98085 = PRESENTATION_STYLE_ASSIGNMENT (( #95960 ) ) ;
#98086 = CARTESIAN_POINT ( 'NONE',  ( 0.1000639402851908749, -0.9014739813196898099, 1.686438745833309438 ) ) ;
#98087 = AXIS2_PLACEMENT_3D ( 'NONE', #109714, #70974, #78198 ) ;
#98088 = CARTESIAN_POINT ( 'NONE',  ( -10.59763834280244232, 13.79999999999999716, -3.303285708550594890 ) ) ;
#98089 = CARTESIAN_POINT ( 'NONE',  ( 8.778014389843965759, 12.32843499053828928, 1.199719254218450271 ) ) ;
#98090 = CARTESIAN_POINT ( 'NONE',  ( 3.859880467719906783, -0.6038372105774907350, 1.980330894321411295 ) ) ;
#98091 = COLOUR_RGB ( '', 0.08235294, 0.09019608, 0.10196078) ;
#98093 = CARTESIAN_POINT ( 'NONE',  ( 1.217891636700708435, -2.108894920778502602, 0.4742063263511315796 ) ) ;
#98092 = CARTESIAN_POINT ( 'NONE',  ( -2.428882075142555497, 5.985446187641602300, 1.040834085586084257E-14 ) ) ;
#98094 = CARTESIAN_POINT ( 'NONE',  ( 4.001666433686186686, -2.185622478633037602, 0.1623105178310546570 ) ) ;
#98095 = CARTESIAN_POINT ( 'NONE',  ( 4.911989969715260251, 4.726297878971393196, -7.499999999999991118 ) ) ;
#98096 = DIRECTION ( 'NONE',  ( 0.04267330865764863701, 0.000000000000000000, 0.9990890794760038940 ) ) ;
#98097 = CARTESIAN_POINT ( 'NONE',  ( -0.2718889520038957341, 8.158259021453911686, 2.022062967018402713 ) ) ;
#98098 = CARTESIAN_POINT ( 'NONE',  ( 1.364683531249996529, 14.52604166700806232, 0.7879004041258405033 ) ) ;
#98099 = CARTESIAN_POINT ( 'NONE',  ( -5.666381855868691808, 5.575476684793721383, 0.000000000000000000 ) ) ;
#98100 = UNCERTAINTY_MEASURE_WITH_UNIT (LENGTH_MEASURE( 1.000000000000000082E-05 ), #26746, 'distance_accuracy_value', 'NONE');
#98101 = CARTESIAN_POINT ( 'NONE',  ( 0.3697678102792775756, -0.2496098759999023087, -2.000856779379902139 ) ) ;
#98102 = CIRCLE ( 'NONE', #170742, 0.08000000000000052902 ) ;
#98103 = CARTESIAN_POINT ( 'NONE',  ( -8.676855123066012254, 12.10645282934361866, -1.082531754730543971 ) ) ;
#98104 = CARTESIAN_POINT ( 'NONE',  ( 4.311429529933403337, -1.718370896367764411, -1.154329086688666184 ) ) ;
#98105 = CARTESIAN_POINT ( 'NONE',  ( 6.011343318556897408, -1.993460012771612222, 0.7135861072808927785 ) ) ;
#98106 = CARTESIAN_POINT ( 'NONE',  ( 5.341022448779654930, 8.318611059296550536, 1.199719254218462483 ) ) ;
#98107 = CARTESIAN_POINT ( 'NONE',  ( 1.364683531249990311, 5.613541667008088432, 0.7879004041258499402 ) ) ;
#98108 = CARTESIAN_POINT ( 'NONE',  ( 3.871889627987592064, -1.941038753702705177, 0.3322218420921344562 ) ) ;
#98109 = CARTESIAN_POINT ( 'NONE',  ( 5.824266732648851530, 2.207754452112113075, 0.6165074292824882507 ) ) ;
#98111 = EDGE_CURVE ( 'NONE', #104869, #169854, #9092, .T. ) ;
#98110 = CARTESIAN_POINT ( 'NONE',  ( 3.826616632296374831, 1.734130841282412128, 0.5711148077138239465 ) ) ;
#98112 = CARTESIAN_POINT ( 'NONE',  ( 4.146814880933355596, 5.931313009212638931, 1.599625672291261402 ) ) ;
#98113 = CARTESIAN_POINT ( 'NONE',  ( 5.653386866774156694, 5.697965554099049257, -0.7216878364870207285 ) ) ;
#98114 = CARTESIAN_POINT ( 'NONE',  ( -6.577640801285370209, 7.702944352034914566, -1.199719254218452047 ) ) ;
#98115 = CARTESIAN_POINT ( 'NONE',  ( 5.367048706163317640, 7.354919138647580290, -1.599625672291281386 ) ) ;
#98116 = ORIENTED_EDGE ( 'NONE', *, *, #3121, .F. ) ;
#98117 = CARTESIAN_POINT ( 'NONE',  ( 4.728775500204083215, 1.385159600073909258, -1.461172115097974622 ) ) ;
#98118 = CARTESIAN_POINT ( 'NONE',  ( 6.469376040731918742, -2.253416215261240918, -0.4533134382209720314 ) ) ;
#98119 = CARTESIAN_POINT ( 'NONE',  ( 4.328923052438288899, -1.828919189252835142, -0.7100325158947774495 ) ) ;
#98120 = CARTESIAN_POINT ( 'NONE',  ( -7.854251061018346469, 8.057714414143200443, -0.7998128361456291469 ) ) ;
#98121 = CARTESIAN_POINT ( 'NONE',  ( -5.135841261478327979, 4.886236314679810455, 0.7998128361456341429 ) ) ;
#98123 = EDGE_CURVE ( 'NONE', #85120, #144017, #202225, .T. ) ;
#98122 = DIRECTION ( 'NONE',  ( -1.000000000000000000, 5.421010862427522170E-16, 0.000000000000000000 ) ) ;
#98124 = CARTESIAN_POINT ( 'NONE',  ( -5.798046968499580345, 6.793418213784815585, 1.199719254218452935 ) ) ;
#98126 = CARTESIAN_POINT ( 'NONE',  ( 5.735142062806906083, -1.598577407953686746, 0.7598067823499834450 ) ) ;
#98125 = CARTESIAN_POINT ( 'NONE',  ( 0.7848512634026264534, 1.842159585024247148, -0.9888006619010838438 ) ) ;
#98127 = CARTESIAN_POINT ( 'NONE',  ( 10.99970480893081692, -5.907420853759282053, 0.08058608058608254798 ) ) ;
#98128 = CARTESIAN_POINT ( 'NONE',  ( 6.527294062531273866, -1.270327234845580078, -1.468905576289506909 ) ) ;
#98129 = CARTESIAN_POINT ( 'NONE',  ( 2.150558370509841666, -1.692889690492072718, 1.391600924549152296 ) ) ;
#98130 = CARTESIAN_POINT ( 'NONE',  ( 1.276469996339978819, 1.608456030955440541, -0.6653204537699786147 ) ) ;
#98131 = CARTESIAN_POINT ( 'NONE',  ( 5.262536180398716290, 9.291375977107183104, -0.7998128361456291469 ) ) ;
#98132 = CARTESIAN_POINT ( 'NONE',  ( 0.1333692844072559003, 5.722267537706915874, -2.647605121726896105 ) ) ;
#98133 = CARTESIAN_POINT ( 'NONE',  ( 1.259898821826772819, 0.6958341084943464594, 1.578493908868659146 ) ) ;
#98134 = CARTESIAN_POINT ( 'NONE',  ( 1.312353134292881141, 1.468346937154514364, -1.627112938194043235 ) ) ;
#98135 = CARTESIAN_POINT ( 'NONE',  ( 3.703933201646680828, -0.6411959742554216302, 2.111683309420588905 ) ) ;
#98136 = CARTESIAN_POINT ( 'NONE',  ( 1.094852686531849084, 2.138608527004157711, 0.3732488551555103173 ) ) ;
#98137 = CARTESIAN_POINT ( 'NONE',  ( -1.244123718695706815, 2.973244533904600750, 0.7750000000000170086 ) ) ;
#98139 = CARTESIAN_POINT ( 'NONE',  ( 2.378245518041781636, -2.112004366230528785, -0.1507482023494610135 ) ) ;
#98138 = B_SPLINE_CURVE_WITH_KNOTS ( 'NONE', 3,
 ( #196425, #162868, #195361, #95751, #213701, #127248, #128321 ),
 .UNSPECIFIED., .F., .F.,
 ( 4, 3, 4 ),
 ( 0.0001788552925466893823, 0.0009000000022260270637, 0.002103779968145176940 ),
 .UNSPECIFIED. ) ;
#98140 = CARTESIAN_POINT ( 'NONE',  ( 6.639320575229255006, 1.299223727596211519, 1.914393416674460946 ) ) ;
#98141 = ORIENTED_EDGE ( 'NONE', *, *, #32339, .T. ) ;
#98143 = CARTESIAN_POINT ( 'NONE',  ( 1.364683531249986537, -0.07395833299191513499, 0.7879004041258500513 ) ) ;
#98142 = CARTESIAN_POINT ( 'NONE',  ( 2.630776572171345418, 0.2838290345775448809, 2.274689434353324824 ) ) ;
#98144 = CARTESIAN_POINT ( 'NONE',  ( 4.330940004561544043, 7.140181541042074365, -1.199719254218452047 ) ) ;
#98145 = CARTESIAN_POINT ( 'NONE',  ( 5.110122900737038343, -0.8006010496643833907, 2.072185752117897461 ) ) ;
#98146 = CARTESIAN_POINT ( 'NONE',  ( -6.941411460516810017, 8.161030127766803588, 1.082531754730549967 ) ) ;
#98147 = LINE ( 'NONE', #15783, #73627 ) ;
#98148 = CARTESIAN_POINT ( 'NONE',  ( 4.853455804012216213, 6.685451076146141425, 1.443375672974062551 ) ) ;
#98149 = AXIS2_PLACEMENT_3D ( 'NONE', #205174, #107774, #88252 ) ;
#98150 = CARTESIAN_POINT ( 'NONE',  ( -6.195713011320783892, 10.17215624660883577, -0.7216878364870267237 ) ) ;
#98151 = AXIS2_PLACEMENT_3D ( 'NONE', #25102, #40313, #91204 ) ;
#98152 = EDGE_CURVE ( 'NONE', #45056, #31312, #144125, .T. ) ;
#98153 = CARTESIAN_POINT ( 'NONE',  ( 5.248414862265931902, 5.295774558831261913, 0.000000000000000000 ) ) ;
#98154 = ORIENTED_EDGE ( 'NONE', *, *, #183845, .F. ) ;
#98155 = CARTESIAN_POINT ( 'NONE',  ( 3.147111449167848019, 0.9091449406319618287, 1.799922684605055556 ) ) ;
#98157 = CARTESIAN_POINT ( 'NONE',  ( 1.235300832636996970, -0.04672723545543105983, -2.062185333280424526 ) ) ;
#98156 = CARTESIAN_POINT ( 'NONE',  ( 7.100719765255169236, 9.307259030929609267, -1.599625672291262513 ) ) ;
#98158 = CARTESIAN_POINT ( 'NONE',  ( -2.946110181334088196, 6.448586377034708050, 0.1685663139843082692 ) ) ;
#98159 = CARTESIAN_POINT ( 'NONE',  ( 5.194182247366878613, 6.192872389083746043, 1.082531754730549078 ) ) ;
#98160 = CIRCLE ( 'NONE', #60097, 11.09999999999999964 ) ;
#98161 = CARTESIAN_POINT ( 'NONE',  ( -1.201851678989727383E-14, 3.571875000341422357, 1.575800808251672791 ) ) ;
#98162 = CARTESIAN_POINT ( 'NONE',  ( 4.048915112334880106, -1.821525731582713359, -1.218098874207810933 ) ) ;
#98163 = CARTESIAN_POINT ( 'NONE',  ( 2.707657903872981553, 1.899618770239443366, 0.6767133375917554483 ) ) ;
#98164 = CARTESIAN_POINT ( 'NONE',  ( 1.575478407343299692, -0.9843019613302635973, 1.555867251595323353 ) ) ;
#98165 = CARTESIAN_POINT ( 'NONE',  ( 8.145751363712157911, 8.397798100619326078, -0.7998128361456281477 ) ) ;
#98166 = CARTESIAN_POINT ( 'NONE',  ( 4.858326754937916547, 0.6996357133068830114, 1.686392194618462570 ) ) ;
#98167 = CARTESIAN_POINT ( 'NONE',  ( 6.469375277500488686, -1.978045142091336306, -0.3906011616893814709 ) ) ;
#98168 = CARTESIAN_POINT ( 'NONE',  ( -7.823218330285243383, 9.085841792542966644, -1.199719254218446718 ) ) ;
#98170 = CARTESIAN_POINT ( 'NONE',  ( -5.875479466675803231, 7.948088359245467416, -1.599625672291271394 ) ) ;
#98169 = CARTESIAN_POINT ( 'NONE',  ( 4.838899928913665605, 0.3820838354035635542, 2.229877907420589001 ) ) ;
#98171 = CARTESIAN_POINT ( 'NONE',  ( 0.7683615598204245334, 1.039662503867449184, 1.831484773650635223 ) ) ;
#98172 = CARTESIAN_POINT ( 'NONE',  ( -7.273023059088104425, 7.449891421883056530, 0.000000000000000000 ) ) ;
#98173 = CARTESIAN_POINT ( 'NONE',  ( 4.721179655770254335, -1.847879960204744432, -0.9338546512941485744 ) ) ;
#98174 = CARTESIAN_POINT ( 'NONE',  ( 9.887974103068218668, 10.43039129653476493, 0.7998128361456462443 ) ) ;
#98175 = CARTESIAN_POINT ( 'NONE',  ( 8.378074386687007546, 27.50815134976858900, 15.76159487570644124 ) ) ;
#98176 = CARTESIAN_POINT ( 'NONE',  ( -8.636707547105197946, 10.03491254549959777, -1.199719254218446718 ) ) ;
#98177 = FILL_AREA_STYLE_COLOUR ( '', #151279 ) ;
#98178 = CARTESIAN_POINT ( 'NONE',  ( 7.686546744304875389, 7.932335721302671949, 0.7998128361456291469 ) ) ;
#98179 = CARTESIAN_POINT ( 'NONE',  ( 5.394965581569445057, 6.295244270701876310, -1.058425382943289028 ) ) ;
#98180 = CARTESIAN_POINT ( 'NONE',  ( -3.602716132929368875, 5.226254793216122074, 1.599625672291267398 ) ) ;
#98182 = CARTESIAN_POINT ( 'NONE',  ( 1.248599636731639428, 1.089134306475655789, -1.936006665247846481 ) ) ;
#98181 = CARTESIAN_POINT ( 'NONE',  ( 1.476976393720278002, -1.495863523836362896, 1.503369785937097136 ) ) ;
#98183 = DIRECTION ( 'NONE',  ( 1.000000000000000000, 0.000000000000000000, 1.224646799147353207E-16 ) ) ;
#98184 = CARTESIAN_POINT ( 'NONE',  ( -7.425025402139490360, 8.691559719698066289, 1.199719254218452047 ) ) ;
#98185 = CARTESIAN_POINT ( 'NONE',  ( 7.461064606222022277, 7.598996883547496139, 1.040834085586084257E-14 ) ) ;
#98186 = CARTESIAN_POINT ( 'NONE',  ( 3.086327779807009009, 1.092107249913790712, -1.629585102321646328 ) ) ;
#98187 = CARTESIAN_POINT ( 'NONE',  ( 6.335737856287750880, 6.286115675290828264, -0.7998128361456281477 ) ) ;
#98188 = CARTESIAN_POINT ( 'NONE',  ( -4.072711641797504001, 7.543564457389225986, 0.4874124537386469447 ) ) ;
#98189 = CARTESIAN_POINT ( 'NONE',  ( 2.686486993802192913, 6.285985259411197568, 0.7998128361456362523 ) ) ;
#98190 = CARTESIAN_POINT ( 'NONE',  ( -4.828112100242283766, 7.686528979374367410, -1.082531754730549967 ) ) ;
#98191 = CARTESIAN_POINT ( 'NONE',  ( -7.402388683381436074, 7.738467673474211495, 0.7216878364870317197 ) ) ;
#98192 = CARTESIAN_POINT ( 'NONE',  ( 2.144932638433934002, 2.058100890041581810, 0.5106320605416380110 ) ) ;
#98193 = CARTESIAN_POINT ( 'NONE',  ( -6.231907884136888676, 7.299589282028351001, -1.199719254218453823 ) ) ;
#98194 = CARTESIAN_POINT ( 'NONE',  ( 5.898874287966751950, 0.3812104124719677412, 1.924297140916144233 ) ) ;
#98195 = CARTESIAN_POINT ( 'NONE',  ( 3.608425205800522839, -0.8741791752944136906, -1.977237025433141504 ) ) ;
#98196 = CARTESIAN_POINT ( 'NONE',  ( 3.104851637799400876, -0.3563606998662186554, 1.806257425991746546 ) ) ;
#98197 = CARTESIAN_POINT ( 'NONE',  ( -4.034767475943390025, 7.597003608976943489, -0.2951547658557127640 ) ) ;
#98198 = CARTESIAN_POINT ( 'NONE',  ( 0.6823417656249882723, -0.5947916663252492686, 1.181850606188755259 ) ) ;
#98199 = CARTESIAN_POINT ( 'NONE',  ( 4.927569761290923722, 0.8905454123377859466, -1.495065219958094938 ) ) ;
#98200 = CARTESIAN_POINT ( 'NONE',  ( 6.727182134110241130, 2.994815527893503138, 2.165292399158074588 ) ) ;
#98201 = CARTESIAN_POINT ( 'NONE',  ( 3.362058906508953449, 6.866226457661676719, -0.7216878364870267237 ) ) ;
#98202 = CARTESIAN_POINT ( 'NONE',  ( 1.797963993548271411, -0.7283430984801853025, 2.035426966748521860 ) ) ;
#98203 = CARTESIAN_POINT ( 'NONE',  ( 4.991564454312596766, 1.928456700051227379, 0.5879293935868237231 ) ) ;
#98204 = CARTESIAN_POINT ( 'NONE',  ( -8.581948047326017459, 11.99572790764693409, 1.082531754730558626 ) ) ;
#98205 = CARTESIAN_POINT ( 'NONE',  ( 0.7081719773709761467, -2.151164098719647200, 0.2130325561137471624 ) ) ;
#98206 = CARTESIAN_POINT ( 'NONE',  ( 3.145733524295030836, 0.7127697582950813793, -1.838151395584181058 ) ) ;
#98207 = CARTESIAN_POINT ( 'NONE',  ( 10.36939107341407507, 1.813436143228259745, 6.039542801432597585 ) ) ;
#98208 = CARTESIAN_POINT ( 'NONE',  ( 3.667467498987980967, 1.081383794499408468, 1.612947176984424802 ) ) ;
#98211 = ORIENTED_EDGE ( 'NONE', *, *, #27310, .F. ) ;
#98210 = LINE ( 'NONE', #644, #177723 ) ;
#98209 = DIRECTION ( 'NONE',  ( -1.000000000000000000, 0.000000000000000000, -8.638326563840826660E-31 ) ) ;
#98212 = CARTESIAN_POINT ( 'NONE',  ( -5.745623237141265882, 9.925253886631958622, 0.7998128361456291469 ) ) ;
#98213 = CARTESIAN_POINT ( 'NONE',  ( 0.07755575628183573877, -0.002876890934064984216, -2.188974970840869005 ) ) ;
#98215 = ORIENTED_EDGE ( 'NONE', *, *, #126245, .F. ) ;
#98214 = CARTESIAN_POINT ( 'NONE',  ( -5.712781623311813384, 7.758274208654143855, -1.599625672291271394 ) ) ;
#98216 = CARTESIAN_POINT ( 'NONE',  ( -9.286972035236635392, 9.937148250638648150, -0.7216878364870267237 ) ) ;
#98217 = CARTESIAN_POINT ( 'NONE',  ( 0.7103623821160671703, -2.195938746145317477, 0.2182302698266261887 ) ) ;
#98218 = CARTESIAN_POINT ( 'NONE',  ( -1.642778471874998480, -1.451041666188708446, 2.845375778867863303 ) ) ;
#98219 = CARTESIAN_POINT ( 'NONE',  ( 5.524254240939322713, 0.9636562883742012531, 1.708648623189083393 ) ) ;
#98220 = CARTESIAN_POINT ( 'NONE',  ( 4.012992375354424546, 0.1078809898697324771, 2.114737393012538824 ) ) ;
#98221 = CARTESIAN_POINT ( 'NONE',  ( 0.7499999999999885647, 2.597916667349486897, -1.299038105676658228 ) ) ;
#98222 = CARTESIAN_POINT ( 'NONE',  ( 9.584290747383175102, -7.189645481338100552, -0.001121896803057515716 ) ) ;
#98223 = CARTESIAN_POINT ( 'NONE',  ( 4.488128036367874607, -0.4058819498431766037, -1.795677737744493019 ) ) ;
#98224 = VERTEX_POINT ( 'NONE', #185395 ) ;
#98225 = CARTESIAN_POINT ( 'NONE',  ( -6.170932472514347289, 10.35117165124207972, 0.000000000000000000 ) ) ;
#98226 = CARTESIAN_POINT ( 'NONE',  ( 7.884707905546932238, -7.003075417673650271, -7.228805602686596110 ) ) ;
#98227 = CARTESIAN_POINT ( 'NONE',  ( 4.658503719480325600, 2.115088938745744329, 0.1532479335744421078 ) ) ;
#98228 = CARTESIAN_POINT ( 'NONE',  ( 5.449487677688982679, 8.445153826357429949, -1.199719254218446718 ) ) ;
#98229 = CARTESIAN_POINT ( 'NONE',  ( 6.239539339872155033, -1.489444859125512277, -1.424447411405028507 ) ) ;
#98232 = CARTESIAN_POINT ( 'NONE',  ( 3.931074656914943954, -1.272613488525012659, -1.330884258478791438 ) ) ;
#98231 = CARTESIAN_POINT ( 'NONE',  ( 0.7657746542184565852, -1.852627923093919771, 0.1767624929009704582 ) ) ;
#98230 = CARTESIAN_POINT ( 'NONE',  ( -4.217958839219735800, 3.978389137448586244, 0.5316758947214468289 ) ) ;
#98233 = CARTESIAN_POINT ( 'NONE',  ( 7.072549687823125097, 11.40305840243567381, -0.7998128361456291469 ) ) ;
#98234 = DIRECTION ( 'NONE',  ( 0.000000000000000000, 1.000000000000000000, 0.000000000000000000 ) ) ;
#98235 = CARTESIAN_POINT ( 'NONE',  ( -6.794571259104023930, 7.956029886156682274, 1.199719254218452047 ) ) ;
#98236 = CARTESIAN_POINT ( 'NONE',  ( -0.4655551865852154414, -8.176568542494919711, -9.512045263456256450 ) ) ;
#98237 = CARTESIAN_POINT ( 'NONE',  ( 3.756632125300945368, 0.7937082651479386852, 2.059386989456575279 ) ) ;
#98238 = CARTESIAN_POINT ( 'NONE',  ( 4.657670937300908420, 0.5017462980881717272, -2.205921056424357651 ) ) ;
#98239 = CARTESIAN_POINT ( 'NONE',  ( -6.643132081016132062, 8.773406732650713025, 1.443375672974078761 ) ) ;
#98240 = CARTESIAN_POINT ( 'NONE',  ( 4.728658910183288988, 1.244086218232887120, -1.317109676944823393 ) ) ;
#98241 = CARTESIAN_POINT ( 'NONE',  ( 5.682812683241409424, 1.562005318756795713, -1.108807820749290851 ) ) ;
#98242 = CARTESIAN_POINT ( 'NONE',  ( 1.364683531249990311, 4.926041667008083991, 0.7879004041258500513 ) ) ;
#98243 = EDGE_CURVE ( 'NONE', #69507, #146527, #86842, .T. ) ;
#98244 = CARTESIAN_POINT ( 'NONE',  ( 6.280143113937574739, -0.9989825818290422044, 1.581392243879369053 ) ) ;
#98245 = CARTESIAN_POINT ( 'NONE',  ( 5.424199618621329044, 0.9171840495176122321, 1.619240327305818683 ) ) ;
#98246 = CARTESIAN_POINT ( 'NONE',  ( 6.631742710195931423, -1.160100399838214891, -1.336722620761298330 ) ) ;
#98247 = CARTESIAN_POINT ( 'NONE',  ( 1.024625454658374624, 0.3981145430279106057, 1.976669095394629982 ) ) ;
#98249 = CARTESIAN_POINT ( 'NONE',  ( 3.194068465612946994, -0.8531780664592978347, 1.925702383005133855 ) ) ;
#98248 = CARTESIAN_POINT ( 'NONE',  ( -10.15522075183580419, 11.80651128435196462, 1.199719254218462483 ) ) ;
#98250 = CARTESIAN_POINT ( 'NONE',  ( 10.08456733046637765, 10.65975006183261087, 0.000000000000000000 ) ) ;
#98252 = CARTESIAN_POINT ( 'NONE',  ( -8.696665468161981494, 12.23352791524263239, -1.199719254218446718 ) ) ;
#98251 = CARTESIAN_POINT ( 'NONE',  ( 3.469446951953614189E-15, 5.229711127717882491, 1.214306433183764966E-14 ) ) ;
#98253 = CARTESIAN_POINT ( 'NONE',  ( 2.074478865019005802, 0.8673736069498124701, 1.824228476594942583 ) ) ;
#98254 = CARTESIAN_POINT ( 'NONE',  ( -1.364683531250012516, 2.030208333674750953, 0.7879004041258379498 ) ) ;
#98255 = CARTESIAN_POINT ( 'NONE',  ( 3.161022370280501814, 6.839609865302569425, 0.000000000000000000 ) ) ;
#98256 = CARTESIAN_POINT ( 'NONE',  ( 3.725982817344280829, -1.284327275973631277, -1.738548686538298416 ) ) ;
#98257 = CARTESIAN_POINT ( 'NONE',  ( 6.620655732516644854, 4.701125524277991907, 2.388986273831222640 ) ) ;
#98260 = DIRECTION ( 'NONE',  ( -1.000000000000000000, 6.308085367188389255E-16, 0.000000000000000000 ) ) ;
#98259 = CARTESIAN_POINT ( 'NONE',  ( 11.94980361058169116, 10.19999999999999929, -1.099999999999998535 ) ) ;
#98258 = CARTESIAN_POINT ( 'NONE',  ( 4.004454267989866700, 5.765225627445230927, 1.599625672291262513 ) ) ;
#98261 = CARTESIAN_POINT ( 'NONE',  ( 9.259855728009286580, 10.86588177317476855, -1.082531754730543083 ) ) ;
#98262 = CARTESIAN_POINT ( 'NONE',  ( 11.89197415570408900, 9.799999999999998934, -0.8055989572471863314 ) ) ;
#98263 = CARTESIAN_POINT ( 'NONE',  ( -7.049876689426103127, 10.20831132343037062, -1.082531754730537976 ) ) ;
#98264 = CARTESIAN_POINT ( 'NONE',  ( -1.364683531250000748, 0.5093750003414208027, 0.000000000000000000 ) ) ;
#98265 = CARTESIAN_POINT ( 'NONE',  ( 0.8201894534925309177, 1.301127354658284663, -1.763390660798454634 ) ) ;
#98266 = DIRECTION ( 'NONE',  ( 1.000000000000000000, 0.000000000000000000, 0.000000000000000000 ) ) ;
#98267 = CARTESIAN_POINT ( 'NONE',  ( 0.9895999521203084903, 1.994116446801162290, -1.068836969126084835 ) ) ;
#98268 = CARTESIAN_POINT ( 'NONE',  ( -7.483210719738908168, 10.81783070874899799, 1.199719254218453823 ) ) ;
#98269 = CARTESIAN_POINT ( 'NONE',  ( -4.894130264408878439, 4.812166184672871161, -0.7216878364870197293 ) ) ;
#98270 = CARTESIAN_POINT ( 'NONE',  ( -1.364683531250010295, 4.092708333674751842, 0.7879004041258379498 ) ) ;
#98271 = CARTESIAN_POINT ( 'NONE',  ( 7.654042494670951690E-16, -13.99999999999999822, -6.249999999999995559 ) ) ;
#98272 = CARTESIAN_POINT ( 'NONE',  ( -1.500000000000015099, 11.47916666666666252, -0.8660254037844309360 ) ) ;
#98273 = CARTESIAN_POINT ( 'NONE',  ( 7.838022202476093270, 8.316983122409855156, 0.7216878364870267237 ) ) ;
#98274 = CARTESIAN_POINT ( 'NONE',  ( 2.969704930451398717, 0.9433242808821461489, 1.497149023046380423 ) ) ;
#98275 = CARTESIAN_POINT ( 'NONE',  ( 8.211434591371064684, 12.73175745657494851, -0.7998128361456352531 ) ) ;
#98276 = CARTESIAN_POINT ( 'NONE',  ( 0.1828346100962909559, -2.042824957133956953, -0.5113311198858895290 ) ) ;
#98277 = CARTESIAN_POINT ( 'NONE',  ( 0.6823417656249969321, 8.776041667008065872, -1.181850606188757036 ) ) ;
#98278 = ORIENTED_EDGE ( 'NONE', *, *, #158238, .T. ) ;
#98279 = CARTESIAN_POINT ( 'NONE',  ( -4.762657100150483380, 8.778460060142702304, 0.000000000000000000 ) ) ;
#98280 = CARTESIAN_POINT ( 'NONE',  ( 5.062125140741547291, -1.117816439015427044, 1.678017345901124058 ) ) ;
#98281 = ORIENTED_EDGE ( 'NONE', *, *, #53503, .F. ) ;
#98282 = CARTESIAN_POINT ( 'NONE',  ( 2.043623373375623942, 0.7184291972081280342, -1.727395513401897453 ) ) ;
#98283 = CARTESIAN_POINT ( 'NONE',  ( 3.221598570378156001, 0.3083542414583049784, -2.047064864394084971 ) ) ;
#98284 = CARTESIAN_POINT ( 'NONE',  ( -5.573810548549546162, 9.516879716700865188, 0.7216878364870267237 ) ) ;
#98285 = CARTESIAN_POINT ( 'NONE',  ( 1.441514601552947417, -1.799640695080907182, 0.6472408003148700795 ) ) ;
#98286 = CARTESIAN_POINT ( 'NONE',  ( -1.420000000000021911, 7.176846818246207960, 4.202462424328227364 ) ) ;
#98287 = CARTESIAN_POINT ( 'NONE',  ( -9.956244568750863166, 5.504298494775027528, -6.025958004757996811 ) ) ;
#98288 =( NAMED_UNIT ( * ) PLANE_ANGLE_UNIT ( ) SI_UNIT ( $, .RADIAN. ) );
#98289 = CIRCLE ( 'NONE', #105113, 0.4000000000000010214 ) ;
#98290 = CARTESIAN_POINT ( 'NONE',  ( -1.364683531250012516, 4.801041667008083991, -0.7879004041258300672 ) ) ;
#98291 = CARTESIAN_POINT ( 'NONE',  ( 0.9668906521006037647, -1.505869814250645478, 1.178657042999963878 ) ) ;
#98292 = CARTESIAN_POINT ( 'NONE',  ( 3.385159196556942085, 0.04556868695702701727, 1.961494628812537444 ) ) ;
#98293 = CARTESIAN_POINT ( 'NONE',  ( 0.2103132415818432799, -1.556605082263945228, -1.280954711483893727 ) ) ;
#98294 = CARTESIAN_POINT ( 'NONE',  ( -6.134138155540168391, 6.121192367743780949, 0.000000000000000000 ) ) ;
#98295 = CARTESIAN_POINT ( 'NONE',  ( 7.313733799568044702, 10.62010763521636214, 1.199719254218460707 ) ) ;
#98296 = CARTESIAN_POINT ( 'NONE',  ( 6.919227946136824237, -0.1375138451006757134, 1.940497564164916922 ) ) ;
#98297 = CARTESIAN_POINT ( 'NONE',  ( -1.201851678989727383E-14, 2.571875000341417472, 1.575800808251672791 ) ) ;
#98298 = CARTESIAN_POINT ( 'NONE',  ( 1.951433385020440836, -1.796364150513751312, 0.9090842167202308755 ) ) ;
#98300 = CARTESIAN_POINT ( 'NONE',  ( 1.863061375884986104, -0.1076188601273372486, -2.114627633294167364 ) ) ;
#98299 = CARTESIAN_POINT ( 'NONE',  ( -6.399085315970137522, 9.449054721065074602, -1.082531754730538864 ) ) ;
#98301 = CARTESIAN_POINT ( 'NONE',  ( 3.279797552538410876, -1.996039814156633785, 0.5495672325947635883 ) ) ;
#98302 = CARTESIAN_POINT ( 'NONE',  ( 3.739016502318667445, 7.584212696005614873, 0.7998128361456271485 ) ) ;
#98304 = CARTESIAN_POINT ( 'NONE',  ( 3.948449050077836642, 5.629609863222681199, 1.599625672291267398 ) ) ;
#98303 = CARTESIAN_POINT ( 'NONE',  ( 5.912080347638632993, 1.404955882617323848, -1.548356120136730851 ) ) ;
#98306 = ORIENTED_EDGE ( 'NONE', *, *, #195535, .F. ) ;
#98305 = CARTESIAN_POINT ( 'NONE',  ( 3.662960631648714216, -1.609669772967847079, -0.8612380056681954166 ) ) ;
#98307 = CARTESIAN_POINT ( 'NONE',  ( 7.892817981449907982, 12.36003807833360391, 0.7998128361456462443 ) ) ;
#98308 = CARTESIAN_POINT ( 'NONE',  ( 6.890000000000008562, 4.693995042360769254, 2.562605081426702736 ) ) ;
#98309 = CARTESIAN_POINT ( 'NONE',  ( 9.348030350560099677, 12.83729060537138089, -6.611360045021780429 ) ) ;
#98310 = CARTESIAN_POINT ( 'NONE',  ( 5.913141818906855640, 1.943543578741913969, 1.045239939247793792 ) ) ;
#98311 = CARTESIAN_POINT ( 'NONE',  ( 0.6823417656249969321, 10.33854166700806587, -1.181850606188757036 ) ) ;
#98312 = ORIENTED_EDGE ( 'NONE', *, *, #169996, .T. ) ;
#98313 = CARTESIAN_POINT ( 'NONE',  ( 4.705663775918221603, 1.419457463540532816, 1.281590252682027087 ) ) ;
#98314 = CARTESIAN_POINT ( 'NONE',  ( -9.297140650669053485, 11.86975006391249643, 1.599625672291281386 ) ) ;
#98315 = CARTESIAN_POINT ( 'NONE',  ( 8.281332899848809603, 8.555976559445431562, 0.7998128361456481317 ) ) ;
#98316 = CARTESIAN_POINT ( 'NONE',  ( -2.754243431018125239E-14, 1.984375000341467299, 1.570758158831788265 ) ) ;
#98317 = CARTESIAN_POINT ( 'NONE',  ( 3.836594282542902246, 7.419851063034623273, 0.7216878364870317197 ) ) ;
#98318 = CARTESIAN_POINT ( 'NONE',  ( -5.595389610960904037, 5.773517989023353003, 0.3570679098348183422 ) ) ;
#98319 = DIRECTION ( 'NONE',  ( 0.1674078377060222722, 0.000000000000000000, 0.9858877298529452604 ) ) ;
#98320 = CARTESIAN_POINT ( 'NONE',  ( 0.2394788589213901198, 1.836227513651207177, 0.1364553164684492448 ) ) ;
#98321 = VERTEX_POINT ( 'NONE', #123704 ) ;
#98322 = CARTESIAN_POINT ( 'NONE',  ( -8.072954122294394352, 8.383144328957069291, -0.7998128361456362523 ) ) ;
#98323 = CARTESIAN_POINT ( 'NONE',  ( 4.921099816907485547, -0.09337705715995942013, 1.868355541605345671 ) ) ;
#98324 = CARTESIAN_POINT ( 'NONE',  ( -1.715338164143663136, 0.7127732114542476571, 0.8729459113246227364 ) ) ;
#98325 = CARTESIAN_POINT ( 'NONE',  ( 8.005163354226054295, 8.304055099544019214, 0.000000000000000000 ) ) ;
#98326 = DIRECTION ( 'NONE',  ( -0.7806247490453480653, -4.396526966619892032E-05, 0.6249999993959538536 ) ) ;
#98327 = CARTESIAN_POINT ( 'NONE',  ( -8.039621903223732602, 8.481906429956900695, 1.040834085586084257E-14 ) ) ;
#98328 = CARTESIAN_POINT ( 'NONE',  ( 4.497554271431305040, 6.270232621468402989, -1.599625672291256295 ) ) ;
#98329 = CARTESIAN_POINT ( 'NONE',  ( 0.7605272443651526215, -0.6583816729706105653, -1.856300379560266833 ) ) ;
#98330 = CARTESIAN_POINT ( 'NONE',  ( 2.073842424929934314, -0.8596134062341630466, 1.824128527830502833 ) ) ;
#98331 = CARTESIAN_POINT ( 'NONE',  ( -7.296259222448620463, 11.66405285949874759, 0.7998128361456481317 ) ) ;
#98332 = CARTESIAN_POINT ( 'NONE',  ( 5.071631979963703962, 8.074598522336444262, 1.199719254218451159 ) ) ;
#98333 = CARTESIAN_POINT ( 'NONE',  ( 6.717748655459634399, -7.246166700180800113, 6.717748655459616636 ) ) ;
#98334 = CARTESIAN_POINT ( 'NONE',  ( 2.572451567087580493, -2.097416440861415321, -0.6350555677336399141 ) ) ;
#98335 = CARTESIAN_POINT ( 'NONE',  ( 2.474351396550318771, 0.3224749582910498846, -0.3303680917369555270 ) ) ;
#98336 = CARTESIAN_POINT ( 'NONE',  ( -9.592557376868645846, 11.15007068022363157, -1.199719254218441611 ) ) ;
#98337 = CARTESIAN_POINT ( 'NONE',  ( -2.889872605471121236, 6.605953636083950364, 2.500000000000000000 ) ) ;
#98338 = CARTESIAN_POINT ( 'NONE',  ( 0.000000000000000000, 7.250000000000006217, 0.000000000000000000 ) ) ;
#98339 = CARTESIAN_POINT ( 'NONE',  ( 3.418064124421011041, 7.001842221884225559, -0.7216878364870338292 ) ) ;
#98340 = CARTESIAN_POINT ( 'NONE',  ( 7.411503528164766763, 11.79850454950093841, 1.040834085586084257E-14 ) ) ;
#98341 = CARTESIAN_POINT ( 'NONE',  ( 3.231779075379137556, 6.036511184309975242, -0.9899555337401846344 ) ) ;
#98342 = CARTESIAN_POINT ( 'NONE',  ( 5.397554552016212703, 8.350878506444006533, 1.082531754730547524 ) ) ;
#98343 = ORIENTED_EDGE ( 'NONE', *, *, #141101, .F. ) ;
#98345 = CARTESIAN_POINT ( 'NONE',  ( 1.717441043944417878, 1.674910534618522906, 1.116504076032026616 ) ) ;
#98344 = CARTESIAN_POINT ( 'NONE',  ( 5.354971380013192395, 0.3533838956982695567, -1.806849549699687696 ) ) ;
#98346 = CARTESIAN_POINT ( 'NONE',  ( 3.567963868821962592, 1.814363981409074844, -1.410851157308941506 ) ) ;
#98347 = CARTESIAN_POINT ( 'NONE',  ( 1.023987020198445341, 0.9106972337104453086, 1.622782493823480943 ) ) ;
#98348 = CARTESIAN_POINT ( 'NONE',  ( 3.285556943750000514, -1.713541666188707735, 1.896917185911906500 ) ) ;
#98349 = CYLINDRICAL_SURFACE ( 'NONE', #29395, 1.500000000000000222 ) ;
#98350 = CARTESIAN_POINT ( 'NONE',  ( 5.361546783204238942, -1.511448857895525855, -1.171587532507123441 ) ) ;
#98351 = CARTESIAN_POINT ( 'NONE',  ( -8.833300774503376473, 10.26427131079744193, 1.199719254218462483 ) ) ;
#98352 = ADVANCED_FACE ( 'NONE', ( #187532 ), #136675, .F. ) ;
#98353 = CARTESIAN_POINT ( 'NONE',  ( -5.451787166470911217, 9.374519104275787384, 0.7216878364870267237 ) ) ;
#98355 = CARTESIAN_POINT ( 'NONE',  ( 3.238977024203249400, -1.650389259550872456, 0.8806316622528218563 ) ) ;
#98354 = CARTESIAN_POINT ( 'NONE',  ( 3.210569733434172512, 1.891194753341999935, 0.8916721373675460249 ) ) ;
#98356 = CARTESIAN_POINT ( 'NONE',  ( 6.290620087060792009, 10.28288116830553101, -0.7216878364870267237 ) ) ;
#98357 = CARTESIAN_POINT ( 'NONE',  ( 6.374545129912787544, -0.09763137639631430664, -1.838803627010993313 ) ) ;
#98358 = CARTESIAN_POINT ( 'NONE',  ( 3.684065054611349144, 5.321161868511784299, -1.599625672291262513 ) ) ;
#98360 = CARTESIAN_POINT ( 'NONE',  ( 5.705283713252285338, 5.550585841749444249, -0.7998128361456211532 ) ) ;
#98359 = CARTESIAN_POINT ( 'NONE',  ( 0.4382560683119228195, -7.666862915010161039, -10.99126615174918520 ) ) ;
#98361 = CARTESIAN_POINT ( 'NONE',  ( 4.582452686631489414, -1.674003568303910949, -0.4152789331205719026 ) ) ;
#98362 = CARTESIAN_POINT ( 'NONE',  ( -7.172426956829277778, 8.326585190177668849, -1.199719254218452935 ) ) ;
#98363 = DIRECTION ( 'NONE',  ( -0.000000000000000000, -1.000000000000000000, -0.000000000000000000 ) ) ;
#98364 = CARTESIAN_POINT ( 'NONE',  ( 1.910130646976109681, 3.278792710263288779, 0.4195261609910589939 ) ) ;
#98365 = CARTESIAN_POINT ( 'NONE',  ( 11.04986227068298277, 11.10939997844336347, -1.056429153205399984 ) ) ;
#98366 = CARTESIAN_POINT ( 'NONE',  ( 9.578245405452067374, -9.921948021430829101, -0.1647502191513116609 ) ) ;
#98367 = CARTESIAN_POINT ( 'NONE',  ( 4.786072553063510426, -1.330480670633835683, -1.715586834332043953 ) ) ;
#98368 = CARTESIAN_POINT ( 'NONE',  ( 3.123480263227970344, -1.759325740769552393, 0.4874977319994436287 ) ) ;
#98369 = CARTESIAN_POINT ( 'NONE',  ( 0.6550357524967264089, 1.634203043994170157, -1.084997510809107446 ) ) ;
#98370 = CARTESIAN_POINT ( 'NONE',  ( 5.331313699870084299, -1.671001674814942994, -1.300292098898154780 ) ) ;
#98372 = CARTESIAN_POINT ( 'NONE',  ( 1.364683531249988535, 3.426041667008085323, 0.7879004041258500513 ) ) ;
#98371 = CARTESIAN_POINT ( 'NONE',  ( 5.636350782834250062, 0.4440221345313396517, 2.248805093627189500 ) ) ;
#98373 = CARTESIAN_POINT ( 'NONE',  ( 4.324687812634887329, 6.068555086205916105, 1.443375672974062551 ) ) ;
#98374 = CARTESIAN_POINT ( 'NONE',  ( 7.242026607993941489, 11.60078147596829901, 0.7998128361456462443 ) ) ;
#98375 = CARTESIAN_POINT ( 'NONE',  ( 1.260569961473339440, 2.118219532560499996, 0.1004958096475216667 ) ) ;
#98376 = CARTESIAN_POINT ( 'NONE',  ( -3.904385051055635270, 6.538571078664754843, 1.082531754730560403 ) ) ;
#98377 = CARTESIAN_POINT ( 'NONE',  ( 6.021229617800532452, 6.197391773621639288, 0.000000000000000000 ) ) ;
#98378 = CARTESIAN_POINT ( 'NONE',  ( -5.572037945092175981, 5.603058478803387032, 0.7216878364870317197 ) ) ;
#98379 = EDGE_CURVE ( 'NONE', #99270, #72363, #132479, .T. ) ;
#98380 = CARTESIAN_POINT ( 'NONE',  ( 6.789883322502159757, -1.411316560962400768, -1.649898940422918514 ) ) ;
#98382 = CARTESIAN_POINT ( 'NONE',  ( 0.7500000000000006661, 13.11458333401613352, 1.299038105676657340 ) ) ;
#98381 = CARTESIAN_POINT ( 'NONE',  ( 6.983263157960404754, 0.5601148359399975574, 2.204851038219941106 ) ) ;
#98384 = ORIENTED_EDGE ( 'NONE', *, *, #132650, .T. ) ;
#98383 = CARTESIAN_POINT ( 'NONE',  ( 1.928696271399105600, -1.050554081124959183, -1.957186058178138399 ) ) ;
#98385 = CARTESIAN_POINT ( 'NONE',  ( 6.346327303948391396, 0.3419391630616851474, -1.987045965717588958 ) ) ;
#98387 = CARTESIAN_POINT ( 'NONE',  ( 5.770399673640999261, -0.9225087518928692942, -1.844811731271531086 ) ) ;
#98386 = CARTESIAN_POINT ( 'NONE',  ( 3.486418057008484617, 7.219238166485217434, 1.040834085586084257E-14 ) ) ;
#98389 = CARTESIAN_POINT ( 'NONE',  ( 3.475000000000000533, -3.004166666666665542, 2.006292185433948827 ) ) ;
#98388 = CARTESIAN_POINT ( 'NONE',  ( 5.204350862799327793, 7.165104988056252289, -1.599625672291281386 ) ) ;
#98390 = CARTESIAN_POINT ( 'NONE',  ( 5.037736595929563244, 8.035053907629919223, -1.199719254218452047 ) ) ;
#98391 = CARTESIAN_POINT ( 'NONE',  ( -1.642778471875000035, -4.105208332855374564, -2.845375778867859751 ) ) ;
#98392 = FACE_OUTER_BOUND ( 'NONE', #109452, .T. ) ;
#98393 = CARTESIAN_POINT ( 'NONE',  ( 4.880324068823122197, -0.2306306682541107433, -1.826696389425507938 ) ) ;
#98395 = ORIENTED_EDGE ( 'NONE', *, *, #4999, .T. ) ;
#98394 = CARTESIAN_POINT ( 'NONE',  ( 5.678167406024951624, 5.518950149984223508, 0.7998128361456341429 ) ) ;
#98396 = CARTESIAN_POINT ( 'NONE',  ( -4.939248034080176097, 4.656877549381960080, 1.214306433183764966E-14 ) ) ;
#98397 = CARTESIAN_POINT ( 'NONE',  ( 2.186159124499872597, -1.690733796973374004, -0.3399922242280882245 ) ) ;
#98398 = CARTESIAN_POINT ( 'NONE',  ( 11.94105721237523277, 10.19999999999999929, 1.187919463087244720 ) ) ;
#98399 = CARTESIAN_POINT ( 'NONE',  ( 1.364683531249988535, 4.176041667008081326, 0.7879004041258500513 ) ) ;
#98400 = CARTESIAN_POINT ( 'NONE',  ( 1.212636322461498217, -1.017548795778918214, -2.020700439389290892 ) ) ;
#98401 = CARTESIAN_POINT ( 'NONE',  ( 3.879594643445562152, 1.983085605235184845, -0.7095211871808704274 ) ) ;
#98402 = CARTESIAN_POINT ( 'NONE',  ( -4.309512724297390740, 6.121127159803966933, 1.599625672291270506 ) ) ;
#98403 = CARTESIAN_POINT ( 'NONE',  ( 2.442341840454059554, 0.3829199517304190947, 1.727643488062768240 ) ) ;
#98404 = CARTESIAN_POINT ( 'NONE',  ( 6.100279051144945619, 9.204410428722734849, -1.199719254218440723 ) ) ;
#98405 = CARTESIAN_POINT ( 'NONE',  ( 3.892599500454932304, 7.555466827257172113, 0.7216878364870257245 ) ) ;
#98406 = CARTESIAN_POINT ( 'NONE',  ( -4.954615070790188369, 7.867802451642154082, -1.199719254218452047 ) ) ;
#98407 = CARTESIAN_POINT ( 'NONE',  ( 6.277061933002785032, 7.385955679000473673, 1.082531754730558626 ) ) ;
#98408 = CARTESIAN_POINT ( 'NONE',  ( -0.7500000000000215383, 1.691666666666688634, 1.299038105676659116 ) ) ;
#98409 = CARTESIAN_POINT ( 'NONE',  ( 5.238630872344578471, 1.322862460432130849, -1.784462157271723859 ) ) ;
#98410 = CARTESIAN_POINT ( 'NONE',  ( 3.978626637211603700, -0.2140425413966473567, -2.180973779111646138 ) ) ;
#98411 = CARTESIAN_POINT ( 'NONE',  ( -4.225337428953291230, 8.081310767087481750, 0.7998128361456341429 ) ) ;
#98412 = CARTESIAN_POINT ( 'NONE',  ( 0.4998684179604583333, 7.978338306496072896, -1.936700108954743316 ) ) ;
#98413 = DIRECTION ( 'NONE',  ( 0.000000000000000000, 0.000000000000000000, 1.000000000000000000 ) ) ;
#98414 = CARTESIAN_POINT ( 'NONE',  ( 0.6823417656249917140, 3.842708333674754506, 1.181850606188765695 ) ) ;
#98415 = CARTESIAN_POINT ( 'NONE',  ( 6.610000000000006537, 7.629137130509094256, 2.600000000000001421 ) ) ;
#98416 = CARTESIAN_POINT ( 'NONE',  ( -4.772106882330241717, 5.630174786549132726, -1.082531754730544860 ) ) ;
#98417 = CARTESIAN_POINT ( 'NONE',  ( 6.222909436229170588, 1.570324008046734221, -1.425282903188800798 ) ) ;
#98418 = CARTESIAN_POINT ( 'NONE',  ( -5.478903473698241378, 9.406154796041011679, -0.7216878364870338292 ) ) ;
#98419 = ORIENTED_EDGE ( 'NONE', *, *, #35037, .F. ) ;
#98421 = PRESENTATION_STYLE_ASSIGNMENT (( #210012 ) ) ;
#98420 = CARTESIAN_POINT ( 'NONE',  ( -5.695833931516914639, 6.778132687258748845, 1.082531754730549078 ) ) ;
#98422 = CARTESIAN_POINT ( 'NONE',  ( 6.491656622844908853, 6.468020902940851968, 0.7998128361456341429 ) ) ;
#98423 = CARTESIAN_POINT ( 'NONE',  ( 6.585540641348407220, -0.7802508550805787868, 1.666130356082276220 ) ) ;
#98424 = CARTESIAN_POINT ( 'NONE',  ( -0.3423093779010132898, 2.999999999999995559, 0.3423093779010045745 ) ) ;
#98425 = PLANE ( 'NONE',  #158752 ) ;
#98426 = CARTESIAN_POINT ( 'NONE',  ( 0.6823417656249899377, 3.988541667008085767, -1.181850606188754593 ) ) ;
#98427 = CARTESIAN_POINT ( 'NONE',  ( 1.839017211142121244, 0.6657927772366920571, -1.608260388387482420 ) ) ;
#98428 = CARTESIAN_POINT ( 'NONE',  ( 2.510230996824538430, 6.080353262937265413, 0.000000000000000000 ) ) ;
#98429 = CARTESIAN_POINT ( 'NONE',  ( 1.499999999999993117, 10.88541666734946389, 0.8660254037844408170 ) ) ;
#98430 = CARTESIAN_POINT ( 'NONE',  ( -1.364683531250000748, -0.1781249996585798634, 0.000000000000000000 ) ) ;
#98431 = DIRECTION ( 'NONE',  ( 0.000000000000000000, 1.000000000000000000, 0.000000000000000000 ) ) ;
#98433 = EDGE_CURVE ( 'NONE', #160735, #88459, #154440, .T. ) ;
#98432 = CARTESIAN_POINT ( 'NONE',  ( 6.016527291255574283, 1.455332790597754000, -1.598591904487467463 ) ) ;
#98434 = AXIS2_PLACEMENT_3D ( 'NONE', #9905, #208099, #160430 ) ;
#98435 = CARTESIAN_POINT ( 'NONE',  ( -2.462777459176719308, 6.024990802348131780, -0.7998128361456281477 ) ) ;
#98436 = CARTESIAN_POINT ( 'NONE',  ( -4.867013957181525186, 8.622007350113015889, 0.7216878364870458196 ) ) ;
#98437 = CARTESIAN_POINT ( 'NONE',  ( 5.612251347527116963, -0.9680786960581324596, -1.932885698521320528 ) ) ;
#98439 = ORIENTED_EDGE ( 'NONE', *, *, #201285, .T. ) ;
#98438 = CARTESIAN_POINT ( 'NONE',  ( 0.000000000000000000, 11.29999999999999893, 0.000000000000000000 ) ) ;
#98440 = CARTESIAN_POINT ( 'NONE',  ( -1.364683531250012516, 2.530208333674753174, 0.7879004041258379498 ) ) ;
#98441 = CARTESIAN_POINT ( 'NONE',  ( 5.958271952116948711, 0.7966545185628256531, 1.803378638538119860 ) ) ;
#98442 = CARTESIAN_POINT ( 'NONE',  ( 5.536419981033642301, 1.670246277208887742, -0.4650152690930853816 ) ) ;
#98443 = CIRCLE ( 'NONE', #32733, 12.00000000000000178 ) ;
#98445 = CARTESIAN_POINT ( 'NONE',  ( 2.384552795368581890, -0.3778730364575392797, -2.158588602542845347 ) ) ;
#98444 = CARTESIAN_POINT ( 'NONE',  ( -1.360316468750034868, -0.3385416663252556191, 0.7853790794158601596 ) ) ;
#98446 = CARTESIAN_POINT ( 'NONE',  ( 3.399772400530599370, 1.817812331725022101, 1.421335012277170629 ) ) ;
#98447 = CARTESIAN_POINT ( 'NONE',  ( 4.429017379523855880, 0.09708327650245980600, 2.058604088861961667 ) ) ;
#98448 = CARTESIAN_POINT ( 'NONE',  ( 0.6560686395847237229, -1.407132438187887136, 1.338565165000434876 ) ) ;
#98449 = CARTESIAN_POINT ( 'NONE',  ( -6.331294547457448019, 10.33033470543493770, 0.7216878364870458196 ) ) ;
#98450 = CARTESIAN_POINT ( 'NONE',  ( -4.817943484809863008, 6.714296380401858499, 1.599625672291263179 ) ) ;
#98451 = CARTESIAN_POINT ( 'NONE',  ( -9.497657700844911233, 15.42018113367679888, 7.334628298493624854 ) ) ;
#98452 = CARTESIAN_POINT ( 'NONE',  ( 3.849942018323779358, -1.464806807754112539, -1.533599281611098597 ) ) ;
#98453 = CARTESIAN_POINT ( 'NONE',  ( 1.740861508391436274, 2.010826320759526720, -0.1511413081683593562 ) ) ;
#98454 = CARTESIAN_POINT ( 'NONE',  ( -5.463572716182839351, 7.397254140345190798, 1.443375672974064550 ) ) ;
#98455 = CARTESIAN_POINT ( 'NONE',  ( 4.085166796624926100, -0.2132991444873769959, -2.196430506890618695 ) ) ;
#98456 = CARTESIAN_POINT ( 'NONE',  ( -3.285556943750000514, -0.2260416661887102996, -1.896917185911906500 ) ) ;
#98457 = STYLED_ITEM ( 'NONE', ( #171071 ), #180544 ) ;
#98458 = FACE_BOUND ( 'NONE', #104054, .T. ) ;
#98459 = CARTESIAN_POINT ( 'NONE',  ( -7.923814432544069142, 8.209148024248356990, 0.000000000000000000 ) ) ;
#98461 = CARTESIAN_POINT ( 'NONE',  ( 6.825078400183544503, 3.684911640780349718, 2.658296617506946458 ) ) ;
#98460 = CARTESIAN_POINT ( 'NONE',  ( -4.595593225409446703, 8.485229224138180371, -0.2149309537713070539 ) ) ;
#98462 = CARTESIAN_POINT ( 'NONE',  ( 1.445103857048098739, 8.688264192037886247, -2.625611233228243968 ) ) ;
#98463 = EDGE_LOOP ( 'NONE', ( #53247, #135894, #130382, #5595 ) ) ;
#98464 = CARTESIAN_POINT ( 'NONE',  ( 4.030192151223922714, 1.103973922444676070, -1.740068238149700353 ) ) ;
#98465 = CARTESIAN_POINT ( 'NONE',  ( 0.6801582343749987825, 1.557291667008103841, -1.178068619123876282 ) ) ;
#98466 = CARTESIAN_POINT ( 'NONE',  ( -6.240830780992103755, 6.175390754112560110, 1.040834085586084257E-14 ) ) ;
#98467 = CARTESIAN_POINT ( 'NONE',  ( 3.967448252881644155, -1.680364903119958120, -1.120146540189705497 ) ) ;
#98468 = CARTESIAN_POINT ( 'NONE',  ( 1.499999999999987121, 0.004166666666691258049, 0.8660254037844524744 ) ) ;
#98469 = CARTESIAN_POINT ( 'NONE',  ( 4.207107738942202246, 3.802713871720993399, 1.214306433183764966E-14 ) ) ;
#98470 = CARTESIAN_POINT ( 'NONE',  ( 8.229962938695207342, 9.560377169021284871, 1.199719254218462483 ) ) ;
#98471 = CARTESIAN_POINT ( 'NONE',  ( 3.362233863015654300, 0.9250742651227459312, 1.841665905919416035 ) ) ;
#98472 = CARTESIAN_POINT ( 'NONE',  ( -9.367496997608917297, 14.57669131241553728, -7.413898975919227752 ) ) ;
#98473 = CARTESIAN_POINT ( 'NONE',  ( 4.385172619016207918, 7.203452924572514959, 1.199719254218462483 ) ) ;
#98474 = DIRECTION ( 'NONE',  ( 0.000000000000000000, 1.000000000000000000, 0.000000000000000000 ) ) ;
#98475 = CARTESIAN_POINT ( 'NONE',  ( 0.7789528443887736575, 1.234723402293058214, 1.365900241759879119 ) ) ;
#98476 = CARTESIAN_POINT ( 'NONE',  ( 6.533804136697315634, -1.437950210024591780, -1.674183229976949905 ) ) ;
#98477 = CARTESIAN_POINT ( 'NONE',  ( 4.850785098639300408, 8.881276058379668825, -0.7998128361456481317 ) ) ;
#98478 = CARTESIAN_POINT ( 'NONE',  ( 1.563986776035675819, 2.129895014553784272, -0.3678597298803277793 ) ) ;
#98479 = CARTESIAN_POINT ( 'NONE',  ( -2.629918611371007575, 6.012062780000711371, 0.7216878364870317197 ) ) ;
#98480 = CARTESIAN_POINT ( 'NONE',  ( 1.499232818411553536, -0.2420282084563407654, 2.001858358113464575 ) ) ;
#98481 = CARTESIAN_POINT ( 'NONE',  ( 1.792731522490832230, -2.164186313916468762, 0.7742391241713635353 ) ) ;
#98482 = EDGE_CURVE ( 'NONE', #174327, #31992, #26402, .T. ) ;
#98483 = CARTESIAN_POINT ( 'NONE',  ( 6.518203450479811423, 5.167241622962440495, -2.437504649502885812 ) ) ;
#98484 = CARTESIAN_POINT ( 'NONE',  ( 0.6021629784135495989, -0.6261829430146518272, -1.762877433595814614 ) ) ;
#98485 =( BOUNDED_SURFACE ( )  B_SPLINE_SURFACE ( 3, 3, ( 
 ( #117612, #86115, #36280, #102357, #197723, #1631, #101288, #98132, #83970, #165231 ),
 ( #15768, #66620, #85042, #167370, #181475, #168429, #33105, #99179, #134889, #18958 ),
 ( #20025, #151130, #150059, #16824, #200896, #556, #51490, #148981, #152185, #183604 ),
 ( #132767, #2697, #69829, #147935, #198770, #135937, #48316, #182529, #81853, #213951 ),
 ( #116539, #67690, #35213, #74140, #90394, #78132, #120825, #206255, #8050, #204089 ),
 ( #104510, #138076, #105591, #87177, #139144, #170554, #157536, #190009, #153243, #103432 ),
 ( #140233, #121898, #41659, #24288, #55742, #5894, #119745, #88250, #53612, #73045 ) ),
 .UNSPECIFIED., .T., .F., .T. ) 
 B_SPLINE_SURFACE_WITH_KNOTS ( ( 4, 3, 4 ),
 ( 4, 1, 1, 1, 1, 1, 1, 4 ),
 ( 0.000000000000000000, 0.5000000000000000000, 1.000000000000000000 ),
 ( 0.000000000000000000, 0.09373397616858752945, 0.1863105892815605236, 0.2574079725677296260, 0.3612190813870841954, 0.5208938042821120717, 0.7336009914826546741, 1.000000000000000000 ),
 .UNSPECIFIED. ) 
 GEOMETRIC_REPRESENTATION_ITEM ( )  RATIONAL_B_SPLINE_SURFACE ( (
 ( 1.000000000000000000, 1.000000000000000000, 0.9999999999999997780, 1.000000000000000000, 1.000000000000000000, 1.000000000000000222, 1.000000000000000444, 1.000000000000000222, 1.000000000000000000, 1.000000000000000000),
 ( 0.3333333333333333703, 0.3333333333333333703, 0.3333333333333332593, 0.3333333333333333703, 0.3333333333333333703, 0.3333333333333334259, 0.3333333333333334814, 0.3333333333333334259, 0.3333333333333333703, 0.3333333333333333703),
 ( 0.3333333333333333703, 0.3333333333333333703, 0.3333333333333332593, 0.3333333333333333703, 0.3333333333333333703, 0.3333333333333334259, 0.3333333333333334814, 0.3333333333333334259, 0.3333333333333333703, 0.3333333333333333703),
 ( 1.000000000000000000, 1.000000000000000000, 0.9999999999999997780, 1.000000000000000000, 1.000000000000000000, 1.000000000000000222, 1.000000000000000444, 1.000000000000000222, 1.000000000000000000, 1.000000000000000000),
 ( 0.3333333333333333703, 0.3333333333333333703, 0.3333333333333332593, 0.3333333333333333703, 0.3333333333333333703, 0.3333333333333334259, 0.3333333333333334814, 0.3333333333333334259, 0.3333333333333333703, 0.3333333333333333703),
 ( 0.3333333333333333703, 0.3333333333333333703, 0.3333333333333332593, 0.3333333333333333703, 0.3333333333333333703, 0.3333333333333334259, 0.3333333333333334814, 0.3333333333333334259, 0.3333333333333333703, 0.3333333333333333703),
 ( 1.000000000000000000, 1.000000000000000000, 0.9999999999999997780, 1.000000000000000000, 1.000000000000000000, 1.000000000000000222, 1.000000000000000444, 1.000000000000000222, 1.000000000000000000, 1.000000000000000000) ) ) 
 REPRESENTATION_ITEM ( '' )  SURFACE ( )  );
#98486 = CARTESIAN_POINT ( 'NONE',  ( 4.504732016840462983, 1.524723275766314279, -1.249774587014943483 ) ) ;
#98487 = COLOUR_RGB ( '', 0.66274510, 0.83137255, 0.94901961) ;
#98488 = CARTESIAN_POINT ( 'NONE',  ( 4.241422899474024177, 0.4370803545316758743, -1.968444674787086512 ) ) ;
#98490 = CARTESIAN_POINT ( 'NONE',  ( 10.37162432432990755, 11.20257592124748136, -0.7216878364870257245 ) ) ;
#98489 = CARTESIAN_POINT ( 'NONE',  ( -1.364683531250012516, 2.530208333674753174, 0.7879004041258379498 ) ) ;
#98492 = CARTESIAN_POINT ( 'NONE',  ( 6.481095854277318935, -0.1012916397761880333, -2.103764601514758414 ) ) ;
#98491 = CARTESIAN_POINT ( 'NONE',  ( -7.562750758324527922, 7.717630727667075696, 1.040834085586084257E-14 ) ) ;
#98493 = CARTESIAN_POINT ( 'NONE',  ( 4.896967953096117654, 0.3505727482827174502, 2.040303948762006492 ) ) ;
#98494 = CARTESIAN_POINT ( 'NONE',  ( 6.765682348419287173, 7.852049813699357728, 1.199719254218462483 ) ) ;
#98495 = CARTESIAN_POINT ( 'NONE',  ( -6.847031270101295419, 7.946956888995021728, -1.199719254218446718 ) ) ;
#98496 = CARTESIAN_POINT ( 'NONE',  ( 6.539320575229260690, 0.5855366995804256458, 2.057005297509428399 ) ) ;
#98497 = CARTESIAN_POINT ( 'NONE',  ( 4.746356070053968423, 1.034628734442550879, -1.734499354260822468 ) ) ;
#98498 = CARTESIAN_POINT ( 'NONE',  ( -1.500000000000001332, -0.8187499993171781787, 0.000000000000000000 ) ) ;
#98499 = CARTESIAN_POINT ( 'NONE',  ( 2.877863741784414842, 2.191074257732894548, -0.7245186886237849899 ) ) ;
#98501 = ADVANCED_FACE ( 'NONE', ( #91129, #153982 ), #137744, .F. ) ;
#98500 = AXIS2_PLACEMENT_3D ( 'NONE', #114360, #160911, #12506 ) ;
#98502 = CARTESIAN_POINT ( 'NONE',  ( 1.534110023759263308, 1.225272132802219360, 1.659075958507538973 ) ) ;
#98503 = CARTESIAN_POINT ( 'NONE',  ( 8.134528978519385944, 8.592631351135175066, -0.7216878364870267237 ) ) ;
#98504 = CARTESIAN_POINT ( 'NONE',  ( 7.042534447655770080, 7.180988041878682004, -0.7998128361456341429 ) ) ;
#98505 = CARTESIAN_POINT ( 'NONE',  ( 6.073126464278658432, 6.050012061272033392, 0.000000000000000000 ) ) ;
#98506 = CARTESIAN_POINT ( 'NONE',  ( -0.6823417656250246877, 0.3635416670080895973, 1.181850606188755259 ) ) ;
#98507 = CARTESIAN_POINT ( 'NONE',  ( 4.583538449871731757, 7.505156070562471804, 1.199719254218451159 ) ) ;
#98508 = CARTESIAN_POINT ( 'NONE',  ( 6.819388077549422889, 8.018669514304889390, -1.082531754730543971 ) ) ;
#98510 = CARTESIAN_POINT ( 'NONE',  ( -4.021726917867474604, 3.853862851527702027, -2.500000000000000444 ) ) ;
#98509 = CARTESIAN_POINT ( 'NONE',  ( 3.701788104937975721, -1.641978770885927252, -1.420606208986204155 ) ) ;
#98511 = CARTESIAN_POINT ( 'NONE',  ( -1.496707356397872557, -0.8887487162373141070, -2.932808216565309767 ) ) ;
#98513 = CARTESIAN_POINT ( 'NONE',  ( 2.893917256732419396, -0.5369380550670297403, -1.761199466696103499 ) ) ;
#98512 = CARTESIAN_POINT ( 'NONE',  ( -5.287316719649550301, 5.270883715786984780, 0.7216878364870317197 ) ) ;
#98514 = CARTESIAN_POINT ( 'NONE',  ( -1.364683531250012516, 4.988541667008084879, -0.7879004041258300672 ) ) ;
#98515 = CARTESIAN_POINT ( 'NONE',  ( 4.528971853086540378, -2.003544689622422936, 0.8885388601788182239 ) ) ;
#98516 = CARTESIAN_POINT ( 'NONE',  ( 7.130034971365033059, 14.53133652881233573, 9.655242375037330405 ) ) ;
#98517 = CARTESIAN_POINT ( 'NONE',  ( 5.928679764299940480, 2.178688510132809064, 0.6099592146414765104 ) ) ;
#98518 = CARTESIAN_POINT ( 'NONE',  ( -5.176859992674639699, 6.655076503622660233, -1.423794717725470171 ) ) ;
#98519 = CARTESIAN_POINT ( 'NONE',  ( 4.827426732796687325, 8.217478009653898852, -0.9130428269800896501 ) ) ;
#98520 = CARTESIAN_POINT ( 'NONE',  ( -5.112833325684908559, 8.018703742390766109, -1.082531754730549967 ) ) ;
#98521 = CARTESIAN_POINT ( 'NONE',  ( 4.340018570150304456, 6.156717313299049366, -1.443375672974068769 ) ) ;
#98522 = CARTESIAN_POINT ( 'NONE',  ( 6.432837487460982828, 0.1759369732093341021, 1.760927613267867953 ) ) ;
#98523 = CARTESIAN_POINT ( 'NONE',  ( 3.651042523073198431, 0.2976914719170896118, 1.990856138409332843 ) ) ;
#98524 = B_SPLINE_CURVE_WITH_KNOTS ( 'NONE', 3,
 ( #193060, #161657, #44713, #110820, #202641, #134506, #166980, #84649 ),
 .UNSPECIFIED., .F., .F.,
 ( 4, 2, 2, 4 ),
 ( 0.000000000000000000, 0.0004845678193365327946, 0.0009691356386730655892, 0.001938271277346135515 ),
 .UNSPECIFIED. ) ;
#98525 = CARTESIAN_POINT ( 'NONE',  ( 6.608709811657416999, 9.797579649320619311, -1.199719254218440723 ) ) ;
#98526 = CARTESIAN_POINT ( 'NONE',  ( 3.153452123856602896, -1.720715631468725526, -1.213874241417127298 ) ) ;
#98527 = CARTESIAN_POINT ( 'NONE',  ( 1.827608144986846206, 0.7312883373844185630, -1.770730004348388453 ) ) ;
#98529 = EDGE_CURVE ( 'NONE', #71497, #85365, #56478, .T. ) ;
#98528 = CARTESIAN_POINT ( 'NONE',  ( 4.359110081993588182, 5.044382169536003602, -1.199719254218452047 ) ) ;
#98530 = CARTESIAN_POINT ( 'NONE',  ( 3.420317264040674932, 0.8831254867164675115, 1.760515127234823840 ) ) ;
#98531 = CARTESIAN_POINT ( 'NONE',  ( 0.5318453760667535279, 0.9654296485097979552, -1.602142582367314549 ) ) ;
#98532 = CARTESIAN_POINT ( 'NONE',  ( 1.240593047436115759, -1.913272810121857237, -0.4332019784048374289 ) ) ;
#98534 = ORIENTED_EDGE ( 'NONE', *, *, #77512, .T. ) ;
#98533 = CARTESIAN_POINT ( 'NONE',  ( 0.6856317642073318508, 1.842354612247762091, -0.5124485439033445999 ) ) ;
#98535 = CARTESIAN_POINT ( 'NONE',  ( 3.877268743828258479, 7.467304601200877023, 0.7216878364870298324 ) ) ;
#98536 = CARTESIAN_POINT ( 'NONE',  ( -1.364683531250014514, 0.5510416670080878765, -0.7879004041258289570 ) ) ;
#98537 = CARTESIAN_POINT ( 'NONE',  ( 5.910993886665249164, 1.650546521282238110, 0.8803886038859505270 ) ) ;
#98538 = CARTESIAN_POINT ( 'NONE',  ( 9.622536337397022521, 12.24937836509514710, 1.599625672291281386 ) ) ;
#98539 = CARTESIAN_POINT ( 'NONE',  ( -4.137364601623837679, 8.820716007809833670, 0.7750000000000002442 ) ) ;
#98540 = LINE ( 'NONE', #181894, #147951 ) ;
#98541 = DIRECTION ( 'NONE',  ( -0.000000000000000000, -0.000000000000000000, 1.000000000000000000 ) ) ;
#98542 = CARTESIAN_POINT ( 'NONE',  ( 1.240778115703184303, -2.019486815914430355, -0.4554155650244652853 ) ) ;
#98543 = CARTESIAN_POINT ( 'NONE',  ( -0.7500000000000215383, 1.191666666666688190, 1.299038105676659116 ) ) ;
#98544 = CARTESIAN_POINT ( 'NONE',  ( 7.935599982700328958, 8.152621489438862667, 0.7998128361456481317 ) ) ;
#98545 = CARTESIAN_POINT ( 'NONE',  ( -8.178592977541617515, 10.56477777859713463, 1.599625672291295375 ) ) ;
#98546 = CARTESIAN_POINT ( 'NONE',  ( 3.881377115262159894, 7.750300077773022878, 0.7998128361456271485 ) ) ;
#98548 = EDGE_CURVE ( 'NONE', #214172, #180436, #33355, .T. ) ;
#98547 = CARTESIAN_POINT ( 'NONE',  ( 5.936213163351176547, -1.177816969253571155, -1.763093882214488817 ) ) ;
#98549 = CARTESIAN_POINT ( 'NONE',  ( 5.032011289327418702, 5.899709921417326974, 1.199719254218452935 ) ) ;
#98550 = CARTESIAN_POINT ( 'NONE',  ( -1.364683531250000748, 1.509375000341421691, 0.000000000000000000 ) ) ;
#98551 = VERTEX_POINT ( 'NONE', #172367 ) ;
#98552 = ADVANCED_FACE ( 'NONE', ( #190722, #156121 ), #138808, .F. ) ;
#98553 = CARTESIAN_POINT ( 'NONE',  ( 0.7499999999999885647, 3.066666666666689522, -1.299038105676658228 ) ) ;
#98555 = CARTESIAN_POINT ( 'NONE',  ( 3.388648328411762556, 6.040841252200647382, 1.199719254218462483 ) ) ;
#98554 = CARTESIAN_POINT ( 'NONE',  ( 6.021922112293466967, 1.933069186966931863, -0.3339256516061983038 ) ) ;
#98556 = CARTESIAN_POINT ( 'NONE',  ( 4.323592178502837058, -1.495822217463145476, 1.351947993609707632 ) ) ;
#98557 = CARTESIAN_POINT ( 'NONE',  ( 3.221808243886138179, 0.8566008913209141040, -1.713579649959365403 ) ) ;
#98558 = CARTESIAN_POINT ( 'NONE',  ( 1.500000000000005329, 4.535416667349485564, 0.8660254037844431485 ) ) ;
#98559 = CARTESIAN_POINT ( 'NONE',  ( 1.242012060539962492, 2.189267750446591609, 0.1026977899005257211 ) ) ;
#98560 = CARTESIAN_POINT ( 'NONE',  ( -1.264911064067355984, 3.850000000000006306, -0.5000000000000004441 ) ) ;
#98561 = CARTESIAN_POINT ( 'NONE',  ( 3.286256049847174676, -1.842268013383094427, -0.3231441395407097517 ) ) ;
#98562 = CARTESIAN_POINT ( 'NONE',  ( 0.7499999999999885647, -0.7354166659838470288, 1.299038105676657340 ) ) ;
#98563 = CARTESIAN_POINT ( 'NONE',  ( -6.157374318900681764, 10.33535380535947290, 0.7998128361456481317 ) ) ;
#98565 = CARTESIAN_POINT ( 'NONE',  ( 5.114917985578482096, 0.1569784262732084601, 2.111484538518786813 ) ) ;
#98564 = CARTESIAN_POINT ( 'NONE',  ( -4.609409038966248318, 5.440360635957812718, -1.082531754730544860 ) ) ;
#98566 = CYLINDRICAL_SURFACE ( 'NONE', #177133, 0.7499999999999997780 ) ;
#98567 = CARTESIAN_POINT ( 'NONE',  ( 6.742638474511262636, -2.029596885996234334, -0.4079607620106340260 ) ) ;
#98569 = CARTESIAN_POINT ( 'NONE',  ( -4.658966671999400511, 7.502878459571090453, -1.089694788465228159 ) ) ;
#98568 = CARTESIAN_POINT ( 'NONE',  ( 1.786781105396139102, 1.817558579408204089, -1.033184933219722934 ) ) ;
#98571 = ORIENTED_EDGE ( 'NONE', *, *, #193499, .T. ) ;
#98570 = CARTESIAN_POINT ( 'NONE',  ( 1.113767329461469835, -0.7700024601069790364, -1.543427451845545084 ) ) ;
#98572 = CARTESIAN_POINT ( 'NONE',  ( 7.772902139336337335, 7.962807338847539107, 0.7998128361456341429 ) ) ;
#98573 = CARTESIAN_POINT ( 'NONE',  ( -0.4019237886466933696, 12.08258545099816850, 1.500000000000005995 ) ) ;
#98574 = FACE_OUTER_BOUND ( 'NONE', #67858, .T. ) ;
#98575 = CARTESIAN_POINT ( 'NONE',  ( -0.06258739273032881689, -9.383611379567486921, 9.609645335164882951 ) ) ;
#98577 = CARTESIAN_POINT ( 'NONE',  ( 8.175203438916005538, 11.52119253116861586, -1.082531754730543083 ) ) ;
#98576 = CARTESIAN_POINT ( 'NONE',  ( 6.388916700537700777, 8.476822122092563916, 1.599625672291281386 ) ) ;
#98579 =( BOUNDED_CURVE ( )  B_SPLINE_CURVE ( 2, ( #187581, #205966, #10956, #109625, #175629, #39208, #105299 ),
 .UNSPECIFIED., .F., .T. ) 
 B_SPLINE_CURVE_WITH_KNOTS ( ( 3, 2, 2, 3 ),
 ( 0.1750000000000002942, 0.1791666666666668351, 0.1833333333333333759, 0.1874999999999999167 ),
 .UNSPECIFIED. ) 
 CURVE ( )  GEOMETRIC_REPRESENTATION_ITEM ( )  RATIONAL_B_SPLINE_CURVE ( ( 0.9999999999999902300, 0.8660254037844484776, 1.000000000000000000, 0.8660254037844387076, 1.000000000000000000, 0.8660254037844413721, 0.9999999999999973355 ) ) 
 REPRESENTATION_ITEM ( '' )  );
#98578 = CARTESIAN_POINT ( 'NONE',  ( -2.995508107964761191, 6.411541510041463887, -0.7147908198718248007 ) ) ;
#98581 = CARTESIAN_POINT ( 'NONE',  ( 2.033590728242135715, -1.756817081591253604, 0.4409998202260062006 ) ) ;
#98580 = CARTESIAN_POINT ( 'NONE',  ( 4.532168488718122390, 8.509556680138327778, 0.7998128361456271485 ) ) ;
#98582 = CARTESIAN_POINT ( 'NONE',  ( -8.193204901359996128, 8.453160561208463264, 1.040834085586084257E-14 ) ) ;
#98583 = CARTESIAN_POINT ( 'NONE',  ( 3.194917754314666514, 6.879154480009089134, 0.7998128361456321445 ) ) ;
#98584 = CARTESIAN_POINT ( 'NONE',  ( -6.068414747559345734, 7.047288584480712714, 1.012934185448462143 ) ) ;
#98585 = CARTESIAN_POINT ( 'NONE',  ( 6.900173834712277632, 7.014900660111269559, -0.7998128361456341429 ) ) ;
#98586 = DIRECTION ( 'NONE',  ( 0.000000000000000000, -1.000000000000000000, 0.000000000000000000 ) ) ;
#98587 = CARTESIAN_POINT ( 'NONE',  ( -15.75000000000000000, 12.69999999999998153, 3.199999999999997957 ) ) ;
#98588 = CARTESIAN_POINT ( 'NONE',  ( 3.995055777641403516, 7.602996552368006533, -0.05680687033517151097 ) ) ;
#98589 = CARTESIAN_POINT ( 'NONE',  ( 9.788623719386617239, 11.48277776311499387, -1.082531754730537088 ) ) ;
#98590 = CARTESIAN_POINT ( 'NONE',  ( 3.261990205869094162, -1.859054838292145240, 0.08865997893938745711 ) ) ;
#98591 = CARTESIAN_POINT ( 'NONE',  ( 0.05214973123207015254, -1.250902960675448483, 1.450897702916327248 ) ) ;
#98592 = CARTESIAN_POINT ( 'NONE',  ( 0.08272424614634911466, -0.1293432359340887239, -1.795996506534849324 ) ) ;
#98593 = CIRCLE ( 'NONE', #109016, 9.999999999999996447 ) ;
#98594 = LINE ( 'NONE', #102581, #187440 ) ;
#98595 = DIRECTION ( 'NONE',  ( 0.6507913734559640506, -0.7592566023653004592, 0.000000000000000000 ) ) ;
#98596 = CARTESIAN_POINT ( 'NONE',  ( 4.601545839464173504, 8.365386937211251706, 0.1680730238927778675 ) ) ;
#98597 = CARTESIAN_POINT ( 'NONE',  ( -11.48806469435255373, 11.33089772872447121, 3.468902948106700634 ) ) ;
#98598 = CARTESIAN_POINT ( 'NONE',  ( -2.968872451712654126, 6.407508927065978632, 1.040834085586084257E-14 ) ) ;
#98599 = TOROIDAL_SURFACE ( 'NONE', #43257, 1.924999999999999822, 0.1000000000000000056 ) ;
#98600 = CARTESIAN_POINT ( 'NONE',  ( 9.422553571817644524, 10.09532670998316384, 0.000000000000000000 ) ) ;
#98601 = CARTESIAN_POINT ( 'NONE',  ( 4.381674357853755808, -1.885861198437089437, 0.5677522405800348171 ) ) ;
#98602 = CARTESIAN_POINT ( 'NONE',  ( 2.016421337698256711, -2.119947128278206971, 0.05498460973795551987 ) ) ;
#98603 = CARTESIAN_POINT ( 'NONE',  ( -5.096975683733680818, 8.033889833409558534, -1.199719254218452047 ) ) ;
#98604 = DIRECTION ( 'NONE',  ( 1.039099362110107450E-15, 1.000000000000000000, -4.583713267641621330E-32 ) ) ;
#98605 = CARTESIAN_POINT ( 'NONE',  ( 1.874158809982179319, 3.299964346911585356, -0.3999999999999993006 ) ) ;
#98606 = CARTESIAN_POINT ( 'NONE',  ( 6.369083545433415594, 2.098215621258665564, -0.6323776016037768732 ) ) ;
#98607 = PRESENTATION_STYLE_ASSIGNMENT (( #128005 ) ) ;
#98608 = CARTESIAN_POINT ( 'NONE',  ( 3.997031241255116552, 1.627850364849007248, -1.029807644849835890 ) ) ;
#98609 = CARTESIAN_POINT ( 'NONE',  ( -7.366157530926372488, 7.488271962369228874, -0.7998128361456291469 ) ) ;
#98610 = CARTESIAN_POINT ( 'NONE',  ( 0.4986989427119004059, 1.520756344202650601, -1.009667857431728599 ) ) ;
#98611 = CARTESIAN_POINT ( 'NONE',  ( 0.5576012004645107822, -1.866542136390366036, -1.177153700605698461 ) ) ;
#98612 = PRESENTATION_STYLE_ASSIGNMENT (( #164673 ) ) ;
#98613 = ORIENTED_EDGE ( 'NONE', *, *, #72903, .T. ) ;
#98614 = ORIENTED_EDGE ( 'NONE', *, *, #128928, .F. ) ;
#98615 = CARTESIAN_POINT ( 'NONE',  ( 6.368014371105396698, -1.954979222910321557, 0.2374047605521299453 ) ) ;
#98616 = CARTESIAN_POINT ( 'NONE',  ( 2.015084816950295732, -1.883260942463622856, 0.4737542896416384597 ) ) ;
#98617 = CARTESIAN_POINT ( 'NONE',  ( 6.450549897212096262, 1.577601184540510681, 1.671684124095852653 ) ) ;
#98619 = CARTESIAN_POINT ( 'NONE',  ( 5.858217239054963166, -1.861131630269092341, -0.001575894832107904492 ) ) ;
#98618 = CARTESIAN_POINT ( 'NONE',  ( -7.282664789195997912, 8.525472337930658284, 1.199719254218452047 ) ) ;
#98620 = CARTESIAN_POINT ( 'NONE',  ( 4.877901405866606588, 8.912911750144889567, 0.7998128361456341429 ) ) ;
#98621 = DIRECTION ( 'NONE',  ( 0.000000000000000000, 1.000000000000000000, 0.000000000000000000 ) ) ;
#98622 = SURFACE_STYLE_FILL_AREA ( #32546 ) ;
#98623 = CARTESIAN_POINT ( 'NONE',  ( -7.040761844198392794, 7.108643661186573759, -0.7998128361456291469 ) ) ;
#98624 = EDGE_CURVE ( 'NONE', #197365, #159860, #133752, .T. ) ;
#98625 = CARTESIAN_POINT ( 'NONE',  ( -3.363831509966363598, 5.978201624052440266, -1.082531754730548412 ) ) ;
#98626 = CARTESIAN_POINT ( 'NONE',  ( 1.242012060539962492, 2.189267750446591609, 0.1026977899005257211 ) ) ;
#98627 = CARTESIAN_POINT ( 'NONE',  ( 3.551873057100274789, 7.087676300018221021, 0.7216878364870298324 ) ) ;
#98628 = CARTESIAN_POINT ( 'NONE',  ( 10.99387514841223279, -6.699757570937918238, -0.3793797362573342880 ) ) ;
#98629 = CARTESIAN_POINT ( 'NONE',  ( 3.615248252392856632, 3.576401842564421951, -2.500000000000000444 ) ) ;
#98630 = CARTESIAN_POINT ( 'NONE',  ( 1.928079105319381314, 1.052063804484974385, -1.491885150056403431 ) ) ;
#98631 = CARTESIAN_POINT ( 'NONE',  ( -3.704402285031864306, 5.344888637335695414, -1.599625672291256295 ) ) ;
#98632 = FACE_OUTER_BOUND ( 'NONE', #141495, .T. ) ;
#98633 = CARTESIAN_POINT ( 'NONE',  ( 6.509000000000035868, 7.629137130509092479, 2.600000000000000977 ) ) ;
#98634 = CIRCLE ( 'NONE', #91699, 0.05000000000000009298 ) ;
#98635 = CARTESIAN_POINT ( 'NONE',  ( 0.4347878448724571410, 3.060161718936325492, 0.4204403343208824584 ) ) ;
#98636 = CARTESIAN_POINT ( 'NONE',  ( 6.410779360540267646, 1.349177972556347971, -1.230185023894624141 ) ) ;
#98637 = CARTESIAN_POINT ( 'NONE',  ( 4.733228419949464971, 0.004064956161661801778, -1.961936380062332397 ) ) ;
#98638 = CARTESIAN_POINT ( 'NONE',  ( -7.690499447449645309, 9.995335326823163058, 1.599625672291295375 ) ) ;
#98639 = CARTESIAN_POINT ( 'NONE',  ( 5.612185521052973414, 8.634967976948757951, -1.199719254218440723 ) ) ;
#98640 = CARTESIAN_POINT ( 'NONE',  ( 4.653055333535057514, 0.3633016933833124185, 2.088981207656291250 ) ) ;
#98641 = CARTESIAN_POINT ( 'NONE',  ( 4.054362073078698891, -1.623213109359676443, 1.472610181411204922 ) ) ;
#98642 = CARTESIAN_POINT ( 'NONE',  ( -7.309817376062285099, 11.67987070538135264, 0.000000000000000000 ) ) ;
#98643 = PRESENTATION_LAYER_ASSIGNMENT (  '', '', ( #192010 ) ) ;
#98644 = FACE_OUTER_BOUND ( 'NONE', #86731, .T. ) ;
#98645 = CARTESIAN_POINT ( 'NONE',  ( 2.413015750098276513, -1.603085927076562500, 1.310038033242977518 ) ) ;
#98647 = CARTESIAN_POINT ( 'NONE',  ( -1.364683531250000748, 0.3218750003414205807, 0.000000000000000000 ) ) ;
#98646 = DIRECTION ( 'NONE',  ( -0.000000000000000000, -1.000000000000000000, -0.000000000000000000 ) ) ;
#98648 = ORIENTED_EDGE ( 'NONE', *, *, #173816, .T. ) ;
#98649 = CARTESIAN_POINT ( 'NONE',  ( 3.041888879667261403, -1.739239095176773775, 1.503071639953108773 ) ) ;
#98650 = CARTESIAN_POINT ( 'NONE',  ( 7.565086526745395723, 10.80938946696957004, -1.082531754730543083 ) ) ;
#98652 = CARTESIAN_POINT ( 'NONE',  ( 0.000000000000000000, -2.996874999522043392, -3.793834371823813001 ) ) ;
#98651 = CARTESIAN_POINT ( 'NONE',  ( 6.292392690518195941, 8.434487120394948079, -1.443375672974078761 ) ) ;
#98653 = CARTESIAN_POINT ( 'NONE',  ( 6.720655732516647163, 3.705577233864749687, 2.340827588962008488 ) ) ;
#98654 = FACE_OUTER_BOUND ( 'NONE', #158264, .T. ) ;
#98655 = CARTESIAN_POINT ( 'NONE',  ( -1.326716514427061987E-15, 2.999999999999988454, -1.225000000000003864 ) ) ;
#98656 = EDGE_LOOP ( 'NONE', ( #112893, #99997, #137562, #211475, #175052, #207137, #44422, #168351, #4127, #147203, #164969, #20315, #93165, #171725, #13151, #155851, #1654, #128728, #162147, #225, #11181, #156327, #129307, #139585, #69938, #182745, #41904, #40763 ) ) ;
#98657 = CARTESIAN_POINT ( 'NONE',  ( -0.1981138333789616013, -9.280569609800540576, 9.498748750704498534 ) ) ;
#98658 = EDGE_CURVE ( 'NONE', #113953, #198880, #108495, .T. ) ;
#98659 = CARTESIAN_POINT ( 'NONE',  ( 4.535362393419643645, -0.08824616237496611670, 1.910463848342447202 ) ) ;
#98660 = LINE ( 'NONE', #212381, #162253 ) ;
#98661 = CARTESIAN_POINT ( 'NONE',  ( 4.981344092214620822, 1.608381032133517019, -0.6233497484429885160 ) ) ;
#98662 = CARTESIAN_POINT ( 'NONE',  ( 3.098842478760281516, 1.825076540557273974, 0.8578426345753201732 ) ) ;
#98663 = CARTESIAN_POINT ( 'NONE',  ( 5.467524615204178318, -2.242144116172717361, -0.5062228086629757540 ) ) ;
#98664 = CARTESIAN_POINT ( 'NONE',  ( -1.500000000000015099, 9.729166666666671404, -0.8660254037844309360 ) ) ;
#98665 = CARTESIAN_POINT ( 'NONE',  ( 1.137671262558290763, -1.993743905544292927, 0.9465009238469668240 ) ) ;
#98666 = CARTESIAN_POINT ( 'NONE',  ( -5.045042558060949034, 6.018876084893449274, 1.082531754730549078 ) ) ;
#98667 = CARTESIAN_POINT ( 'NONE',  ( 6.151566388294868126, 0.5118450565497618676, -1.694058711534670358 ) ) ;
#98669 = CARTESIAN_POINT ( 'NONE',  ( 2.098001248608129199, -2.291667096838309270, 0.05881920129262825647 ) ) ;
#98668 = CARTESIAN_POINT ( 'NONE',  ( 7.198453214212898743, 7.362893269528701268, 0.7998128361456291469 ) ) ;
#98670 = CARTESIAN_POINT ( 'NONE',  ( 6.421814705521882161, 1.055779539018763646, -1.508159643570324393 ) ) ;
#98671 = CARTESIAN_POINT ( 'NONE',  ( -6.071018923869249129, 10.30488218781460574, 0.7998128361456291469 ) ) ;
#98672 = CARTESIAN_POINT ( 'NONE',  ( -3.871735385154307263, 6.674719161725423788, -1.199719254218450271 ) ) ;
#98673 = CARTESIAN_POINT ( 'NONE',  ( -1.360316468750014884, 0.1927083336747308917, 0.7853790794158901356 ) ) ;
#98674 = CARTESIAN_POINT ( 'NONE',  ( -11.41381678389398502, 12.57120581758917055, 3.704697885617667996 ) ) ;
#98675 = CARTESIAN_POINT ( 'NONE',  ( 6.654741963219192868, -0.5482099483974657295, -1.996413779700876301 ) ) ;
#98676 = CARTESIAN_POINT ( 'NONE',  ( 2.466030083290056130, -1.032479112849067793, 1.731996155473938259 ) ) ;
#98677 = CARTESIAN_POINT ( 'NONE',  ( 0.7499999999999885647, 0.2645833340161538039, 1.299038105676657340 ) ) ;
#98678 = CARTESIAN_POINT ( 'NONE',  ( 5.865835041973252117, 1.897565194821029033, -0.3318024074076031948 ) ) ;
#98679 = CARTESIAN_POINT ( 'NONE',  ( -0.6823417656250003738, 12.40104166700806232, 1.181850606188754593 ) ) ;
#98680 = CARTESIAN_POINT ( 'NONE',  ( 2.162617739553638785, 2.221014589654236371, 0.04931172913892957477 ) ) ;
#98681 = ORIENTED_EDGE ( 'NONE', *, *, #85583, .T. ) ;
#98682 = CARTESIAN_POINT ( 'NONE',  ( 6.745710774231037377, -7.818797203689475950, 6.689804758640298665 ) ) ;
#98683 = CARTESIAN_POINT ( 'NONE',  ( -6.116136693096207999, 6.308116694799911883, 0.7216878364870257245 ) ) ;
#98684 = CARTESIAN_POINT ( 'NONE',  ( 9.915090410295563927, 10.46202698829998567, -0.7998128361456281477 ) ) ;
#98685 = DIRECTION ( 'NONE',  ( 1.000000000000000000, -6.165071176878339540E-16, 0.000000000000000000 ) ) ;
#98686 = CARTESIAN_POINT ( 'NONE',  ( -10.56536251450128994, 9.840389374505219777, 3.404319718479181578 ) ) ;
#98687 = CARTESIAN_POINT ( 'NONE',  ( 5.038483826543846078, -1.489082695810162837, 0.9007512145987550678 ) ) ;
#98688 = CARTESIAN_POINT ( 'NONE',  ( 3.683996026499200660, -1.166640140252427793, -1.577160851978461009 ) ) ;
#98690 = CARTESIAN_POINT ( 'NONE',  ( -8.026063749610063525, 8.466088584074293877, -0.7216878364870278340 ) ) ;
#98689 = CARTESIAN_POINT ( 'NONE',  ( 3.497113557321089861, 6.167384019261527683, -1.199719254218446718 ) ) ;
#98691 = EDGE_CURVE ( 'NONE', #90168, #176780, #158543, .T. ) ;
#98692 =( NAMED_UNIT ( * ) SI_UNIT ( $, .STERADIAN. ) SOLID_ANGLE_UNIT ( ) );
#98693 = CARTESIAN_POINT ( 'NONE',  ( 4.552213317786341307, 2.262020173471789963, -0.04951151886351152359 ) ) ;
#98694 = CARTESIAN_POINT ( 'NONE',  ( 1.416547059616825699, 0.8341270235591256021, 1.886661834507087798 ) ) ;
#98695 = CARTESIAN_POINT ( 'NONE',  ( -7.393273838153706201, 7.519907654134449615, 0.7998128361456341429 ) ) ;
#98696 = CARTESIAN_POINT ( 'NONE',  ( -3.972175818679615222, 4.696921878956699103, 1.082531754730558626 ) ) ;
#98697 = CARTESIAN_POINT ( 'NONE',  ( 1.885968558009487595, 1.560753693757486849, 1.638220756346415508 ) ) ;
#98698 = ORIENTED_EDGE ( 'NONE', *, *, #188812, .F. ) ;
#98699 = CARTESIAN_POINT ( 'NONE',  ( -1.500000000000013101, -0.04791666598384902026, 0.8660254037844403729 ) ) ;
#98700 = CARTESIAN_POINT ( 'NONE',  ( 2.213927045526514537, -0.8776910013945339317, -1.651823421649289081 ) ) ;
#98701 = CARTESIAN_POINT ( 'NONE',  ( 1.582203977811939000, -0.5845794355729941882, 1.632800797419992955 ) ) ;
#98702 = CARTESIAN_POINT ( 'NONE',  ( 5.302338810847701644, 1.659911028786088538, -1.431018553749352051 ) ) ;
#98703 = CARTESIAN_POINT ( 'NONE',  ( 6.633790087849154027, -1.500048720590658302, -1.753619728580549708 ) ) ;
#98704 = CARTESIAN_POINT ( 'NONE',  ( 0.9716393833266089297, 1.986344416073432484, -0.5490401152750885583 ) ) ;
#98705 = CARTESIAN_POINT ( 'NONE',  ( 4.171774378167571129, -1.117019396711134371, 1.588354668226848565 ) ) ;
#98706 = CARTESIAN_POINT ( 'NONE',  ( -2.779058300676974014, 6.186059084191009916, -0.7216878364870257245 ) ) ;
#98707 = B_SPLINE_SURFACE_WITH_KNOTS ( 'NONE', 1, 3, ( 
 ( #164749, #99749, #18481, #53126, #117125, #118196, #16340, #69351, #4345, #83486, #67215, #169010, #17402, #150649, #82421, #151714, #2210, #68287, #48878, #1152, #101882, #36866, #135461, #134420, #33675, #184184, #86695, #19549, #3284, #165819, #102950, #70412, #197239, #149569, #114996, #133350, #148510, #77, #66142, #198292, #10503, #202550, #157853, #44104, #127566, #11576, #43047, #124360, #126485, #111289, #92860, #191381, #190317, #176232, #110224, #109160, #41975, #27834, #108086, #71487, #174115, #93930, #193535, #142688, #61403, #91796, #58201, #120340, #159971, #161040, #12635, #192449, #25688, #9447, #75518, #141630, #37951, #137600, #207639, #136530, #59257, #54200, #158907, #125415, #26759, #77646, #45177, #186316, #175172, #76576, #177295, #104023, #143768, #209762, #208698, #28909, #60325, #94994, #170071, #21657, #87763, #153839, #5409, #203617, #32103, #64600, #66684, #13705, #29977, #131778, #130741, #196734, #128628, #179432, #198835, #163181, #162115, #181534, #166358, #211901, #82968, #180484, #147997, #96062, #48375, #114487, #79778, #98188, #164236, #129693, #100291, #210840, #80856, #15824, #145890, #149041, #62466, #132831, #197781, #81909, #194595, #146947, #214007, #14766, #65629, #49419, #115539, #33162, #46239, #50480, #99243, #112356, #195676, #165292, #616, #212962, #16886, #178369, #116601, #78706, #31053, #182595, #63538, #47312, #34218, #113426, #97129, #144832, #17948, #67751, #84035, #1697, #150124, #133901, #199908, #51554, #117679, #183672, #35275, #101353, #24834, #90933, #57350, #190531, #191592, #189477, #193734, #74667, #93070, #25897, #60536, #61607, #140770, #43253, #77853, #42187, #108302, #208904, #173253, #126696, #156999, #8586, #192657, #10713, #206783, #58417, #143977, #45379, #159112, #124570, #174322, #141843, #28047, #209968, #107232, #26962, #11780, #127779, #176435, #44310, #125631, #109372, #111496, #9652, #158066, #41120, #76782, #92008, #177502, #75730, #29115, #95200, #207848, #175379, #142904, #94141, #7508, #73590, #59474, #139692, #110433, #205714, #160179, #123513, #99844, #2301 ),
 ( #64150, #183215, #118284, #197331, #181086, #68377, #131337, #16433, #146489, #51092, #82511, #182136, #162727, #115090, #1242, #84651, #34819, #167, #81462, #83580, #134508, #50024, #148598, #147540, #133442, #67302, #66234, #213561, #199449, #65183, #31656, #48973, #117216, #150740, #165909, #18573, #32704, #196281, #116148, #100895, #166983, #200512, #149662, #132383, #198383, #52157, #98786, #164841, #130292, #17493, #97733, #184270, #163790, #96677, #14298, #15369, #33766, #80393, #212509, #47928, #114041, #180034, #172311, #88939, #23900, #22824, #90006, #57490, #21749, #54293, #187478, #136618, #85713, #156060, #38042, #185338, #152855, #137686, #204771, #186405, #87857, #151800, #7648, #36962, #138753, #3375, #120430, #205858, #35894, #4433, #72657, #139830, #104112, #70502, #135550, #123651, #101971, #69442, #168039, #202644, #73733, #153929, #201575, #53220, #103042, #19642, #154992, #119351, #170160, #169096, #6577, #39108, #20695, #86786, #5497, #71578, #203707, #55354, #106291, #121505, #105192, #171229, #56426, #122585, #188547, #40177, #159245, #126839, #44455, #143045, #42325, #206923, #58552, #24973, #158203, #10845, #157136, #161400, #108441, #60676, #207986, #28184, #29258, #174461, #76919, #45522, #9792, #75867, #176573, #140910, #94279, #124706, #190665, #160320, #192796, #26037, #92150, #111638, #12984, #110571, #141974, #59614, #109509, #210113, #177649, #144119, #125771, #27106, #91076, #95350, #191732, #77996, #8728, #43388, #145176, #189613, #175517, #11924, #79058, #93213, #209040, #74809, #62807, #211181, #61753, #41259, #127921, #107369, #193873, #173390, #14038, #130034, #2040, #181873, #162462, #64934, #46584, #99582, #132120, #166717, #196025, #178713, #84393, #47661, #113772, #199181, #112703, #179775, #194948, #80124, #150480, #67044, #128968, #98518, #65971, #198130, #82250, #31392, #146229, #212246, #30329, #97467, #164580, #96413, #100640, #163523, #214341, #147277, #33509, #182954, #15110, #16165, #50828, #81199, #213309, #115888, #63880, #165646, #131084, #197073, #17234, #49762, #48710, #114824, #116955, #18307 ) ),
 .UNSPECIFIED., .F., .T., .F.,
 ( 2, 2 ),
 ( 4, 2, 2, 2, 2, 2, 2, 2, 2, 2, 2, 2, 2, 2, 2, 2, 2, 2, 2, 2, 2, 2, 2, 2, 2, 2, 2, 2, 2, 2, 2, 2, 2, 2, 2, 2, 2, 2, 2, 2, 2, 2, 2, 2, 2, 2, 2, 2, 2, 2, 2, 2, 2, 2, 2, 2, 2, 2, 2, 2, 2, 2, 2, 2, 2, 2, 2, 2, 2, 2, 2, 2, 2, 2, 2, 2, 2, 2, 2, 2, 2, 2, 2, 2, 2, 2, 2, 2, 2, 2, 2, 2, 2, 2, 2, 2, 2, 2, 2, 2, 2, 2, 2, 2, 2, 2, 2, 2, 2, 2, 2, 2, 2, 2, 2, 2, 2, 2, 2, 2, 2, 2, 4 ),
 ( 0.000000000000000000, 1.000000000000000000 ),
 ( -6.441036414471523752E-08, 0.0001394059631734492798, 0.0002788763367110432749, 0.0004183467102486372428, 0.0004532143036330357755, 0.0004880818970174342539, 0.0005578170837862312650, 0.0006275522705550282219, 0.0006972874573238252872, 0.0007670226440926222440, 0.0008367578308614192009, 0.0009064930176302162662, 0.0009413606110146147989, 0.0009762282043990132231, 0.001045963391167810180, 0.001115698577936607245, 0.001255168951474201159, 0.001324904138242998224, 0.001394639325011795290, 0.001464374511780592355, 0.001534109698549389203, 0.001603844885318186052, 0.001673580072086983117, 0.001743315258855780182, 0.001813050445624577248, 0.001882785632393374313, 0.001917653225777772846, 0.001952520819162171161, 0.002022256005930968010, 0.002091991192699765075, 0.002231461566237359206, 0.002301196753006155837, 0.002370931939774952903, 0.002405799533159351435, 0.002440667126543749968, 0.002510402313312547033, 0.002649872686850141164, 0.002719607873618938229, 0.002789343060387735294, 0.002859078247156532360, 0.002928813433925329425, 0.002998548620694126490, 0.003068283807462923122, 0.003207754181000516819, 0.003277489367769313884, 0.003312356961153712417, 0.003347224554538110949, 0.003416959741306908015, 0.003486694928075705080, 0.003626165301613299211, 0.003695900488382096276, 0.003765635675150893341, 0.003800503268535291874, 0.003835370861919690406, 0.003905106048688487038, 0.003974841235457283670, 0.004044576422226080735, 0.004114311608994877800, 0.004184046795763674866, 0.004253781982532471931, 0.004323517169301268996, 0.004393252356070066061, 0.004462987542838863127, 0.004532722729607660192, 0.004602457916376456390, 0.004672193103145253455, 0.004741928289914050521, 0.004811663476682847586, 0.004881398663451644651, 0.004951133850220441716, 0.005020869036989238782, 0.005090604223758035847, 0.005125471817142434813, 0.005160339410526832912, 0.005299809784064427043, 0.005439280157602021173, 0.005509015344370818239, 0.005578750531139615304, 0.005613618124524013403, 0.005648485717908412369, 0.005718220904677209435, 0.005857691278214803565, 0.005927426464983600631, 0.005997161651752397696, 0.006066896838521193894, 0.006136632025289990959, 0.006206367212058788024, 0.006276102398827584222, 0.006415572772365178353, 0.006485307959133975418, 0.006520175552518374384, 0.006555043145902772483, 0.006624778332671569549, 0.006694513519440366614, 0.006833983892977960745, 0.006903719079746757810, 0.006973454266515554875, 0.007043189453284351940, 0.007112924640053149006, 0.007182659826821946071, 0.007252395013590743136, 0.007322130200359540202, 0.007391865387128337267, 0.007461600573897134332, 0.007496468167281533299, 0.007531335760665931398, 0.007601070947434728463, 0.007670806134203525528, 0.007810276507741118791, 0.007880011694509915857, 0.007949746881278712055, 0.007984614474663111888, 0.008019482068047509987, 0.008089217254816306185, 0.008228687628353900316, 0.008298422815122698248, 0.008368158001891494446, 0.008437893188660290644, 0.008472760782044688743, 0.008507628375429088577, 0.008647098748966682707, 0.008786569122504276838, 0.008926039496041870969 ),
 .UNSPECIFIED. ) ;
#98708 = CARTESIAN_POINT ( 'NONE',  ( 6.257094453949625823, -1.604276942902042480, -0.9616840659161308702 ) ) ;
#98709 = CARTESIAN_POINT ( 'NONE',  ( 0.7187500000000003331, -0.7852924748299483504, 1.895863743164105220 ) ) ;
#98710 = CARTESIAN_POINT ( 'NONE',  ( 4.088303131848604721, 7.475188365022519932, -0.6044521916458069910 ) ) ;
#98711 = CARTESIAN_POINT ( 'NONE',  ( 6.837263156049210089, -1.242709075549037312, 1.588189626643407681 ) ) ;
#98712 = CARTESIAN_POINT ( 'NONE',  ( 11.86145016429273191, 12.59412123665269512, 1.099999999999996758 ) ) ;
#98713 = CARTESIAN_POINT ( 'NONE',  ( -1.360316468750040642, 1.911458333674787236, 0.7853790794158660438 ) ) ;
#98714 = CARTESIAN_POINT ( 'NONE',  ( 5.994767569012836361, -2.000857541758268354, 0.2496038112331094849 ) ) ;
#98715 = CARTESIAN_POINT ( 'NONE',  ( -9.992522908471816123, 11.61669713376064372, 1.199719254218462483 ) ) ;
#98716 = CARTESIAN_POINT ( 'NONE',  ( 7.796102023057898123, 9.054206100777749455, -1.199719254218441611 ) ) ;
#98717 = CARTESIAN_POINT ( 'NONE',  ( 3.607351389687783794, 6.366271167014519783, 1.199719254218451159 ) ) ;
#98718 = CARTESIAN_POINT ( 'NONE',  ( 2.578497204056416692, -1.747032809129964503, -0.5301130021647950663 ) ) ;
#98719 = DIRECTION ( 'NONE',  ( -0.7384114592165696989, -9.626321597927967204E-15, 0.6743504407188123384 ) ) ;
#98720 = CARTESIAN_POINT ( 'NONE',  ( -10.10575425844435138, 4.358269247758318699, 5.859476710806498900 ) ) ;
#98721 = ORIENTED_EDGE ( 'NONE', *, *, #20380, .F. ) ;
#98722 = CARTESIAN_POINT ( 'NONE',  ( -4.299344108864949554, 8.030002203735486788, -0.7216878364870338292 ) ) ;
#98723 = CARTESIAN_POINT ( 'NONE',  ( -3.719872605471121751, 6.605953636083950364, 7.500000000000000000 ) ) ;
#98724 = CARTESIAN_POINT ( 'NONE',  ( -8.296699936558862731, 11.76690146170562201, 1.199719254218453823 ) ) ;
#98725 = CARTESIAN_POINT ( 'NONE',  ( 0.2639333133152200750, 0.6296502125625064172, -1.919233096100453118 ) ) ;
#98726 = CARTESIAN_POINT ( 'NONE',  ( 0.4520119014386895229, -1.502510013782244025, -1.496567369470555020 ) ) ;
#98727 = EDGE_CURVE ( 'NONE', #21587, #117081, #93719, .T. ) ;
#98728 = VERTEX_POINT ( 'NONE', #160375 ) ;
#98729 = CARTESIAN_POINT ( 'NONE',  ( -5.264308783856126439, 9.363720357799287797, -0.7998128361456362523 ) ) ;
#98730 = CARTESIAN_POINT ( 'NONE',  ( 5.027376032568989572, 4.759693547618927489, 0.7998128361456341429 ) ) ;
#98731 = CARTESIAN_POINT ( 'NONE',  ( 0.1280963075596490419, -1.331634228802502928, -1.703589906866372017 ) ) ;
#98732 = CARTESIAN_POINT ( 'NONE',  ( 4.799454022740247794, 1.388487131293577592, -1.462444391756134943 ) ) ;
#98733 = ORIENTED_EDGE ( 'NONE', *, *, #64021, .F. ) ;
#98734 = ORIENTED_EDGE ( 'NONE', *, *, #32479, .T. ) ;
#98735 = CARTESIAN_POINT ( 'NONE',  ( 2.897268479386962969, 6.441866702775564058, 0.3987452234321529065 ) ) ;
#98736 = CARTESIAN_POINT ( 'NONE',  ( 8.018721507839716267, 8.319872945426633137, -0.7998128361456341429 ) ) ;
#98739 = ORIENTED_EDGE ( 'NONE', *, *, #110855, .T. ) ;
#98738 = CARTESIAN_POINT ( 'NONE',  ( -3.811250579217344558, 5.539821323877241355, 0.000000000000000000 ) ) ;
#98737 = CARTESIAN_POINT ( 'NONE',  ( -6.143779885648060102, 7.196773283791382703, 1.199719254218452047 ) ) ;
#98740 = CARTESIAN_POINT ( 'NONE',  ( 5.966021608595377224, 7.209656400309186530, 1.216315744458285719 ) ) ;
#98741 = CARTESIAN_POINT ( 'NONE',  ( 5.202499893966790800, -1.423744420606623429, -1.427717849564233532 ) ) ;
#98742 = CARTESIAN_POINT ( 'NONE',  ( 4.681507052731401330, -0.8653998779965512700, 1.625073734443114759 ) ) ;
#98743 = DIRECTION ( 'NONE',  ( -0.000000000000000000, -1.000000000000000000, -0.000000000000000000 ) ) ;
#98744 = CARTESIAN_POINT ( 'NONE',  ( 3.123938245303990335, -2.224009237659807958, 0.6155878327348850432 ) ) ;
#98745 = CARTESIAN_POINT ( 'NONE',  ( 7.178115983792402233, 7.339166500704784823, 0.7998128361456281477 ) ) ;
#98746 = EDGE_CURVE ( 'NONE', #131991, #141689, #160831, .T. ) ;
#98747 = CARTESIAN_POINT ( 'NONE',  ( 6.204392391313840349, -0.7715976231806520591, -2.019385000091134419 ) ) ;
#98748 = CARTESIAN_POINT ( 'NONE',  ( 5.798083248138522272, 9.916180889470295412, 0.7998128361456462443 ) ) ;
#98749 = CARTESIAN_POINT ( 'NONE',  ( 1.558044835347382362, -1.372074245553561722, 1.374660786877460072 ) ) ;
#98750 = CARTESIAN_POINT ( 'NONE',  ( -5.284980951228653190, 5.060232619388524533, 0.000000000000000000 ) ) ;
#98751 = ORIENTED_EDGE ( 'NONE', *, *, #75480, .F. ) ;
#98752 = CARTESIAN_POINT ( 'NONE',  ( 4.886215977948979550, -0.1196125283245419307, 2.295398719017431866 ) ) ;
#98753 = CARTESIAN_POINT ( 'NONE',  ( -9.421011374587449083, 15.43484797186988011, -7.432750069690781558 ) ) ;
#98754 = CARTESIAN_POINT ( 'NONE',  ( -5.167592825464113915, 6.057888380243431570, 1.199719254218452935 ) ) ;
#98755 = CARTESIAN_POINT ( 'NONE',  ( 2.992876365407059147, 1.605230647100181596, -0.9602576221170722182 ) ) ;
#98756 = VECTOR ( 'NONE', #104793, 1000.000000000000114 ) ;
#98759 = CARTESIAN_POINT ( 'NONE',  ( -7.123883369337781879, 7.275895117174344229, 0.7998128361456341429 ) ) ;
#98758 = CARTESIAN_POINT ( 'NONE',  ( 0.7499999999999885647, 0.5145833340161540814, 1.299038105676657340 ) ) ;
#98757 = CARTESIAN_POINT ( 'NONE',  ( 1.459083999156213451, -1.613880964290700160, 1.025699646091532857 ) ) ;
#98760 = CARTESIAN_POINT ( 'NONE',  ( 2.508667999599442755, -0.8457060194008919618, -2.038605049697986615 ) ) ;
#98761 = B_SPLINE_CURVE_WITH_KNOTS ( 'NONE', 3,
 ( #88850, #43303, #175428, #138664, #174372, #121416 ),
 .UNSPECIFIED., .F., .F.,
 ( 4, 2, 4 ),
 ( 0.000000000000000000, 0.0003778774010236168619, 0.0007557548020472337237 ),
 .UNSPECIFIED. ) ;
#98762 = CARTESIAN_POINT ( 'NONE',  ( -0.1394461523061352182, -0.009327122704730076569, -2.280146446826668782 ) ) ;
#98763 = CARTESIAN_POINT ( 'NONE',  ( 3.029357257649615054, 5.621668336311468117, -1.199719254218446718 ) ) ;
#98764 = CARTESIAN_POINT ( 'NONE',  ( 4.855228407025239612, 8.678533884922511987, 0.000000000000000000 ) ) ;
#98765 = CARTESIAN_POINT ( 'NONE',  ( -3.810004860640155311, 4.403759411290286252, 1.199719254218462483 ) ) ;
#98766 = CARTESIAN_POINT ( 'NONE',  ( -5.438229012412888252, 9.358701257874761481, -0.7216878364870338292 ) ) ;
#98767 = CARTESIAN_POINT ( 'NONE',  ( 0.7550724807275938089, -1.663022853828221681, -1.058333363951379003 ) ) ;
#98768 = CARTESIAN_POINT ( 'NONE',  ( 0.2183775786483640735, -2.262126603235939282, 0.4550015798871313577 ) ) ;
#98770 = ADVANCED_FACE ( 'NONE', ( #178771 ), #62861, .F. ) ;
#98769 = CARTESIAN_POINT ( 'NONE',  ( 1.644895634054041933, -0.2845770130874228365, -1.940982728367894206 ) ) ;
#98771 = CARTESIAN_POINT ( 'NONE',  ( 4.926661567281545473, -1.351126562560464484, 1.558462338037209349 ) ) ;
#98772 = CARTESIAN_POINT ( 'NONE',  ( 4.446711195602238931, 6.210915699667823198, -1.443375672974051449 ) ) ;
#98773 = CARTESIAN_POINT ( 'NONE',  ( 7.178115983792402233, 7.339166500704784823, 0.7998128361456281477 ) ) ;
#98774 = ORIENTED_EDGE ( 'NONE', *, *, #30625, .F. ) ;
#98775 =( BOUNDED_SURFACE ( )  B_SPLINE_SURFACE ( 3, 2, ( 
 ( #208054, #126909, #75937 ),
 ( #29325, #191798, #124776 ),
 ( #76991, #144191, #125841 ),
 ( #43461, #41330, #142038 ),
 ( #91144, #59681, #145246 ),
 ( #158272, #11990, #211252 ),
 ( #175586, #140982, #107439 ),
 ( #8797, #173463, #93280 ) ),
 .UNSPECIFIED., .F., .F., .T. ) 
 B_SPLINE_SURFACE_WITH_KNOTS ( ( 4, 2, 2, 4 ),
 ( 3, 3 ),
 ( 2.710505431213761085E-20, 0.0002475938981900018118, 0.0004951877963800036236, 0.0009903755927600072471 ),
 ( 0.000000000000000000, 1.000000000000000000 ),
 .UNSPECIFIED. ) 
 GEOMETRIC_REPRESENTATION_ITEM ( )  RATIONAL_B_SPLINE_SURFACE ( (
 ( 1.000000000000000000, 0.9238795325112864054, 1.000000000000000000),
 ( 1.000000000000000000, 0.9248499699752872338, 1.000000000000000000),
 ( 1.000000000000000000, 0.9171047238584292272, 1.000000000000000000),
 ( 1.000000000000000000, 0.8907236462368525176, 1.000000000000000000),
 ( 1.000000000000000000, 0.8725411758597159118, 1.000000000000000000),
 ( 1.000000000000000000, 0.8105159241137848136, 1.000000000000000000),
 ( 1.000000000000000000, 0.7599483315144378581, 1.000000000000000000),
 ( 1.000000000000000000, 0.7045118851637622859, 1.000000000000000000) ) ) 
 REPRESENTATION_ITEM ( '' )  SURFACE ( )  );
#98776 = CARTESIAN_POINT ( 'NONE',  ( -1.364683531250010295, 4.842708333674756283, 0.7879004041258379498 ) ) ;
#98777 = CARTESIAN_POINT ( 'NONE',  ( -15.75000000000000000, 10.90000000000000036, -3.600000000000002309 ) ) ;
#98778 = CARTESIAN_POINT ( 'NONE',  ( 2.860407222358956503, 6.280966159486672140, 0.7216878364870338292 ) ) ;
#98779 = CARTESIAN_POINT ( 'NONE',  ( 0.6905673677243575614, 1.117554423744430592, -1.861242299804190869 ) ) ;
#98781 = CARTESIAN_POINT ( 'NONE',  ( 5.829618728418341611, 0.9018330327132916269, -1.605192750430362025 ) ) ;
#98780 = CARTESIAN_POINT ( 'NONE',  ( 10.76345817711984409, -5.427673425445473043, -0.4370932794886462913 ) ) ;
#98782 = DIRECTION ( 'NONE',  ( 0.000000000000000000, 0.000000000000000000, -1.000000000000000000 ) ) ;
#98783 = DIRECTION ( 'NONE',  ( 0.000000000000000000, -1.000000000000000000, 0.000000000000000000 ) ) ;
#98784 = CARTESIAN_POINT ( 'NONE',  ( 1.317418832401914930, -1.826178791559311509, 0.4043020138455517554 ) ) ;
#98785 = CARTESIAN_POINT ( 'NONE',  ( 5.800121417639972243, -2.161773191644947634, -0.006422599366645573467 ) ) ;
#98786 = CARTESIAN_POINT ( 'NONE',  ( -5.816164686850935794, 6.201415483580719368, 0.9813818067917270405 ) ) ;
#98787 = SURFACE_SIDE_STYLE ('',( #80394 ) ) ;
#98788 = CARTESIAN_POINT ( 'NONE',  ( -1.201851678989727383E-14, 5.259375000341421469, -1.575800808251660134 ) ) ;
#98789 = CARTESIAN_POINT ( 'NONE',  ( 1.189939518123926510, 1.139724415472416652, 1.535358521287055300 ) ) ;
#98790 = CARTESIAN_POINT ( 'NONE',  ( 3.221328931188462086, -1.705978018192667811, 0.4708956190180821344 ) ) ;
#98791 = CIRCLE ( 'NONE', #50381, 0.4999999999999995559 ) ;
#98792 = CARTESIAN_POINT ( 'NONE',  ( 0.6801455168885979230, 0.9429141125626202546, 1.663586755705208420 ) ) ;
#98794 = CARTESIAN_POINT ( 'NONE',  ( 5.993738795899758998, -1.900512161056673088, 0.2395553810000446704 ) ) ;
#98793 = CARTESIAN_POINT ( 'NONE',  ( 0.4499999999999729772, 3.999999999999940936, -0.5000000000000368594 ) ) ;
#98795 = CARTESIAN_POINT ( 'NONE',  ( 6.092246201825009422, 0.9720536035879873138, -1.712898845271645820 ) ) ;
#98796 = CARTESIAN_POINT ( 'NONE',  ( 0.7499999999999920064, 4.483333333333352932, 1.299038105676669330 ) ) ;
#98797 = CARTESIAN_POINT ( 'NONE',  ( 0.8969213510382867405, -2.070190491330957006, -0.4589741369691033857 ) ) ;
#98798 = CARTESIAN_POINT ( 'NONE',  ( 2.370002892456526844, -0.1903694832692610361, -0.4477549104883266629 ) ) ;
#98799 = CARTESIAN_POINT ( 'NONE',  ( 3.819104250046548632, -0.1383300533824398659, 1.865606469731183825 ) ) ;
#98801 = ORIENTED_EDGE ( 'NONE', *, *, #55794, .T. ) ;
#98800 = CARTESIAN_POINT ( 'NONE',  ( 0.6272434487209905818, -1.734552980249819631, 0.5698080454362154379 ) ) ;
#98803 = CARTESIAN_POINT ( 'NONE',  ( 10.30245174296181254, 3.603753425775774843, 5.948123287112013102 ) ) ;
#98802 = CARTESIAN_POINT ( 'NONE',  ( 4.178501018151202118, -1.271701901513167421, 1.803451139310302986 ) ) ;
#98804 = CARTESIAN_POINT ( 'NONE',  ( 1.364683531249988535, 5.217708333674750065, -0.7879004041258300672 ) ) ;
#98805 = CARTESIAN_POINT ( 'NONE',  ( 2.207554788950978786, -1.655329399669298818, -1.230451883716067174 ) ) ;
#98806 = CARTESIAN_POINT ( 'NONE',  ( 4.611744806942754238, 8.532119374741881757, -0.7998128361456231517 ) ) ;
#98807 = CARTESIAN_POINT ( 'NONE',  ( -9.203287345578106127, 9.631590079462940324, 0.7998128361456462443 ) ) ;
#98808 = DIRECTION ( 'NONE',  ( 0.6507913734559654939, -0.7592566023652992380, 0.000000000000000000 ) ) ;
#98809 = CARTESIAN_POINT ( 'NONE',  ( -3.423460510979340121, -0.02136329652385748901, -0.4189541688200317804 ) ) ;
#98810 = CIRCLE ( 'NONE', #157558, 0.5000000000000016653 ) ;
#98811 = CARTESIAN_POINT ( 'NONE',  ( 0.1753634416057732182, 7.629137130509072051, -2.744001747789548418 ) ) ;
#98812 = ORIENTED_EDGE ( 'NONE', *, *, #6746, .T. ) ;
#98813 = CARTESIAN_POINT ( 'NONE',  ( 4.633297751427938316, 0.003287558298453730800, -2.070544812459538253 ) ) ;
#98814 = CARTESIAN_POINT ( 'NONE',  ( -1.001543065824772872E-14, 5.212500000000019895, 1.732050807568877637 ) ) ;
#98815 = CARTESIAN_POINT ( 'NONE',  ( 0.9839146201040609441, 1.450980403326153301, 1.602422216231303320 ) ) ;
#98816 = CARTESIAN_POINT ( 'NONE',  ( -5.265531293961836390, 7.681012046988098696, -1.216234931179949186 ) ) ;
#98818 = EDGE_CURVE ( 'NONE', #170262, #170765, #70652, .T. ) ;
#98817 = CARTESIAN_POINT ( 'NONE',  ( 1.893228994919902153, -0.1012422250811425839, -2.017274448259358977 ) ) ;
#98819 = CARTESIAN_POINT ( 'NONE',  ( -6.966220764712169000, 6.002124920821316323, -2.500000000000000444 ) ) ;
#98820 = ORIENTED_EDGE ( 'NONE', *, *, #110343, .F. ) ;
#98821 = AXIS2_PLACEMENT_3D ( 'NONE', #164966, #148725, #143702 ) ;
#98822 = EDGE_CURVE ( 'NONE', #151228, #51181, #213156, .T. ) ;
#98824 = CARTESIAN_POINT ( 'NONE',  ( 8.026063749610047537, 10.38682701267698150, -1.443375672974057666 ) ) ;
#98823 = CARTESIAN_POINT ( 'NONE',  ( -1.737500000000000266, -3.558333333333333570, -3.009438278150923907 ) ) ;
#98825 = CARTESIAN_POINT ( 'NONE',  ( -2.155383234892699562, 5.458438174109348395, 1.040834085586084257E-14 ) ) ;
#98826 = CARTESIAN_POINT ( 'NONE',  ( -0.06521966986864842497, -1.616690375843790051, 1.205047459138554045 ) ) ;
#98827 = CARTESIAN_POINT ( 'NONE',  ( 6.639320575229257670, 2.427506520031021520, 2.484945200759064665 ) ) ;
#98828 = CARTESIAN_POINT ( 'NONE',  ( 4.581673536070863584, -1.032772929490553215, 1.932928240684625099 ) ) ;
#98829 = CARTESIAN_POINT ( 'NONE',  ( 0.7499999999999902300, 3.264583334016149418, 1.299038105676669330 ) ) ;
#98830 = CARTESIAN_POINT ( 'NONE',  ( 3.533378866418676711, -0.1359047358975660202, 1.907598245988059826 ) ) ;
#98831 = CARTESIAN_POINT ( 'NONE',  ( -4.874319919312905647, 5.645460313075203018, -1.199719254218446718 ) ) ;
#98832 = CARTESIAN_POINT ( 'NONE',  ( 3.673896439178923057, 5.309298483840612093, 1.443375672974066548 ) ) ;
#98834 = CARTESIAN_POINT ( 'NONE',  ( 1.792592436991577109, 1.492242793082170449, -1.356315429364700176 ) ) ;
#98833 = CARTESIAN_POINT ( 'NONE',  ( -8.473482818416657736, 12.82955435488738516, -0.7216878364870267237 ) ) ;
#98835 = CARTESIAN_POINT ( 'NONE',  ( -1.364683531250010295, 12.69270833367473550, 0.7879004041258445001 ) ) ;
#98837 = CARTESIAN_POINT ( 'NONE',  ( -4.167152111353897403, 5.955039778036558040, 1.599625672291270506 ) ) ;
#98836 = CARTESIAN_POINT ( 'NONE',  ( 0.2754559168597633390, 2.135984121793169432, -0.8326521888945382921 ) ) ;
#98838 = CARTESIAN_POINT ( 'NONE',  ( 4.137519252912919221, -1.190027120290118257, -1.248710780074323567 ) ) ;
#98839 = DIRECTION ( 'NONE',  ( 0.000000000000000000, 1.000000000000000000, 0.000000000000000000 ) ) ;
#98840 = CARTESIAN_POINT ( 'NONE',  ( 4.695201269034174452, 4.372156323494968966, 1.214306433183764966E-14 ) ) ;
#98841 = CARTESIAN_POINT ( 'NONE',  ( 11.88235317400313917, 11.25664239773029607, 0.9089793033029930358 ) ) ;
#98842 = CARTESIAN_POINT ( 'NONE',  ( 0.07479286986305370977, 0.004866263145587856019, -1.855573292446038414 ) ) ;
#98843 = CARTESIAN_POINT ( 'NONE',  ( 3.867100128395839942, 5.534702787927018974, -1.599625672291255185 ) ) ;
#98844 = CARTESIAN_POINT ( 'NONE',  ( 0.07516593201273635838, 1.359561921253334749, -2.300590921312398951 ) ) ;
#98845 = ORIENTED_EDGE ( 'NONE', *, *, #101958, .F. ) ;
#98846 = ORIENTED_EDGE ( 'NONE', *, *, #133466, .F. ) ;
#98847 = CARTESIAN_POINT ( 'NONE',  ( 5.057183878474817540, -1.550805960166462105, 0.9359391756664036111 ) ) ;
#98848 = ORIENTED_EDGE ( 'NONE', *, *, #16981, .T. ) ;
#98849 = CARTESIAN_POINT ( 'NONE',  ( 5.123001941117305336, 7.070197912760590064, 1.599625672291268286 ) ) ;
#98850 = CARTESIAN_POINT ( 'NONE',  ( 7.334597915313080918, 9.580116872663850813, 1.040834085586084257E-14 ) ) ;
#98851 = CARTESIAN_POINT ( 'NONE',  ( 5.672461423068217989, 0.7400952288921599509, 1.653588109013460095 ) ) ;
#98852 = CARTESIAN_POINT ( 'NONE',  ( 5.194182247366861738, 9.073980031987776584, 0.7216878364870317197 ) ) ;
#98853 = CARTESIAN_POINT ( 'NONE',  ( -1.387358672527355008, 7.251968950354660493, 4.302625267139497112 ) ) ;
#98854 = CARTESIAN_POINT ( 'NONE',  ( 2.466951935624495551, 0.1062163371072753354, -2.188993582743845590 ) ) ;
#98856 = CARTESIAN_POINT ( 'NONE',  ( 10.06423010004587759, 10.63602329300870153, 0.000000000000000000 ) ) ;
#98855 = CARTESIAN_POINT ( 'NONE',  ( 6.267989458847986306, -1.846849288558198188, 0.2287129521939580412 ) ) ;
#98857 = CARTESIAN_POINT ( 'NONE',  ( 3.761272268043499345, 1.802513535502557218, -0.6487917036162252904 ) ) ;
#98858 = CARTESIAN_POINT ( 'NONE',  ( -6.588752024304622701, -8.074889850123406987, -6.844216539294235346 ) ) ;
#98859 = CARTESIAN_POINT ( 'NONE',  ( -1.500000000000001110, 12.02083333333333570, 0.8660254037844418162 ) ) ;
#98860 = CARTESIAN_POINT ( 'NONE',  ( -1.364683531250014514, 0.2385416670080863499, -0.7879004041258359514 ) ) ;
#98861 = CARTESIAN_POINT ( 'NONE',  ( 6.236387472606139681, 8.298871356172400127, -1.443375672974057666 ) ) ;
#98863 = CARTESIAN_POINT ( 'NONE',  ( 5.313701412219064224, -1.345319185855331279, -1.634962184252206630 ) ) ;
#98862 = CARTESIAN_POINT ( 'NONE',  ( -9.707274797704657843, 11.38787068781932987, 1.082531754730558626 ) ) ;
#98864 = CARTESIAN_POINT ( 'NONE',  ( 0.7608789386071808103, -1.564954856162886765, 1.491513986042219297 ) ) ;
#98865 = CARTESIAN_POINT ( 'NONE',  ( -4.613517410400161722, 8.604463755433990002, -0.7998128361456362523 ) ) ;
#98866 = CARTESIAN_POINT ( 'NONE',  ( 3.379725431556547477, 7.165039780116438273, -1.734723475976807094E-15 ) ) ;
#98867 = CARTESIAN_POINT ( 'NONE',  ( 1.078802750678783395, -0.04027803099338270881, -1.825304540826321542 ) ) ;
#98868 = CARTESIAN_POINT ( 'NONE',  ( -5.440899717785814715, 5.242137847038546461, 0.7998128361456341429 ) ) ;
#98869 = CARTESIAN_POINT ( 'NONE',  ( 4.102439050647597618, -0.5725816820084869141, -1.733541218493547476 ) ) ;
#98870 = CARTESIAN_POINT ( 'NONE',  ( 9.940066813768632770, 11.27778190843423545, -8.363988134642921679 ) ) ;
#98871 = ORIENTED_EDGE ( 'NONE', *, *, #20366, .T. ) ;
#98872 = CARTESIAN_POINT ( 'NONE',  ( 2.558991062574625275, 1.583523548174452733, -1.170949712736363502 ) ) ;
#98873 = ORIENTED_EDGE ( 'NONE', *, *, #152121, .F. ) ;
#98874 = CARTESIAN_POINT ( 'NONE',  ( 4.651864714057460048, 0.7465859729765094155, 1.793013943324140769 ) ) ;
#98875 = CARTESIAN_POINT ( 'NONE',  ( -2.979759899953417612, 6.698413326579433225, 0.7998128361456352531 ) ) ;
#98877 = CARTESIAN_POINT ( 'NONE',  ( 5.133110336712339183, 1.960249873928998410, 0.8093987030339530042 ) ) ;
#98876 = CARTESIAN_POINT ( 'NONE',  ( 7.191674137406095291, 7.354984346587396082, 0.000000000000000000 ) ) ;
#98878 = B_SPLINE_CURVE_WITH_KNOTS ( 'NONE', 3,
 ( #204853, #40262, #170243, #71656 ),
 .UNSPECIFIED., .F., .F.,
 ( 4, 4 ),
 ( 0.000000000000000000, 9.170750102251441879E-05 ),
 .UNSPECIFIED. ) ;
#98879 = DIRECTION ( 'NONE',  ( -0.6507913734559640506, -0.7592566023653005702, 0.000000000000000000 ) ) ;
#98880 = CARTESIAN_POINT ( 'NONE',  ( 2.982959643696237784, -1.767753630637520779, -0.7297678730374329570 ) ) ;
#98881 = CARTESIAN_POINT ( 'NONE',  ( 6.043473040404234276, 6.060458613201341826, -0.4842117992061110154 ) ) ;
#98882 = CARTESIAN_POINT ( 'NONE',  ( -1.244123718695689496, 3.108005466778244852, -0.7749999999999918066 ) ) ;
#98883 = CARTESIAN_POINT ( 'NONE',  ( 4.553559489343365740, 6.405848385690952718, -1.599625672291269396 ) ) ;
#98884 = CARTESIAN_POINT ( 'NONE',  ( 3.635557746758808495, 7.393234471193928847, -0.7998128361456291469 ) ) ;
#98885 = CARTESIAN_POINT ( 'NONE',  ( 4.108068219531130438, -0.7683648849950328596, 1.860876229713221086 ) ) ;
#98886 = LINE ( 'NONE', #211541, #40753 ) ;
#98887 = CARTESIAN_POINT ( 'NONE',  ( 5.303274670167754223, 1.494737065598227943, 1.048009559513597866 ) ) ;
#98888 = CARTESIAN_POINT ( 'NONE',  ( 0.7661813929631040576, -2.060537521029872643, 0.2012509062776293156 ) ) ;
#98889 = CARTESIAN_POINT ( 'NONE',  ( -7.687109909268394325, 11.91211929421440097, 0.000000000000000000 ) ) ;
#98890 = CARTESIAN_POINT ( 'NONE',  ( -6.155278136343885542, 7.070130543739276519, 1.092798041965221900 ) ) ;
#98891 = CARTESIAN_POINT ( 'NONE',  ( 11.35605497252127272, 11.11418145951645542, -3.553547709190210124 ) ) ;
#98892 = CARTESIAN_POINT ( 'NONE',  ( 5.717618200960680852, -1.824738551054584379, 0.4112096411929695439 ) ) ;
#98893 = CARTESIAN_POINT ( 'NONE',  ( 7.124973419181436007, 8.271222729588529887, -1.199719254218446718 ) ) ;
#98894 = CARTESIAN_POINT ( 'NONE',  ( -3.815730167242251003, 6.539103397502874948, -1.199719254218452047 ) ) ;
#98895 = CARTESIAN_POINT ( 'NONE',  ( 3.460355519985863548, 5.060167411448709629, 1.599625672291267398 ) ) ;
#98896 = CARTESIAN_POINT ( 'NONE',  ( -1.402160292154681736E-14, 10.23437500034139447, 1.575800808251682339 ) ) ;
#98897 = CARTESIAN_POINT ( 'NONE',  ( -4.089755892816631544, 7.923132308261379819, -0.7998128361456281477 ) ) ;
#98898 = CARTESIAN_POINT ( 'NONE',  ( 4.383363735919856730, 4.008345868194933104, -0.7998128361456211532 ) ) ;
#98899 = CARTESIAN_POINT ( 'NONE',  ( -8.106849506328558164, 8.422688943663599659, 0.000000000000000000 ) ) ;
#98900 = VECTOR ( 'NONE', #113173, 1000.000000000000000 ) ;
#98901 = CARTESIAN_POINT ( 'NONE',  ( -4.720210035852093533, 8.658662141802762946, -0.7998128361456281477 ) ) ;
#98902 = CARTESIAN_POINT ( 'NONE',  ( 6.631686460494314872, 2.080164978358085559, -0.6217935382996344629 ) ) ;
#98903 = CARTESIAN_POINT ( 'NONE',  ( 1.863061375884986104, -0.1076188601273372486, -2.114627633294167364 ) ) ;
#98904 =( GEOMETRIC_REPRESENTATION_CONTEXT ( 3 ) GLOBAL_UNCERTAINTY_ASSIGNED_CONTEXT ( ( #76828 ) ) GLOBAL_UNIT_ASSIGNED_CONTEXT ( ( #12589, #79733, #127522 ) ) REPRESENTATION_CONTEXT ( 'NONE', 'WORKASPACE' ) );
#98905 = CARTESIAN_POINT ( 'NONE',  ( 9.887974103068218668, 10.43039129653476493, 0.7998128361456462443 ) ) ;
#98906 = CARTESIAN_POINT ( 'NONE',  ( 0.4170821662628915183, 3.033599471985643170, 0.4170821662628724225 ) ) ;
#98907 = CARTESIAN_POINT ( 'NONE',  ( 6.508651864089095795, 0.6437109847576475419, 1.967739590238902991 ) ) ;
#98908 = CARTESIAN_POINT ( 'NONE',  ( 4.145277420728366025, 7.638539262984231470, 0.7997124044470202975 ) ) ;
#98909 = CARTESIAN_POINT ( 'NONE',  ( 6.317736394288147039, 6.473040002865377396, 0.7216878364870317197 ) ) ;
#98911 = CARTESIAN_POINT ( 'NONE',  ( -4.900611166869239810E-10, 15.51845925587262798, -11.92000000000000171 ) ) ;
#98910 = CARTESIAN_POINT ( 'NONE',  ( 1.737499999999999378, -3.966666666666666785, -3.009438278150925683 ) ) ;
#98912 = CARTESIAN_POINT ( 'NONE',  ( 2.818655624875044285, 2.158736131429010996, 0.7712820022114060814 ) ) ;
#98914 = DIRECTION ( 'NONE',  ( 7.993605777301127091E-15, 0.000000000000000000, -1.000000000000000000 ) ) ;
#98913 = CARTESIAN_POINT ( 'NONE',  ( -9.499065438569621378, -8.103879979615419060, 0.1510907968719145678 ) ) ;
#98915 = CARTESIAN_POINT ( 'NONE',  ( 2.777492966359981441, 0.2764497561681695803, -1.892163382976944419 ) ) ;
#98916 = ORIENTED_EDGE ( 'NONE', *, *, #52034, .T. ) ;
#98917 = CARTESIAN_POINT ( 'NONE',  ( 6.277061933002769045, 10.26706332190449622, 0.7216878364870438212 ) ) ;
#98918 = CARTESIAN_POINT ( 'NONE',  ( 0.7385399849154888896, 1.195762776690506790, -1.619497776973168213 ) ) ;
#98919 = CARTESIAN_POINT ( 'NONE',  ( 1.006607400890747295, 0.5640878064397096825, 1.878940696355746454 ) ) ;
#98920 = CARTESIAN_POINT ( 'NONE',  ( 5.427790276013049642, 4.356734706464521878, -2.440341524156855790 ) ) ;
#98921 = CARTESIAN_POINT ( 'NONE',  ( -7.711890448074853133, 7.891627032375787998, -0.7998128361456291469 ) ) ;
#98922 = CARTESIAN_POINT ( 'NONE',  ( -9.645001968711920171, 4.042125922905831281, 6.587946042608958663 ) ) ;
#98924 = CARTESIAN_POINT ( 'NONE',  ( 2.184116879877880724, -1.735013770989551896, -0.3484325113714877298 ) ) ;
#98923 = CARTESIAN_POINT ( 'NONE',  ( 3.644548676374514518, -1.708972400646594503, 1.203939368798632836 ) ) ;
#98925 = DIRECTION ( 'NONE',  ( 2.345077562848777574E-16, -0.000000000000000000, 1.000000000000000000 ) ) ;
#98926 = CARTESIAN_POINT ( 'NONE',  ( 5.806620824396801162, 2.019002025885249463, 1.085389930784508961 ) ) ;
#98927 = CARTESIAN_POINT ( 'NONE',  ( 4.874825007975835511, 1.622202256106145102, -0.6307315249329782381 ) ) ;
#98928 = EDGE_CURVE ( 'NONE', #86628, #92745, #116453, .T. ) ;
#98929 = CARTESIAN_POINT ( 'NONE',  ( 9.589694723567584234, 10.08239868711733855, -0.7998128361456281477 ) ) ;
#98930 = CARTESIAN_POINT ( 'NONE',  ( 5.357406976055401948, 6.279338222599979424, 1.199719254218452935 ) ) ;
#98931 = CARTESIAN_POINT ( 'NONE',  ( 3.110371403566422277, 0.6269696901312575843, -1.616694140604297614 ) ) ;
#98932 = CARTESIAN_POINT ( 'NONE',  ( 4.316952289276101418, -1.611618797226920252, 1.455085969030824211 ) ) ;
#98933 = CARTESIAN_POINT ( 'NONE',  ( 3.846762897975340767, 5.510976019103107859, -1.599625672291256295 ) ) ;
#98934 = CARTESIAN_POINT ( 'NONE',  ( 5.419157771004846857, -1.820987890746316173, 0.8666037247077316152 ) ) ;
#98936 = CIRCLE ( 'NONE', #185344, 0.5000000000000008882 ) ;
#98935 = CARTESIAN_POINT ( 'NONE',  ( 0.09375222243388467436, -1.895918425137008034, -0.7852924748299833224 ) ) ;
#98937 = CARTESIAN_POINT ( 'NONE',  ( -1.500000000000011324, 4.202083334016156080, 0.8660254037844403729 ) ) ;
#98938 = CARTESIAN_POINT ( 'NONE',  ( 1.887598533328225692, 1.326653652590740418, 1.397000115363009609 ) ) ;
#98939 = CARTESIAN_POINT ( 'NONE',  ( -0.7500000000000006661, 10.48958333401613174, -1.299038105676657340 ) ) ;
#98940 = CARTESIAN_POINT ( 'NONE',  ( 5.748318879583719010, 1.095320496750437966, -1.932492775422405717 ) ) ;
#98941 = EDGE_LOOP ( 'NONE', ( #98873, #46366, #45750, #110698 ) ) ;
#98942 = CARTESIAN_POINT ( 'NONE',  ( 6.983263157960366563, 2.432509251381759441, 2.428019605373044509 ) ) ;
#98943 = CARTESIAN_POINT ( 'NONE',  ( -1.201851678989727383E-14, 2.962500000000025224, 1.732050807568877637 ) ) ;
#98944 = CARTESIAN_POINT ( 'NONE',  ( 6.775324078527185989, 8.927630729746953264, -1.599625672291262513 ) ) ;
#98945 = EDGE_CURVE ( 'NONE', #159860, #142717, #36756, .T. ) ;
#98946 = CARTESIAN_POINT ( 'NONE',  ( 6.496542546517183325, 1.940334402339534581, 0.2891159199209930031 ) ) ;
#98947 = CARTESIAN_POINT ( 'NONE',  ( 7.131225611108079399, 11.26358761302737754, 0.7216878364870438212 ) ) ;
#98948 = EDGE_CURVE ( 'NONE', #51181, #116972, #194185, .T. ) ;
#98949 = CARTESIAN_POINT ( 'NONE',  ( -10.58855478214856660, 11.45566145536924552, -0.7216878364870217277 ) ) ;
#98950 = CIRCLE ( 'NONE', #92006, 0.08000000000000014044 ) ;
#98951 = CARTESIAN_POINT ( 'NONE',  ( 5.239300017038202917, 5.077214539491492928, 0.000000000000000000 ) ) ;
#98952 = CARTESIAN_POINT ( 'NONE',  ( -3.024877669624710386, 6.543124691288523920, 0.000000000000000000 ) ) ;
#98954 = CARTESIAN_POINT ( 'NONE',  ( 4.387212324874685265, 0.09821595252585722802, 2.060445151624993976 ) ) ;
#98953 = CARTESIAN_POINT ( 'NONE',  ( 9.378489572351044856, 11.96465713920816043, -1.599625672291262513 ) ) ;
#98955 = CARTESIAN_POINT ( 'NONE',  ( -3.066115294984855133, 6.728884944124295053, 0.7998128361456341429 ) ) ;
#98956 = CARTESIAN_POINT ( 'NONE',  ( -0.7499999999999972244, 5.389583334016151639, -1.299038105676652899 ) ) ;
#98957 = CARTESIAN_POINT ( 'NONE',  ( 0.6823417656249864960, -0.8239583329919114574, -1.181850606188749264 ) ) ;
#98958 = CARTESIAN_POINT ( 'NONE',  ( 5.694569522353672753, -0.4537686991618712362, -1.814561337198366875 ) ) ;
#98959 = CARTESIAN_POINT ( 'NONE',  ( 4.869590383887318019, -0.2189826452120811340, -1.720196969245034513 ) ) ;
#98960 = CARTESIAN_POINT ( 'NONE',  ( 4.440767568709752311, -1.349020001278607550, -1.099687749275481741 ) ) ;
#98961 = CARTESIAN_POINT ( 'NONE',  ( 5.508690485854129903, 5.321227076451600091, 1.040834085586084257E-14 ) ) ;
#98962 = CARTESIAN_POINT ( 'NONE',  ( 1.787097420474514031, 1.992035690054320574, -1.134270899834391999 ) ) ;
#98963 = CARTESIAN_POINT ( 'NONE',  ( 1.364683531249986981, -1.115624999658580752, 0.000000000000000000 ) ) ;
#98964 = CARTESIAN_POINT ( 'NONE',  ( 5.812080397998875547, 1.403551008015807788, -1.549792465900756477 ) ) ;
#98965 = CARTESIAN_POINT ( 'NONE',  ( 0.6734667703603390843, -1.024904740748554532, 1.529287851792550335 ) ) ;
#98966 = VECTOR ( 'NONE', #98925, 1000.000000000000000 ) ;
#98967 = CARTESIAN_POINT ( 'NONE',  ( -0.4000000000000281664, 3.963633530850221742, 0.9046180958550756879 ) ) ;
#98968 = CARTESIAN_POINT ( 'NONE',  ( 2.830704105008190030, 0.7231396562890278767, -1.882474209725725434 ) ) ;
#98969 = CARTESIAN_POINT ( 'NONE',  ( 0.7619990552875830492, 1.083242598816274382, 1.904929396514772444 ) ) ;
#98970 = CARTESIAN_POINT ( 'NONE',  ( 7.864583096620019198, 14.80247548031949201, -8.638774414189107631 ) ) ;
#98971 = CARTESIAN_POINT ( 'NONE',  ( -7.576308911938196999, 7.733448573549685179, 0.7998128361456462443 ) ) ;
#98972 = CARTESIAN_POINT ( 'NONE',  ( 1.363825363374836286, -0.5049007678423790280, 2.007717453658082629 ) ) ;
#98973 = CARTESIAN_POINT ( 'NONE',  ( 6.166260936116925606, 6.088392601758203071, 0.7998128361456341429 ) ) ;
#98974 = CARTESIAN_POINT ( 'NONE',  ( -1.360316468750000674, -0.3489583329919356824, -0.7853790794158941324 ) ) ;
#98975 = CARTESIAN_POINT ( 'NONE',  ( 3.985108911058360182, -1.979049277059058864, -0.7619450576143712572 ) ) ;
#98976 = CARTESIAN_POINT ( 'NONE',  ( 0.6823417656249882723, -0.07395833299191079124, -1.181850606188749264 ) ) ;
#98977 = CARTESIAN_POINT ( 'NONE',  ( 5.479063914364931343, -0.04889757770590653918, -1.825204647902956889 ) ) ;
#98978 = ORIENTED_EDGE ( 'NONE', *, *, #36800, .T. ) ;
#98979 = CARTESIAN_POINT ( 'NONE',  ( -6.656127069666307072, 6.730179434224282886, 0.7998128361456341429 ) ) ;
#98980 = CARTESIAN_POINT ( 'NONE',  ( 7.913155211870404493, 12.38376484715752213, 0.7998128361456462443 ) ) ;
#98981 = CARTESIAN_POINT ( 'NONE',  ( 6.414416072596830887, 8.576847732820027659, -1.443375672974078761 ) ) ;
#98982 = CARTESIAN_POINT ( 'NONE',  ( -1.737500000000000266, -3.164583332377419289, -3.009438278150923907 ) ) ;
#98983 = CARTESIAN_POINT ( 'NONE',  ( -5.259673527097670664, 8.223703984000886535, -1.199719254218446718 ) ) ;
#98984 = CARTESIAN_POINT ( 'NONE',  ( 3.726823374262774990, 1.425363347867984798, -1.431309510556647346 ) ) ;
#98985 = CARTESIAN_POINT ( 'NONE',  ( 6.510767885691055135, 1.639592601025055885, -1.477219212978691409 ) ) ;
#98986 = CARTESIAN_POINT ( 'NONE',  ( -7.117104292530948229, 7.267986194233038155, -0.7998128361456362523 ) ) ;
#98987 = CARTESIAN_POINT ( 'NONE',  ( 8.269583629331492602, 11.73526576994040482, 1.199719254218450271 ) ) ;
#98988 = CARTESIAN_POINT ( 'NONE',  ( 4.785918264633797214, -1.142728415277466159, -1.468712688171626812 ) ) ;
#98989 = CARTESIAN_POINT ( 'NONE',  ( 7.242026607993941489, 11.60078147596829901, 0.7998128361456462443 ) ) ;
#98990 = FACE_OUTER_BOUND ( 'NONE', #17061, .T. ) ;
#98991 = CARTESIAN_POINT ( 'NONE',  ( -2.415323921528888196, 5.969628341758991930, 0.7998128361456341429 ) ) ;
#98992 = CARTESIAN_POINT ( 'NONE',  ( -7.705111371268023923, 7.883718109434487253, 1.040834085586084257E-14 ) ) ;
#98993 = CARTESIAN_POINT ( 'NONE',  ( 0.3390366800232989530, 0.3710982241871863541, 2.129449491308422537 ) ) ;
#98995 = CARTESIAN_POINT ( 'NONE',  ( -5.066364649336571269, 6.741537443998309342, 1.444296757982476587 ) ) ;
#98994 = CARTESIAN_POINT ( 'NONE',  ( -5.576146316970437944, 9.727530813099326323, 0.000000000000000000 ) ) ;
#98996 = CARTESIAN_POINT ( 'NONE',  ( 1.364683531249986537, 0.6135416670080880985, 0.7879004041258500513 ) ) ;
#98997 = CARTESIAN_POINT ( 'NONE',  ( 2.108352191060134828, 0.6683163022180199642, -1.600079515618204606 ) ) ;
#98998 = CARTESIAN_POINT ( 'NONE',  ( 0.8490573499697011695, 1.738566659290440963, -0.08130723561216267326 ) ) ;
#99000 = CARTESIAN_POINT ( 'NONE',  ( 7.049876689426101350, 9.247942109129029475, -1.443375672974057666 ) ) ;
#98999 = CARTESIAN_POINT ( 'NONE',  ( 0.2886476729930695373, -1.083662648423104891, 2.037333779670726930 ) ) ;
#99001 = CARTESIAN_POINT ( 'NONE',  ( 6.616470431587431200, 6.759375818431882621, 0.1137606100791552777 ) ) ;
#99002 = CARTESIAN_POINT ( 'NONE',  ( 2.389980588989379040, -0.8839831138988951675, 1.861718010716238547 ) ) ;
#99003 = CARTESIAN_POINT ( 'NONE',  ( 6.328958779480917229, 6.278206752349526631, 0.7998128361456341429 ) ) ;
#99004 = CARTESIAN_POINT ( 'NONE',  ( 0.9310172746952742884, 0.9912447863934905623, 1.755501862388042067 ) ) ;
#99005 = CARTESIAN_POINT ( 'NONE',  ( -7.664830294503444996, -5.907420853759296264, 7.777967379493320621 ) ) ;
#99006 = CARTESIAN_POINT ( 'NONE',  ( -4.288121723672178476, 8.224835454251337552, -0.7998128361456362523 ) ) ;
#99007 = CARTESIAN_POINT ( 'NONE',  ( 6.789956943122251509, -0.7972922127613899512, 1.690610701080223821 ) ) ;
#99009 = CARTESIAN_POINT ( 'NONE',  ( -6.536439455564198475, 8.719208346281938304, 1.443375672974064550 ) ) ;
#99008 = CARTESIAN_POINT ( 'NONE',  ( 5.168181644781757456, 1.909928461159452251, -0.09994665148223277895 ) ) ;
#99010 = CARTESIAN_POINT ( 'NONE',  ( 6.481111342790009999, -0.1036386110354891726, -2.204582208980155222 ) ) ;
#99011 = CARTESIAN_POINT ( 'NONE',  ( -6.360183458142173230, 9.473945563590925545, 1.082531754730549967 ) ) ;
#99012 = CARTESIAN_POINT ( 'NONE',  ( 6.556249800660121529, 9.806652646482286073, 1.199719254218452047 ) ) ;
#99013 = CARTESIAN_POINT ( 'NONE',  ( -2.984203208339354152, 6.495671153122273722, 0.000000000000000000 ) ) ;
#99014 = CARTESIAN_POINT ( 'NONE',  ( 0.4869804533438352734, -1.902474711392083684, -0.6784070981462678729 ) ) ;
#99015 = VERTEX_POINT ( 'NONE', #3162 ) ;
#99016 = CARTESIAN_POINT ( 'NONE',  ( 0.000000000000000000, -9.331509131462439655, 0.000000000000000000 ) ) ;
#99017 = CARTESIAN_POINT ( 'NONE',  ( 4.225798673374229431, -2.209433879803673673, 0.6658836873896284425 ) ) ;
#99019 = ADVANCED_FACE ( 'NONE', ( #15164 ), #64981, .F. ) ;
#99018 = CARTESIAN_POINT ( 'NONE',  ( 4.457442142980160504, 1.574409630067734156, 1.170308293268598421 ) ) ;
#99020 = CARTESIAN_POINT ( 'NONE',  ( 1.727322521004183598, 0.1496332796787832875, -1.956138870750294023 ) ) ;
#99021 = CARTESIAN_POINT ( 'NONE',  ( 9.103410076571945453, 12.70806329172093818, 1.199719254218450271 ) ) ;
#99022 = CARTESIAN_POINT ( 'NONE',  ( -9.549485338732782935, 14.79470350949243951, 7.267374014142787608 ) ) ;
#99023 = ORIENTED_EDGE ( 'NONE', *, *, #195893, .T. ) ;
#99024 = CARTESIAN_POINT ( 'NONE',  ( 6.473846665049121540, -0.8576149079453172508, 1.823233050095712349 ) ) ;
#99026 = CARTESIAN_POINT ( 'NONE',  ( -7.458957065812611198, 11.85386701009007204, 0.7998128361456481317 ) ) ;
#99025 = CARTESIAN_POINT ( 'NONE',  ( -4.466521540698216164, 7.298359999868178960, -1.199719254218452047 ) ) ;
#99027 = CARTESIAN_POINT ( 'NONE',  ( 1.394213304513430174, 1.506067903837378097, -1.058747118707924262 ) ) ;
#99028 = ORIENTED_EDGE ( 'NONE', *, *, #92149, .F. ) ;
#99030 = MECHANICAL_DESIGN_GEOMETRIC_PRESENTATION_REPRESENTATION (  '', ( #119793 ), #133689 ) ;
#99029 = CARTESIAN_POINT ( 'NONE',  ( 4.557605255626766549, 1.740051450181074877, 1.298158460866901454 ) ) ;
#99031 = CARTESIAN_POINT ( 'NONE',  ( 9.843279382890161244, 11.92209134021086037, -6.866670447127348531 ) ) ;
#99032 = CARTESIAN_POINT ( 'NONE',  ( 2.092179824929023102, 1.308410154019133076, 1.668721082780571408 ) ) ;
#99033 = CARTESIAN_POINT ( 'NONE',  ( 1.499999999999989120, 2.556250000682817713, 1.214306433183764966E-14 ) ) ;
#99034 = CARTESIAN_POINT ( 'NONE',  ( 8.269583629331492602, 11.73526576994040482, 1.199719254218450271 ) ) ;
#99035 = CARTESIAN_POINT ( 'NONE',  ( 6.604949037901548969, 6.766875157141204689, 0.08182522243922914218 ) ) ;
#99036 = CARTESIAN_POINT ( 'NONE',  ( 2.548181945144313953, 2.060261615984103400, 0.05380422017278729124 ) ) ;
#99038 = CARTESIAN_POINT ( 'NONE',  ( 8.641284494170047736, 13.75145223737358613, -8.262855152994331931 ) ) ;
#99037 = CARTESIAN_POINT ( 'NONE',  ( -8.666686507633592385, 11.13422023037111330, 1.599625672291269396 ) ) ;
#99039 = CARTESIAN_POINT ( 'NONE',  ( -1.364683531250012516, 3.488541667008085767, -0.7879004041258300672 ) ) ;
#99040 = CARTESIAN_POINT ( 'NONE',  ( 0.07735805125222078305, -0.0005418671161615954465, -2.088975025666544472 ) ) ;
#99041 = EDGE_CURVE ( 'NONE', #15524, #36822, #114429, .T. ) ;
#99042 = FACE_OUTER_BOUND ( 'NONE', #14316, .T. ) ;
#99043 = CARTESIAN_POINT ( 'NONE',  ( 5.443983014310386892, -1.216401775450553169, -1.475513148251464068 ) ) ;
#99044 = CARTESIAN_POINT ( 'NONE',  ( 1.499999999999996891, 9.427083334016128191, -0.8660254037844378194 ) ) ;
#99045 = CARTESIAN_POINT ( 'NONE',  ( 1.845381457188604690, -1.911753278855784943, 1.209540087214598270 ) ) ;
#99046 = CARTESIAN_POINT ( 'NONE',  ( -8.758204044748012507, 11.24099069033793974, 1.443375672974064550 ) ) ;
#99047 = CARTESIAN_POINT ( 'NONE',  ( 1.054613590283080660, 0.3547985653672180439, 1.776302104178028252 ) ) ;
#99048 = CARTESIAN_POINT ( 'NONE',  ( 1.762754532109143124, -0.09793373165993285445, -1.913366418544469205 ) ) ;
#99049 = CARTESIAN_POINT ( 'NONE',  ( 3.473154722801426786, 1.870513717286937494, 0.8877811045280564750 ) ) ;
#99050 = CARTESIAN_POINT ( 'NONE',  ( -0.6823417656250212460, 2.113541667008083991, 1.181850606188767472 ) ) ;
#99051 = CARTESIAN_POINT ( 'NONE',  ( 1.446098081747126951, 1.969109070040415910, 0.09893570862591105630 ) ) ;
#99052 = CARTESIAN_POINT ( 'NONE',  ( 5.074797080785846681, -1.814676937445957039, -0.6471642872378483569 ) ) ;
#99054 = CARTESIAN_POINT ( 'NONE',  ( 5.834480046583573554, 7.201333694826374199, -1.164487238324034557 ) ) ;
#99053 = CARTESIAN_POINT ( 'NONE',  ( 1.454236823263599376, 0.6660240913333862478, -2.209497540817098038 ) ) ;
#99055 = CARTESIAN_POINT ( 'NONE',  ( -1.201851678989727383E-14, 1.571875000341420581, 1.575800808251672791 ) ) ;
#99056 = CARTESIAN_POINT ( 'NONE',  ( 5.494603814743470593, 2.031562770168824361, 0.3561260095714424700 ) ) ;
#99057 = CARTESIAN_POINT ( 'NONE',  ( -5.250031796989778066, 7.148123067953287446, 1.599625672291267398 ) ) ;
#99058 = CARTESIAN_POINT ( 'NONE',  ( 6.775324078527185989, 8.927630729746953264, -1.599625672291262513 ) ) ;
#99059 = CARTESIAN_POINT ( 'NONE',  ( -1.150222622689996532, 2.858395032273045810, 0.7749999999993751887 ) ) ;
#99061 = CARTESIAN_POINT ( 'NONE',  ( 1.499999999999989120, 5.045833333333354709, -0.8660254037844323793 ) ) ;
#99060 = CARTESIAN_POINT ( 'NONE',  ( 6.651405291617982662, -1.688965747674558759, -1.257743519153362355 ) ) ;
#99062 = AXIS2_PLACEMENT_3D ( 'NONE', #62398, #144766, #128562 ) ;
#99063 = CARTESIAN_POINT ( 'NONE',  ( -0.6823417656250212460, 2.613541667008084879, 1.181850606188767472 ) ) ;
#99064 = CARTESIAN_POINT ( 'NONE',  ( 5.255217470067075070, -1.823004960263453489, -1.161262906855420329 ) ) ;
#99066 = EDGE_CURVE ( 'NONE', #124240, #138555, #74815, .T. ) ;
#99065 = CARTESIAN_POINT ( 'NONE',  ( 5.145178147197468022, 0.1505999202349363186, 2.014131245181075336 ) ) ;
#99067 = PLANE ( 'NONE',  #18269 ) ;
#99068 = CARTESIAN_POINT ( 'NONE',  ( -5.341549334104202629, 7.254893527920112994, 1.443375672974064550 ) ) ;
#99069 = ADVANCED_FACE ( 'NONE', ( #34623 ), #180879, .F. ) ;
#99072 = CARTESIAN_POINT ( 'NONE',  ( 4.826339496784873617, 8.574553812983598533, -0.7216878364870257245 ) ) ;
#99071 = CARTESIAN_POINT ( 'NONE',  ( -1.642778471874998480, -1.101041666188708801, 2.845375778867863303 ) ) ;
#99070 = CARTESIAN_POINT ( 'NONE',  ( 5.501576472095266901, 9.640532660744973725, -0.7998128361456481317 ) ) ;
#99073 = CARTESIAN_POINT ( 'NONE',  ( -5.818384198920079520, 6.817144982608731141, 1.199719254218452935 ) ) ;
#99074 = CARTESIAN_POINT ( 'NONE',  ( 3.450407915430803385, -1.350735839785843773, 1.497501794165828626 ) ) ;
#99075 = CARTESIAN_POINT ( 'NONE',  ( -9.338868881714763148, 9.789768538289042255, -0.7998128361456291469 ) ) ;
#99077 = CARTESIAN_POINT ( 'NONE',  ( -10.99643026930483813, -5.229832900979425325, 0.2868663046952791285 ) ) ;
#99076 = CARTESIAN_POINT ( 'NONE',  ( -8.663296969452339624, 13.05100419776235299, 1.040834085586084257E-14 ) ) ;
#99078 =( REPRESENTATION_RELATIONSHIP ('NONE','NONE', #84563, #189584 ) REPRESENTATION_RELATIONSHIP_WITH_TRANSFORMATION ( #10239 )SHAPE_REPRESENTATION_RELATIONSHIP( ) );
#99079 = CARTESIAN_POINT ( 'NONE',  ( -1.364683531249997417, 5.509375000341417916, 1.214306433183764966E-14 ) ) ;
#99081 = CARTESIAN_POINT ( 'NONE',  ( 1.364683531249997417, 8.984375000341396245, 2.602085213965210642E-15 ) ) ;
#99080 = CARTESIAN_POINT ( 'NONE',  ( 5.120075222393803749, -1.153228217640640985, -1.828211184805514922 ) ) ;
#99082 = LINE ( 'NONE', #148886, #148461 ) ;
#99083 = CARTESIAN_POINT ( 'NONE',  ( -11.68315434942572217, 7.483877878977486020, -2.545616869505754831 ) ) ;
#99085 = CARTESIAN_POINT ( 'NONE',  ( 5.378529868213833609, -0.4926607797600784933, -1.955169007017331317 ) ) ;
#99084 = CARTESIAN_POINT ( 'NONE',  ( -7.009202228140751778, 9.200488570962775725, -1.443375672974058777 ) ) ;
#99086 = CARTESIAN_POINT ( 'NONE',  ( 0.6823417656249882723, -0.2614583329919109578, -1.181850606188749264 ) ) ;
#99087 = CARTESIAN_POINT ( 'NONE',  ( 1.189626395179286478, -0.7786649258869399182, 1.539184141221685787 ) ) ;
#99088 = CARTESIAN_POINT ( 'NONE',  ( 4.224247379109608680, 7.085983154673295203, -1.199719254218452047 ) ) ;
#99090 = CARTESIAN_POINT ( 'NONE',  ( 6.318982112420993502, 9.529840343536603697, -1.199719254218452047 ) ) ;
#99089 = CARTESIAN_POINT ( 'NONE',  ( 8.758204044748010730, 9.320252261735261001, 0.7216878364870438212 ) ) ;
#99091 = CARTESIAN_POINT ( 'NONE',  ( -10.50060100873255031, 5.377693802073529206, 5.808388628131297970 ) ) ;
#99092 = CARTESIAN_POINT ( 'NONE',  ( 0.2800358821246723418, -1.714356997462190835, -0.4388462949536375279 ) ) ;
#99093 = CARTESIAN_POINT ( 'NONE',  ( 0.3639315877056762405, 0.6293089562653730873, -1.912281478549708202 ) ) ;
#99094 = CARTESIAN_POINT ( 'NONE',  ( 6.539320575229250920, 3.702490941164796379, 2.411252750440337156 ) ) ;
#99095 = CARTESIAN_POINT ( 'NONE',  ( -6.577113915960841162, 7.806292669110006521, -1.082531754730549967 ) ) ;
#99096 = VERTEX_POINT ( 'NONE', #32499 ) ;
#99097 = CARTESIAN_POINT ( 'NONE',  ( 7.890482213029013536, 12.14938698193514277, 1.040834085586084257E-14 ) ) ;
#99099 = CARTESIAN_POINT ( 'NONE',  ( 1.599232692168949699, -0.2440074622011619843, 2.001515180871694888 ) ) ;
#99098 = CARTESIAN_POINT ( 'NONE',  ( 2.121885542695590487, -0.4617877489709980576, 2.069441001874790409 ) ) ;
#99100 = CARTESIAN_POINT ( 'NONE',  ( 2.250024469429566132, 0.8508988043372580634, -1.599271047475413932 ) ) ;
#99101 = CARTESIAN_POINT ( 'NONE',  ( 7.095713291905693332, 9.371694488680407886, 1.599625672291268286 ) ) ;
#99102 = CARTESIAN_POINT ( 'NONE',  ( 6.403215362905616992, 1.794359850238020693, 1.205212418099836480 ) ) ;
#99103 = ORIENTED_EDGE ( 'NONE', *, *, #144905, .F. ) ;
#99104 = VECTOR ( 'NONE', #126553, 1000.000000000000000 ) ;
#99105 = CARTESIAN_POINT ( 'NONE',  ( 7.298366762858032430, 7.409182732956175244, 1.040834085586084257E-14 ) ) ;
#99107 = CARTESIAN_POINT ( 'NONE',  ( 0.6377201071205064187, 1.913410132493647442, -0.09706281964840141052 ) ) ;
#99106 = CARTESIAN_POINT ( 'NONE',  ( -4.741601036477307574, 6.554953847355395880, 1.599625672291267398 ) ) ;
#99108 = CARTESIAN_POINT ( 'NONE',  ( -2.670845766169893665, 0.4339950243563579502, -0.1191324417346312919 ) ) ;
#99109 = DIRECTION ( 'NONE',  ( 9.436895709313856232E-16, -0.8656921114426507913, -0.5005768354468325132 ) ) ;
#99110 = CARTESIAN_POINT ( 'NONE',  ( 6.304178240230120522, 6.457222156464352381, -0.7216878364870257245 ) ) ;
#99111 = CARTESIAN_POINT ( 'NONE',  ( 1.364683531249986537, 0.4260416670080872659, 0.7879004041258500513 ) ) ;
#99112 = DIRECTION ( 'NONE',  ( 0.8660254037844399289, 0.000000000000000000, 0.4999999999999978906 ) ) ;
#99113 = CARTESIAN_POINT ( 'NONE',  ( -10.14557902172788495, 10.73093036830436553, 1.040834085586084257E-14 ) ) ;
#99114 = AXIS2_PLACEMENT_3D ( 'NONE', #112242, #129574, #46125 ) ;
#99115 = CARTESIAN_POINT ( 'NONE',  ( 4.030267251519312310, 1.158562084521784108, -1.824840551714689507 ) ) ;
#99116 = CARTESIAN_POINT ( 'NONE',  ( -5.153507786970262572, 9.026526494858359229, -0.7216878364870338292 ) ) ;
#99117 = CARTESIAN_POINT ( 'NONE',  ( 4.556949027968946631, 8.330541276023501140, -0.7216878364870357165 ) ) ;
#99118 = CARTESIAN_POINT ( 'NONE',  ( 2.408575119285644384, -2.115224228095522907, -0.1514441693673748146 ) ) ;
#99119 = CARTESIAN_POINT ( 'NONE',  ( 6.458013382736495167, 1.820430347099718293, -0.1376817787434730933 ) ) ;
#99120 = CARTESIAN_POINT ( 'NONE',  ( 2.882053135459626159, -1.016639628983921684, 1.688880165396142718 ) ) ;
#99121 = CARTESIAN_POINT ( 'NONE',  ( 5.765855477156511810, 0.5488314196105298359, -1.831976909803390896 ) ) ;
#99122 = ORIENTED_EDGE ( 'NONE', *, *, #105759, .F. ) ;
#99123 = FACE_OUTER_BOUND ( 'NONE', #99191, .T. ) ;
#99125 = EDGE_CURVE ( 'NONE', #178226, #75675, #142231, .T. ) ;
#99124 = CARTESIAN_POINT ( 'NONE',  ( 6.514111218838506190, 1.964378047669375293, -0.1432920118879192073 ) ) ;
#99126 = CARTESIAN_POINT ( 'NONE',  ( 1.763517528630250686, 0.9983118466501934574, 1.665567687315899992 ) ) ;
#99127 = ORIENTED_EDGE ( 'NONE', *, *, #165199, .F. ) ;
#99128 = CARTESIAN_POINT ( 'NONE',  ( -5.496904935697871863, 5.377753611261092637, 0.7998128361456281477 ) ) ;
#99130 = CARTESIAN_POINT ( 'NONE',  ( 1.846545397494917973, 2.494430857982443683, -2.490037463721383126 ) ) ;
#99129 = CARTESIAN_POINT ( 'NONE',  ( -6.238160076063538284, 9.331584951165851294, 1.082531754730549967 ) ) ;
#99132 = CARTESIAN_POINT ( 'NONE',  ( 7.039708073993665494, 9.236078724457858158, 1.599625672291281386 ) ) ;
#99131 = CARTESIAN_POINT ( 'NONE',  ( 2.308638494240814687, 1.867967618895223447, 0.9389952993345984655 ) ) ;
#99134 = CARTESIAN_POINT ( 'NONE',  ( 6.007671464186837618, 6.181573927739029806, 0.7216878364870328300 ) ) ;
#99133 = CARTESIAN_POINT ( 'NONE',  ( 7.820355676984174664, 8.018169799436671852, -0.7998128361456281477 ) ) ;
#99136 = ORIENTED_EDGE ( 'NONE', *, *, #169996, .F. ) ;
#99135 = CARTESIAN_POINT ( 'NONE',  ( 6.041656841763191288, -1.799011877964010520, 0.6487133288125003228 ) ) ;
#99137 = CARTESIAN_POINT ( 'NONE',  ( 4.108205984530819421, -2.201057848371779535, 0.1611738814469021175 ) ) ;
#99138 = CARTESIAN_POINT ( 'NONE',  ( 2.028631293930313717, 1.270571802522667992, -1.804104215285810886 ) ) ;
#99139 = CARTESIAN_POINT ( 'NONE',  ( -0.1025498324992805826, -6.714092063936416999, -10.99981089498244202 ) ) ;
#99140 = CARTESIAN_POINT ( 'NONE',  ( 0.9965660710522583621, -1.865815080690262917, -0.4182784585613218420 ) ) ;
#99141 = CARTESIAN_POINT ( 'NONE',  ( -2.449742653233059286, 3.300000000000011369, 0.3999999999999750422 ) ) ;
#99142 = CARTESIAN_POINT ( 'NONE',  ( 11.44779964734654776, 13.49810470129596318, -3.599999963171534478 ) ) ;
#99143 = CARTESIAN_POINT ( 'NONE',  ( 4.686024408448190570, -1.271122505372159761, -1.634150330299996012 ) ) ;
#99144 = CARTESIAN_POINT ( 'NONE',  ( -4.401593425930945713, 8.286942763561420122, 1.040834085586084257E-14 ) ) ;
#99146 = CARTESIAN_POINT ( 'NONE',  ( 2.167066695894452888, -1.976221826324360498, -0.8764929760368763700 ) ) ;
#99145 = CARTESIAN_POINT ( 'NONE',  ( -4.613852347352193739, 4.277249248199312071, 1.214306433183764966E-14 ) ) ;
#99147 = CARTESIAN_POINT ( 'NONE',  ( 3.140350738262797314, 0.5347024899306859202, 2.125194831261326911 ) ) ;
#99148 = CARTESIAN_POINT ( 'NONE',  ( -4.326460414921602826, 8.061637894134911164, 8.322892513849239118E-08 ) ) ;
#99149 = CARTESIAN_POINT ( 'NONE',  ( 3.390947817193682656, 6.009837315817661008, -1.082531754730549967 ) ) ;
#99150 = CARTESIAN_POINT ( 'NONE',  ( 0.7499999999999920064, 4.764583334016150751, 1.299038105676669330 ) ) ;
#99151 = CARTESIAN_POINT ( 'NONE',  ( -1.364683531250014514, 14.65104166700806410, -0.7879004041258335089 ) ) ;
#99152 = CARTESIAN_POINT ( 'NONE',  ( -3.318713740295064163, 7.093859473644694269, 0.000000000000000000 ) ) ;
#99153 = CARTESIAN_POINT ( 'NONE',  ( 6.065060216814489813, -0.9193275656586662459, 1.470200510888696632 ) ) ;
#99154 = CARTESIAN_POINT ( 'NONE',  ( -9.991996023591624976, 10.75967623705280296, 1.040834085586084257E-14 ) ) ;
#99155 = CARTESIAN_POINT ( 'NONE',  ( 4.662978783614929235, 1.603679166536524869, -1.309313232293010776 ) ) ;
#99156 = CARTESIAN_POINT ( 'NONE',  ( 5.237957716521472129, 2.114759263080950635, -0.1049963987776857816 ) ) ;
#99157 = CARTESIAN_POINT ( 'NONE',  ( 5.774883364416965037, 8.824782127540085952, -1.199719254218440723 ) ) ;
#99158 = CARTESIAN_POINT ( 'NONE',  ( 9.649010003797931390, 3.730310916805957167, 7.134817918383254742 ) ) ;
#99159 = CARTESIAN_POINT ( 'NONE',  ( 3.379706166375577414, -1.899257087701329949, 0.5209217831910922802 ) ) ;
#99160 = CARTESIAN_POINT ( 'NONE',  ( 5.929661055573363981, 1.134796830042347660, -1.991584109881129327 ) ) ;
#99161 = CARTESIAN_POINT ( 'NONE',  ( 3.053144290054691901, -1.492835736363472110, -1.050712463094093385 ) ) ;
#99162 = CARTESIAN_POINT ( 'NONE',  ( 4.415115299905642665, 5.179997933758551554, -1.199719254218450271 ) ) ;
#99163 = CARTESIAN_POINT ( 'NONE',  ( 4.867013957181530515, 5.740899707208986236, -1.082531754730548412 ) ) ;
#99164 = CARTESIAN_POINT ( 'NONE',  ( -7.542413527904030524, 7.693903958843159252, 1.040834085586084257E-14 ) ) ;
#99165 = CARTESIAN_POINT ( 'NONE',  ( 6.042093733545556233, 7.078139439671806699, -1.199719254218452047 ) ) ;
#99166 = ORIENTED_EDGE ( 'NONE', *, *, #36958, .F. ) ;
#99167 = CARTESIAN_POINT ( 'NONE',  ( 4.113543134289789016, 1.619545278408863975, 1.195698625712667384 ) ) ;
#99168 = CARTESIAN_POINT ( 'NONE',  ( 4.346505277090593644, -1.939800950321630690, -0.2920161945778113055 ) ) ;
#99169 = CARTESIAN_POINT ( 'NONE',  ( -5.693534442735004752, 8.729875052244421951, 1.199719254218452047 ) ) ;
#99170 = AXIS2_PLACEMENT_3D ( 'NONE', #210431, #96731, #27422 ) ;
#99171 = CARTESIAN_POINT ( 'NONE',  ( -4.569261463005423352, 5.289558780716470565, -1.199719254218446718 ) ) ;
#99172 = FILL_AREA_STYLE ('',( #212901 ) ) ;
#99174 = CARTESIAN_POINT ( 'NONE',  ( 6.121911923048983795, -0.9866791243483238327, -1.469064191006617337 ) ) ;
#99173 = CARTESIAN_POINT ( 'NONE',  ( 0.4860219701983969909, -2.075441973172939214, -0.2518264690121001514 ) ) ;
#99175 = PLANE ( 'NONE',  #19147 ) ;
#99176 = CARTESIAN_POINT ( 'NONE',  ( 1.412352946837617473, 1.469754387505791460, -1.625674263109680329 ) ) ;
#99177 = CARTESIAN_POINT ( 'NONE',  ( 0.8897394992621279197, -0.4213058873485018840, -1.688518545418623340 ) ) ;
#99178 = CARTESIAN_POINT ( 'NONE',  ( 5.880485940025228508, 7.883652901494672349, 1.599625672291267398 ) ) ;
#99179 = CARTESIAN_POINT ( 'NONE',  ( 0.1335669894368864408, 5.721243636067999461, -2.747585559332069494 ) ) ;
#99180 = CARTESIAN_POINT ( 'NONE',  ( 2.033451192367647042, -1.125475165956592694, -1.307177254964901003 ) ) ;
#99181 = CARTESIAN_POINT ( 'NONE',  ( 1.089736160853293168, 1.367490553916232754, -1.847165887925501515 ) ) ;
#99182 =( BOUNDED_CURVE ( )  B_SPLINE_CURVE ( 2, ( #142807, #25806, #191499, #91915, #109278, #175287, #26873, #10616, #60441 ),
 .UNSPECIFIED., .F., .T. ) 
 B_SPLINE_CURVE_WITH_KNOTS ( ( 3, 2, 2, 2, 3 ),
 ( 0.6339285714285713969, 0.6369047619047618625, 0.6428571428571429047, 0.6488095238095238360, 0.6517857142857143016 ),
 .UNSPECIFIED. ) 
 CURVE ( )  GEOMETRIC_REPRESENTATION_ITEM ( )  RATIONAL_B_SPLINE_CURVE ( ( 0.9330127018922194093, 0.9330127018922194093, 1.000000000000000000, 0.8660254037844387076, 1.000000000000000000, 0.8660254037844387076, 1.000000000000000000, 0.9330127018922194093, 0.9330127018922194093 ) ) 
 REPRESENTATION_ITEM ( '' )  );
#99183 = CARTESIAN_POINT ( 'NONE',  ( 0.02921319935947005314, -2.001080581411585513, 0.8940957790435491992 ) ) ;
#99184 = CARTESIAN_POINT ( 'NONE',  ( -0.03512515232485542011, -1.681152455970882809, -0.4250410675877940303 ) ) ;
#99185 = CARTESIAN_POINT ( 'NONE',  ( 3.405080638938757343, 1.739790774466195789, -1.357627211771177178 ) ) ;
#99186 = CARTESIAN_POINT ( 'NONE',  ( 1.006951398661716901, 0.6282198290366995952, 2.078224816918782025 ) ) ;
#99187 = CARTESIAN_POINT ( 'NONE',  ( 1.123270288254022198, 3.158552654332631882, -0.7749999999939810591 ) ) ;
#99188 = CARTESIAN_POINT ( 'NONE',  ( 1.921263159425983913, -1.888806403119867916, 0.9570566162820994816 ) ) ;
#99189 = CARTESIAN_POINT ( 'NONE',  ( 6.727182134110222478, 7.629137130509071163, 2.789055895399249252 ) ) ;
#99190 = CARTESIAN_POINT ( 'NONE',  ( 5.825206220505295462, -0.04701585971965925592, 1.925982856303788182 ) ) ;
#99191 = EDGE_LOOP ( 'NONE', ( #179598, #208662, #35957, #180985, #87992 ) ) ;
#99193 = CARTESIAN_POINT ( 'NONE',  ( -0.6823417656250003738, -0.4697916663252491021, -1.181850606188749264 ) ) ;
#99192 = CARTESIAN_POINT ( 'NONE',  ( 2.191363998320290385, 1.774703082125920428, 1.451028844865470901 ) ) ;
#99194 = CARTESIAN_POINT ( 'NONE',  ( 2.984766373302843778, 6.633977868828633717, -0.7998128361456291469 ) ) ;
#99195 = CARTESIAN_POINT ( 'NONE',  ( 3.655894977179307226, 7.416961240017848844, -0.7998128361456291469 ) ) ;
#99196 = EDGE_CURVE ( 'NONE', #58494, #87474, #60570, .T. ) ;
#99197 = CARTESIAN_POINT ( 'NONE',  ( 5.215582523826345351, 1.815199501411597582, 1.280085896050622507 ) ) ;
#99198 = CARTESIAN_POINT ( 'NONE',  ( -6.561783159334121152, 10.59923808595773664, -0.7216878364870278340 ) ) ;
#99199 = CARTESIAN_POINT ( 'NONE',  ( 0.2435857797690321180, -7.709701271428945901, -10.99755231369147168 ) ) ;
#99200 = AXIS2_PLACEMENT_3D ( 'NONE', #89655, #140560, #25689 ) ;
#99201 = CARTESIAN_POINT ( 'NONE',  ( 5.992340707560160240, 7.053780915984068756, 1.082531754730558626 ) ) ;
#99202 = CARTESIAN_POINT ( 'NONE',  ( -8.012505595552038784, 8.450270737673262644, 0.7216878364870578100 ) ) ;
#99203 = CARTESIAN_POINT ( 'NONE',  ( 4.665414256878284149, 6.536345614481700927, -1.443375672974068769 ) ) ;
#99205 = ORIENTED_EDGE ( 'NONE', *, *, #25220, .T. ) ;
#99204 = VECTOR ( 'NONE', #192160, 1000.000000000000000 ) ;
#99206 = CARTESIAN_POINT ( 'NONE',  ( 2.795546247670523954, 1.458556481301529706, -1.392545902517070111 ) ) ;
#99208 = CARTESIAN_POINT ( 'NONE',  ( 1.428664617098963863, -1.311459235982143534, 1.591897985181329966 ) ) ;
#99207 = CARTESIAN_POINT ( 'NONE',  ( 5.438792177376376991, 9.497007973581119700, 1.040834085586084257E-14 ) ) ;
#99209 = CARTESIAN_POINT ( 'NONE',  ( -11.89844258446855285, 13.82852689329959439, 1.560502987793273233 ) ) ;
#99210 = CARTESIAN_POINT ( 'NONE',  ( 6.034787771414195312, 6.213209619504250547, -0.7216878364870458196 ) ) ;
#99211 = CARTESIAN_POINT ( 'NONE',  ( -6.389500218612176319, -8.186910008818838236, -7.047919418996370311 ) ) ;
#99212 = CARTESIAN_POINT ( 'NONE',  ( -1.001543065824772872E-14, 4.321875000341417916, 1.575800808251672791 ) ) ;
#99213 = CARTESIAN_POINT ( 'NONE',  ( 3.714928722721734911, -0.1615716889580356697, 2.185543052782303874 ) ) ;
#99214 = CARTESIAN_POINT ( 'NONE',  ( 1.125625214514534900, 0.3961039030971893471, 1.976955501819408711 ) ) ;
#99215 = CARTESIAN_POINT ( 'NONE',  ( 1.364538772237647413, 0.1349417713633893900, -1.836341338755695940 ) ) ;
#99216 = CARTESIAN_POINT ( 'NONE',  ( 4.470543924053159479, -0.002573283451708791025, -1.841320590191763973 ) ) ;
#99217 = CARTESIAN_POINT ( 'NONE',  ( 7.527801604085637699, 9.805521176231838609, 1.599625672291281386 ) ) ;
#99218 = EDGE_CURVE ( 'NONE', #161364, #187417, #158655, .T. ) ;
#99219 = CARTESIAN_POINT ( 'NONE',  ( 4.735264887803245060, -1.668767028523497675, 0.7406363711058363553 ) ) ;
#99220 = CARTESIAN_POINT ( 'NONE',  ( 5.871720251644387822, -0.2986239867289949834, -1.994071864161291119 ) ) ;
#99221 = CARTESIAN_POINT ( 'NONE',  ( -7.316596452869116973, 11.68777962832266049, 0.7998128361456481317 ) ) ;
#99223 = CARTESIAN_POINT ( 'NONE',  ( -7.306918443122272677, 7.489436036589583345, 0.7998128361456341429 ) ) ;
#99222 = CARTESIAN_POINT ( 'NONE',  ( 4.276442053719103242, -1.305714526237568229, 1.847550228136185302 ) ) ;
#99224 = CARTESIAN_POINT ( 'NONE',  ( 0.5046868689226053917, -0.7117215327378585421, -1.982300686916990573 ) ) ;
#99225 = CARTESIAN_POINT ( 'NONE',  ( -6.400331034103001748, 9.624747418832267698, 1.199719254218452935 ) ) ;
#99226 = CARTESIAN_POINT ( 'NONE',  ( 4.299325596424930396, -1.802881993240162961, 1.017688063649782482 ) ) ;
#99227 = CARTESIAN_POINT ( 'NONE',  ( 8.218213668177886788, 12.73966637951625813, 0.7998128361456462443 ) ) ;
#99228 = DIRECTION ( 'NONE',  ( 5.578564026256490882E-16, 1.000000000000000000, 9.066213480720158442E-32 ) ) ;
#99229 = APPLICATION_PROTOCOL_DEFINITION ( 'draft international standard', 'automotive_design', 1998, #60163 ) ;
#99230 = CARTESIAN_POINT ( 'NONE',  ( -6.665805079413154921, 10.92852302595736447, 0.7998128361456481317 ) ) ;
#99231 = UNCERTAINTY_MEASURE_WITH_UNIT (LENGTH_MEASURE( 1.000000000000000082E-05 ), #194148, 'distance_accuracy_value', 'NONE');
#99232 = CARTESIAN_POINT ( 'NONE',  ( 11.06298571000738917, 11.25678692636136979, 0.9087567263023067499 ) ) ;
#99233 = CARTESIAN_POINT ( 'NONE',  ( 5.989670002187236442, 10.20997511251894529, -0.7998128361456481317 ) ) ;
#99234 = CARTESIAN_POINT ( 'NONE',  ( 5.016205007133085481, 6.569753085731051989, -1.234251006731339917 ) ) ;
#99235 = CARTESIAN_POINT ( 'NONE',  ( -10.49364770729726359, 11.34493653470939023, 0.7216878364870438212 ) ) ;
#99237 = CARTESIAN_POINT ( 'NONE',  ( 1.740793075861684303, 1.274151022659695709, -1.819517169034337467 ) ) ;
#99236 = CARTESIAN_POINT ( 'NONE',  ( 0.9320672075895162223, -2.067649466203642206, 0.4702014512557165515 ) ) ;
#99238 = FACE_OUTER_BOUND ( 'NONE', #206064, .T. ) ;
#99239 = CARTESIAN_POINT ( 'NONE',  ( -8.072954122294394352, 8.383144328957069291, -0.7998128361456362523 ) ) ;
#99240 = CARTESIAN_POINT ( 'NONE',  ( 6.745345117998789775, 7.828323044875442172, 1.199719254218462483 ) ) ;
#99241 = CARTESIAN_POINT ( 'NONE',  ( 2.875390130891414042, -0.1950805366632331617, 1.952157403750237163 ) ) ;
#99242 = CARTESIAN_POINT ( 'NONE',  ( 5.636439174979242850, 7.598931675607687453, -1.599625672291262513 ) ) ;
#99243 = CARTESIAN_POINT ( 'NONE',  ( -4.026828402897194792, 7.608452879803509816, -0.2354461595876176927 ) ) ;
#99244 = CARTESIAN_POINT ( 'NONE',  ( 3.497113557321089861, 6.167384019261527683, -1.199719254218446718 ) ) ;
#99245 = CARTESIAN_POINT ( 'NONE',  ( -5.424670859243583720, 8.382514198209223721, 1.082531754730550855 ) ) ;
#99246 = CARTESIAN_POINT ( 'NONE',  ( -6.887178846062105286, 10.97886638714038554, -0.7216878364870267237 ) ) ;
#99247 =( BOUNDED_CURVE ( )  B_SPLINE_CURVE ( 2, ( #155299, #156375, #106599 ),
 .UNSPECIFIED., .F., .T. ) 
 B_SPLINE_CURVE_WITH_KNOTS ( ( 3, 3 ),
 ( 0.5249999999999998002, 0.5283518216537415046 ),
 .UNSPECIFIED. ) 
 CURVE ( )  GEOMETRIC_REPRESENTATION_ITEM ( )  RATIONAL_B_SPLINE_CURVE ( ( 1.000000000000003553, 0.9461129256824096778, 0.9355746183778924641 ) ) 
 REPRESENTATION_ITEM ( '' )  );
#99248 = CARTESIAN_POINT ( 'NONE',  ( 2.232824136269210502, 1.381628265877183903, -1.608862310199298928 ) ) ;
#99249 = CARTESIAN_POINT ( 'NONE',  ( -6.961185525973791144, 7.086080966583015339, 0.7998128361456341429 ) ) ;
#99250 = CARTESIAN_POINT ( 'NONE',  ( 4.756279191188107269, -1.961398630904508833, -0.05015466537350299348 ) ) ;
#99251 = CARTESIAN_POINT ( 'NONE',  ( 2.782270202741622178, -1.112240752214749273, 1.853481441253836071 ) ) ;
#99252 = CARTESIAN_POINT ( 'NONE',  ( 2.718100415690410721, 1.734538518968967935, 0.6181264464550640936 ) ) ;
#99253 = CARTESIAN_POINT ( 'NONE',  ( -4.088362842241233253, 7.522098425605555860, -0.5455919966513862462 ) ) ;
#99254 = CARTESIAN_POINT ( 'NONE',  ( 3.497640442201256139, 7.024404915969360452, 1.040834085586084257E-14 ) ) ;
#99255 = CARTESIAN_POINT ( 'NONE',  ( 4.646296158022299672, -1.395249218123927104, 1.039982334504330197 ) ) ;
#99256 = CARTESIAN_POINT ( 'NONE',  ( -1.878313713276733132, 14.99999999999692157, -12.68000002627077905 ) ) ;
#99257 = CARTESIAN_POINT ( 'NONE',  ( 5.043269954603547767, 4.986162489899998995, -0.7216878364870197293 ) ) ;
#99258 = CARTESIAN_POINT ( 'NONE',  ( -10.47476631618627252, 5.237304525980054137, 5.169966676860812349 ) ) ;
#99259 = CIRCLE ( 'NONE', #5817, 9.999999999999998224 ) ;
#99260 = CARTESIAN_POINT ( 'NONE',  ( 1.340939272977889951, 0.4221563536682856332, 2.119910705745978508 ) ) ;
#99261 = CARTESIAN_POINT ( 'NONE',  ( 4.165388622617651748, -0.6297791189726584804, -1.915306643112117291 ) ) ;
#99262 = CARTESIAN_POINT ( 'NONE',  ( -7.497295758232712437, 11.69066945133944380, -0.7216878364870267237 ) ) ;
#99263 = CARTESIAN_POINT ( 'NONE',  ( 1.551884642779034262, 0.6273040060550126862, -2.068667048528524344 ) ) ;
#99264 = CARTESIAN_POINT ( 'NONE',  ( 3.326987498081665162, 0.04702425985559504501, 1.971060134238045602 ) ) ;
#99265 = CARTESIAN_POINT ( 'NONE',  ( 2.671113287583181339, 0.1005484070672260644, -1.968930098583418387 ) ) ;
#99266 = CARTESIAN_POINT ( 'NONE',  ( 6.509000000000021657, 1.267728212239338959, 2.115804336118334295 ) ) ;
#99267 = CARTESIAN_POINT ( 'NONE',  ( 3.368632357871951033, 0.04486925901568206143, -1.941695523777670740 ) ) ;
#99270 = VERTEX_POINT ( 'NONE', #87652 ) ;
#99269 = CARTESIAN_POINT ( 'NONE',  ( -3.187575512988701565, 6.732938841879847480, 0.000000000000000000 ) ) ;
#99268 = CARTESIAN_POINT ( 'NONE',  ( -10.60211293576223213, 11.47147930125185589, 1.040834085586084257E-14 ) ) ;
#99271 = AXIS2_PLACEMENT_3D ( 'NONE', #115506, #165258, #49387 ) ;
#99272 = CARTESIAN_POINT ( 'NONE',  ( -5.126391479298592735, 5.153413945369351268, 0.000000000000000000 ) ) ;
#99273 = CARTESIAN_POINT ( 'NONE',  ( 5.585032934186686226, 5.480569609498057382, 0.000000000000000000 ) ) ;
#99274 = CARTESIAN_POINT ( 'NONE',  ( -4.633854640820660009, 8.628190524257904670, -0.7998128361456362523 ) ) ;
#99275 = CARTESIAN_POINT ( 'NONE',  ( -8.622622508166983835, 13.00355065959610279, 1.040834085586084257E-14 ) ) ;
#99276 = CARTESIAN_POINT ( 'NONE',  ( 1.132168909276673796, -1.401036632855560349, -1.704990472574128502 ) ) ;
#99278 = EDGE_CURVE ( 'NONE', #175693, #99756, #171024, .T. ) ;
#99277 = CARTESIAN_POINT ( 'NONE',  ( 1.642778471875000035, -3.376041666188708046, -2.845375778867859751 ) ) ;
#99279 = CARTESIAN_POINT ( 'NONE',  ( 5.647302737930705696, 1.731814717071546772, -0.9215059220915235993 ) ) ;
#99280 = ORIENTED_EDGE ( 'NONE', *, *, #192402, .T. ) ;
#99281 = CARTESIAN_POINT ( 'NONE',  ( 3.327469932021313692, -1.606305723110455608, -1.379610029357878798 ) ) ;
#99282 = CARTESIAN_POINT ( 'NONE',  ( -0.7500000000000006661, 3.139583334016149418, -1.299038105676652011 ) ) ;
#99284 = CARTESIAN_POINT ( 'NONE',  ( -6.254388934605767503, 6.191208599995166040, 0.7998128361456341429 ) ) ;
#99283 = CARTESIAN_POINT ( 'NONE',  ( 0.07479286986305369589, 0.2526433113205875935, -1.890777245541554574 ) ) ;
#99285 = CARTESIAN_POINT ( 'NONE',  ( 4.013478867934616723, -0.9481684062532383939, -1.578073411074693899 ) ) ;
#99286 = ORIENTED_EDGE ( 'NONE', *, *, #8612, .F. ) ;
#99287 = CARTESIAN_POINT ( 'NONE',  ( -9.104463846776669200, 10.58062822844965645, -1.199719254218441611 ) ) ;
#99288 = CARTESIAN_POINT ( 'NONE',  ( 0.3405876332337480772, 3.079852035184937886, 0.4461735512527765790 ) ) ;
#99289 = CARTESIAN_POINT ( 'NONE',  ( 5.062787373817618786, 0.6179034821891697948, 2.028544477791139222 ) ) ;
#99290 =( NAMED_UNIT ( * ) SI_UNIT ( $, .STERADIAN. ) SOLID_ANGLE_UNIT ( ) );
#99291 = CARTESIAN_POINT ( 'NONE',  ( 5.931855901178834323, 6.879252291918818152, 1.199719254218462483 ) ) ;
#99292 = CARTESIAN_POINT ( 'NONE',  ( 5.712203248095857333, -0.9225367590200548307, -1.842806303608224949 ) ) ;
#99295 = CARTESIAN_POINT ( 'NONE',  ( 1.979791773625012352, -1.805961398883266344, -0.3578489297004632808 ) ) ;
#99294 = CARTESIAN_POINT ( 'NONE',  ( 0.6251817401201573698, 0.1879592460329523318, -1.851551742960926727 ) ) ;
#99293 = CARTESIAN_POINT ( 'NONE',  ( 2.482948226198858688, 5.072301959192136778, -2.419999999999995044 ) ) ;
#99296 = CARTESIAN_POINT ( 'NONE',  ( 7.527801604085637699, 9.805521176231838609, 1.599625672291281386 ) ) ;
#99297 = DIRECTION ( 'NONE',  ( 1.000000000000000000, 0.000000000000000000, 0.000000000000000000 ) ) ;
#99298 = CARTESIAN_POINT ( 'NONE',  ( -7.445362632559989535, 8.715286488521982733, 1.199719254218452047 ) ) ;
#99300 = EDGE_LOOP ( 'NONE', ( #153577, #64138, #143327, #150158, #24812 ) ) ;
#99299 = CARTESIAN_POINT ( 'NONE',  ( -0.04234008746932169803, -7.776896528353619331, -9.555169238417182243 ) ) ;
#99301 = CARTESIAN_POINT ( 'NONE',  ( 3.106307083854151774, -2.204334110825040494, 0.1085914373066959593 ) ) ;
#99302 = CARTESIAN_POINT ( 'NONE',  ( 4.604895111943496211, 1.752856212930454127, -1.430419756957083566 ) ) ;
#99303 = CARTESIAN_POINT ( 'NONE',  ( -6.155038550924159857, 8.203964280876741455, 1.443375672974078761 ) ) ;
#99304 = CARTESIAN_POINT ( 'NONE',  ( 4.447391390197759975, -1.653601938829275975, 0.7403539279892316083 ) ) ;
#99305 = CARTESIAN_POINT ( 'NONE',  ( 5.559766488213514712, 1.146785110015311915, 1.534377285673252267 ) ) ;
#99306 = CARTESIAN_POINT ( 'NONE',  ( 0.6823417656249899377, 5.238541667008086655, -1.181850606188754593 ) ) ;
#99307 = CARTESIAN_POINT ( 'NONE',  ( 5.067206508511894469, 0.1826785619755930679, -1.861722072867748823 ) ) ;
#99308 = CARTESIAN_POINT ( 'NONE',  ( 4.932013296703669170, 1.071099452130529039, 1.521725064211083112 ) ) ;
#99309 = CARTESIAN_POINT ( 'NONE',  ( -1.364683531250010295, 5.238541667008086655, -0.7879004041258300672 ) ) ;
#99310 = CARTESIAN_POINT ( 'NONE',  ( 6.139478286200317214, -1.284810642169451622, -1.217457132491184035 ) ) ;
#99311 = CARTESIAN_POINT ( 'NONE',  ( -0.06521966986864842497, -1.616690375843790051, 1.205047459138554045 ) ) ;
#99313 = CARTESIAN_POINT ( 'NONE',  ( 2.719469050394443421, -0.2056238487441063856, 2.096000168696035448 ) ) ;
#99312 = CARTESIAN_POINT ( 'NONE',  ( -3.809477975315625375, 4.507107728365378208, 1.082531754730558626 ) ) ;
#99314 = CARTESIAN_POINT ( 'NONE',  ( 10.07100917685271035, 10.64393221595000938, 0.7998128361456462443 ) ) ;
#99316 = CARTESIAN_POINT ( 'NONE',  ( 7.034482758620714371, 5.227586206896606136, 1.214306433183764966E-14 ) ) ;
#99315 = DIRECTION ( 'NONE',  ( 0.000000000000000000, 1.000000000000000000, 0.000000000000000000 ) ) ;
#99318 = EDGE_CURVE ( 'NONE', #27864, #155393, #147642, .T. ) ;
#99317 = CARTESIAN_POINT ( 'NONE',  ( 1.459246395511590189, -1.704040126542965661, 1.084046338683493982 ) ) ;
#99319 = CARTESIAN_POINT ( 'NONE',  ( -1.364683531250012516, 2.780208333674754506, 0.7879004041258379498 ) ) ;
#99320 = CARTESIAN_POINT ( 'NONE',  ( 4.039439701867726384, 6.800097854565950506, 1.199719254218462483 ) ) ;
#99321 = ORIENTED_EDGE ( 'NONE', *, *, #162091, .T. ) ;
#99322 = CARTESIAN_POINT ( 'NONE',  ( 2.776834730583700228, -2.067601613962879448, -0.6303956341740593050 ) ) ;
#99323 = CARTESIAN_POINT ( 'NONE',  ( 6.610000000000030518, 1.266345627986571021, 2.115470293623383569 ) ) ;
#99325 = DIRECTION ( 'NONE',  ( 1.000000000000000000, -0.000000000000000000, -0.000000000000000000 ) ) ;
#99324 = CARTESIAN_POINT ( 'NONE',  ( 3.088225128862704949, 6.824956093640315302, 0.7998128361456281477 ) ) ;
#99326 = CARTESIAN_POINT ( 'NONE',  ( 8.392133896734652154, 12.73464727959172293, 0.7216878364870438212 ) ) ;
#99327 = CARTESIAN_POINT ( 'NONE',  ( -7.834474503270852708, -6.459788825448645078, 7.722692672890439702 ) ) ;
#99328 = CARTESIAN_POINT ( 'NONE',  ( -8.527715433315703919, 9.051348881730875817, 1.040834085586084257E-14 ) ) ;
#99329 = EDGE_CURVE ( 'NONE', #121012, #29173, #127002, .T. ) ;
#99331 = CARTESIAN_POINT ( 'NONE',  ( 0.8025787753177977546, 1.655945718051672566, -1.435626523826734280 ) ) ;
#99330 = B_SPLINE_CURVE_WITH_KNOTS ( 'NONE', 3,
 ( #38151, #167089, #104223, #170270, #18680, #107485, #8839, #58665, #12035, #27219, #190779 ),
 .UNSPECIFIED., .F., .F.,
 ( 4, 1, 1, 1, 1, 1, 1, 1, 4 ),
 ( 0.000000000000000000, 0.2254179815473072723, 0.3971144120416517653, 0.5241699701252212629, 0.6156743509408303394, 0.6807935377546089351, 0.7289379548928518471, 0.7696256121123346006, 1.000000000000000000 ),
 .UNSPECIFIED. ) ;
#99332 = CARTESIAN_POINT ( 'NONE',  ( 0.006913841192815062958, 8.234242197375175820, 1.999988128101762408 ) ) ;
#99333 = CARTESIAN_POINT ( 'NONE',  ( 1.059873865361460332, 0.4390357074517194369, -2.219354932451859330 ) ) ;
#99334 = CARTESIAN_POINT ( 'NONE',  ( -7.157815033010924921, 10.43820240756634199, 1.199719254218453823 ) ) ;
#99335 = CARTESIAN_POINT ( 'NONE',  ( -4.026408433134269771, 6.680931691089825541, 1.082531754730560403 ) ) ;
#99336 = CARTESIAN_POINT ( 'NONE',  ( -1.364683531250012516, 2.801041667008090652, -0.7879004041258289570 ) ) ;
#99337 = CARTESIAN_POINT ( 'NONE',  ( 4.713861384769566953, 8.227931952640012980, -0.6562286284988675389 ) ) ;
#99338 = CARTESIAN_POINT ( 'NONE',  ( 0.7500000000000006661, 11.66666666666666607, -1.299038105676657340 ) ) ;
#99339 = CARTESIAN_POINT ( 'NONE',  ( 3.770049233051776749, 6.556085317605844232, 1.199719254218451159 ) ) ;
#99340 = CARTESIAN_POINT ( 'NONE',  ( 3.655294433216628391, 0.4326292253380575881, -1.715882644387234590 ) ) ;
#99341 = CARTESIAN_POINT ( 'NONE',  ( 6.563508857876433567, 0.3837567690821128696, -2.173003994120882076 ) ) ;
#99342 = CARTESIAN_POINT ( 'NONE',  ( -0.6823417656250039265, 14.38020833367473195, -1.181850606188755259 ) ) ;
#99343 = EDGE_LOOP ( 'NONE', ( #170738, #105357, #167042, #193101 ) ) ;
#99344 = CARTESIAN_POINT ( 'NONE',  ( -4.776215253764153346, 8.794277906025310898, -0.7998128361456362523 ) ) ;
#99345 = CARTESIAN_POINT ( 'NONE',  ( 5.325796065338770369, 0.8146125389149364571, -1.844717355016491478 ) ) ;
#99346 = ORIENTED_EDGE ( 'NONE', *, *, #20908, .F. ) ;
#99347 = CARTESIAN_POINT ( 'NONE',  ( 2.940157781200231746, 1.856316385841882965, 0.2306766016651334850 ) ) ;
#99348 = CARTESIAN_POINT ( 'NONE',  ( 3.327070777303439364, -1.911029926764183040, -0.7966718667702379353 ) ) ;
#99349 = EDGE_CURVE ( 'NONE', #62746, #57689, #57235, .T. ) ;
#99350 = CARTESIAN_POINT ( 'NONE',  ( -7.065207446052809814, 9.336104335185325453, -1.443375672974066548 ) ) ;
#99351 = CARTESIAN_POINT ( 'NONE',  ( 1.670022949053862948, 1.907054940702714863, -0.1439945843566131367 ) ) ;
#99352 = LINE ( 'NONE', #67867, #171129 ) ;
#99353 = VECTOR ( 'NONE', #198421, 1000.000000000000000 ) ;
#99354 = CARTESIAN_POINT ( 'NONE',  ( -10.81015953665327345, 5.524082113754967160, -6.547048903644186346 ) ) ;
#99355 = CARTESIAN_POINT ( 'NONE',  ( 0.2333690889706717397, 7.629137130509078268, -2.653349640194931247 ) ) ;
#99356 = CARTESIAN_POINT ( 'NONE',  ( -1.201851678989727383E-14, 4.134375000341417028, 1.575800808251672791 ) ) ;
#99357 = CARTESIAN_POINT ( 'NONE',  ( 0.9844543725016400293, -1.211084316286781037, 1.480072698922259677 ) ) ;
#99358 = CARTESIAN_POINT ( 'NONE',  ( 5.506019780925567986, 8.477421273504887722, -1.082531754730548412 ) ) ;
#99359 = CARTESIAN_POINT ( 'NONE',  ( 3.297265573180406584, -1.731424309613574852, 0.9225008839797432802 ) ) ;
#99360 = DIRECTION ( 'NONE',  ( 0.7592566023653005702, 0.6507913734559639396, 0.000000000000000000 ) ) ;
#99361 = CARTESIAN_POINT ( 'NONE',  ( -3.637330350216213759, 7.465578851886037093, -0.7998128361456481317 ) ) ;
#99362 = CARTESIAN_POINT ( 'NONE',  ( 5.765915565743810589, 0.6138260544302426291, -2.029845472315944921 ) ) ;
#99363 = CARTESIAN_POINT ( 'NONE',  ( 8.992082194361556091, 11.51384853155376220, 1.599625672291279388 ) ) ;
#99364 = CARTESIAN_POINT ( 'NONE',  ( 6.872342997630815020, -1.214913955043941174, 1.553259342649115249 ) ) ;
#99365 = CARTESIAN_POINT ( 'NONE',  ( 1.364683531249988535, 2.613541667008089764, 0.7879004041258500513 ) ) ;
#99366 = CARTESIAN_POINT ( 'NONE',  ( 2.021741635325131625, -0.4369018484469379682, 1.965087169840364245 ) ) ;
#99368 = CARTESIAN_POINT ( 'NONE',  ( 0.7556430218940900501, 2.039295976802601995, -0.5688827987148316057 ) ) ;
#99367 = CARTESIAN_POINT ( 'NONE',  ( -7.388830529767770550, 7.722649827591604677, 1.040834085586084257E-14 ) ) ;
#99369 = LINE ( 'NONE', #180604, #7651 ) ;
#99370 = CARTESIAN_POINT ( 'NONE',  ( 2.840353284027045344, -1.066491845456703835, 1.774417039089710935 ) ) ;
#99371 = CARTESIAN_POINT ( 'NONE',  ( 5.598591087800349086, 5.496387455380669529, -0.7998128361456481317 ) ) ;
#99373 = CARTESIAN_POINT ( 'NONE',  ( 5.040934186182656873, 4.775511393501539636, 1.040834085586084257E-14 ) ) ;
#99372 = CARTESIAN_POINT ( 'NONE',  ( 6.281206920390010495, 1.440802673026912117, 1.515107276980606654 ) ) ;
#99375 = ORIENTED_EDGE ( 'NONE', *, *, #51127, .T. ) ;
#99374 = CARTESIAN_POINT ( 'NONE',  ( 4.032112419961201510, 0.9767663869549062516, -1.542106374223570775 ) ) ;
#99376 = CARTESIAN_POINT ( 'NONE',  ( 9.565441069641300587, 11.11843498845840905, -1.199719254218440723 ) ) ;
#99377 = CARTESIAN_POINT ( 'NONE',  ( 6.890000000000007674, 6.036127733823692054, 2.594896729422516923 ) ) ;
#99378 = CARTESIAN_POINT ( 'NONE',  ( 10.43308898320764833, 8.755712671243168543, -3.803521280157781792 ) ) ;
#99379 = CARTESIAN_POINT ( 'NONE',  ( 5.860442804830619856, 0.8892231252738895808, 2.019869304780027353 ) ) ;
#99380 = CARTESIAN_POINT ( 'NONE',  ( -1.364683531250014514, 10.90104166700806942, -0.7879004041258335089 ) ) ;
#99381 = ORIENTED_EDGE ( 'NONE', *, *, #92162, .F. ) ;
#99382 = CARTESIAN_POINT ( 'NONE',  ( 3.738835060935014276, 1.816739721148411757, 0.5971339541979635568 ) ) ;
#99384 = CARTESIAN_POINT ( 'NONE',  ( -8.611400122974211868, 13.19838391011195888, 1.040834085586084257E-14 ) ) ;
#99383 = COLOUR_RGB ( '', 0.72549020, 0.75294118, 0.79215686) ;
#99385 = CARTESIAN_POINT ( 'NONE',  ( 8.308449207076147758, 8.587612251210650527, -0.7998128361456281477 ) ) ;
#99386 = CARTESIAN_POINT ( 'NONE',  ( 1.360316468749978469, 1.046875000341403128, -2.602085213965210642E-14 ) ) ;
#99387 = CARTESIAN_POINT ( 'NONE',  ( 3.660338285565247762, 7.214219066560688454, 1.040834085586084257E-14 ) ) ;
#99388 = CARTESIAN_POINT ( 'NONE',  ( 6.532779862045914321, -1.958661757936002612, 0.9833580883553474372 ) ) ;
#99389 = FACE_OUTER_BOUND ( 'NONE', #20636, .T. ) ;
#99390 = CARTESIAN_POINT ( 'NONE',  ( 0.3800845246329161431, -0.2246070939678334044, -1.827447590993152682 ) ) ;
#99391 = EDGE_LOOP ( 'NONE', ( #159936, #52396, #48407, #66299 ) ) ;
#99392 = CARTESIAN_POINT ( 'NONE',  ( 5.044982899572335810, 7.898304261840563001, 1.131119777890549516 ) ) ;
#99393 = CARTESIAN_POINT ( 'NONE',  ( 4.850782132498069998, -1.503350029756752804, 1.112868480285071460 ) ) ;
#99394 = CARTESIAN_POINT ( 'NONE',  ( 0.7500000000000006661, 10.83333333333333393, 1.299038105676657340 ) ) ;
#99395 = CARTESIAN_POINT ( 'NONE',  ( -1.445103857048104512, 8.688264192037884470, -2.625611233228243524 ) ) ;
#99396 = CARTESIAN_POINT ( 'NONE',  ( -6.887178846062116833, 9.058127958537705027, -1.443375672974059665 ) ) ;
#99397 = CARTESIAN_POINT ( 'NONE',  ( 3.876741858503734761, 6.610283703974623393, 1.199719254218462483 ) ) ;
#99398 = CARTESIAN_POINT ( 'NONE',  ( 1.164831386079593134, 1.494809975433964100, -1.282432929305108438 ) ) ;
#99399 = CARTESIAN_POINT ( 'NONE',  ( 2.232046197884657968, 2.016035414700023676, 0.04665772616015140262 ) ) ;
#99400 = CARTESIAN_POINT ( 'NONE',  ( -8.843996274815957293, 9.212417163573759282, 1.040834085586084257E-14 ) ) ;
#99401 = CARTESIAN_POINT ( 'NONE',  ( 5.345657705538078730, 9.458627433094950021, 0.7998128361456331437 ) ) ;
#99402 = DIRECTION ( 'NONE',  ( 0.000000000000000000, 0.7999999999999973799, -0.6000000000000034195 ) ) ;
#99403 = CARTESIAN_POINT ( 'NONE',  ( 3.047022719409075986, -1.791863632763015968, -1.261349808265788797 ) ) ;
#99404 = DIRECTION ( 'NONE',  ( 0.000000000000000000, 0.000000000000000000, -1.000000000000000000 ) ) ;
#99405 = CARTESIAN_POINT ( 'NONE',  ( -4.783329267523015460, 4.474972321731942593, -0.7998128361456221525 ) ) ;
#99406 = CARTESIAN_POINT ( 'NONE',  ( 6.825078400183554272, 2.980425674467934272, 2.309322343017068402 ) ) ;
#99407 = CARTESIAN_POINT ( 'NONE',  ( -11.97929049433705373, 12.22000000000000064, -0.7046979865771834106 ) ) ;
#99408 = CARTESIAN_POINT ( 'NONE',  ( 3.743459811148990291, 7.381470523066878009, -0.7216878364870338292 ) ) ;
#99409 = CARTESIAN_POINT ( 'NONE',  ( 7.587759525142423911, 12.00413654597487501, 0.7998128361456462443 ) ) ;
#99410 = CARTESIAN_POINT ( 'NONE',  ( -1.608462485350604432, 8.735270501766748907, -2.463594439587635687 ) ) ;
#99411 = CARTESIAN_POINT ( 'NONE',  ( 4.909461021924231616, 8.741805268971372556, 0.7216878364870317197 ) ) ;
#99412 = EDGE_LOOP ( 'NONE', ( #21405, #193829, #177779, #87662 ) ) ;
#99414 = CARTESIAN_POINT ( 'NONE',  ( 0.8033857101962671443, 1.774305754185826034, -0.9510189173033887222 ) ) ;
#99413 = CARTESIAN_POINT ( 'NONE',  ( 4.792441439910442469, 1.527937338083688923, -1.027124420945781935 ) ) ;
#99415 = CARTESIAN_POINT ( 'NONE',  ( 2.935265884076414977, 1.227738246725296634, 1.942841054583419602 ) ) ;
#99417 = CARTESIAN_POINT ( 'NONE',  ( 1.147037741594110427, 1.644639672688326559, -0.8707446802224245719 ) ) ;
#99416 = CARTESIAN_POINT ( 'NONE',  ( 4.067082894419602468, 3.847277586352047862, -0.7216878364870188411 ) ) ;
#99418 = CARTESIAN_POINT ( 'NONE',  ( 3.285556943750000070, -3.434374999522042060, 0.000000000000000000 ) ) ;
#99419 = CARTESIAN_POINT ( 'NONE',  ( -4.386226389220933441, 5.076017861301227008, -1.199719254218446718 ) ) ;
#99420 = CARTESIAN_POINT ( 'NONE',  ( -0.02319159430949970652, 0.003959926571647092407, -1.810968101872318714 ) ) ;
#99421 = CARTESIAN_POINT ( 'NONE',  ( 4.535362393419643645, -0.08824616237496611670, 1.910463848342447202 ) ) ;
#99422 = CARTESIAN_POINT ( 'NONE',  ( -7.483210719738908168, 10.81783070874899799, 1.199719254218453823 ) ) ;
#99423 = CARTESIAN_POINT ( 'NONE',  ( -5.478903473698241378, 9.406154796041011679, -0.7216878364870338292 ) ) ;
#99425 = CARTESIAN_POINT ( 'NONE',  ( 2.746779440450992649, -1.556306552617524597, 1.037596984913228937 ) ) ;
#99424 = CARTESIAN_POINT ( 'NONE',  ( 3.192999258835881093, 1.649592175042478015, 1.284459162532962440 ) ) ;
#99426 = CARTESIAN_POINT ( 'NONE',  ( 8.446366511633696561, 8.956441806435218922, 1.040834085586084257E-14 ) ) ;
#99427 = CARTESIAN_POINT ( 'NONE',  ( -1.364683531250010740, 5.801041667008088432, -0.7879004041258300672 ) ) ;
#99428 = CARTESIAN_POINT ( 'NONE',  ( 6.040549724581927293, -1.551790349881351450, 0.9907606852931831742 ) ) ;
#99429 = CARTESIAN_POINT ( 'NONE',  ( 3.277320446201373638, 4.846626492033466072, 1.599625672291267398 ) ) ;
#99431 = CARTESIAN_POINT ( 'NONE',  ( 4.005544317833563461, 6.760553239859419250, -1.199719254218452047 ) ) ;
#99430 = DIRECTION ( 'NONE',  ( -3.491481338843133750E-15, -0.000000000000000000, -1.000000000000000000 ) ) ;
#99432 = CARTESIAN_POINT ( 'NONE',  ( 5.074679841287068172, -1.625846828454122983, -0.5764380256386961721 ) ) ;
#99433 = CARTESIAN_POINT ( 'NONE',  ( -7.549192604710863286, 7.701812881784464437, -0.7998128361456291469 ) ) ;
#99434 = CARTESIAN_POINT ( 'NONE',  ( 0.3517064098005295292, 0.1722828621854489983, -1.725525930370126249 ) ) ;
#99435 = DIRECTION ( 'NONE',  ( 0.000000000000000000, -1.000000000000000000, 0.000000000000000000 ) ) ;
#99436 = FILL_AREA_STYLE_COLOUR ( '', #27385 ) ;
#99437 = CARTESIAN_POINT ( 'NONE',  ( 4.522458045437067753, 1.018072405813482018, 1.917541202323807203 ) ) ;
#99438 = CARTESIAN_POINT ( 'NONE',  ( 3.228933428962964758, 0.04559371896543929631, 1.825288036790246204 ) ) ;
#99439 = CARTESIAN_POINT ( 'NONE',  ( 0.5847188370675902025, 1.875566754216885013, 0.5750099747552291918 ) ) ;
#99440 = CARTESIAN_POINT ( 'NONE',  ( 5.507064729579815854, -0.04930729212004316547, 2.116909390494752685 ) ) ;
#99441 = ORIENTED_EDGE ( 'NONE', *, *, #25840, .F. ) ;
#99443 = CARTESIAN_POINT ( 'NONE',  ( -1.201851678989727383E-14, 4.009375000341416140, -1.575800808251660134 ) ) ;
#99442 = CARTESIAN_POINT ( 'NONE',  ( 6.444901331192640193, -1.838261776244881185, -1.369441068571846554 ) ) ;
#99444 = CARTESIAN_POINT ( 'NONE',  ( 9.915090410295563927, 10.46202698829998567, -0.7998128361456281477 ) ) ;
#99445 = EDGE_CURVE ( 'NONE', #36910, #200036, #186464, .T. ) ;
#99446 = CARTESIAN_POINT ( 'NONE',  ( 1.506653248757179320, -2.110590818861147078, -0.2044851626497797559 ) ) ;
#99447 = CARTESIAN_POINT ( 'NONE',  ( -4.772106882330227506, 7.550913215151819458, -1.082531754730549967 ) ) ;
#99448 = CARTESIAN_POINT ( 'NONE',  ( -4.812781342726871969, 6.637997537979888563, 1.443375672974064550 ) ) ;
#99449 = CARTESIAN_POINT ( 'NONE',  ( 6.807499178464245126, -1.738453852359397978, -1.300317965242798968 ) ) ;
#99451 = CARTESIAN_POINT ( 'NONE',  ( 0.7500000000000006661, 13.19791666734946389, -1.299038105676657340 ) ) ;
#99450 = CARTESIAN_POINT ( 'NONE',  ( 6.883263157960369583, 7.629137130509070275, 2.653810918356712900 ) ) ;
#99453 = VERTEX_POINT ( 'NONE', #137483 ) ;
#99452 = CARTESIAN_POINT ( 'NONE',  ( 1.823182589357236205, 1.643363032943769397, -1.494666050352111863 ) ) ;
#99454 = CARTESIAN_POINT ( 'NONE',  ( 6.311172677262812059, 1.158691452862798954, -1.650079838712660063 ) ) ;
#99456 = CARTESIAN_POINT ( 'NONE',  ( 4.065324354713106381, 1.766439233411433163, 1.064669890786486661 ) ) ;
#99455 = CARTESIAN_POINT ( 'NONE',  ( 4.497554271431305040, 6.270232621468402989, -1.599625672291256295 ) ) ;
#99458 = CARTESIAN_POINT ( 'NONE',  ( -0.2408018239683913930, 0.6935112996086059134, -2.180753846165773169 ) ) ;
#99457 = CARTESIAN_POINT ( 'NONE',  ( 6.530187263637528439, 7.647581891445782709, -1.199719254218452047 ) ) ;
#99459 = CARTESIAN_POINT ( 'NONE',  ( 4.688087255275310561, 8.691461907788344377, -0.7998128361456381397 ) ) ;
#99460 = CARTESIAN_POINT ( 'NONE',  ( 3.285556943750000070, -3.171874999522043215, 0.000000000000000000 ) ) ;
#99461 = SURFACE_SIDE_STYLE ('',( #181749 ) ) ;
#99462 = CARTESIAN_POINT ( 'NONE',  ( 0.9024203131168639924, 1.581833000263275224, -1.367050110207337799 ) ) ;
#99463 = CARTESIAN_POINT ( 'NONE',  ( 4.177188522404684079, 1.205947341878073287, 1.391433828303423326 ) ) ;
#99464 = CARTESIAN_POINT ( 'NONE',  ( 5.626797444871351139, 6.523350759560078593, 1.199719254218462483 ) ) ;
#99465 = CARTESIAN_POINT ( 'NONE',  ( 1.781837903662389477, -0.9264376740152606704, 1.454631767934653208 ) ) ;
#99466 = CARTESIAN_POINT ( 'NONE',  ( 0.6027503803631119039, 1.865048444749048517, 0.7672877736318933772 ) ) ;
#99467 = CARTESIAN_POINT ( 'NONE',  ( 1.583111924021431305, -0.7688449931826674133, 2.166437542035759556 ) ) ;
#99468 = CARTESIAN_POINT ( 'NONE',  ( 1.364683531249988535, 4.426041667008082214, 0.7879004041258500513 ) ) ;
#99469 = CARTESIAN_POINT ( 'NONE',  ( 1.265308524177723326, -2.045349560253268084, -0.9672931750909097293 ) ) ;
#99470 = CARTESIAN_POINT ( 'NONE',  ( 4.494815117402239935, -0.4609086856197233684, -2.054844913126519401 ) ) ;
#99471 = CARTESIAN_POINT ( 'NONE',  ( -7.919371124158132602, 8.411890197705517380, -0.7216878364870338292 ) ) ;
#99472 = CARTESIAN_POINT ( 'NONE',  ( 2.811481186154769496, -1.751065702721636308, 0.2553572387639922447 ) ) ;
#99473 = CARTESIAN_POINT ( 'NONE',  ( 5.126954644262057492, 9.133197518281081173, 0.7998128361456462443 ) ) ;
#99474 = CARTESIAN_POINT ( 'NONE',  ( 6.333067150914820864, 6.561202228921677815, 0.7216878364870328300 ) ) ;
#99475 = CARTESIAN_POINT ( 'NONE',  ( 5.968750000000003553, 0.7852924748296689073, -1.895863743164208026 ) ) ;
#99476 = CARTESIAN_POINT ( 'NONE',  ( -6.410307701162927252, 6.373113827645189744, -0.7998128361456291469 ) ) ;
#99477 = UNCERTAINTY_MEASURE_WITH_UNIT (LENGTH_MEASURE( 1.000000000000000082E-05 ), #108248, 'distance_accuracy_value', 'NONE');
#99478 = CARTESIAN_POINT ( 'NONE',  ( -0.7500000000000215383, 2.441666666666689078, 1.299038105676671107 ) ) ;
#99479 = CARTESIAN_POINT ( 'NONE',  ( -4.569261463005423352, 5.289558780716470565, -1.199719254218446718 ) ) ;
#99480 = CARTESIAN_POINT ( 'NONE',  ( 5.080443840416010381, 1.095562506470529884, 1.932424796230156616 ) ) ;
#99481 = CARTESIAN_POINT ( 'NONE',  ( 3.627062487484993714, -2.024900418628313936, 0.8384617360315260726 ) ) ;
#99482 = CARTESIAN_POINT ( 'NONE',  ( -5.382750679825375251, 6.238629533673094585, -1.199719254218446718 ) ) ;
#99483 = CARTESIAN_POINT ( 'NONE',  ( -11.96533679318059917, 9.847539888129954733, 0.9151144679398905968 ) ) ;
#99484 = CARTESIAN_POINT ( 'NONE',  ( 6.076833508651091620, -1.499762292660647311, 1.499315088411487640 ) ) ;
#99485 = CARTESIAN_POINT ( 'NONE',  ( 1.364683531249990311, 3.884375000341417028, 1.214306433183764966E-14 ) ) ;
#99486 = CARTESIAN_POINT ( 'NONE',  ( 6.890000000000050306, -0.002781820520068867264, 1.999840353888074240 ) ) ;
#99487 = CARTESIAN_POINT ( 'NONE',  ( -3.633221978782283923, 7.182583375313884133, -0.7216878364870267237 ) ) ;
#99489 = CARTESIAN_POINT ( 'NONE',  ( 5.783468009189684622, 0.1541500780414573890, -2.115021274163720211 ) ) ;
#99488 = AXIS2_PLACEMENT_3D ( 'NONE', #35220, #101296, #169499 ) ;
#99490 = CARTESIAN_POINT ( 'NONE',  ( -5.302647476720585118, 9.200522799567075083, 0.000000000000000000 ) ) ;
#99491 = VERTEX_POINT ( 'NONE', #206718 ) ;
#99493 = CARTESIAN_POINT ( 'NONE',  ( 6.819229411136438657, -0.1619093195798972928, 2.126376854085454404 ) ) ;
#99492 = CARTESIAN_POINT ( 'NONE',  ( -5.668717624289589807, 5.786127781192186958, 0.7216878364870257245 ) ) ;
#99494 = CARTESIAN_POINT ( 'NONE',  ( 5.681030059326015014, 6.586622143090519188, -1.199719254218445830 ) ) ;
#99495 = CARTESIAN_POINT ( 'NONE',  ( 5.776868925826902590, 1.698781319366513998, -0.7106697882480541573 ) ) ;
#99496 = DIRECTION ( 'NONE',  ( 0.000000000000000000, -0.000000000000000000, 1.000000000000000000 ) ) ;
#99497 = CARTESIAN_POINT ( 'NONE',  ( 1.364683531249990311, 2.946875000341416140, 1.214306433183764966E-14 ) ) ;
#99498 = CARTESIAN_POINT ( 'NONE',  ( 1.100653536641453156, -0.4241352534964801801, 1.687842229193817989 ) ) ;
#99499 = CARTESIAN_POINT ( 'NONE',  ( 4.220665892555866883, 3.818531717603609987, -0.7998128361456211532 ) ) ;
#99500 = CARTESIAN_POINT ( 'NONE',  ( -6.776370306708066948, -7.161464053357560644, -6.781144757626046626 ) ) ;
#99501 = CARTESIAN_POINT ( 'NONE',  ( -0.6823417656250246877, -0.6364583329919113464, 1.181850606188755259 ) ) ;
#99502 = CARTESIAN_POINT ( 'NONE',  ( -4.229020061460118107, 7.343517960532633282, -0.8650006913940473385 ) ) ;
#99503 = CARTESIAN_POINT ( 'NONE',  ( 5.120075222393803749, -1.153228217640640985, -1.828211184805514922 ) ) ;
#99504 = CARTESIAN_POINT ( 'NONE',  ( -3.379006598303881059, 4.965260336153046516, -1.599625672291256295 ) ) ;
#99505 = CARTESIAN_POINT ( 'NONE',  ( -5.531363484251157203, 9.397081798360927607, 0.000000000000000000 ) ) ;
#99506 = CARTESIAN_POINT ( 'NONE',  ( 5.067319851952804655, 0.2155487944876262052, -2.150937003660175595 ) ) ;
#99508 = EDGE_LOOP ( 'NONE', ( #49030, #133047, #141103, #62054, #107320, #136632 ) ) ;
#99507 = CARTESIAN_POINT ( 'NONE',  ( 0.000000000000000000, 13.49999999999999822, 0.000000000000000000 ) ) ;
#99509 = CARTESIAN_POINT ( 'NONE',  ( -1.364683531249997417, 2.759375000341422801, 1.214306433183764966E-14 ) ) ;
#99510 = CARTESIAN_POINT ( 'NONE',  ( 6.204366038997092936, -0.7071694579776456324, -1.840334891991159738 ) ) ;
#99511 = CARTESIAN_POINT ( 'NONE',  ( 5.255145817263100483, -1.720984288211702795, -0.2101651147246290929 ) ) ;
#99513 = CARTESIAN_POINT ( 'NONE',  ( 1.997856853652695497, -2.190977152517746163, 0.05759783203293508680 ) ) ;
#99512 = CARTESIAN_POINT ( 'NONE',  ( 1.360316468749969587, -0.7343749996585879902, -3.642919299551294898E-14 ) ) ;
#99514 = CARTESIAN_POINT ( 'NONE',  ( 1.694772972888843210, -2.296637362782745218, -0.2246623637925919403 ) ) ;
#99515 = CARTESIAN_POINT ( 'NONE',  ( 4.376282966308748357, -1.189761084491423926, 1.682430632154131578 ) ) ;
#99516 = CARTESIAN_POINT ( 'NONE',  ( 6.585517519612275272, -0.8250364709028266130, 1.756089425624817180 ) ) ;
#99517 = CARTESIAN_POINT ( 'NONE',  ( -7.687109908824056426, 8.070642436490613747, 0.7216878364870438212 ) ) ;
#99518 = CARTESIAN_POINT ( 'NONE',  ( -4.085803189671902480, 5.860132702740892263, -1.599625672291271394 ) ) ;
#99519 = CARTESIAN_POINT ( 'NONE',  ( 3.972980863544761654, -1.569110274459505350, 1.426624754300914510 ) ) ;
#99520 = CARTESIAN_POINT ( 'NONE',  ( 9.579764304849151202, -9.999999999999994671, -0.06720017513373727214 ) ) ;
#99521 = CARTESIAN_POINT ( 'NONE',  ( 1.072888940501380839, -0.9041080511620370741, 1.802418165037560138 ) ) ;
#99522 = CARTESIAN_POINT ( 'NONE',  ( -7.849807752188049825, 8.260456587081938196, 0.7216878364870578100 ) ) ;
#99523 = CARTESIAN_POINT ( 'NONE',  ( 4.700333112842928429, -2.206180118464650786, -0.05804534286662357823 ) ) ;
#99524 = CARTESIAN_POINT ( 'NONE',  ( 3.285556943750000070, -1.421874999522041660, 0.000000000000000000 ) ) ;
#99525 = CARTESIAN_POINT ( 'NONE',  ( -1.123270288250318494, 3.235197346350006331, -0.7749999999993560929 ) ) ;
#99526 = DIRECTION ( 'NONE',  ( 0.000000000000000000, 0.000000000000000000, 1.000000000000000000 ) ) ;
#99527 = CARTESIAN_POINT ( 'NONE',  ( 7.005397802120315376, 5.950282834973755541, -2.500000000000000444 ) ) ;
#99529 = CARTESIAN_POINT ( 'NONE',  ( -0.1291982275798781721, -0.004298614154785804914, -2.073875112923000863 ) ) ;
#99528 = CARTESIAN_POINT ( 'NONE',  ( -5.281148723220589147, 7.765029056575591504, -1.308346332658766986 ) ) ;
#99530 = CARTESIAN_POINT ( 'NONE',  ( 0.09201470549763642037, 7.049384003815710287, 3.948455284462528248 ) ) ;
#99531 = VERTEX_POINT ( 'NONE', #58346 ) ;
#99532 = CARTESIAN_POINT ( 'NONE',  ( 3.379809591947144032, 1.306296513425331263, 1.594013207155994261 ) ) ;
#99533 = CARTESIAN_POINT ( 'NONE',  ( 1.360316468749963592, 1.286458333674704191, -0.7853790794158961308 ) ) ;
#99534 = CARTESIAN_POINT ( 'NONE',  ( -5.205440912643032547, 8.160432600470439723, 1.199719254218452047 ) ) ;
#99535 = CARTESIAN_POINT ( 'NONE',  ( 3.615882686718306260, -0.5843173316345972035, 1.933312988646131103 ) ) ;
#99536 = CARTESIAN_POINT ( 'NONE',  ( 1.499999999999987566, -0.9749999999999827693, 0.000000000000000000 ) ) ;
#99537 = CARTESIAN_POINT ( 'NONE',  ( 8.405692050792682224, 12.75046512599275772, -0.7216878364870328300 ) ) ;
#99538 = CARTESIAN_POINT ( 'NONE',  ( 2.254824865002862389, -1.593768082018555354, 1.306595953347834849 ) ) ;
#99539 = CARTESIAN_POINT ( 'NONE',  ( 5.412729640353754590, 7.337937218544611895, 1.599625672291267398 ) ) ;
#99540 = VECTOR ( 'NONE', #125461, 1000.000000000000000 ) ;
#99541 = CARTESIAN_POINT ( 'NONE',  ( -0.2411972340276230808, 0.2378665717568603510, -1.934216014300967235 ) ) ;
#99542 = CARTESIAN_POINT ( 'NONE',  ( 1.464538624043790316, 0.1369371521719800755, -1.836096087760468398 ) ) ;
#99543 = CARTESIAN_POINT ( 'NONE',  ( 6.199877634063251541, -0.7475181258948644381, 2.076568058718592624 ) ) ;
#99544 = CARTESIAN_POINT ( 'NONE',  ( 7.049313524462606395, 7.188896964819984525, 0.000000000000000000 ) ) ;
#99545 = CARTESIAN_POINT ( 'NONE',  ( 1.880366631079612549, -1.158069840294423392, 1.825029014904603342 ) ) ;
#99546 = CARTESIAN_POINT ( 'NONE',  ( -3.307826292054310890, 5.842585859829892314, -1.082531754730549967 ) ) ;
#99547 = CARTESIAN_POINT ( 'NONE',  ( 1.921111612355221654, -1.799121770747251547, 0.9110121207814986244 ) ) ;
#99548 = MECHANICAL_DESIGN_GEOMETRIC_PRESENTATION_REPRESENTATION (  '', ( #165247 ), #182403 ) ;
#99549 = CARTESIAN_POINT ( 'NONE',  ( -3.122502256758252770E-14, 3.499999999999961364, -3.816391647148975608E-14 ) ) ;
#99550 = CARTESIAN_POINT ( 'NONE',  ( 0.2329894512427649333, -1.712236961970284632, 0.7538099095961707796 ) ) ;
#99551 = CARTESIAN_POINT ( 'NONE',  ( 11.49966000274946332, 11.24232845564745809, 3.429881629453402248 ) ) ;
#99552 = CARTESIAN_POINT ( 'NONE',  ( 4.610209453490740295, -0.8421727957172200352, -1.782655373600953386 ) ) ;
#99553 = CARTESIAN_POINT ( 'NONE',  ( 3.942592416894859841, -1.490970858180175940, 1.357867534901323614 ) ) ;
#99555 = CARTESIAN_POINT ( 'NONE',  ( 8.229436053370658755, 12.54483312900040026, 0.7216878364870438212 ) ) ;
#99554 = CARTESIAN_POINT ( 'NONE',  ( -1.402160292154681736E-14, 2.196875000341423689, -1.575800808251660134 ) ) ;
#99557 = CARTESIAN_POINT ( 'NONE',  ( 6.199853529602823876, -0.7113111419616345854, 1.982453129600779462 ) ) ;
#99556 = CARTESIAN_POINT ( 'NONE',  ( -8.376239975144482486, 8.666701480623698828, 1.040834085586084257E-14 ) ) ;
#99558 = CARTESIAN_POINT ( 'NONE',  ( 4.984861949208964305, 1.980195279717174905, 0.6042863919064264122 ) ) ;
#99559 = CARTESIAN_POINT ( 'NONE',  ( 6.928380191783277908, 8.041863964290678624, 1.199719254218462483 ) ) ;
#99560 = CARTESIAN_POINT ( 'NONE',  ( -6.521635583373313061, 7.567328587812373719, -1.199719254218446718 ) ) ;
#99561 = CARTESIAN_POINT ( 'NONE',  ( 1.898923903056394913, 3.739065552179445806, -0.4000000000000273337 ) ) ;
#99562 = CARTESIAN_POINT ( 'NONE',  ( 5.256120111591911837, 0.8147005317804748570, -1.848364005614275163 ) ) ;
#99563 = B_SPLINE_CURVE_WITH_KNOTS ( 'NONE', 3,
 ( #214194, #29103, #130928, #212087, #180673, #143962, #112544, #196922, #49608, #31240, #98364, #113615, #78897, #209957, #145020, #178554, #96253, #197980, #48560, #146074, #45365, #63723 ),
 .UNSPECIFIED., .F., .F.,
 ( 4, 3, 3, 3, 3, 3, 3, 4 ),
 ( -1.454680003659494146E-06, 0.000000000000000000, 2.747234201904476952E-05, 5.316625080980220638E-05, 7.164957654724449416E-05, 8.369272870876657113E-05, 9.574357740276803535E-05, 0.0001078040709964530740 ),
 .UNSPECIFIED. ) ;
#99564 = CARTESIAN_POINT ( 'NONE',  ( -1.500000000000015099, -1.047916665983845919, 0.8660254037844403729 ) ) ;
#99565 = CARTESIAN_POINT ( 'NONE',  ( 3.493080449939501619, -0.4495562565045966852, -2.263328358674908003 ) ) ;
#99566 = CARTESIAN_POINT ( 'NONE',  ( 0.9540547974491294658, -0.7459001080754708024, 1.923128640884926410 ) ) ;
#99567 = CARTESIAN_POINT ( 'NONE',  ( 8.270110514656026979, 10.67154823856396817, 1.443375672974076540 ) ) ;
#99568 = CARTESIAN_POINT ( 'NONE',  ( 7.666209513884374438, 7.908608952478760834, 0.7998128361456281477 ) ) ;
#99569 = CARTESIAN_POINT ( 'NONE',  ( 5.520104819419390907, 6.469152373191302985, 1.199719254218452935 ) ) ;
#99570 = CARTESIAN_POINT ( 'NONE',  ( -0.6823417656250212460, 1.363541667008083547, 1.181850606188755259 ) ) ;
#99571 = CARTESIAN_POINT ( 'NONE',  ( 5.228604516725597229, 6.129068686715179126, -1.199719254218450271 ) ) ;
#99572 = CARTESIAN_POINT ( 'NONE',  ( 6.385527161912102123, 9.433236874664039817, -1.082531754730537976 ) ) ;
#99573 = CARTESIAN_POINT ( 'NONE',  ( 3.543588177981399134, 1.964110833604881812, -0.9256020844959752525 ) ) ;
#99574 = DIRECTION ( 'NONE',  ( 0.000000000000000000, 0.000000000000000000, 1.000000000000000000 ) ) ;
#99576 = CARTESIAN_POINT ( 'NONE',  ( 2.630204301513817455, 0.2276190002089127917, 1.827071974840013269 ) ) ;
#99575 = CARTESIAN_POINT ( 'NONE',  ( -4.202664430556263930, 5.926194473780837413, 1.443375672974064550 ) ) ;
#99577 = EDGE_CURVE ( 'NONE', #97860, #84679, #16275, .T. ) ;
#99578 = CARTESIAN_POINT ( 'NONE',  ( 1.364683531249988535, 4.363541667008090208, 0.7879004041258500513 ) ) ;
#99579 = CARTESIAN_POINT ( 'NONE',  ( 4.458633810090739225, -1.957822973221786444, -0.9849130632908836835 ) ) ;
#99580 = DIRECTION ( 'NONE',  ( -0.06086575749407437119, 0.9962285034897238045, 0.06183953750876716726 ) ) ;
#99581 = CARTESIAN_POINT ( 'NONE',  ( 4.540055829149266309, 0.9713072833863345412, -2.043554373614121289 ) ) ;
#99582 = CARTESIAN_POINT ( 'NONE',  ( -4.798872725802947770, 6.964071866812478362, -1.434128239971976138 ) ) ;
#99583 = CARTESIAN_POINT ( 'NONE',  ( 5.583942420111207561, 7.395222456726187943, -1.242479836444350783 ) ) ;
#99584 = CARTESIAN_POINT ( 'NONE',  ( -6.278834536460198734, 6.497930845391236332, 0.7216878364870257245 ) ) ;
#99585 = CARTESIAN_POINT ( 'NONE',  ( 5.587368702607580673, 5.691220705896524734, -0.7216878364870458196 ) ) ;
#99586 = CARTESIAN_POINT ( 'NONE',  ( 6.046140008783082109, 1.767849252625730783, 0.08484812824352709615 ) ) ;
#99587 = CARTESIAN_POINT ( 'NONE',  ( 4.565094110769337910, -1.615551665759178412, 1.200850101804177283 ) ) ;
#99588 = CARTESIAN_POINT ( 'NONE',  ( 7.365103760721646076, 9.615707025640515937, 1.599625672291281386 ) ) ;
#99589 = CARTESIAN_POINT ( 'NONE',  ( 2.977667800601135895, 2.000151994021987623, -0.6593727523046940542 ) ) ;
#99590 = CARTESIAN_POINT ( 'NONE',  ( 0.5092220205753159590, -1.818610674291549323, 0.6019667691262234888 ) ) ;
#99591 = CARTESIAN_POINT ( 'NONE',  ( 2.659370686574860976, 6.254349567645977714, -0.7998128361456291469 ) ) ;
#99592 = CARTESIAN_POINT ( 'NONE',  ( 2.506254056688070886, 1.969067392671639771, 0.05118484259234063610 ) ) ;
#99593 = CARTESIAN_POINT ( 'NONE',  ( 0.3560485870845608858, 0.7116971694140910021, 1.730184004908103867 ) ) ;
#99594 = CARTESIAN_POINT ( 'NONE',  ( 1.504273306027693602, 1.959471947749168663, 0.09963418240711149898 ) ) ;
#99596 = ORIENTED_EDGE ( 'NONE', *, *, #136321, .T. ) ;
#99595 = CARTESIAN_POINT ( 'NONE',  ( 0.03522015555855115276, -0.09184495783944729430, 1.910282976853895587 ) ) ;
#99597 = CARTESIAN_POINT ( 'NONE',  ( 4.500943810056890371, 8.194925511800951412, -0.7216878364870207285 ) ) ;
#99598 = CARTESIAN_POINT ( 'NONE',  ( -1.402160292154681736E-14, 1.259375000341419248, -1.575800808251659024 ) ) ;
#99599 = CARTESIAN_POINT ( 'NONE',  ( 5.963714631206167738, 1.842656449598079060, -0.3214700631931910468 ) ) ;
#99600 = CARTESIAN_POINT ( 'NONE',  ( -5.606595252507366567, 5.572856915785063592, -0.3451608010808376870 ) ) ;
#99601 = CARTESIAN_POINT ( 'NONE',  ( 6.297728486381423352, -1.495382609916453998, -1.431936454106122358 ) ) ;
#99602 = FILL_AREA_STYLE ('',( #68136 ) ) ;
#99603 = ADVANCED_FACE ( 'NONE', ( #104984 ), #82720, .T. ) ;
#99604 = CARTESIAN_POINT ( 'NONE',  ( 1.275928261265106833, -2.020323679977220621, 0.4517519998969782291 ) ) ;
#99605 = CARTESIAN_POINT ( 'NONE',  ( 1.499999999999987121, 0.2541666666666844154, 0.8660254037844524744 ) ) ;
#99606 = CARTESIAN_POINT ( 'NONE',  ( 6.368579470117202490, 8.453095353268645695, 1.599625672291281386 ) ) ;
#99607 = CARTESIAN_POINT ( 'NONE',  ( -8.202846631467911820, 9.528741477256060577, 1.199719254218462483 ) ) ;
#99608 = CARTESIAN_POINT ( 'NONE',  ( 5.337069745634900997, 6.255611453776062980, 1.199719254218452047 ) ) ;
#99609 = CARTESIAN_POINT ( 'NONE',  ( 5.654972079148370412, 0.4136758123431219514, 2.079573305287989449 ) ) ;
#99610 = CARTESIAN_POINT ( 'NONE',  ( 5.086243903782109221, 5.962981304947771122, -1.199719254218452047 ) ) ;
#99611 = CARTESIAN_POINT ( 'NONE',  ( -1.364683531250014514, 0.9885416670080898749, -0.7879004041258289570 ) ) ;
#99612 = VERTEX_POINT ( 'NONE', #176367 ) ;
#99613 = CARTESIAN_POINT ( 'NONE',  ( -1.499999999999997780, 3.150000000000020783, 1.214306433183764966E-14 ) ) ;
#99615 = CARTESIAN_POINT ( 'NONE',  ( 2.822068529938852155, 6.444163718237301275, -0.7998128361456291469 ) ) ;
#99614 = CARTESIAN_POINT ( 'NONE',  ( 6.057081135787192316, 1.604708697955498087, -1.128374156723031430 ) ) ;
#99616 = CARTESIAN_POINT ( 'NONE',  ( 3.374374892241317703, -0.3960410224921434019, 1.976653181598592601 ) ) ;
#99617 = CARTESIAN_POINT ( 'NONE',  ( 4.083139574666094340, 1.542046283821847830, 1.136513224425585555 ) ) ;
#99618 = SPHERICAL_SURFACE ( 'NONE', #169420, 0.08000000000000000167 ) ;
#99619 = CARTESIAN_POINT ( 'NONE',  ( 1.101424459656743071, -0.5276332240332289869, 2.126988402630064279 ) ) ;
#99620 = CARTESIAN_POINT ( 'NONE',  ( 0.1331715793776652446, 7.629137130509056952, -2.553547540661147419 ) ) ;
#99621 = CARTESIAN_POINT ( 'NONE',  ( 3.532352470753961082, 1.824241569866682289, 0.4128566369710484629 ) ) ;
#99622 = CARTESIAN_POINT ( 'NONE',  ( -1.500000000000015099, -0.08958333265051321437, -0.8660254037844383745 ) ) ;
#99623 = CARTESIAN_POINT ( 'NONE',  ( -7.640183256500752584, 8.872300873127729304, -1.199719254218446718 ) ) ;
#99625 = CARTESIAN_POINT ( 'NONE',  ( 5.044581972647897317, -1.532752649812264778, 1.460808053437604226 ) ) ;
#99624 = CARTESIAN_POINT ( 'NONE',  ( -3.633221978782283923, 7.182583375313884133, -0.7216878364870267237 ) ) ;
#99626 = CARTESIAN_POINT ( 'NONE',  ( -1.402722028335470661, 13.31903653030363266, -0.2864402455888475085 ) ) ;
#99627 = DIRECTION ( 'NONE',  ( -0.000000000000000000, 1.000000000000000000, -0.000000000000000000 ) ) ;
#99629 = CARTESIAN_POINT ( 'NONE',  ( -4.894942725380222015, 7.314395937714276208, -1.216140164365722143 ) ) ;
#99628 = CARTESIAN_POINT ( 'NONE',  ( 1.980132433977495499, -2.051005990652774447, -0.4047881525126810209 ) ) ;
#99631 = EDGE_LOOP ( 'NONE', ( #129070, #99166, #201768, #160564, #152406, #131296, #127039 ) ) ;
#99630 = CARTESIAN_POINT ( 'NONE',  ( 0.6567381767516925484, -1.453278249834984326, -0.9285724537800400524 ) ) ;
#99632 = CARTESIAN_POINT ( 'NONE',  ( 7.396136491454752715, 8.587579647240744407, 1.199719254218462483 ) ) ;
#99633 = CARTESIAN_POINT ( 'NONE',  ( 7.499003223742838564, 15.48049048347138879, 9.369984475626267795 ) ) ;
#99634 = DIRECTION ( 'NONE',  ( 0.000000000000000000, 0.000000000000000000, 1.000000000000000000 ) ) ;
#99635 = CARTESIAN_POINT ( 'NONE',  ( 7.415946836550727284, 7.754285518838408109, 0.7216878364870317197 ) ) ;
#99636 = LINE ( 'NONE', #82307, #51164 ) ;
#99638 = CARTESIAN_POINT ( 'NONE',  ( 0.5569035977302905227, -1.554463864252687122, 0.9298500530290281230 ) ) ;
#99637 = CARTESIAN_POINT ( 'NONE',  ( 6.690022453700429139, 6.769724048930809701, 0.7998128361456331437 ) ) ;
#99639 = CARTESIAN_POINT ( 'NONE',  ( -7.542413527904030524, 7.693903958843159252, 1.040834085586084257E-14 ) ) ;
#99640 = CIRCLE ( 'NONE', #103049, 0.8299999999999999600 ) ;
#99641 = CARTESIAN_POINT ( 'NONE',  ( 3.357615597678655917, 7.068968630600412695, 0.7998128361456321445 ) ) ;
#99642 = CARTESIAN_POINT ( 'NONE',  ( -6.316227922719336974, 6.878322274790401814, 0.7073135764556655047 ) ) ;
#99643 = CARTESIAN_POINT ( 'NONE',  ( 4.552505719138623341, 8.533283448962240669, 0.7998128361456341429 ) ) ;
#99644 = CARTESIAN_POINT ( 'NONE',  ( 6.539320575229251808, 0.01001626003939220556, 1.796977979958065852 ) ) ;
#99645 = FACE_OUTER_BOUND ( 'NONE', #6910, .T. ) ;
#99646 = CARTESIAN_POINT ( 'NONE',  ( 4.019038269249470829, 7.568960612331900428, -0.3200009682147019752 ) ) ;
#99647 = CARTESIAN_POINT ( 'NONE',  ( 7.768458830950378591, 12.00702636951006497, 1.040834085586084257E-14 ) ) ;
#99648 = ORIENTED_EDGE ( 'NONE', *, *, #100082, .F. ) ;
#99649 = CARTESIAN_POINT ( 'NONE',  ( 2.717075380476912994, -1.617705633067820559, -0.9199624106535415624 ) ) ;
#99650 = CARTESIAN_POINT ( 'NONE',  ( 0.5092220205753159590, -1.818610674291549323, 0.6019667691262234888 ) ) ;
#99651 = CARTESIAN_POINT ( 'NONE',  ( 0.1295496576057716120, -1.118478952742516519, -1.443350188048427851 ) ) ;
#99652 = FILL_AREA_STYLE_COLOUR ( '', #43470 ) ;
#99653 = CIRCLE ( 'NONE', #155017, 3.970406073902761790 ) ;
#99654 = CARTESIAN_POINT ( 'NONE',  ( -1.528885273045263116, 8.694317336386671258, -2.518424357262861069 ) ) ;
#99655 = CARTESIAN_POINT ( 'NONE',  ( -4.948362879307902418, 4.875437568721725512, 1.214306433183764966E-14 ) ) ;
#99656 = CARTESIAN_POINT ( 'NONE',  ( 7.293923454472069245, 11.45340176361870199, 0.7216878364870438212 ) ) ;
#99657 = CARTESIAN_POINT ( 'NONE',  ( 4.926587155384105188, -1.289601243782242834, 1.488548236191704177 ) ) ;
#99658 = CARTESIAN_POINT ( 'NONE',  ( 1.207859650372544280, 1.608047128250057689, 1.382383069919224106 ) ) ;
#99659 = CARTESIAN_POINT ( 'NONE',  ( -6.715366157470410435, 6.729015360003925750, -0.7998128361456291469 ) ) ;
#99660 = DIRECTION ( 'NONE',  ( 0.000000000000000000, 1.000000000000000000, -8.546850786086437571E-32 ) ) ;
#99661 = CARTESIAN_POINT ( 'NONE',  ( 1.737499999999999378, -2.566666666666668650, -3.009438278150925683 ) ) ;
#99662 = CARTESIAN_POINT ( 'NONE',  ( 6.140607899229072686, -1.853288307406484758, 1.169240172944140621 ) ) ;
#99663 = SURFACE_STYLE_FILL_AREA ( #32532 ) ;
#99664 = CARTESIAN_POINT ( 'NONE',  ( 4.049766240643924320, 0.6497466500948418933, -1.813626049157530229 ) ) ;
#99665 = CARTESIAN_POINT ( 'NONE',  ( -5.533699252672048985, 9.607732894759390518, -0.7998128361456231517 ) ) ;
#99666 = CARTESIAN_POINT ( 'NONE',  ( 0.3756504392133250825, 1.046533627790873000, 1.495644344755317823 ) ) ;
#99667 = CARTESIAN_POINT ( 'NONE',  ( 1.032169062358662348, -1.402649970393770484, -1.703791656331831605 ) ) ;
#99668 = CARTESIAN_POINT ( 'NONE',  ( -0.3171178118501576382, 7.220087385434831972, 2.081545611384598704 ) ) ;
#99669 = ORIENTED_EDGE ( 'NONE', *, *, #121307, .T. ) ;
#99670 = CARTESIAN_POINT ( 'NONE',  ( 0.7500000000000006661, 10.69791666734946212, -1.299038105676657340 ) ) ;
#99671 = ORIENTED_EDGE ( 'NONE', *, *, #38147, .F. ) ;
#99672 = CARTESIAN_POINT ( 'NONE',  ( 6.789911431267126041, -1.283970416288570116, -1.493486111907322389 ) ) ;
#99673 = CARTESIAN_POINT ( 'NONE',  ( 1.716251783418326848, 1.812799857666002934, 0.6971432602522424915 ) ) ;
#99674 = CARTESIAN_POINT ( 'NONE',  ( 6.169324051992485458, -0.8183585724929974825, -2.147936757437307165 ) ) ;
#99676 = CARTESIAN_POINT ( 'NONE',  ( 4.627703445648046809, 1.805782058207167529, -0.4492820238155226797 ) ) ;
#99675 = CARTESIAN_POINT ( 'NONE',  ( -5.661411662158206681, 8.762674818229999829, -1.199719254218452047 ) ) ;
#99677 = CARTESIAN_POINT ( 'NONE',  ( 6.984385409695311964, 8.177479728513226576, 1.199719254218452935 ) ) ;
#99678 = CARTESIAN_POINT ( 'NONE',  ( 2.449293598294706414E-16, 0.000000000000000000, -2.000000000000000000 ) ) ;
#99679 = FILL_AREA_STYLE_COLOUR ( '', #212504 ) ;
#99681 = B_SPLINE_CURVE_WITH_KNOTS ( 'NONE', 3,
 ( #112259, #44008, #178273, #63442, #29883, #145798, #129592, #195580, #47216, #80762, #146851, #168398, #52511, #198738, #182497, #100196, #115451, #134858, #33070, #99148 ),
 .UNSPECIFIED., .F., .F.,
 ( 4, 2, 2, 1, 2, 2, 1, 2, 2, 2, 4 ),
 ( 0.6057107753108389447, 0.6187864442436151746, 0.6253242787100032896, 0.6261415080183017068, 0.6265501226724510264, 0.6269587373266002350, 0.6285931959431972915, 0.6318621131763914045, 0.6580134510419443084, 0.6841647889074973232, 0.7103161267730502271 ),
 .UNSPECIFIED. ) ;
#99680 = CARTESIAN_POINT ( 'NONE',  ( -6.579784621333750749, 6.570836901177822931, 0.7998128361456341429 ) ) ;
#99682 = CARTESIAN_POINT ( 'NONE',  ( -4.095971805104331231, 5.871996087412059140, 1.443375672974065660 ) ) ;
#99683 = CARTESIAN_POINT ( 'NONE',  ( -0.04112450405316381286, -1.960553898366865555, -0.9795403211517728082 ) ) ;
#99684 = CARTESIAN_POINT ( 'NONE',  ( 5.504247177468190699, 5.523969249908757817, 0.7216878364870317197 ) ) ;
#99685 = CARTESIAN_POINT ( 'NONE',  ( 4.344593448898664693E-13, 13.36537488277823371, -1.375075632470054154 ) ) ;
#99686 = DIRECTION ( 'NONE',  ( 0.7592566023653005702, 0.6507913734559639396, 0.000000000000000000 ) ) ;
#99687 = CARTESIAN_POINT ( 'NONE',  ( 1.119449510670032177, -1.781678707675336870, 0.3977030049751931196 ) ) ;
#99688 = CARTESIAN_POINT ( 'NONE',  ( -3.411848212133334446, 7.132240014130862171, 0.7998128361456341429 ) ) ;
#99689 = VECTOR ( 'NONE', #201119, 1000.000000000000000 ) ;
#99690 = CARTESIAN_POINT ( 'NONE',  ( 3.428057853464313798, -1.315526611184931527, -1.130013928329278494 ) ) ;
#99691 = CARTESIAN_POINT ( 'NONE',  ( -6.297925439369929101, 6.970297724909739756, -0.9421744322617598977 ) ) ;
#99692 = CARTESIAN_POINT ( 'NONE',  ( 6.609000000000047947, 7.053019707385148607, 2.498153760597703332 ) ) ;
#99693 = CARTESIAN_POINT ( 'NONE',  ( 0.1331565106231328843, 0.003911343561965873426, -1.946049565259087455 ) ) ;
#99694 = CARTESIAN_POINT ( 'NONE',  ( 6.358013415952256331, 1.820405254634300363, -0.1396899356524081148 ) ) ;
#99695 = CARTESIAN_POINT ( 'NONE',  ( 4.276187414114787089, -1.004825795036960567, -1.684713053385626269 ) ) ;
#99696 = TOROIDAL_SURFACE ( 'NONE', #71984, 10.75000000000000000, 0.5000000000000007772 ) ;
#99697 = CARTESIAN_POINT ( 'NONE',  ( -9.338868881714763148, 9.789768538289042255, -0.7998128361456291469 ) ) ;
#99698 = CARTESIAN_POINT ( 'NONE',  ( 7.135668919494039031, 7.219368582364847242, 1.040834085586084257E-14 ) ) ;
#99699 = EDGE_CURVE ( 'NONE', #25653, #108029, #175315, .T. ) ;
#99700 = CARTESIAN_POINT ( 'NONE',  ( 4.582752651445391123, -1.384437811569695587, 1.606279107262520434 ) ) ;
#99701 = CARTESIAN_POINT ( 'NONE',  ( -7.323375529675950624, 11.69568855126397011, -0.7998128361456291469 ) ) ;
#99702 = CARTESIAN_POINT ( 'NONE',  ( 5.657830175604453338, 5.495223381160312393, 0.7998128361456341429 ) ) ;
#99703 = CARTESIAN_POINT ( 'NONE',  ( 3.450112209602332669, -0.8433740631265237431, 1.890881698631073249 ) ) ;
#99704 = CARTESIAN_POINT ( 'NONE',  ( 0.6823417656249882723, 0.1552083336747514530, 1.181850606188755259 ) ) ;
#99705 = ORIENTED_EDGE ( 'NONE', *, *, #200040, .F. ) ;
#99706 = CARTESIAN_POINT ( 'NONE',  ( 3.411010488035473909, -1.370397956465055245, -1.845398096504316410 ) ) ;
#99707 = CARTESIAN_POINT ( 'NONE',  ( 8.975134502566660899, 10.53370701015836275, -1.082531754730543083 ) ) ;
#99709 = CARTESIAN_POINT ( 'NONE',  ( -3.285556943749998737, -3.230208332855375897, 1.896917185911908499 ) ) ;
#99708 = CARTESIAN_POINT ( 'NONE',  ( 5.397554552016204710, 9.311247720745345902, 0.7216878364870317197 ) ) ;
#99710 = CARTESIAN_POINT ( 'NONE',  ( -15.75000000000000000, 12.30000000000000071, -1.800000000000001155 ) ) ;
#99711 = ORIENTED_EDGE ( 'NONE', *, *, #117706, .T. ) ;
#99713 = EDGE_CURVE ( 'NONE', #190223, #119587, #127103, .T. ) ;
#99712 = CARTESIAN_POINT ( 'NONE',  ( -5.607868592924734941, 6.187540734389447294, -0.8708238738269019619 ) ) ;
#99714 = CARTESIAN_POINT ( 'NONE',  ( 4.306835718904429733, -0.4242474483713705169, -1.864571660543254961 ) ) ;
#99715 = CARTESIAN_POINT ( 'NONE',  ( -1.214306433183764966E-14, 3.299999999999969624, -3.122502256758252770E-14 ) ) ;
#99716 = CARTESIAN_POINT ( 'NONE',  ( 5.473588350598873831, 1.661195908839340873, -0.4637430927098630806 ) ) ;
#99717 = CARTESIAN_POINT ( 'NONE',  ( 3.520720487665735643, 0.3006478860226591276, 1.993893439002386581 ) ) ;
#99718 = CARTESIAN_POINT ( 'NONE',  ( 4.940191063930403637, -1.940984743010031544, -1.231243198015237628 ) ) ;
#99719 = CARTESIAN_POINT ( 'NONE',  ( 4.067155351693835485E-15, 1.250000000682825130, -1.225000000000013411 ) ) ;
#99720 = CARTESIAN_POINT ( 'NONE',  ( 0.5400322017136415242, -1.563516176313231920, -1.557742479837947558 ) ) ;
#99721 = CARTESIAN_POINT ( 'NONE',  ( -5.641601317062259646, 5.754492089426966217, -0.7216878364870338292 ) ) ;
#99722 = CARTESIAN_POINT ( 'NONE',  ( 5.342920941031360726, -1.517576202870707380, 0.9101455627106845858 ) ) ;
#99724 = CARTESIAN_POINT ( 'NONE',  ( 1.974976472051133136, -0.1153332747052069479, -2.289479170392795915 ) ) ;
#99723 = CARTESIAN_POINT ( 'NONE',  ( 6.008198349511364000, 7.038594824965278995, 1.199719254218453823 ) ) ;
#99725 = CARTESIAN_POINT ( 'NONE',  ( 0.09317796543232242934, -1.739829294281483474, -0.04824335600969902743 ) ) ;
#99726 = CARTESIAN_POINT ( 'NONE',  ( -3.810004860640155311, 4.403759411290286252, 1.199719254218462483 ) ) ;
#99727 = DIRECTION ( 'NONE',  ( 1.000000000000000000, 0.000000000000000000, 0.000000000000000000 ) ) ;
#99728 = CARTESIAN_POINT ( 'NONE',  ( -5.178288325776719603, 5.006034233019745372, 0.000000000000000000 ) ) ;
#99729 = DIRECTION ( 'NONE',  ( 0.000000000000000000, -1.000000000000000000, -1.804652791718263484E-16 ) ) ;
#99730 = DIRECTION ( 'NONE',  ( -1.000000000000000000, -1.224646799147353454E-16, 0.000000000000000000 ) ) ;
#99731 = CARTESIAN_POINT ( 'NONE',  ( 0.5730174903513629570, 1.496870926018354364, -1.572904236412080436 ) ) ;
#99732 = CARTESIAN_POINT ( 'NONE',  ( 2.553923023464285347, 1.082840749376843270, 1.700961377887353798 ) ) ;
#99733 = CARTESIAN_POINT ( 'NONE',  ( -0.7500000000000249800, -0.02708333265051543481, 1.299038105676659116 ) ) ;
#99734 = CARTESIAN_POINT ( 'NONE',  ( 5.988885569479125870, -0.2852814255829403955, -1.905149068243816579 ) ) ;
#99735 = CARTESIAN_POINT ( 'NONE',  ( -0.6823417656250039265, 12.31770833367473017, -1.181850606188755259 ) ) ;
#99736 = CARTESIAN_POINT ( 'NONE',  ( 2.672393786618231015, 2.210292516208379521, -0.2222851140616446397 ) ) ;
#99737 = VERTEX_POINT ( 'NONE', #26897 ) ;
#99738 = DIRECTION ( 'NONE',  ( -0.000000000000000000, 1.000000000000000000, -0.000000000000000000 ) ) ;
#99739 = DIRECTION ( 'NONE',  ( -1.000000000000000000, -3.451266460341926649E-31, -8.638326563840809144E-31 ) ) ;
#99741 = EDGE_CURVE ( 'NONE', #143955, #66223, #2257, .T. ) ;
#99740 = CARTESIAN_POINT ( 'NONE',  ( 7.703003830858588863, 12.13858823597705872, -0.7998128361456291469 ) ) ;
#99742 = DIRECTION ( 'NONE',  ( 0.000000000000000000, 0.000000000000000000, 1.000000000000000000 ) ) ;
#99743 =( NAMED_UNIT ( * ) PLANE_ANGLE_UNIT ( ) SI_UNIT ( $, .RADIAN. ) );
#99744 = STYLED_ITEM ( 'NONE', ( #82512 ), #33195 ) ;
#99745 = CARTESIAN_POINT ( 'NONE',  ( 4.528681460942417303, -1.588859801488880175, 0.7108448094420779517 ) ) ;
#99746 = CARTESIAN_POINT ( 'NONE',  ( 3.877359892829432386, -0.1466975079335990917, 1.956454564409334296 ) ) ;
#99748 = CARTESIAN_POINT ( 'NONE',  ( -6.507550544879489252, 9.575597488125954015, 1.082531754730548412 ) ) ;
#99747 = CARTESIAN_POINT ( 'NONE',  ( 3.174580523894166006, 6.855427711185178019, 0.7998128361456341429 ) ) ;
#99749 = CARTESIAN_POINT ( 'NONE',  ( -5.812277037385564782, 6.060071624232533871, -0.5253754717876522040 ) ) ;
#99750 = CARTESIAN_POINT ( 'NONE',  ( 10.40319425600960201, -5.787668213791926419, -0.4366904681731619831 ) ) ;
#99751 = CARTESIAN_POINT ( 'NONE',  ( 0.6431264911748921786, -0.2508561283167276557, -2.047287668789533832 ) ) ;
#99752 = CARTESIAN_POINT ( 'NONE',  ( -8.206763054973658100, 8.468978407091068306, 0.7998128361456602331 ) ) ;
#99753 = SHAPE_REPRESENTATION ( 'cover for positive', ( #200407 ), #155604 ) ;
#99754 = CARTESIAN_POINT ( 'NONE',  ( -2.914639836813632812, 6.344237543017112735, 0.7216878364870317197 ) ) ;
#99755 = CARTESIAN_POINT ( 'NONE',  ( 0.6555950923613624859, -1.913042455388717311, -1.207739878423098823 ) ) ;
#99756 = VERTEX_POINT ( 'NONE', #75664 ) ;
#99758 = EDGE_CURVE ( 'NONE', #100909, #18401, #46900, .T. ) ;
#99757 = CARTESIAN_POINT ( 'NONE',  ( 1.499999999999985123, -0.4229166659838508036, -0.8660254037844323793 ) ) ;
#99759 = CARTESIAN_POINT ( 'NONE',  ( 2.372138566722302500, -1.154253592077842727, 1.471842878544210809 ) ) ;
#99760 = CARTESIAN_POINT ( 'NONE',  ( 1.248208839261849112, 1.708581046602712039, -0.2955488178391346143 ) ) ;
#99761 = B_SPLINE_CURVE_WITH_KNOTS ( 'NONE', 3,
 ( #135093, #122114, #1838, #88472, #72181, #188079, #6111, #52747 ),
 .UNSPECIFIED., .F., .F.,
 ( 4, 2, 2, 4 ),
 ( 2.602085213965179827E-18, 0.0002461874215021541226, 0.0004923748430043056431, 0.0009847496860086130208 ),
 .UNSPECIFIED. ) ;
#99762 = CARTESIAN_POINT ( 'NONE',  ( 5.319949580897746166, 1.306013235697962571, -1.759773446019400778 ) ) ;
#99763 = CARTESIAN_POINT ( 'NONE',  ( 6.194374175331438082, -2.295634644278636394, -0.2347168956345067892 ) ) ;
#99764 = CARTESIAN_POINT ( 'NONE',  ( 1.059529560858112340, 0.4028119719261863962, -2.020956803572224736 ) ) ;
#99765 = CARTESIAN_POINT ( 'NONE',  ( 3.837779778221518168, 1.932683437559437500, 0.1894486881511766863 ) ) ;
#99766 = CARTESIAN_POINT ( 'NONE',  ( -5.111060722227552588, 6.025620933095978238, 1.082531754730546636 ) ) ;
#99767 = ADVANCED_FACE ( 'NONE', ( #160108 ), #156123, .T. ) ;
#99768 = CARTESIAN_POINT ( 'NONE',  ( 5.307814152003552444, -1.861618091082300808, 0.1822119596564600597 ) ) ;
#99769 = CARTESIAN_POINT ( 'NONE',  ( 1.812500000000001554, 1.451031289061194052, 1.451031289061046170 ) ) ;
#99770 = CARTESIAN_POINT ( 'NONE',  ( 1.367928747935657885, 13.31884955369513968, 0.3977952243826033407 ) ) ;
#99771 = CARTESIAN_POINT ( 'NONE',  ( 0.2448742905335095366, -1.679455039217644829, -0.4304099419733271592 ) ) ;
#99772 = CARTESIAN_POINT ( 'NONE',  ( 2.929970594329034395, 6.432399770110250437, -0.7216878364870338292 ) ) ;
#99773 = CARTESIAN_POINT ( 'NONE',  ( -1.360316468750056851, 1.369791667008064318, -0.7853790794159101196 ) ) ;
#99774 = CARTESIAN_POINT ( 'NONE',  ( 4.307267641921147749, 1.238321930042911578, -1.591317616567271775 ) ) ;
#99775 = CARTESIAN_POINT ( 'NONE',  ( -4.731432421044888592, 4.622352034081546712, -0.7216878364870207285 ) ) ;
#99776 = CARTESIAN_POINT ( 'NONE',  ( 7.587759525142423911, 12.00413654597487501, 0.7998128361456462443 ) ) ;
#99777 = CARTESIAN_POINT ( 'NONE',  ( 4.390861645979372341, 6.216034235099629157, -1.599625672291269396 ) ) ;
#99779 = DIRECTION ( 'NONE',  ( 0.000000000000000000, 0.000000000000000000, 1.000000000000000000 ) ) ;
#99778 = CARTESIAN_POINT ( 'NONE',  ( 2.455445036260803349, 0.4872311372507812655, -1.759406031448563557 ) ) ;
#99780 = DIRECTION ( 'NONE',  ( 1.000000000000000000, 0.000000000000000000, 0.000000000000000000 ) ) ;
#99781 = CARTESIAN_POINT ( 'NONE',  ( -10.37901820579008039, 4.889546506944066451, 5.358714317323078014 ) ) ;
#99782 = ORIENTED_EDGE ( 'NONE', *, *, #168889, .T. ) ;
#99783 = CARTESIAN_POINT ( 'NONE',  ( -5.519577934094894722, 7.532869904567736974, 1.443375672974058777 ) ) ;
#99784 = CARTESIAN_POINT ( 'NONE',  ( 4.632188385292959509, 8.431376123677011947, -0.5646427909330701267 ) ) ;
#99785 = CARTESIAN_POINT ( 'NONE',  ( -8.995998617867369873, 10.45408546138876993, 1.199719254218462483 ) ) ;
#99786 = CARTESIAN_POINT ( 'NONE',  ( 6.639320575229294086, 0.002105643433562148347, 2.003388605011639179 ) ) ;
#99787 = CARTESIAN_POINT ( 'NONE',  ( -0.004992717928550480244, -2.057963470346049650, -0.5107951590591561786 ) ) ;
#99788 = ORIENTED_EDGE ( 'NONE', *, *, #164365, .T. ) ;
#99789 = CARTESIAN_POINT ( 'NONE',  ( -5.589704470584107909, 9.743348658981940247, -0.7998128361456362523 ) ) ;
#99790 = CARTESIAN_POINT ( 'NONE',  ( 3.981290663907289140, 7.796589541200495965, -0.7998128361456221525 ) ) ;
#99791 = CARTESIAN_POINT ( 'NONE',  ( 6.719606831986117967, -1.999679869198322413, 0.4981698227890380970 ) ) ;
#99792 = CARTESIAN_POINT ( 'NONE',  ( 5.274064633610318076, 1.777012466945230962, -0.9530095070046653571 ) ) ;
#99793 = ORIENTED_EDGE ( 'NONE', *, *, #65255, .F. ) ;
#99794 = ORIENTED_EDGE ( 'NONE', *, *, #185760, .F. ) ;
#99795 = CARTESIAN_POINT ( 'NONE',  ( 4.726684935852882852, 4.891486930089099516, -0.8194250277325197951 ) ) ;
#99796 = DIRECTION ( 'NONE',  ( -0.6029061840396265914, 0.7978120914393163066, 0.000000000000000000 ) ) ;
#99797 = AXIS2_PLACEMENT_3D ( 'NONE', #21590, #5337, #198234 ) ;
#99800 = ORIENTED_EDGE ( 'NONE', *, *, #157010, .F. ) ;
#99799 = DIRECTION ( 'NONE',  ( 1.000000000000000000, 0.000000000000000000, 0.000000000000000000 ) ) ;
#99798 = CARTESIAN_POINT ( 'NONE',  ( -4.959250327548641479, 9.007818825440551791, -0.7998128361456362523 ) ) ;
#99801 = CARTESIAN_POINT ( 'NONE',  ( 4.613585901703492809, 8.466914752176691650, -0.2784627230535564046 ) ) ;
#99802 = CARTESIAN_POINT ( 'NONE',  ( 5.237657596305253627, -1.897407540178517316, -0.6818907625677357309 ) ) ;
#99803 = CARTESIAN_POINT ( 'NONE',  ( 4.206863059814883066, -0.3125640686512491384, 1.814249101404527220 ) ) ;
#99804 = CARTESIAN_POINT ( 'NONE',  ( 0.07661050522430808141, 2.897279719329011627, -2.199986835335824953 ) ) ;
#99805 = CARTESIAN_POINT ( 'NONE',  ( 3.721538942197761379, -0.1710094959430948913, 2.301408321908961607 ) ) ;
#99806 = CARTESIAN_POINT ( 'NONE',  ( 7.991605200612358573, 8.288237253661408843, 0.7998128361456281477 ) ) ;
#99807 = CARTESIAN_POINT ( 'NONE',  ( 4.306063477043454490, -2.156128079323017754, 0.1542669963271598166 ) ) ;
#99808 = CARTESIAN_POINT ( 'NONE',  ( 6.795661308947685164, 8.951357498570873261, -1.599625672291262513 ) ) ;
#99809 = CARTESIAN_POINT ( 'NONE',  ( 0.6263844939735198070, 0.1443197301355322315, 1.936771776935701794 ) ) ;
#99810 = CARTESIAN_POINT ( 'NONE',  ( -4.946027110887008860, 4.664786472323266153, -0.7998128361456221525 ) ) ;
#99811 = VERTEX_POINT ( 'NONE', #212028 ) ;
#99812 = CARTESIAN_POINT ( 'NONE',  ( 2.660307654469997285, 0.4179397774614675987, -0.1320628536826753963 ) ) ;
#99813 = CARTESIAN_POINT ( 'NONE',  ( -4.142898457427624415, 6.991076079377632091, 1.199719254218452935 ) ) ;
#99814 = CARTESIAN_POINT ( 'NONE',  ( 3.625732356982212412, -1.113523340526129335, -1.502988901547596567 ) ) ;
#99815 = AXIS2_PLACEMENT_3D ( 'NONE', #45004, #156615, #172869 ) ;
#99818 = CARTESIAN_POINT ( 'NONE',  ( -6.622231685632140596, 6.690634819517756959, 0.000000000000000000 ) ) ;
#99817 = CARTESIAN_POINT ( 'NONE',  ( 1.499999999999985123, -0.4229166659838508036, -0.8660254037844323793 ) ) ;
#99816 = CARTESIAN_POINT ( 'NONE',  ( 1.740342883905017013, 1.098329146349947827, -1.565357986077076990 ) ) ;
#99819 = CARTESIAN_POINT ( 'NONE',  ( 2.649284799151204073, -1.834272514977531632, 1.226802785254533568 ) ) ;
#99820 = DIRECTION ( 'NONE',  ( 0.000000000000000000, 0.000000000000000000, 1.000000000000000000 ) ) ;
#99821 = CARTESIAN_POINT ( 'NONE',  ( 4.867540842506059562, 5.637551390133895168, -1.199719254218452047 ) ) ;
#99822 = CARTESIAN_POINT ( 'NONE',  ( 5.844973620822823790, 9.833236634353070826, 0.7216878364870317197 ) ) ;
#99823 = CARTESIAN_POINT ( 'NONE',  ( -4.135400547368138113, 4.783387712472935149, 1.199719254218462483 ) ) ;
#99824 = CARTESIAN_POINT ( 'NONE',  ( -6.902509602688818191, 9.146290184594002781, -1.443375672974066548 ) ) ;
#99825 = CARTESIAN_POINT ( 'NONE',  ( 0.5441301207207068780, 1.965759916638841309, 0.1495998195316684265 ) ) ;
#99826 = CARTESIAN_POINT ( 'NONE',  ( 6.656845493208900955, -1.788705722188275837, 1.457663220358196732 ) ) ;
#99827 = CARTESIAN_POINT ( 'NONE',  ( 1.486689167417578394, 1.889818972856545987, 0.5264814339432166701 ) ) ;
#99828 = CARTESIAN_POINT ( 'NONE',  ( 4.258677893805890236, -0.6421077783588696741, -1.960174235369451123 ) ) ;
#99829 = CARTESIAN_POINT ( 'NONE',  ( 4.690757960648221037, 7.456006139856155457, 1.082531754730558626 ) ) ;
#99830 = CARTESIAN_POINT ( 'NONE',  ( 6.180537922983273091, 8.303989891604203422, -1.599625672291281386 ) ) ;
#99831 = EDGE_LOOP ( 'NONE', ( #167995, #188302, #211140, #167867 ) ) ;
#99832 = CARTESIAN_POINT ( 'NONE',  ( 6.439759776366758892, 10.45687747249582955, 0.7216878364870438212 ) ) ;
#99833 = CARTESIAN_POINT ( 'NONE',  ( -1.364683531250010295, 4.592708333674755394, 0.7879004041258379498 ) ) ;
#99834 = CARTESIAN_POINT ( 'NONE',  ( -10.17648486856286816, 3.632311211988387800, -6.360307065827860207 ) ) ;
#99835 = CARTESIAN_POINT ( 'NONE',  ( 2.833290915131624566, 6.249330467721451399, -0.7216878364870267237 ) ) ;
#99836 = CARTESIAN_POINT ( 'NONE',  ( 0.4621001773846104554, -0.5802113591629636247, 2.092003544004197302 ) ) ;
#99838 = CARTESIAN_POINT ( 'NONE',  ( 5.917501325027624048, -1.028386522942719816, -1.527094029191010893 ) ) ;
#99837 = CARTESIAN_POINT ( 'NONE',  ( 10.55905904256946215, -5.631911363926713321, -0.4368516432692077789 ) ) ;
#99839 = ADVANCED_FACE ( 'NONE', ( #191523 ), #159045, .F. ) ;
#99840 = DIRECTION ( 'NONE',  ( -0.000000000000000000, -0.000000000000000000, -1.000000000000000000 ) ) ;
#99841 = CARTESIAN_POINT ( 'NONE',  ( -11.84104725192624130, 12.49016462548582851, -1.443823348526935169 ) ) ;
#99842 = CARTESIAN_POINT ( 'NONE',  ( 1.194370141144196706, -0.4488658031855938813, -1.815784161679114606 ) ) ;
#99843 = CARTESIAN_POINT ( 'NONE',  ( 5.237646302014136168, -1.524508687941978469, -1.532700278705993790 ) ) ;
#99844 = CARTESIAN_POINT ( 'NONE',  ( -5.780146447551155475, 6.079674369897793085, -0.5991446231495625163 ) ) ;
#99845 = DIRECTION ( 'NONE',  ( 0.000000000000000000, 1.000000000000000000, 0.000000000000000000 ) ) ;
#99846 = CARTESIAN_POINT ( 'NONE',  ( 6.252685474373055996, 7.003816019006632310, -0.9791501464874209359 ) ) ;
#99847 = CARTESIAN_POINT ( 'NONE',  ( 1.364683531249988535, 5.717708333674752730, -0.7879004041258300672 ) ) ;
#99848 = COLOUR_RGB ( '', 0.09019608, 0.27058824, 0.51372549) ;
#99849 = CARTESIAN_POINT ( 'NONE',  ( 0.9262460828363195953, -0.8603794558708978135, -1.707882697979688391 ) ) ;
#99850 =( BOUNDED_CURVE ( )  B_SPLINE_CURVE ( 2, ( #69517, #119426, #18646, #84724, #150813, #66311, #135625 ),
 .UNSPECIFIED., .F., .T. ) 
 B_SPLINE_CURVE_WITH_KNOTS ( ( 3, 2, 2, 3 ),
 ( 0.2999999999999999889, 0.3083333333333334036, 0.3166666666666667629, 0.3250000000000001776 ),
 .UNSPECIFIED. ) 
 CURVE ( )  GEOMETRIC_REPRESENTATION_ITEM ( )  RATIONAL_B_SPLINE_CURVE ( ( 1.000000000000000000, 0.8660254037844387076, 1.000000000000000000, 0.8660254037844387076, 1.000000000000000000, 0.8660254037844360431, 1.000000000000002665 ) ) 
 REPRESENTATION_ITEM ( '' )  );
#99851 = CARTESIAN_POINT ( 'NONE',  ( 3.098275772329066591, -0.5124342443764763333, -1.694037474313156988 ) ) ;
#99852 = CARTESIAN_POINT ( 'NONE',  ( 0.6098336241119780565, -0.6879379538977903330, 1.784437680087819666 ) ) ;
#99854 = CARTESIAN_POINT ( 'NONE',  ( 5.747645016999404888, 1.886384853835708642, -0.3323884645628824019 ) ) ;
#99853 = CARTESIAN_POINT ( 'NONE',  ( 7.458876248284573407, -7.605490376493627025, -6.801849632070416263 ) ) ;
#99855 = CARTESIAN_POINT ( 'NONE',  ( 0.1861046438572169504, -1.272802160389638892, -1.633586439835111648 ) ) ;
#99856 = CARTESIAN_POINT ( 'NONE',  ( 0.6508261300204335464, 2.090236094481153550, 0.3566229023672163878 ) ) ;
#99857 = DIRECTION ( 'NONE',  ( -0.000000000000000000, -1.000000000000000000, -0.000000000000000000 ) ) ;
#99858 = CARTESIAN_POINT ( 'NONE',  ( 3.801501934187266230, -0.5436965770258190833, 1.789884385262895616 ) ) ;
#99860 = ORIENTED_EDGE ( 'NONE', *, *, #207810, .F. ) ;
#99859 = CARTESIAN_POINT ( 'NONE',  ( 0.6799654140086827114, -1.016662149479659494, 1.516215539243186639 ) ) ;
#99862 = CARTESIAN_POINT ( 'NONE',  ( -5.939880696118548187, 6.102484698325975288, 0.000000000000000000 ) ) ;
#99861 = CARTESIAN_POINT ( 'NONE',  ( 2.983271218942393332, -0.1628219013674602478, -2.200934326520533446 ) ) ;
#99863 = CARTESIAN_POINT ( 'NONE',  ( -1.364683531249997417, 4.321875000341417028, 1.214306433183764966E-14 ) ) ;
#99864 = CARTESIAN_POINT ( 'NONE',  ( 1.451709319293143396, 1.560653109857246701, 1.348772525646862341 ) ) ;
#99865 = CARTESIAN_POINT ( 'NONE',  ( 6.043183783389218355, 8.073467052085995022, 1.599625672291267398 ) ) ;
#99866 = CARTESIAN_POINT ( 'NONE',  ( -9.016335848287868160, 10.47781223021269170, 1.199719254218462483 ) ) ;
#99867 = DIRECTION ( 'NONE',  ( 4.440892098500621231E-16, -6.661338147750950089E-16, 1.000000000000000000 ) ) ;
#99868 = DIRECTION ( 'NONE',  ( -0.000000000000000000, -1.000000000000000000, -0.000000000000000000 ) ) ;
#99869 = CARTESIAN_POINT ( 'NONE',  ( 5.820193082016415609, 10.01225203898631655, 0.000000000000000000 ) ) ;
#99870 = ORIENTED_EDGE ( 'NONE', *, *, #138683, .T. ) ;
#99871 = CARTESIAN_POINT ( 'NONE',  ( 4.809070886388271404, -1.664838503569150419, 1.230558894880565246 ) ) ;
#99872 = CARTESIAN_POINT ( 'NONE',  ( -1.402160292154681736E-14, -0.6156249996585817508, 1.575800808251672791 ) ) ;
#99873 = CARTESIAN_POINT ( 'NONE',  ( 1.265152180075890254, -1.953616520262021039, -0.9254636565915741464 ) ) ;
#99874 = CARTESIAN_POINT ( 'NONE',  ( -5.018153416333300143, 7.915986710968343054, -1.079799343345327234 ) ) ;
#99875 = CARTESIAN_POINT ( 'NONE',  ( 1.981123565540498177, -1.847491841353067210, -0.8164113852280636685 ) ) ;
#99876 = FACE_OUTER_BOUND ( 'NONE', #6629, .T. ) ;
#99877 = EDGE_LOOP ( 'NONE', ( #151631, #175064, #133247, #146838 ) ) ;
#99878 = EDGE_CURVE ( 'NONE', #75117, #138779, #9247, .T. ) ;
#99880 = CARTESIAN_POINT ( 'NONE',  ( 8.771762198361678031, 9.336070107617867819, 1.040834085586084257E-14 ) ) ;
#99879 = CARTESIAN_POINT ( 'NONE',  ( 0.000000000000000000, -3.237499999999997602, -4.012584370867899430 ) ) ;
#99881 = CARTESIAN_POINT ( 'NONE',  ( -7.142181811248260459E-15, -5.907420853759270507, 10.91970695577495221 ) ) ;
#99882 = CARTESIAN_POINT ( 'NONE',  ( 6.491422787562372676, -0.4091076066058823013, 1.878265147811091662 ) ) ;
#99883 = CARTESIAN_POINT ( 'NONE',  ( 6.539320575229255361, 7.051987793746187450, 2.801414728815339039 ) ) ;
#99884 = CARTESIAN_POINT ( 'NONE',  ( 4.739868811304373430, 2.185674081084403753, 0.1610935195608814985 ) ) ;
#99885 = CARTESIAN_POINT ( 'NONE',  ( -0.7500000000000215383, 3.722916667349487785, 1.299038105676671107 ) ) ;
#99886 = CARTESIAN_POINT ( 'NONE',  ( 4.095896644567202038, 1.253117935160457552, 1.444681106026260320 ) ) ;
#99887 = CARTESIAN_POINT ( 'NONE',  ( -6.254388934605767503, 6.191208599995166040, 0.7998128361456341429 ) ) ;
#99888 = CARTESIAN_POINT ( 'NONE',  ( 4.161989969270902812, 4.918371721313249623, 1.082531754730560403 ) ) ;
#99890 = CARTESIAN_POINT ( 'NONE',  ( 2.706657832681820697, 1.899625987897411772, 0.6766965020792228280 ) ) ;
#99889 = CARTESIAN_POINT ( 'NONE',  ( -9.124274191872631334, 12.62844174295135069, -1.082531754730543083 ) ) ;
#99891 = CARTESIAN_POINT ( 'NONE',  ( 0.6823417656249934904, 12.00520833367473017, 1.181850606188764807 ) ) ;
#99892 = CIRCLE ( 'NONE', #6466, 0.09999999999999992228 ) ;
#99894 = CARTESIAN_POINT ( 'NONE',  ( -5.991777542596674166, 5.955104985976372944, 0.000000000000000000 ) ) ;
#99893 = CARTESIAN_POINT ( 'NONE',  ( 0.4512259348973605699, -1.940755322566484642, -1.219765617878470376 ) ) ;
#99895 = CARTESIAN_POINT ( 'NONE',  ( 4.330854930063167352, 0.08572247821646634958, 1.722753318990229099 ) ) ;
#99896 = CARTESIAN_POINT ( 'NONE',  ( 8.188198428010544205, 8.517596018959260107, 0.000000000000000000 ) ) ;
#99897 = CARTESIAN_POINT ( 'NONE',  ( 4.142179624174931796, 4.791296635414242111, 1.199719254218464037 ) ) ;
#99898 = CARTESIAN_POINT ( 'NONE',  ( 0.000000000000000000, 0.000000000000000000, 0.000000000000000000 ) ) ;
#99899 = CARTESIAN_POINT ( 'NONE',  ( 0.6956633456795427994, -1.384754418207832405, -1.389998539416361423 ) ) ;
#99900 = DIRECTION ( 'NONE',  ( -1.124869321039521280E-29, -7.437565543542506798E-15, -1.000000000000000000 ) ) ;
#99901 = CARTESIAN_POINT ( 'NONE',  ( 4.330940004561544043, 7.140181541042074365, -1.199719254218452047 ) ) ;
#99902 = CARTESIAN_POINT ( 'NONE',  ( 0.07556134207194721564, 2.859159929750184848, -2.732257853551669946 ) ) ;
#99903 = EDGE_LOOP ( 'NONE', ( #197833, #60111, #208572, #135316 ) ) ;
#99904 = CARTESIAN_POINT ( 'NONE',  ( 0.2333690889706682703, 0.003390530909083006028, -2.053566628440507635 ) ) ;
#99905 = ORIENTED_EDGE ( 'NONE', *, *, #33468, .F. ) ;
#99906 = CARTESIAN_POINT ( 'NONE',  ( 4.723216582411014386, 1.578617123877921857, 0.8883131493910937371 ) ) ;
#99907 = ORIENTED_EDGE ( 'NONE', *, *, #38982, .F. ) ;
#99908 = CARTESIAN_POINT ( 'NONE',  ( 7.042534447655770080, 7.180988041878682004, -0.7998128361456341429 ) ) ;
#99909 = CARTESIAN_POINT ( 'NONE',  ( 5.373626179778474565, 0.3473841915581803996, -1.777664473148509838 ) ) ;
#99910 = CARTESIAN_POINT ( 'NONE',  ( 6.983858524370782028, 8.280828045588322084, 1.082531754730549967 ) ) ;
#99911 = TOROIDAL_SURFACE ( 'NONE', #134247, 1.749999999999999778, 0.5000000000000007772 ) ;
#99912 = CARTESIAN_POINT ( 'NONE',  ( 8.024744567526232331, -5.166862915010145052, -7.523999700038788596 ) ) ;
#99913 = CARTESIAN_POINT ( 'NONE',  ( 5.622931663646434153, 6.144404617744410046, -0.8283694935172694063 ) ) ;
#99914 = EDGE_CURVE ( 'NONE', #160319, #170502, #57649, .T. ) ;
#99916 = CARTESIAN_POINT ( 'NONE',  ( 0.6823417656249969321, 15.27604166700806410, -1.181850606188757036 ) ) ;
#99915 = CARTESIAN_POINT ( 'NONE',  ( 6.391040216397121831, 0.1834577666269270046, 1.851959058998996710 ) ) ;
#99917 = CARTESIAN_POINT ( 'NONE',  ( 3.374530662324583652, -0.3768237823980990497, -1.877989258545700535 ) ) ;
#99918 = CARTESIAN_POINT ( 'NONE',  ( -6.496114076516063207, -8.169775483750591150, -6.932145363377419045 ) ) ;
#99919 = DIRECTION ( 'NONE',  ( -0.9999980456341537316, 0.000000000000000000, -0.001977050295958610645 ) ) ;
#99920 = CARTESIAN_POINT ( 'NONE',  ( -1.364683531250014514, -0.9697916663252473812, 0.7879004041258379498 ) ) ;
#99921 = CARTESIAN_POINT ( 'NONE',  ( 7.158341918335438869, 7.453746447587225710, -0.7216878364870257245 ) ) ;
#99923 = CARTESIAN_POINT ( 'NONE',  ( 5.577400755804389654, 1.605162776699980753, 1.380938528300587276 ) ) ;
#99922 = CARTESIAN_POINT ( 'NONE',  ( -3.195971524519394702, 4.751719416737803847, -1.599625672291262513 ) ) ;
#99924 = CARTESIAN_POINT ( 'NONE',  ( 1.235488887756378551, -1.954010380348418119, 0.9248176494114216384 ) ) ;
#99925 = CARTESIAN_POINT ( 'NONE',  ( -5.960744811863571968, 6.983232364376142698, 1.199719254218452935 ) ) ;
#99926 = CARTESIAN_POINT ( 'NONE',  ( 3.528865121306874464, 7.339036084825155015, -0.7998128361456362523 ) ) ;
#99927 = CARTESIAN_POINT ( 'NONE',  ( 1.026062881544724137, 1.091098483296793820, -1.463488004260153907 ) ) ;
#99928 = CARTESIAN_POINT ( 'NONE',  ( -3.255929445576174697, 6.950334786480840243, -0.7998128361456281477 ) ) ;
#99929 = CARTESIAN_POINT ( 'NONE',  ( 3.399243825379614226, 1.438455020490635450, 1.123966471122700650 ) ) ;
#99930 = CARTESIAN_POINT ( 'NONE',  ( 10.17148340815012020, 11.75186938811109627, -7.510838954888964025 ) ) ;
#99931 = CARTESIAN_POINT ( 'NONE',  ( 2.654443970922310214, 1.898414275235399407, 0.2300336082040748686 ) ) ;
#99932 = ORIENTED_EDGE ( 'NONE', *, *, #45961, .T. ) ;
#99933 = CARTESIAN_POINT ( 'NONE',  ( 2.980859429886784984, 1.853565342000351501, 0.6662430357459552255 ) ) ;
#99934 = CARTESIAN_POINT ( 'NONE',  ( 4.353030786369998850, 0.4220677823760305980, -1.895499586301018224 ) ) ;
#99935 = CARTESIAN_POINT ( 'NONE',  ( -7.937372586157736443, 8.224965870130965584, 0.7998128361456341429 ) ) ;
#99937 = CARTESIAN_POINT ( 'NONE',  ( 5.045234882716379765, 0.1584239314957915090, 2.114765283346302205 ) ) ;
#99936 = CARTESIAN_POINT ( 'NONE',  ( 7.178115983792402233, 7.339166500704784823, 0.7998128361456281477 ) ) ;
#99938 = CARTESIAN_POINT ( 'NONE',  ( 0.000000000000000000, -9.999999999999994671, 0.000000000000000000 ) ) ;
#99939 = CARTESIAN_POINT ( 'NONE',  ( 6.050032868414796816, 6.056328681155354055, -0.4621489055621590403 ) ) ;
#99940 = CARTESIAN_POINT ( 'NONE',  ( 0.2331563151865729544, 6.948071805571808035, -2.540803835148666145 ) ) ;
#99941 = CARTESIAN_POINT ( 'NONE',  ( -8.150208238660177074, 14.48038068602284056, 8.818988908991837405 ) ) ;
#99942 = CARTESIAN_POINT ( 'NONE',  ( 5.551137550152489553, 5.441024994791534120, 0.7998128361456352531 ) ) ;
#99943 = CARTESIAN_POINT ( 'NONE',  ( 0.09770433987276584686, -9.919999999999998153, 9.499497670693809681 ) ) ;
#99944 = CARTESIAN_POINT ( 'NONE',  ( 4.547361323050268744, -1.413013347330991598, -1.156083184146582177 ) ) ;
#99945 = CARTESIAN_POINT ( 'NONE',  ( 10.99958311221863028, -9.919613946868095056, -0.09579086958120625050 ) ) ;
#99946 = CARTESIAN_POINT ( 'NONE',  ( -8.758204044748012507, 11.24099069033793974, 1.443375672974064550 ) ) ;
#99947 = AXIS2_PLACEMENT_3D ( 'NONE', #56814, #25374, #203035 ) ;
#99948 = CARTESIAN_POINT ( 'NONE',  ( -6.472689817967896886, 6.776322833669464529, -0.2902398332882798471 ) ) ;
#99949 = CARTESIAN_POINT ( 'NONE',  ( -0.4000000000000304423, 3.999999999999981348, -0.8338124244295984644 ) ) ;
#99950 = CARTESIAN_POINT ( 'NONE',  ( 6.157094445334826638, -1.605393284960114242, -0.9600186418455139981 ) ) ;
#99951 = CARTESIAN_POINT ( 'NONE',  ( 7.239163954692881653, 10.53310948286200599, -1.199719254218441611 ) ) ;
#99952 = CARTESIAN_POINT ( 'NONE',  ( -5.434120640978981065, 5.234228924097237723, -0.7998128361456221525 ) ) ;
#99953 = EDGE_CURVE ( 'NONE', #159976, #148658, #149139, .T. ) ;
#99954 = CARTESIAN_POINT ( 'NONE',  ( -1.364683531250010295, 10.44270833367473017, 0.7879004041258445001 ) ) ;
#99955 = CARTESIAN_POINT ( 'NONE',  ( -6.437424008390261854, 6.404749519410410485, 0.7998128361456341429 ) ) ;
#99956 = CARTESIAN_POINT ( 'NONE',  ( 2.184835310096557404, 5.700724961754617404, 1.040834085586084257E-14 ) ) ;
#99957 = CARTESIAN_POINT ( 'NONE',  ( -4.217995187182965289, 6.014356699837137832, 1.443375672974065660 ) ) ;
#99958 = CARTESIAN_POINT ( 'NONE',  ( -6.403528624356093601, 6.365204904703887223, 1.040834085586084257E-14 ) ) ;
#99959 = VECTOR ( 'NONE', #208388, 1000.000000000000000 ) ;
#99960 = CARTESIAN_POINT ( 'NONE',  ( 6.754729744842355110, -0.5704115468931982846, -2.094772688322795506 ) ) ;
#99961 = CARTESIAN_POINT ( 'NONE',  ( 1.282980312568120951, 1.728570797422763095, -1.222324810828350428 ) ) ;
#99962 = CARTESIAN_POINT ( 'NONE',  ( 9.240045382913317340, 10.73880668727576015, -1.199719254218446718 ) ) ;
#99963 = CARTESIAN_POINT ( 'NONE',  ( -1.201851678989727383E-14, 3.587500000000020339, -1.732050807568863648 ) ) ;
#99964 = CARTESIAN_POINT ( 'NONE',  ( 5.787960296632533641, -1.308950758395693414, -1.603975846202657429 ) ) ;
#99965 = CARTESIAN_POINT ( 'NONE',  ( 4.046752668985390322, 7.764364035880440440, -0.4786816536347000550 ) ) ;
#99966 = CARTESIAN_POINT ( 'NONE',  ( 4.853455804012203778, 8.606189504748821051, 0.7216878364870438212 ) ) ;
#99968 = CARTESIAN_POINT ( 'NONE',  ( 0.000000000000000000, 0.000000000000000000, 0.000000000000000000 ) ) ;
#99967 = CARTESIAN_POINT ( 'NONE',  ( -11.07790593930098311, 9.799999999999998934, 0.6999999999999992895 ) ) ;
#99969 = CARTESIAN_POINT ( 'NONE',  ( 1.904612379804408118, 1.696638126304336858, -1.541566781129146912 ) ) ;
#99971 = CARTESIAN_POINT ( 'NONE',  ( 0.08053691275167890185, 19.00000000000000000, 11.99972973886014316 ) ) ;
#99970 = CARTESIAN_POINT ( 'NONE',  ( -6.392116398764494001, 6.567141947923602174, 2.438447736781127695 ) ) ;
#99972 = CARTESIAN_POINT ( 'NONE',  ( 2.039183100597967258, 0.003605121848727563250, 1.912571728241836633 ) ) ;
#99973 = VERTEX_POINT ( 'NONE', #48502 ) ;
#99975 = ADVANCED_FACE ( 'NONE', ( #65763 ), #71534, .T. ) ;
#99974 = CARTESIAN_POINT ( 'NONE',  ( 6.927853306458743532, 9.105581495667113501, 1.443375672974076540 ) ) ;
#99976 = CARTESIAN_POINT ( 'NONE',  ( 0.08813964471556486047, 1.162479488604960753, 1.643474645366525877 ) ) ;
#99977 = CARTESIAN_POINT ( 'NONE',  ( 1.041763817972749750, 1.313373124611896703, 1.457441342770829262 ) ) ;
#99978 = CARTESIAN_POINT ( 'NONE',  ( -9.541187415715041809, 12.15447128979948310, -1.599625672291263179 ) ) ;
#99979 = CARTESIAN_POINT ( 'NONE',  ( -6.530223543276495235, 10.77034456713125188, -0.7998128361456291469 ) ) ;
#99981 = CARTESIAN_POINT ( 'NONE',  ( 2.834531330521594228, 0.2145198750864007742, 1.756709382032408451 ) ) ;
#99980 = CARTESIAN_POINT ( 'NONE',  ( 3.591813267288586520, -2.088258123952376977, -0.1022297611361303732 ) ) ;
#99983 = CARTESIAN_POINT ( 'NONE',  ( 5.349693066923443041, 2.289838395228523282, -0.1081633463214677210 ) ) ;
#99982 = CARTESIAN_POINT ( 'NONE',  ( 2.275435306267621804, 5.643409308550367598, 0.5316758947214432762 ) ) ;
#99984 = CARTESIAN_POINT ( 'NONE',  ( 3.134399458026761121, -1.534476879465409782, 0.8210378458504956622 ) ) ;
#99985 = CARTESIAN_POINT ( 'NONE',  ( 3.541704441667858472, 5.155074486744371853, -1.599625672291262513 ) ) ;
#99986 = AXIS2_PLACEMENT_3D ( 'NONE', #173652, #185583, #155240 ) ;
#99987 = CARTESIAN_POINT ( 'NONE',  ( 4.817943484809818600, 6.714296380401858499, 1.599625672291269396 ) ) ;
#99988 = CARTESIAN_POINT ( 'NONE',  ( 3.532318661231689916, 1.691930322982236667, -0.3780173437282279281 ) ) ;
#99989 = CARTESIAN_POINT ( 'NONE',  ( 3.262351433937484835, -2.168797558456833308, 0.1038475075719157148 ) ) ;
#99990 = CARTESIAN_POINT ( 'NONE',  ( 3.822509244049070887, 6.547012320444182798, -1.199719254218452047 ) ) ;
#99991 = CARTESIAN_POINT ( 'NONE',  ( 5.717982508692024624, 0.9896897593998502662, -1.756851901128737348 ) ) ;
#99992 = CARTESIAN_POINT ( 'NONE',  ( 0.3437500000590538174, 1.895863741711102612, 0.7852924748299703328 ) ) ;
#99993 = CARTESIAN_POINT ( 'NONE',  ( 1.499999999999989120, 4.827083334016149863, -0.8660254037844323793 ) ) ;
#99994 = CARTESIAN_POINT ( 'NONE',  ( 2.344641424807081709, 0.4199494819796690814, 1.879913682802894614 ) ) ;
#99995 = CARTESIAN_POINT ( 'NONE',  ( 1.499999999999993117, 8.885416667349462116, 0.8660254037844409281 ) ) ;
#99996 = CARTESIAN_POINT ( 'NONE',  ( 5.590131909697702461, 1.323030080273413844, 1.784280720909060758 ) ) ;
#99997 = ORIENTED_EDGE ( 'NONE', *, *, #86051, .T. ) ;
#99998 = CARTESIAN_POINT ( 'NONE',  ( 10.50000000000000178, 12.69999999999999929, -3.600000000000000977 ) ) ;
#99999 = CARTESIAN_POINT ( 'NONE',  ( -1.402160292154681736E-14, 2.087500000000021227, -1.732050807568863648 ) ) ;
#100000 = CARTESIAN_POINT ( 'NONE',  ( 7.124973419181436007, 8.271222729588529887, -1.199719254218446718 ) ) ;
#100001 = CARTESIAN_POINT ( 'NONE',  ( 4.731432421044862835, 6.543090462684225450, -1.443375672974051449 ) ) ;
#100002 = CARTESIAN_POINT ( 'NONE',  ( 1.642778471875000035, -0.9260416661887073131, -2.845375778867859751 ) ) ;
#100003 = CARTESIAN_POINT ( 'NONE',  ( 1.893536009595264469, -0.1129285828431712546, -2.218558826778730619 ) ) ;
#100004 = CARTESIAN_POINT ( 'NONE',  ( 6.584431417889404337, 1.130572321132311098, -1.603143135845342515 ) ) ;
#100005 = CARTESIAN_POINT ( 'NONE',  ( 8.351459436338029008, 10.76645531385962862, -1.443375672974063439 ) ) ;
#100006 = VECTOR ( 'NONE', #99868, 1000.000000000000000 ) ;
#100007 = CARTESIAN_POINT ( 'NONE',  ( 0.001169091720979649387, 3.496131414459332731, 2.003411285068362968 ) ) ;
#100008 = CARTESIAN_POINT ( 'NONE',  ( 4.960304097753311936, 6.880383762169266504, 1.599625672291268286 ) ) ;
#100009 = CARTESIAN_POINT ( 'NONE',  ( -4.177320726786328819, 5.966903162707725805, -1.443375672974066548 ) ) ;
#100010 = CARTESIAN_POINT ( 'NONE',  ( 4.422371107804410784, 0.9697015505613596487, 1.820508916172391300 ) ) ;
#100011 = CARTESIAN_POINT ( 'NONE',  ( -6.078132937628113908, 5.985576603521232109, 1.040834085586084257E-14 ) ) ;
#100013 = EDGE_CURVE ( 'NONE', #43199, #78277, #137428, .T. ) ;
#100012 = CARTESIAN_POINT ( 'NONE',  ( 0.7499999999999902300, 3.764583334016149863, 1.299038105676669330 ) ) ;
#100014 = CARTESIAN_POINT ( 'NONE',  ( 0.6823417656249882723, 0.1760416670080894308, -1.181850606188749264 ) ) ;
#100015 = CARTESIAN_POINT ( 'NONE',  ( 5.553920895479774522, 1.868435625992425742, -0.09091641586010666687 ) ) ;
#100016 = CARTESIAN_POINT ( 'NONE',  ( 5.221237796217499394, 1.709784868986977902, 0.2885349091684140665 ) ) ;
#100017 = CARTESIAN_POINT ( 'NONE',  ( 4.475936636375839051, -1.689578365139619009, -0.4171736215478424881 ) ) ;
#100018 = CARTESIAN_POINT ( 'NONE',  ( 3.174580523894166006, 6.855427711185178019, 0.7998128361456341429 ) ) ;
#100019 = CARTESIAN_POINT ( 'NONE',  ( 1.558568218312964326, -1.617219677351620089, 1.624929221499067600 ) ) ;
#100020 = CARTESIAN_POINT ( 'NONE',  ( -1.001543065824772872E-14, 5.384375000341415252, 1.575800808251672791 ) ) ;
#100021 = CARTESIAN_POINT ( 'NONE',  ( 5.390208805286830440, -0.5092157624977285968, -2.027641083400610000 ) ) ;
#100022 = CARTESIAN_POINT ( 'NONE',  ( 1.552429278155377679, -1.578373273985161473, -0.9476568548090894550 ) ) ;
#100023 = EDGE_CURVE ( 'NONE', #160372, #19980, #29980, .T. ) ;
#100024 = CARTESIAN_POINT ( 'NONE',  ( -0.07538891330675576152, -7.154544010627095219, 9.499700864329900796 ) ) ;
#100025 = CARTESIAN_POINT ( 'NONE',  ( 1.828750219146151323, 0.7691198443132395424, -1.864169014999479623 ) ) ;
#100026 = CARTESIAN_POINT ( 'NONE',  ( 0.000000000000000000, -2.079999999999998295, 0.000000000000000000 ) ) ;
#100027 = LINE ( 'NONE', #39292, #13848 ) ;
#100028 = CARTESIAN_POINT ( 'NONE',  ( -6.795661308947694934, 8.951357498570873261, -1.599625672291263179 ) ) ;
#100029 =( BOUNDED_CURVE ( )  B_SPLINE_CURVE ( 3, ( #151861, #37018, #87914, #203769 ),
 .UNSPECIFIED., .F., .T. ) 
 B_SPLINE_CURVE_WITH_KNOTS ( ( 4, 4 ),
 ( 3.141592653589619921, 4.712388980384721648 ),
 .UNSPECIFIED. ) 
 CURVE ( )  GEOMETRIC_REPRESENTATION_ITEM ( )  RATIONAL_B_SPLINE_CURVE ( ( 1.000000000000000000, 0.8047378541243166428, 0.8047378541243166428, 1.000000000000000000 ) ) 
 REPRESENTATION_ITEM ( '' )  );
#100030 = CARTESIAN_POINT ( 'NONE',  ( 3.818592820543298405, 7.606775390609172405, -0.7998128361456221525 ) ) ;
#100031 = CARTESIAN_POINT ( 'NONE',  ( -1.360316468750040642, 1.911458333674787236, 0.7853790794158660438 ) ) ;
#100032 = CARTESIAN_POINT ( 'NONE',  ( 4.020270485675044192, -2.114722421624544157, 0.1573160286183969692 ) ) ;
#100033 = CARTESIAN_POINT ( 'NONE',  ( 1.364683531249986537, -0.3864583329919166199, 0.7879004041258500513 ) ) ;
#100034 = CARTESIAN_POINT ( 'NONE',  ( 5.232948167349782409, 0.1380416123818763163, 1.820529236867339584 ) ) ;
#100035 = ORIENTED_EDGE ( 'NONE', *, *, #150613, .T. ) ;
#100036 = CARTESIAN_POINT ( 'NONE',  ( -6.954406449166956605, 7.078172043641714595, -0.7998128361456362523 ) ) ;
#100037 = LINE ( 'NONE', #169299, #119672 ) ;
#100038 = CARTESIAN_POINT ( 'NONE',  ( 1.737499999999999378, -2.872916665710750106, -3.009438278150925683 ) ) ;
#100039 = PRESENTATION_LAYER_ASSIGNMENT (  '', '', ( #207328 ) ) ;
#100040 = CARTESIAN_POINT ( 'NONE',  ( -5.357443255694392725, 9.402100898285455699, 0.000000000000000000 ) ) ;
#100041 = CARTESIAN_POINT ( 'NONE',  ( 2.953383392634020943, -1.779389778202213446, 0.9557246442400985087 ) ) ;
#100042 = CARTESIAN_POINT ( 'NONE',  ( 0.4113322892924773377, 1.832542443981843405, 1.037592781499405259 ) ) ;
#100043 = CARTESIAN_POINT ( 'NONE',  ( 9.134442807305049428, 11.67993591332117376, 1.599625672291281386 ) ) ;
#100044 = CARTESIAN_POINT ( 'NONE',  ( 3.696024482597393135, 0.8403398683093143973, -1.660512506883378370 ) ) ;
#100045 = CARTESIAN_POINT ( 'NONE',  ( 8.809047120577066181, 11.30030761213851953, 1.599625672291281386 ) ) ;
#100046 = CARTESIAN_POINT ( 'NONE',  ( 0.000000000000000000, -7.699999999999998401, 0.000000000000000000 ) ) ;
#100047 = CARTESIAN_POINT ( 'NONE',  ( -3.952365473583647315, 4.569846793057691592, 1.199719254218462483 ) ) ;
#100048 = CARTESIAN_POINT ( 'NONE',  ( -8.128276786592724790, 9.441743324901704426, -1.199719254218446718 ) ) ;
#100049 = CARTESIAN_POINT ( 'NONE',  ( 6.754767742037871336, -1.594745458351163103, 1.305156173170081813 ) ) ;
#100051 = CARTESIAN_POINT ( 'NONE',  ( -4.119138978170663989, 7.660627806941648466, 0.7993094217999627826 ) ) ;
#100050 = CARTESIAN_POINT ( 'NONE',  ( -7.774674742793745708, 8.035151719539642912, 0.7998128361456341429 ) ) ;
#100052 = CARTESIAN_POINT ( 'NONE',  ( 0.6823417656249882723, 0.6760416670080898749, -1.181850606188749264 ) ) ;
#100053 = CARTESIAN_POINT ( 'NONE',  ( 2.213800448916534158, -1.389428533404401422, -1.036884654713841725 ) ) ;
#100054 = CARTESIAN_POINT ( 'NONE',  ( 1.235833198037468827, 0.3363826672934740469, 1.707315539672292104 ) ) ;
#100056 = CARTESIAN_POINT ( 'NONE',  ( 8.812436659202669276, 10.34389285956704363, -1.082531754730543083 ) ) ;
#100055 = CARTESIAN_POINT ( 'NONE',  ( 6.721333375000203780, -0.1674226297891309168, 2.271100132491596479 ) ) ;
#100057 = CARTESIAN_POINT ( 'NONE',  ( -11.52570357830391323, 8.091488070261075194, -2.173620758456770830 ) ) ;
#100058 = CARTESIAN_POINT ( 'NONE',  ( 1.335309304440901235, -1.864295028495915441, 0.8784465167368092908 ) ) ;
#100059 = CARTESIAN_POINT ( 'NONE',  ( 6.179819089730593795, 6.104210447640811665, 1.040834085586084257E-14 ) ) ;
#100060 = CARTESIAN_POINT ( 'NONE',  ( 0.5091384654962345380, 2.010518347751136137, 0.1511200514899835312 ) ) ;
#100061 = FACE_OUTER_BOUND ( 'NONE', #131482, .T. ) ;
#100062 = CARTESIAN_POINT ( 'NONE',  ( -6.283277845290492714, 6.295188672452495915, -0.7998128361456362523 ) ) ;
#100063 = CARTESIAN_POINT ( 'NONE',  ( 6.526239545637954720, 1.075124705556152138, -1.530631868311462362 ) ) ;
#100065 = CARTESIAN_POINT ( 'NONE',  ( -7.295696057929500711, 7.684269287105433222, 0.7216878364870317197 ) ) ;
#100064 = CARTESIAN_POINT ( 'NONE',  ( 4.552931727387078631, 0.3324577288378940954, 1.883125075537089854 ) ) ;
#100066 = CARTESIAN_POINT ( 'NONE',  ( 6.516270054225981490, -1.036149114087565382, -1.948532232987249424 ) ) ;
#100067 = CARTESIAN_POINT ( 'NONE',  ( -6.549078289569726152, -6.948428148671506932, -6.549078289569697731 ) ) ;
#100068 = CARTESIAN_POINT ( 'NONE',  ( 4.882344714252594642, 4.868692719482363707, 0.000000000000000000 ) ) ;
#100069 = CARTESIAN_POINT ( 'NONE',  ( -3.811250578772981346, 6.500190537660166079, -1.082531754730546636 ) ) ;
#100070 = CARTESIAN_POINT ( 'NONE',  ( 0.1178396879437521028, -0.5365784638422869124, 1.947031292057841645 ) ) ;
#100071 = ORIENTED_EDGE ( 'NONE', *, *, #168924, .T. ) ;
#100072 = CARTESIAN_POINT ( 'NONE',  ( 3.382123439733915493, 1.462175888237092547, 1.785228103979496384 ) ) ;
#100073 = CARTESIAN_POINT ( 'NONE',  ( 4.826587731031282580, -1.282962940432516907, 1.484285152025546672 ) ) ;
#100074 = CARTESIAN_POINT ( 'NONE',  ( 1.323018481131872370, -1.771187822987334570, -0.8437873667686208723 ) ) ;
#100075 = CARTESIAN_POINT ( 'NONE',  ( 8.401248741962376698, 12.95320729893149370, 0.7998128361456462443 ) ) ;
#100076 = CARTESIAN_POINT ( 'NONE',  ( -9.438074502436650803, 15.48601905264195899, 7.411038320713698724 ) ) ;
#100077 = ORIENTED_EDGE ( 'NONE', *, *, #44421, .T. ) ;
#100078 = CARTESIAN_POINT ( 'NONE',  ( -0.08258987484092288056, -1.932961894807160963, 0.8646260017347202620 ) ) ;
#100080 = CARTESIAN_POINT ( 'NONE',  ( -6.808165692356648258, 11.09461040772476714, 0.7998128361456481317 ) ) ;
#100079 = CARTESIAN_POINT ( 'NONE',  ( -4.761938266897808525, 6.578680616179308771, 1.599625672291267398 ) ) ;
#100081 = CARTESIAN_POINT ( 'NONE',  ( 1.183273638618479673, -0.8294958387620559037, 1.643756842616146630 ) ) ;
#100082 = EDGE_CURVE ( 'NONE', #123409, #197571, #82040, .T. ) ;
#100083 = CARTESIAN_POINT ( 'NONE',  ( 4.188457025382522403, 1.166365143183651920, -1.831003835250759604 ) ) ;
#100084 = CARTESIAN_POINT ( 'NONE',  ( 10.24619468639153652, 10.82263080639484976, -6.252197070581264171 ) ) ;
#100085 = CARTESIAN_POINT ( 'NONE',  ( 1.810938747355747447, -0.5704394276861005642, -2.042344090522000055 ) ) ;
#100086 = CARTESIAN_POINT ( 'NONE',  ( -1.500000000000011324, 3.452083334016151639, 0.8660254037844403729 ) ) ;
#100087 = CARTESIAN_POINT ( 'NONE',  ( 10.70146331988817323, 11.37946204949139251, 0.7998128361456341429 ) ) ;
#100088 = CARTESIAN_POINT ( 'NONE',  ( 11.97929049433705728, 13.88000000000000078, -0.7046979865771821894 ) ) ;
#100089 = CARTESIAN_POINT ( 'NONE',  ( 6.184762415132515123, 7.051423785172313607, -1.050594063207562545 ) ) ;
#100090 = CARTESIAN_POINT ( 'NONE',  ( 2.653650601580277879, 0.5529494111683015412, -1.985115717065755847 ) ) ;
#100092 = CARTESIAN_POINT ( 'NONE',  ( 7.304951286220124906, 14.53038845894318953, -9.465418723554037683 ) ) ;
#100091 = CARTESIAN_POINT ( 'NONE',  ( -9.854078719034067291, 10.39084668182823634, 0.7998128361456462443 ) ) ;
#100093 = CARTESIAN_POINT ( 'NONE',  ( -0.6823417656250003738, 1.467708333674752730, -1.181850606188749264 ) ) ;
#100094 = CARTESIAN_POINT ( 'NONE',  ( 0.07775346131141076811, 6.946779003630084048, -2.883989925229225815 ) ) ;
#100095 = CARTESIAN_POINT ( 'NONE',  ( 5.835368547082574686, 7.298705356223742058, -1.329342603381425958 ) ) ;
#100096 = VERTEX_POINT ( 'NONE', #35424 ) ;
#100097 = CARTESIAN_POINT ( 'NONE',  ( 4.301352856729808494, 1.706663192164651122, -0.8627939227693476321 ) ) ;
#100098 =( GEOMETRIC_REPRESENTATION_CONTEXT ( 3 ) GLOBAL_UNCERTAINTY_ASSIGNED_CONTEXT ( ( #37695 ) ) GLOBAL_UNIT_ASSIGNED_CONTEXT ( ( #169790, #183903, #33386 ) ) REPRESENTATION_CONTEXT ( 'NONE', 'WORKASPACE' ) );
#100099 = CARTESIAN_POINT ( 'NONE',  ( 11.07790593930098311, 13.79999999999999893, -0.7000000000000009548 ) ) ;
#100100 = CARTESIAN_POINT ( 'NONE',  ( 1.177466099744011174, -0.05591215127281846942, -2.261859306125458158 ) ) ;
#100101 = CARTESIAN_POINT ( 'NONE',  ( -9.571693261567968847, 12.19006144329456731, 1.443375672974076540 ) ) ;
#100102 = CARTESIAN_POINT ( 'NONE',  ( 0.9139796618767962455, -1.811767225755844146, 0.001225010880583424656 ) ) ;
#100103 = CARTESIAN_POINT ( 'NONE',  ( 1.411203511878999173, -1.802517209299081102, 0.6490724346438890846 ) ) ;
#100104 = CARTESIAN_POINT ( 'NONE',  ( 2.840353284027045344, -1.066491845456703835, 1.774417039089710935 ) ) ;
#100105 = CARTESIAN_POINT ( 'NONE',  ( -0.6823417656250212460, 0.8635416670080899859, 1.181850606188755259 ) ) ;
#100106 = CARTESIAN_POINT ( 'NONE',  ( 0.6199196518563926395, -1.052708125740812628, -1.666702442819472774 ) ) ;
#100107 = CARTESIAN_POINT ( 'NONE',  ( 5.022062012317437762, -1.032219231902216761, -1.626458924502146797 ) ) ;
#100109 = CARTESIAN_POINT ( 'NONE',  ( 5.348725299209624140, 7.591689785053232775, -1.238827213252717163 ) ) ;
#100108 = CARTESIAN_POINT ( 'NONE',  ( 1.243279834139981999, 0.4545127484847265031, 2.262342451343732463 ) ) ;
#100110 = CARTESIAN_POINT ( 'NONE',  ( -1.402160292154681736E-14, 1.446875000341420137, -1.575800808251659024 ) ) ;
#100111 = CARTESIAN_POINT ( 'NONE',  ( 4.932111759923301975, 1.184877397895794493, 1.688235060362786255 ) ) ;
#100112 = CARTESIAN_POINT ( 'NONE',  ( -5.526920175865215334, 9.599823971818089774, 0.7998128361456481317 ) ) ;
#100113 = CARTESIAN_POINT ( 'NONE',  ( 7.239163954692881653, 10.53310948286200599, -1.199719254218441611 ) ) ;
#100114 = CARTESIAN_POINT ( 'NONE',  ( -1.000000000000017097, 9.200000000000018829, -0.3999999999999961919 ) ) ;
#100116 = CARTESIAN_POINT ( 'NONE',  ( -1.500000000000011324, 3.920833333333357817, 0.8660254037844403729 ) ) ;
#100115 = CARTESIAN_POINT ( 'NONE',  ( 4.840906100885360885, 0.3572417793257404717, 2.075268335340733739 ) ) ;
#100117 = CARTESIAN_POINT ( 'NONE',  ( 1.399139394074319753, 0.4229888639164773867, 2.129416274499373429 ) ) ;
#100118 = CARTESIAN_POINT ( 'NONE',  ( -1.201851678989727383E-14, 2.884375000341418804, 1.575800808251672791 ) ) ;
#100119 = CARTESIAN_POINT ( 'NONE',  ( 5.097027542433036018, 1.800287743887505121, -1.196142203056582920 ) ) ;
#100120 = CARTESIAN_POINT ( 'NONE',  ( 5.426427855750480589, -0.9099042507111715361, -1.803185865349592021 ) ) ;
#100121 = CARTESIAN_POINT ( 'NONE',  ( -11.89942855770814134, 11.29999999999999893, -0.7000000000000009548 ) ) ;
#100124 = CARTESIAN_POINT ( 'NONE',  ( 4.690757960648221037, 7.456006139856155457, 1.082531754730558626 ) ) ;
#100123 = CARTESIAN_POINT ( 'NONE',  ( -3.285556943750000514, -2.588541666188707513, -1.896917185911906500 ) ) ;
#100122 = CARTESIAN_POINT ( 'NONE',  ( -4.779899193377088906, 14.55303452941223341, -10.96779284377108077 ) ) ;
#100125 = CARTESIAN_POINT ( 'NONE',  ( -5.498713818794216834, 8.572860667638675380, -1.199719254218452047 ) ) ;
#100126 = CARTESIAN_POINT ( 'NONE',  ( 3.098842478760281516, 1.825076540557273974, 0.8578426345753201732 ) ) ;
#100127 = CARTESIAN_POINT ( 'NONE',  ( -7.720478407978036195, 11.09464301169468037, -1.199719254218446718 ) ) ;
#100129 = CARTESIAN_POINT ( 'NONE',  ( -10.94526678918444951, -5.600264386820970941, 0.03132844593997358151 ) ) ;
#100128 = CARTESIAN_POINT ( 'NONE',  ( -2.442440228756222353, 6.001264033524212671, -0.7998128361456281477 ) ) ;
#100130 = CARTESIAN_POINT ( 'NONE',  ( -0.6823417656250212460, 3.301041667008085323, 1.181850606188767472 ) ) ;
#100131 = CARTESIAN_POINT ( 'NONE',  ( 5.067319851952804655, 0.2155487944876262052, -2.150937003660175595 ) ) ;
#100132 = CARTESIAN_POINT ( 'NONE',  ( 6.720655732516647163, -0.004400176169771369272, 2.173773060281408931 ) ) ;
#100134 = CARTESIAN_POINT ( 'NONE',  ( 6.081657687927014777, -0.6766999560612970699, 1.899624756701682626 ) ) ;
#100133 = CARTESIAN_POINT ( 'NONE',  ( -6.846504384776755714, 9.971043634672792422, -1.082531754730537088 ) ) ;
#100135 = CARTESIAN_POINT ( 'NONE',  ( -0.7500000000000215383, 4.691666666666684193, 1.299038105676671107 ) ) ;
#100136 = CARTESIAN_POINT ( 'NONE',  ( 0.9786238818701101794, -0.03817194980801525556, -1.724638339026884903 ) ) ;
#100137 = CARTESIAN_POINT ( 'NONE',  ( 3.413620815590684199, 7.204584394822967752, 0.7998128361456281477 ) ) ;
#100139 = CARTESIAN_POINT ( 'NONE',  ( 6.964048179274811012, 8.153752959689313684, 1.199719254218452047 ) ) ;
#100138 = CARTESIAN_POINT ( 'NONE',  ( 8.432808358020025707, 9.900993174853955026, 1.082531754730558626 ) ) ;
#100140 = CARTESIAN_POINT ( 'NONE',  ( -5.246642258364174971, 5.223430177620755011, 0.7216878364870457085 ) ) ;
#100141 = CARTESIAN_POINT ( 'NONE',  ( 6.591075523649926993, 1.627300515804396941, -0.9222108319836411772 ) ) ;
#100142 = CARTESIAN_POINT ( 'NONE',  ( -0.04036574886347610303, -1.557478217179044888, -1.275100411523772737 ) ) ;
#100143 = CARTESIAN_POINT ( 'NONE',  ( 7.632173801829039911E-16, 0.4330127018922214077, -6.200000000000000178 ) ) ;
#100144 = CARTESIAN_POINT ( 'NONE',  ( -7.282137903871469753, 8.628820655005750240, 1.082531754730549078 ) ) ;
#100145 = EDGE_LOOP ( 'NONE', ( #179899, #145285, #126338, #18515 ) ) ;
#100146 = CARTESIAN_POINT ( 'NONE',  ( 9.368320956918614328, 10.99242454023565507, 1.082531754730549967 ) ) ;
#100148 = CARTESIAN_POINT ( 'NONE',  ( 1.511342449054883019, -1.897691915346022107, 0.6820157586827846341 ) ) ;
#100147 = CARTESIAN_POINT ( 'NONE',  ( 2.209781436637091367, 1.640924847721588975, 1.343087772177023131 ) ) ;
#100149 = CARTESIAN_POINT ( 'NONE',  ( 1.915983733309385872, -1.811150802387480274, 0.04719988836864030118 ) ) ;
#100150 = CARTESIAN_POINT ( 'NONE',  ( 4.895902867866261055, 4.884510565364971413, -0.7216878364870458196 ) ) ;
#100151 = EDGE_CURVE ( 'NONE', #183827, #181742, #101502, .T. ) ;
#100152 = CARTESIAN_POINT ( 'NONE',  ( 6.245025451202089073, -1.828886558906620774, 1.152162773130911644 ) ) ;
#100153 = ORIENTED_EDGE ( 'NONE', *, *, #203402, .T. ) ;
#100155 = ADVANCED_FACE ( 'NONE', ( #214135 ), #68975, .F. ) ;
#100154 = AXIS2_PLACEMENT_3D ( 'NONE', #193372, #45017, #175014 ) ;
#100156 = CARTESIAN_POINT ( 'NONE',  ( 5.452350330990040739, 9.512825819463730070, 0.7998128361456462443 ) ) ;
#100158 = CARTESIAN_POINT ( 'NONE',  ( 0.1455191377820958532, 1.894478286654190269, -0.2837363430458189062 ) ) ;
#100157 = CARTESIAN_POINT ( 'NONE',  ( -4.904298879841297421, 6.744767997946721216, 1.599625672291267398 ) ) ;
#100159 = SURFACE_SIDE_STYLE ('',( #34088 ) ) ;
#100160 = DIRECTION ( 'NONE',  ( 0.000000000000000000, 0.000000000000000000, 1.000000000000000000 ) ) ;
#100161 = CARTESIAN_POINT ( 'NONE',  ( 5.219525951136835928, 7.112532914458205013, -1.443375672974051449 ) ) ;
#100162 = CARTESIAN_POINT ( 'NONE',  ( -1.364683531250014514, -0.1989583329919157317, -0.7879004041258359514 ) ) ;
#100163 = CARTESIAN_POINT ( 'NONE',  ( 3.606105671554957759, 4.269840040644637291, -1.082531754730543083 ) ) ;
#100164 = CARTESIAN_POINT ( 'NONE',  ( -8.435144125996554720, 12.99275191363802229, 0.7998128361456341429 ) ) ;
#100165 = CARTESIAN_POINT ( 'NONE',  ( 4.557600102482579629, 0.4766696971462945909, -2.108333899287537339 ) ) ;
#100166 = CARTESIAN_POINT ( 'NONE',  ( -5.139949633356594383, 9.010708648975750634, 0.000000000000000000 ) ) ;
#100167 = CARTESIAN_POINT ( 'NONE',  ( 5.722950238744209273, 6.809768379023969587, 1.082531754730549967 ) ) ;
#100168 = CARTESIAN_POINT ( 'NONE',  ( 2.267978396857213585, 0.5610993688725562922, -2.044979925899123252 ) ) ;
#100169 = CARTESIAN_POINT ( 'NONE',  ( 6.756878055424797580, -1.408711550780303412, 1.160885376127060553 ) ) ;
#100170 = CARTESIAN_POINT ( 'NONE',  ( 3.233620971007169942, -1.321289716990686980, -1.463211747571713461 ) ) ;
#100171 = CARTESIAN_POINT ( 'NONE',  ( 5.801015586618943232, -0.2871438832755985326, -1.890612906794430614 ) ) ;
#100172 = ORIENTED_EDGE ( 'NONE', *, *, #189732, .T. ) ;
#100173 = CARTESIAN_POINT ( 'NONE',  ( 9.606148981167445200, -6.583980363594983842, -0.4355862708379997228 ) ) ;
#100174 = CARTESIAN_POINT ( 'NONE',  ( 6.461384246211865801, 1.636644077835234246, 1.095356925007910265 ) ) ;
#100175 = CARTESIAN_POINT ( 'NONE',  ( 1.587728922880219384, -1.932555244376774617, -0.1907308274580049312 ) ) ;
#100176 = ORIENTED_EDGE ( 'NONE', *, *, #193642, .F. ) ;
#100177 = CARTESIAN_POINT ( 'NONE',  ( -5.483346782084204563, 5.361935765378481378, 0.000000000000000000 ) ) ;
#100179 = CARTESIAN_POINT ( 'NONE',  ( 1.872311050889111650, 2.480935488296869273, -2.470734331491561520 ) ) ;
#100178 = CARTESIAN_POINT ( 'NONE',  ( -5.126391479742927970, 8.994890803093138487, 0.7216878364870267237 ) ) ;
#100180 = CARTESIAN_POINT ( 'NONE',  ( 6.551614543901692400, 8.666636272683888365, 1.599625672291281386 ) ) ;
#100182 = CARTESIAN_POINT ( 'NONE',  ( 5.031484404002879884, 6.963427452793765404, 1.443375672974065660 ) ) ;
#100181 = CARTESIAN_POINT ( 'NONE',  ( 5.459129407796876166, 9.520734742405036144, 1.040834085586084257E-14 ) ) ;
#100184 = EDGE_LOOP ( 'NONE', ( #188504, #150207, #209715, #209111 ) ) ;
#100183 = CARTESIAN_POINT ( 'NONE',  ( 6.024064539286675846, -1.897261554996135802, 0.2387622092476364699 ) ) ;
#100185 = CARTESIAN_POINT ( 'NONE',  ( 2.807470779205251343, 1.864772411128329477, 1.179945617918669143 ) ) ;
#100186 = CARTESIAN_POINT ( 'NONE',  ( 2.309865001130634976, -0.4838574416936823885, 2.152911442350906146 ) ) ;
#100187 = DIRECTION ( 'NONE',  ( 0.1510067114093955887, 0.000000000000000000, 0.9885327375000383388 ) ) ;
#100188 = CARTESIAN_POINT ( 'NONE',  ( 1.084454188491505988, -1.212558158303609135, 1.478703618145213783 ) ) ;
#100189 = CARTESIAN_POINT ( 'NONE',  ( -0.4363033266127427923, -8.563898737988809629, 10.12670668089736736 ) ) ;
#100190 = CARTESIAN_POINT ( 'NONE',  ( 11.52901446936659013, 13.79425527467587465, -3.330874149800854944 ) ) ;
#100191 = CARTESIAN_POINT ( 'NONE',  ( 4.457524453155742528, 1.660904245173303373, 1.235824716467534667 ) ) ;
#100192 = CARTESIAN_POINT ( 'NONE',  ( -4.076197739202962467, 7.907314462378773001, 1.040834085586084257E-14 ) ) ;
#100194 = CARTESIAN_POINT ( 'NONE',  ( 1.797963993548271411, -0.7283430984801853025, 2.035426966748521860 ) ) ;
#100193 = CARTESIAN_POINT ( 'NONE',  ( -3.090368948911150770, 5.692848642783215674, 1.199719254218462483 ) ) ;
#100195 = CARTESIAN_POINT ( 'NONE',  ( 3.773127072069931032, 2.063069237518061705, -0.7396954945804237180 ) ) ;
#100196 = CARTESIAN_POINT ( 'NONE',  ( -4.891544523420352952, 7.514763430510271291, 1.198184914803653633 ) ) ;
#100197 = DIRECTION ( 'NONE',  ( 0.9486832980505138790, -0.3162277660168376636, -3.312310031615527152E-15 ) ) ;
#100198 = CARTESIAN_POINT ( 'NONE',  ( 1.500000000000009104, 4.785416667349486453, 0.8660254037844407060 ) ) ;
#100199 = CARTESIAN_POINT ( 'NONE',  ( -1.364683531250000748, 13.92187500034140157, 0.000000000000000000 ) ) ;
#100200 = CARTESIAN_POINT ( 'NONE',  ( -4.782994330570982555, 8.802186828966616972, 0.000000000000000000 ) ) ;
#100201 = CARTESIAN_POINT ( 'NONE',  ( 6.047464834240314779, -1.219521636822028077, 1.233209766127696616 ) ) ;
#100202 = CARTESIAN_POINT ( 'NONE',  ( -8.649738815838677652, 13.03518635187974262, 0.7216878364870357165 ) ) ;
#100203 = CARTESIAN_POINT ( 'NONE',  ( 3.028250241984064228, 1.103615759228196325, 1.751372171329562688 ) ) ;
#100204 = CARTESIAN_POINT ( 'NONE',  ( 6.134383104757832328, 0.6643169034818379171, 2.010352329694592655 ) ) ;
#100205 = CARTESIAN_POINT ( 'NONE',  ( 5.717788096661236885, 7.693838750903348789, 1.599625672291267398 ) ) ;
#100206 = CARTESIAN_POINT ( 'NONE',  ( -1.364683531250010740, 5.030208333674756283, 0.7879004041258379498 ) ) ;
#100207 = CARTESIAN_POINT ( 'NONE',  ( 3.414863416077691838, -1.494280747806640885, 1.283048038104795507 ) ) ;
#100208 = CARTESIAN_POINT ( 'NONE',  ( 0.5274218815167727170, -0.2782315536139517431, 1.891897276498944347 ) ) ;
#100209 = CARTESIAN_POINT ( 'NONE',  ( 5.578174268327147800, -2.235363620237617255, -0.5069547310770585735 ) ) ;
#100210 = CARTESIAN_POINT ( 'NONE',  ( 2.385134503015675200, 1.669401249834654211, -0.7394980648879891927 ) ) ;
#100211 = CARTESIAN_POINT ( 'NONE',  ( 5.401997860402196316, 5.267028690082820930, 0.000000000000000000 ) ) ;
#100213 = EDGE_CURVE ( 'NONE', #53056, #207943, #54249, .T. ) ;
#100212 = CARTESIAN_POINT ( 'NONE',  ( 4.324687812634882000, 7.028924300507257250, 1.082531754730558626 ) ) ;
#100214 = CARTESIAN_POINT ( 'NONE',  ( -6.507023659554960204, 9.678945805201045971, 1.199719254218452047 ) ) ;
#100215 = ORIENTED_EDGE ( 'NONE', *, *, #66008, .F. ) ;
#100216 = ORIENTED_EDGE ( 'NONE', *, *, #194375, .T. ) ;
#100217 = CARTESIAN_POINT ( 'NONE',  ( 3.814701174604028466, -0.6354162253871125099, -1.910337659313849024 ) ) ;
#100218 = CARTESIAN_POINT ( 'NONE',  ( 4.416819765676714304, -1.456490764316048292, 1.314424223973277961 ) ) ;
#100219 = CARTESIAN_POINT ( 'NONE',  ( -6.482770005628665011, 10.71498210654212002, 0.7998128361456481317 ) ) ;
#100220 = CARTESIAN_POINT ( 'NONE',  ( -4.894657149733403045, 5.669187081899118574, -1.199719254218446718 ) ) ;
#100221 = CARTESIAN_POINT ( 'NONE',  ( 0.07536363704233051131, 7.629137130509080045, -2.744199452819145790 ) ) ;
#100223 = CARTESIAN_POINT ( 'NONE',  ( 5.295665003108637414, -0.6346038033320391403, 1.652335088206556613 ) ) ;
#100222 = CARTESIAN_POINT ( 'NONE',  ( -0.1116087887279961222, -0.4605761454780517572, -2.046466910313152532 ) ) ;
#100224 = CARTESIAN_POINT ( 'NONE',  ( 10.99948089704798271, -5.389012432655394313, -0.1178541238725870494 ) ) ;
#100225 = CARTESIAN_POINT ( 'NONE',  ( 2.009981539508858273, -1.034714594384738229, -1.931790675223004738 ) ) ;
#100226 = CARTESIAN_POINT ( 'NONE',  ( 6.580030513128129144, -1.708294420148011472, -0.3314369902002142765 ) ) ;
#100227 = CARTESIAN_POINT ( 'NONE',  ( 7.772902139336337335, 7.962807338847539107, 0.7998128361456341429 ) ) ;
#100228 = CARTESIAN_POINT ( 'NONE',  ( 0.9786238818701101794, -0.03817194980801525556, -1.724638339026884903 ) ) ;
#100229 = CARTESIAN_POINT ( 'NONE',  ( 1.107258645251009144, 0.9300933289658299685, -2.101954592823534362 ) ) ;
#100231 = EDGE_CURVE ( 'NONE', #32206, #62256, #189064, .T. ) ;
#100230 = CARTESIAN_POINT ( 'NONE',  ( 0.8729168595149154886, -0.05911722906676297740, -2.190938979806676734 ) ) ;
#100232 = CARTESIAN_POINT ( 'NONE',  ( 6.169268014014505752, -0.6277043665407368023, -1.616433383845305105 ) ) ;
#100233 = CARTESIAN_POINT ( 'NONE',  ( 2.860232119962682784, 2.196193069775736362, -0.2169517147150926140 ) ) ;
#100234 = CARTESIAN_POINT ( 'NONE',  ( 6.742638747055813120, -2.127943412135436585, -0.4303581323979056017 ) ) ;
#100235 = CARTESIAN_POINT ( 'NONE',  ( -1.150196859685106876, 3.020291321728038714, 0.7750000000000152323 ) ) ;
#100236 = CARTESIAN_POINT ( 'NONE',  ( 2.079462195143897851, 1.640249684897076898, 1.338979269010678985 ) ) ;
#100237 = CARTESIAN_POINT ( 'NONE',  ( 6.827182134110198142, 3.677047352536796154, 2.802821765677898203 ) ) ;
#100238 = CARTESIAN_POINT ( 'NONE',  ( 5.473632971755619359, 1.856580101505003411, -0.5137103415125721106 ) ) ;
#100239 = ORIENTED_EDGE ( 'NONE', *, *, #173052, .T. ) ;
#100241 = CARTESIAN_POINT ( 'NONE',  ( 0.7499999999999920064, 5.233333333333353821, 1.299038105676669330 ) ) ;
#100240 = CARTESIAN_POINT ( 'NONE',  ( 2.560454162224240271, -1.578354536769586591, 1.662689614829175211 ) ) ;
#100242 = CARTESIAN_POINT ( 'NONE',  ( 4.518945272056516416, 4.166524327021037699, 0.7998128361456341429 ) ) ;
#100243 = CARTESIAN_POINT ( 'NONE',  ( 4.843287188579786573, 6.673587691474970107, -1.599625672291256295 ) ) ;
#100244 = CARTESIAN_POINT ( 'NONE',  ( 5.092532722643547061, -1.235012376581679172, 1.846140261684477091 ) ) ;
#100245 = CARTESIAN_POINT ( 'NONE',  ( -8.365017589951714072, 8.861534731139549592, 1.040834085586084257E-14 ) ) ;
#100246 = CYLINDRICAL_SURFACE ( 'NONE', #170419, 1.250000000000000000 ) ;
#100247 = CARTESIAN_POINT ( 'NONE',  ( 5.992340707560151358, 8.014150130285418783, 1.443375672974062551 ) ) ;
#100248 = CARTESIAN_POINT ( 'NONE',  ( -6.683806541412756985, 10.74159869838281622, -0.7216878364870267237 ) ) ;
#100249 = CARTESIAN_POINT ( 'NONE',  ( 4.882344714696929877, 8.710169577206153591, -0.7216878364870458196 ) ) ;
#100250 = ORIENTED_EDGE ( 'NONE', *, *, #42999, .T. ) ;
#100251 = CARTESIAN_POINT ( 'NONE',  ( 2.549454116737331244, -1.388485404012842261, 1.462446031800922253 ) ) ;
#100253 = CARTESIAN_POINT ( 'NONE',  ( 0.8661725458788569476, -2.052963606700756394, 0.1985000389403013821 ) ) ;
#100252 = CARTESIAN_POINT ( 'NONE',  ( 5.926885707468349196, 10.06645042535509660, 1.040834085586084257E-14 ) ) ;
#100254 =( NAMED_UNIT ( * ) SI_UNIT ( $, .STERADIAN. ) SOLID_ANGLE_UNIT ( ) );
#100255 = CARTESIAN_POINT ( 'NONE',  ( 7.146556367734776316, 7.510272981878305387, 0.7216878364870267237 ) ) ;
#100257 = EDGE_CURVE ( 'NONE', #71638, #189856, #12770, .T. ) ;
#100256 = CARTESIAN_POINT ( 'NONE',  ( -15.75000000000000000, 9.799999999999998934, -1.800000000000001155 ) ) ;
#100258 = CARTESIAN_POINT ( 'NONE',  ( 1.364683531249990311, 3.134375000341423245, 1.214306433183764966E-14 ) ) ;
#100259 = CARTESIAN_POINT ( 'NONE',  ( 3.627062487484993714, -2.024900418628313936, 0.8384617360315260726 ) ) ;
#100260 = CARTESIAN_POINT ( 'NONE',  ( 1.600232647554021392, -0.2440283035436350279, 2.001511509883910911 ) ) ;
#100261 = CARTESIAN_POINT ( 'NONE',  ( 0.9074547957551477584, -0.8278116715597811925, -1.644758345054016191 ) ) ;
#100262 = CARTESIAN_POINT ( 'NONE',  ( 5.214511053166543064, 2.117144789807279270, 0.8794703464902029477 ) ) ;
#100263 = CARTESIAN_POINT ( 'NONE',  ( 4.013478867934616723, -0.9481684062532383939, -1.578073411074693899 ) ) ;
#100264 = ADVANCED_FACE ( 'NONE', ( #21290 ), #196030, .T. ) ;
#100265 = CARTESIAN_POINT ( 'NONE',  ( 8.308449207076147758, 8.587612251210650527, -0.7998128361456281477 ) ) ;
#100266 =( LENGTH_UNIT ( ) NAMED_UNIT ( * ) SI_UNIT ( .MILLI., .METRE. ) );
#100267 = CARTESIAN_POINT ( 'NONE',  ( 3.979382468966369935, 1.719079831940514502, -0.6148086763930470378 ) ) ;
#100268 = CARTESIAN_POINT ( 'NONE',  ( 4.447888798048591497, -1.802416534049579910, -0.9041112711936499791 ) ) ;
#100269 = CARTESIAN_POINT ( 'NONE',  ( -7.153898609505128015, 11.49796547773133604, 0.7998128361456481317 ) ) ;
#100271 = CARTESIAN_POINT ( 'NONE',  ( -4.782994330570982555, 8.802186828966616972, 0.000000000000000000 ) ) ;
#100270 = CARTESIAN_POINT ( 'NONE',  ( 4.698257824713211406, -2.261882422057570619, -0.06011341499151043322 ) ) ;
#100272 = CARTESIAN_POINT ( 'NONE',  ( 0.08283480907551789285, -2.043431366640800384, -0.5094137356045270737 ) ) ;
#100273 = CARTESIAN_POINT ( 'NONE',  ( 5.195788487752976081, -1.461605715988937515, -1.466586839339318882 ) ) ;
#100274 = CARTESIAN_POINT ( 'NONE',  ( 8.727698198895078363, 11.20540053684285553, -1.599625672291257406 ) ) ;
#100275 = CARTESIAN_POINT ( 'NONE',  ( 0.6801582343750022241, 2.838541667008094738, -1.178068619123834759 ) ) ;
#100276 = APPLICATION_PROTOCOL_DEFINITION ( 'draft international standard', 'automotive_design', 1998, #168032 ) ;
#100278 = CARTESIAN_POINT ( 'NONE',  ( 2.490742943097464135, -0.3295026218355610603, -1.897965567226393979 ) ) ;
#100277 = CARTESIAN_POINT ( 'NONE',  ( -7.316596452869116973, 11.68777962832266049, 0.7998128361456481317 ) ) ;
#100279 = FACE_OUTER_BOUND ( 'NONE', #83101, .T. ) ;
#100280 = CARTESIAN_POINT ( 'NONE',  ( 0.3968417698968416674, 0.3330189415953662690, 1.941018003364772593 ) ) ;
#100281 = CARTESIAN_POINT ( 'NONE',  ( 5.528692779322568640, 9.672168352510192690, 0.7998128361456341429 ) ) ;
#100282 = CARTESIAN_POINT ( 'NONE',  ( 5.430853319176391025, 6.270791292598644873, -1.030804022418196464 ) ) ;
#100283 = CARTESIAN_POINT ( 'NONE',  ( -8.514157279702017078, 12.87700789305364069, -0.7216878364870267237 ) ) ;
#100285 = CARTESIAN_POINT ( 'NONE',  ( 1.881385292706035051, -2.033259550720186049, -0.8950972351880029931 ) ) ;
#100284 = CARTESIAN_POINT ( 'NONE',  ( 0.8793290508635929204, -1.919567575575848339, -0.9014759086384205311 ) ) ;
#100286 = CARTESIAN_POINT ( 'NONE',  ( 3.364387735031381332, 0.9452183826245286191, 1.881983119561444040 ) ) ;
#100287 = CARTESIAN_POINT ( 'NONE',  ( -5.589704470584107909, 9.743348658981940247, -0.7998128361456362523 ) ) ;
#100288 = CARTESIAN_POINT ( 'NONE',  ( 6.252281394196331554, 10.44607872653774372, 1.040834085586084257E-14 ) ) ;
#100289 = CARTESIAN_POINT ( 'NONE',  ( 3.385159196556942085, 0.04556868695702701727, 1.961494628812537444 ) ) ;
#100290 = CARTESIAN_POINT ( 'NONE',  ( 6.661133543015731462, 6.665743976473484267, -0.7998128361456281477 ) ) ;
#100291 = CARTESIAN_POINT ( 'NONE',  ( -4.054949276293840832, 7.568305524423037056, 0.4105793130844727079 ) ) ;
#100292 = CARTESIAN_POINT ( 'NONE',  ( 4.792970997630896512, 5.550553237779539018, 1.199719254218464037 ) ) ;
#100293 = CARTESIAN_POINT ( 'NONE',  ( -6.943184063974186415, 7.273005294157565359, -0.7216878364870338292 ) ) ;
#100294 = CARTESIAN_POINT ( 'NONE',  ( -8.365017589951714072, 8.861534731139549592, 1.040834085586084257E-14 ) ) ;
#100295 = CARTESIAN_POINT ( 'NONE',  ( 1.617596980227502756, 1.765956010477184535, 1.173731981927571555 ) ) ;
#100296 = CARTESIAN_POINT ( 'NONE',  ( -7.123883369337781879, 7.275895117174344229, 0.7998128361456341429 ) ) ;
#100298 = CARTESIAN_POINT ( 'NONE',  ( 4.896903505236655185, 0.3334610245491422265, 1.933150054703360432 ) ) ;
#100297 = CARTESIAN_POINT ( 'NONE',  ( 0.6124999999999914957, 1.333333333333339255, 1.060881119635932679 ) ) ;
#100300 = CARTESIAN_POINT ( 'NONE',  ( 3.749029689823797806, -1.768526636652943296, 1.242828150824742961 ) ) ;
#100299 = B_SPLINE_CURVE_WITH_KNOTS ( 'NONE', 3,
 ( #196643, #77551, #46148, #143674, #163089, #177198, #64506, #27741, #80764, #180390, #129595, #113333, #93836, #195582, #112261, #160949 ),
 .UNSPECIFIED., .F., .F.,
 ( 4, 2, 2, 2, 2, 2, 2, 4 ),
 ( 8.553866477534004096E-06, 0.002693891933807479599, 0.004036560967472453514, 0.005379230001137425693, 0.006721899034802396138, 0.008064568068467368317, 0.009407237102132339629, 0.01074990613579731094 ),
 .UNSPECIFIED. ) ;
#100301 = CARTESIAN_POINT ( 'NONE',  ( 2.366542893654680402, 0.08848056876738576160, -1.839231530397527736 ) ) ;
#100302 = CARTESIAN_POINT ( 'NONE',  ( -4.275059339850010076, 7.289437269727999436, -0.9335736327708322735 ) ) ;
#100303 = CARTESIAN_POINT ( 'NONE',  ( -3.285556943750000070, -0.1112512837626866702, 0.000000000000000000 ) ) ;
#100304 = CARTESIAN_POINT ( 'NONE',  ( 4.312277775531628166, 1.592579213294993634, 0.7021690120074929320 ) ) ;
#100305 = CARTESIAN_POINT ( 'NONE',  ( 0.3554123170485448124, 15.00000000000058265, -12.67999999502907471 ) ) ;
#100306 = CARTESIAN_POINT ( 'NONE',  ( 6.493992391265805075, 6.678671999339316656, 1.040834085586084257E-14 ) ) ;
#100307 = CARTESIAN_POINT ( 'NONE',  ( -10.07159190936562432, 5.946254181132138328, -5.792974557957699666 ) ) ;
#100308 = CARTESIAN_POINT ( 'NONE',  ( 1.920999885407469243, 2.016935458891587096, 0.7782144962657986387 ) ) ;
#100309 = AXIS2_PLACEMENT_3D ( 'NONE', #39959, #186180, #24748 ) ;
#100310 = CARTESIAN_POINT ( 'NONE',  ( 4.850935385407137979, -0.9528642855485233154, 1.776740034556321568 ) ) ;
#100311 = CARTESIAN_POINT ( 'NONE',  ( 1.639762333045853726, -1.565812861550972324, -1.490595759849028035 ) ) ;
#100312 = CARTESIAN_POINT ( 'NONE',  ( 3.555508008102294060, 0.4801912113073670829, -1.911968381370426684 ) ) ;
#100313 = CARTESIAN_POINT ( 'NONE',  ( -6.495588733991166208, 6.829233952181008149, 0.6942782964225120423 ) ) ;
#100314 = B_SPLINE_CURVE_WITH_KNOTS ( 'NONE', 3,
 ( #33233, #199983, #117755, #151263, #184796, #36424, #16959, #102500, #168564, #20163 ),
 .UNSPECIFIED., .F., .F.,
 ( 4, 1, 1, 1, 1, 1, 1, 4 ),
 ( 0.000000000000000000, 0.09790276019723312406, 0.1918320694002237370, 0.2608036337010187777, 0.3626611837559554630, 0.5214803378330250538, 0.7337833476510040587, 1.000000000000000000 ),
 .UNSPECIFIED. ) ;
#100315 = CARTESIAN_POINT ( 'NONE',  ( 3.544416897000971289, -1.586007893901800969, 1.120530928797113246 ) ) ;
#100318 = EDGE_LOOP ( 'NONE', ( #40127, #57102, #21906, #109189 ) ) ;
#100317 = CARTESIAN_POINT ( 'NONE',  ( -3.174017359375036929, 6.717120995997236221, 0.7216878364870338292 ) ) ;
#100316 = CARTESIAN_POINT ( 'NONE',  ( -8.473482818416657736, 12.82955435488738516, -0.7216878364870267237 ) ) ;
#100319 = CARTESIAN_POINT ( 'NONE',  ( -5.596483547390937119, 9.751257581923240991, 0.000000000000000000 ) ) ;
#100320 = CARTESIAN_POINT ( 'NONE',  ( 4.598150373690133463, 5.393538853173795111, -1.199719254218452047 ) ) ;
#100321 = CARTESIAN_POINT ( 'NONE',  ( -5.113360211009450040, 5.994616996712990975, -1.199719254218453823 ) ) ;
#100322 = CARTESIAN_POINT ( 'NONE',  ( -6.469175572376043348, 7.576401584974034265, 1.199719254218452047 ) ) ;
#100323 = CARTESIAN_POINT ( 'NONE',  ( -10.27671724903424888, 11.09185100006920877, 1.040834085586084257E-14 ) ) ;
#100324 = CARTESIAN_POINT ( 'NONE',  ( 0.2709337360254741034, -1.439471777561899035, 1.672717458380864608 ) ) ;
#100325 = CARTESIAN_POINT ( 'NONE',  ( -1.642778471875000035, -3.667708332855373676, -2.845375778867859751 ) ) ;
#100326 = CARTESIAN_POINT ( 'NONE',  ( 5.225427317040848507, 0.1961275920050585819, -1.951957996302315257 ) ) ;
#100327 = CARTESIAN_POINT ( 'NONE',  ( 1.688125190044654556, 1.678006053171029688, 1.117831401076685660 ) ) ;
#100328 = VERTEX_POINT ( 'NONE', #5036 ) ;
#100329 = CARTESIAN_POINT ( 'NONE',  ( 3.749298086285374865, 0.2552367968642406115, -2.101811201404654827 ) ) ;
#100330 = CARTESIAN_POINT ( 'NONE',  ( 0.7499999999999902300, 2.264583334016148530, 1.299038105676669330 ) ) ;
#100332 = CARTESIAN_POINT ( 'NONE',  ( -7.054319997812058318, 7.124461507069184130, 1.040834085586084257E-14 ) ) ;
#100331 = CARTESIAN_POINT ( 'NONE',  ( 9.586610838029429260, -7.161464053357567749, -0.003376046620571108124 ) ) ;
#100333 = CARTESIAN_POINT ( 'NONE',  ( 4.101369424419714527, -1.836060619117799497, 0.1375280490283348478 ) ) ;
#100334 = ORIENTED_EDGE ( 'NONE', *, *, #191341, .F. ) ;
#100335 = UNCERTAINTY_MEASURE_WITH_UNIT (LENGTH_MEASURE( 1.000000000000000082E-05 ), #107185, 'distance_accuracy_value', 'NONE');
#100336 = CARTESIAN_POINT ( 'NONE',  ( -7.635213062790267458, 12.05949900656400686, 0.000000000000000000 ) ) ;
#100337 =( NAMED_UNIT ( * ) SI_UNIT ( $, .STERADIAN. ) SOLID_ANGLE_UNIT ( ) );
#100338 = CARTESIAN_POINT ( 'NONE',  ( 5.730757696090861941, 1.422813033107739988, -1.572628729999878905 ) ) ;
#100339 = CARTESIAN_POINT ( 'NONE',  ( -5.534330892379054845, 5.955497452077792353, -0.9177112583351170194 ) ) ;
#100340 = CARTESIAN_POINT ( 'NONE',  ( 6.205881626753210867, 8.263281202677319470, 1.599625672291281386 ) ) ;
#100341 = CARTESIAN_POINT ( 'NONE',  ( 5.800091581907264704, -2.060967560761736372, -0.004405934171711199318 ) ) ;
#100344 = CARTESIAN_POINT ( 'NONE',  ( 2.471991059931688106, -1.762569054296094340, -0.5325411743367302053 ) ) ;
#100343 = CARTESIAN_POINT ( 'NONE',  ( 1.134942894344723507, -0.04051261866679262136, -1.860784445789311903 ) ) ;
#100342 = CARTESIAN_POINT ( 'NONE',  ( -3.147653791585727667, 8.920000000000001705, -2.499999999999998668 ) ) ;
#100345 = CARTESIAN_POINT ( 'NONE',  ( 8.072990401933337168, 11.50590700464255356, -1.199719254218446718 ) ) ;
#100346 = CARTESIAN_POINT ( 'NONE',  ( 4.184706906422049677, 7.590773377626947038, -0.8858016570119742195 ) ) ;
#100347 = CARTESIAN_POINT ( 'NONE',  ( -1.403499169903600574, 7.376709478543776122, 4.304123474983186703 ) ) ;
#100348 = CARTESIAN_POINT ( 'NONE',  ( 0.6124999999999932720, 2.229166667349451014, -1.060881119635948444 ) ) ;
#100349 = CARTESIAN_POINT ( 'NONE',  ( 1.682535984017709874, -1.178549783888741320, 1.865657194899547733 ) ) ;
#100350 = CARTESIAN_POINT ( 'NONE',  ( 5.079486683540675784, 2.113528219476542347, -0.8076395688127128158 ) ) ;
#100351 = CARTESIAN_POINT ( 'NONE',  ( -6.399085315970137522, 9.449054721065074602, -1.082531754730538864 ) ) ;
#100352 = CARTESIAN_POINT ( 'NONE',  ( 4.236430684147264536, 1.109505083903281619, -1.432011362939947574 ) ) ;
#100353 = CARTESIAN_POINT ( 'NONE',  ( 5.735529463276822781, 0.5494309942872098729, -1.835271804430014919 ) ) ;
#100354 = CARTESIAN_POINT ( 'NONE',  ( -1.364683531250010295, 5.592708333674750953, 0.7879004041258379498 ) ) ;
#100355 = AXIS2_PLACEMENT_3D ( 'NONE', #144734, #194500, #46145 ) ;
#100356 = CARTESIAN_POINT ( 'NONE',  ( 5.049604242677837362, 0.5861553263475408615, -1.776501995420045832 ) ) ;
#100357 = CARTESIAN_POINT ( 'NONE',  ( 4.474962758555542486, 1.701137449889396747, 0.7551977096921670407 ) ) ;
#100358 = CARTESIAN_POINT ( 'NONE',  ( -1.364683531249997417, 5.759375000341418804, 1.214306433183764966E-14 ) ) ;
#100359 = CARTESIAN_POINT ( 'NONE',  ( 5.401144703012512593, 1.448466425555764658, 1.016686210146000358 ) ) ;
#100360 = CARTESIAN_POINT ( 'NONE',  ( 0.07540816263147330500, 1.497505997221737273, 1.350731191893522976 ) ) ;
#100362 = CARTESIAN_POINT ( 'NONE',  ( 1.471456325463766479, 0.1532790705911575568, -2.100547924479207129 ) ) ;
#100361 = CARTESIAN_POINT ( 'NONE',  ( -2.751941993449643409, 6.154423392425789174, 0.7216878364870317197 ) ) ;
#100363 = CARTESIAN_POINT ( 'NONE',  ( 8.778014389843965759, 12.32843499053828928, 1.199719254218450271 ) ) ;
#100365 = CARTESIAN_POINT ( 'NONE',  ( -1.206235080191141895, 2.838937307313431191, -0.7749999999999979128 ) ) ;
#100364 = CARTESIAN_POINT ( 'NONE',  ( -10.87339650836132776, 5.131772588966429183, -5.487095527168452058 ) ) ;
#100366 = CARTESIAN_POINT ( 'NONE',  ( 3.533539421053989660, -0.1523460092780377639, 2.115156586662121363 ) ) ;
#100367 = CARTESIAN_POINT ( 'NONE',  ( -10.15369940311292929, 1.000000000000000888, -6.195664267729944719 ) ) ;
#100368 = CARTESIAN_POINT ( 'NONE',  ( 2.109634291106620818, 1.563931847922779728, 1.278184196155268904 ) ) ;
#100369 = CARTESIAN_POINT ( 'NONE',  ( 1.364683531249988535, 2.613541667008089764, 0.7879004041258500513 ) ) ;
#100370 = CARTESIAN_POINT ( 'NONE',  ( -0.07933194154488934502, -7.609852571077998284, 9.499668754385634628 ) ) ;
#100371 = CARTESIAN_POINT ( 'NONE',  ( 5.034155109375821446, 4.767602470560229122, -0.7998128361456221525 ) ) ;
#100372 = ORIENTED_EDGE ( 'NONE', *, *, #23766, .T. ) ;
#100373 = CARTESIAN_POINT ( 'NONE',  ( 1.968271169257681752, 1.109365460190291586, 1.855047589327807778 ) ) ;
#100374 = CARTESIAN_POINT ( 'NONE',  ( 6.889999999999970370, 3.679256271150095792, 2.793895465809397294 ) ) ;
#100377 = CARTESIAN_POINT ( 'NONE',  ( 4.647606103345025552, 8.407977806742819027, 0.6343139517084724899 ) ) ;
#100376 = CARTESIAN_POINT ( 'NONE',  ( 0.7500000000000006661, 13.11458333401613352, 1.299038105676657340 ) ) ;
#100375 = CARTESIAN_POINT ( 'NONE',  ( 4.329849954717849947, 6.144853928627882489, 1.599625672291262513 ) ) ;
#100378 = CARTESIAN_POINT ( 'NONE',  ( 7.876924059415351564, 12.13356913605253240, -0.7216878364870267237 ) ) ;
#100379 = CARTESIAN_POINT ( 'NONE',  ( -8.042162931142703641, -6.699677480914128402, 7.505515594164491766 ) ) ;
#100380 = CARTESIAN_POINT ( 'NONE',  ( -6.236387472606141458, 10.21960978477508952, -0.7216878364870278340 ) ) ;
#100381 = CARTESIAN_POINT ( 'NONE',  ( 0.4861908890553789941, -2.175720422541329580, -0.2624175912114696252 ) ) ;
#100382 = CARTESIAN_POINT ( 'NONE',  ( 0.5528008270654922729, 7.812676398891469809, 1.922238454054872037 ) ) ;
#100383 = CARTESIAN_POINT ( 'NONE',  ( 1.411376899827078368, 1.996129479730743617, 1.065132602888875457 ) ) ;
#100384 = CARTESIAN_POINT ( 'NONE',  ( -7.344766530301162000, 9.591980256816594164, 1.599625672291295375 ) ) ;
#100385 = CARTESIAN_POINT ( 'NONE',  ( 4.452361426671761713, -1.313546101436880109, 1.530156479064001207 ) ) ;
#100386 = CARTESIAN_POINT ( 'NONE',  ( -5.219525951136862574, 5.191794485855519170, -0.7216878364870197293 ) ) ;
#100387 = CARTESIAN_POINT ( 'NONE',  ( -1.364683531250012516, 2.592708333674753174, 0.7879004041258379498 ) ) ;
#100388 = CARTESIAN_POINT ( 'NONE',  ( 4.702859892337409420, 8.240897811179339172, 0.6291740908887258898 ) ) ;
#100389 = ADVANCED_FACE ( 'NONE', ( #171844 ), #102637, .T. ) ;
#100390 = CARTESIAN_POINT ( 'NONE',  ( -0.7500000000000006661, 10.95833333333333393, -1.299038105676657340 ) ) ;
#100391 = CARTESIAN_POINT ( 'NONE',  ( 6.373741612200160667, 9.489763409991955001, 1.082531754730549078 ) ) ;
#100392 = CARTESIAN_POINT ( 'NONE',  ( 3.690472162876729190, -0.3426837954879756731, -1.736044821310823938 ) ) ;
#100393 = CARTESIAN_POINT ( 'NONE',  ( 6.247136877606230598, -1.867572634706683443, 1.175315980461520304 ) ) ;
#100394 = CARTESIAN_POINT ( 'NONE',  ( 0.6823417656249969321, 15.33854166700806410, -1.181850606188757036 ) ) ;
#100395 = ORIENTED_EDGE ( 'NONE', *, *, #148090, .F. ) ;
#100396 = CARTESIAN_POINT ( 'NONE',  ( -5.152980901645737077, 8.169505597632108262, -1.199719254218453823 ) ) ;
#100397 = CARTESIAN_POINT ( 'NONE',  ( 5.308220328704632784, 1.198845711980157214, -1.621194722098241003 ) ) ;
#100398 = ORIENTED_EDGE ( 'NONE', *, *, #119470, .T. ) ;
#100399 = ADVANCED_FACE ( 'NONE', ( #153463 ), #136154, .T. ) ;
#100400 = CARTESIAN_POINT ( 'NONE',  ( 2.149089010626914931, -1.500894351328721621, -1.116326037436713881 ) ) ;
#100401 = EDGE_CURVE ( 'NONE', #198538, #95302, #90617, .T. ) ;
#100402 = CARTESIAN_POINT ( 'NONE',  ( 2.465759480183654428, -0.4578044685884518072, 2.018832516862689275 ) ) ;
#100403 = CARTESIAN_POINT ( 'NONE',  ( -6.739811759324828344, 8.956476034002674780, -1.443375672974066548 ) ) ;
#100404 = CARTESIAN_POINT ( 'NONE',  ( 2.320441991784210067, -0.7354482596747033973, -1.765520077574176394 ) ) ;
#100405 = CARTESIAN_POINT ( 'NONE',  ( -5.276698331947687670, 7.500886158655696967, 1.250003795154420061 ) ) ;
#100406 = CARTESIAN_POINT ( 'NONE',  ( -10.14895191580505163, 4.000029896383376027, -7.601392964056682189 ) ) ;
#100407 = DIRECTION ( 'NONE',  ( -0.5620411653127326268, -0.8271092603120251407, 0.000000000000000000 ) ) ;
#100408 = CARTESIAN_POINT ( 'NONE',  ( -0.6823417656250212460, 3.863541667008085767, 1.181850606188767472 ) ) ;
#100409 = CARTESIAN_POINT ( 'NONE',  ( 0.5449873876890097835, 0.1430962203496731200, 1.907122450762772425 ) ) ;
#100410 = CARTESIAN_POINT ( 'NONE',  ( 6.400857919427532572, 6.640291458853147866, -0.7216878364870458196 ) ) ;
#100411 = CARTESIAN_POINT ( 'NONE',  ( 2.031626174157370457, 1.878314540015123102, -0.5664888411779643862 ) ) ;
#100412 = CARTESIAN_POINT ( 'NONE',  ( 1.841702881098854272, -0.1987311101661408952, 0.6151380925063543170 ) ) ;
#100413 = CARTESIAN_POINT ( 'NONE',  ( -6.147696309153835692, 6.137010213626392208, 0.7998128361456281477 ) ) ;
#100414 = CARTESIAN_POINT ( 'NONE',  ( 5.326475955075804514, -0.9554483686352827077, -1.893264085526874974 ) ) ;
#100415 = CARTESIAN_POINT ( 'NONE',  ( 8.235688245297327015, 11.69572115523387268, -1.199719254218446718 ) ) ;
#100416 = CARTESIAN_POINT ( 'NONE',  ( 6.837195077073701555, -1.761838062178729070, 0.8845485525767071699 ) ) ;
#100417 = CARTESIAN_POINT ( 'NONE',  ( 1.364683531249988757, 2.384375000341422357, 1.214306433183764966E-14 ) ) ;
#100418 = CARTESIAN_POINT ( 'NONE',  ( 1.670183121039736207, 2.007516039388768991, -0.1524388337148015193 ) ) ;
#100420 = CARTESIAN_POINT ( 'NONE',  ( 0.7029266809492543677, 1.957958796488759035, 0.8061104088524527755 ) ) ;
#100419 = CARTESIAN_POINT ( 'NONE',  ( -7.402388683381436074, 7.738467673474211495, 0.7216878364870317197 ) ) ;
#100421 = CARTESIAN_POINT ( 'NONE',  ( 11.87652835678391128, 6.750173569295289333, -1.734648985301914470 ) ) ;
#100422 = CARTESIAN_POINT ( 'NONE',  ( 2.172408243068229439, -0.9739482337229148357, -1.826950231780352762 ) ) ;
#100423 = CARTESIAN_POINT ( 'NONE',  ( 4.472210567661338843, 6.310941310395290493, 1.599625672291261402 ) ) ;
#100424 = CARTESIAN_POINT ( 'NONE',  ( 5.357406976055401948, 6.279338222599979424, 1.199719254218452935 ) ) ;
#100425 = ORIENTED_EDGE ( 'NONE', *, *, #187534, .F. ) ;
#100427 = CARTESIAN_POINT ( 'NONE',  ( 4.355193658487811703, 6.104145239700998538, -1.599625672291255185 ) ) ;
#100426 = CARTESIAN_POINT ( 'NONE',  ( 5.472635741755179417, -0.05041999219103148605, -2.090201512065153366 ) ) ;
#100430 = EDGE_LOOP ( 'NONE', ( #196941, #25979 ) ) ;
#100429 = CARTESIAN_POINT ( 'NONE',  ( 2.771877521378500742, 1.802570752484193184, -0.1794005705246705940 ) ) ;
#100428 = CARTESIAN_POINT ( 'NONE',  ( 4.243042751400435186, -1.588269943899191183, 0.8999137264355041577 ) ) ;
#100431 = CARTESIAN_POINT ( 'NONE',  ( 9.240045382913317340, 10.73880668727576015, -1.199719254218446718 ) ) ;
#100432 =( NAMED_UNIT ( * ) PLANE_ANGLE_UNIT ( ) SI_UNIT ( $, .RADIAN. ) );
#100433 = CARTESIAN_POINT ( 'NONE',  ( 10.67342974040751180, 8.362853195376180437, 3.128047310392558344 ) ) ;
#100434 = CARTESIAN_POINT ( 'NONE',  ( 5.561621765989873900, 0.4355406452380207738, -2.163202247768724718 ) ) ;
#100436 =( BOUNDED_SURFACE ( )  B_SPLINE_SURFACE ( 3, 2, ( 
 ( #58233, #153607, #70184 ),
 ( #53968, #72325, #5178 ),
 ( #56103, #173066, #122260 ),
 ( #170909, #22504, #24647 ) ),
 .UNSPECIFIED., .F., .F., .F. ) 
 B_SPLINE_SURFACE_WITH_KNOTS ( ( 4, 4 ),
 ( 3, 3 ),
 ( 0.005025772024296196530, 0.008052159968022380709 ),
 ( 0.000000000000000000, 1.000000000000000000 ),
 .UNSPECIFIED. ) 
 GEOMETRIC_REPRESENTATION_ITEM ( )  RATIONAL_B_SPLINE_SURFACE ( (
 ( 1.000000000000000000, 0.7187737999613663664, 1.000000000000000000),
 ( 1.000000000000000000, 0.7186585579881031860, 1.000000000000000000),
 ( 1.000000000000000000, 0.7185467277397551422, 1.000000000000000000),
 ( 1.000000000000000000, 0.7184380228464064544, 1.000000000000000000) ) ) 
 REPRESENTATION_ITEM ( '' )  SURFACE ( )  );
#100435 = CARTESIAN_POINT ( 'NONE',  ( 1.364683531249996529, 11.02604166700807120, 0.7879004041258403923 ) ) ;
#100437 = ORIENTED_EDGE ( 'NONE', *, *, #167257, .T. ) ;
#100438 = CARTESIAN_POINT ( 'NONE',  ( 3.703681524037071071, 1.387051605615218008, 1.316649548728260344 ) ) ;
#100439 = CARTESIAN_POINT ( 'NONE',  ( -2.598358995313378550, 6.183169261174235487, 0.7998128361456341429 ) ) ;
#100440 = CARTESIAN_POINT ( 'NONE',  ( 6.123478934866503742, 10.29580919065294431, 0.7998128361456462443 ) ) ;
#100441 = CARTESIAN_POINT ( 'NONE',  ( 1.360316468749980023, 0.7968750003414099004, -3.122502256758252770E-14 ) ) ;
#100442 = CARTESIAN_POINT ( 'NONE',  ( 4.650083499362867911, 6.448183387388563226, 1.443375672974062551 ) ) ;
#100443 = DIRECTION ( 'NONE',  ( -1.000000000000000000, 0.000000000000000000, 0.000000000000000000 ) ) ;
#100444 = CARTESIAN_POINT ( 'NONE',  ( 7.325202985640204112, 14.51512205016421397, -9.507936040486299589 ) ) ;
#100445 = CARTESIAN_POINT ( 'NONE',  ( -0.09456490281532430042, -0.7861721075429689565, -1.663503389917226460 ) ) ;
#100446 = ORIENTED_EDGE ( 'NONE', *, *, #28580, .F. ) ;
#100447 = CARTESIAN_POINT ( 'NONE',  ( 3.708139779478221598, -0.7553879706188313392, -1.711406342686023541 ) ) ;
#100448 = CARTESIAN_POINT ( 'NONE',  ( 6.373214726875630731, 9.593111727067046957, 1.199719254218452047 ) ) ;
#100449 = CARTESIAN_POINT ( 'NONE',  ( -11.04536101718726293, 13.40000000000000036, -1.100000000000002087 ) ) ;
#100450 = CARTESIAN_POINT ( 'NONE',  ( -5.734735788900501952, 9.634349487118505806, 0.000000000000000000 ) ) ;
#100451 = CARTESIAN_POINT ( 'NONE',  ( 4.473300617505036492, 7.306268922809479704, -1.199719254218452047 ) ) ;
#100452 = CARTESIAN_POINT ( 'NONE',  ( 6.403194803628889709, -1.752124481401344358, 1.102429006916323395 ) ) ;
#100453 = CARTESIAN_POINT ( 'NONE',  ( 1.775017769237042353, 1.753020666602569166, -0.9963212463810557917 ) ) ;
#100454 = CARTESIAN_POINT ( 'NONE',  ( -7.309817376062285099, 11.67987070538135264, 0.000000000000000000 ) ) ;
#100455 = CARTESIAN_POINT ( 'NONE',  ( 6.424584688029230328, 8.588711117491191871, 1.599625672291268286 ) ) ;
#100456 = CARTESIAN_POINT ( 'NONE',  ( 2.941561714372803227, 0.7881326131919093037, -2.044999658057600644 ) ) ;
#100457 = CARTESIAN_POINT ( 'NONE',  ( 6.393173274427864428, 1.585754722747900969, -0.9045919592586546543 ) ) ;
#100458 = CARTESIAN_POINT ( 'NONE',  ( -4.081167932913447594, 4.720116328942494555, -1.199719254218452047 ) ) ;
#100459 = CARTESIAN_POINT ( 'NONE',  ( 1.718115394875207702, -1.600000000000000755, -2.017567716309123682 ) ) ;
#100460 = CARTESIAN_POINT ( 'NONE',  ( 4.990809943606266508, 6.915973915664348937, -1.443375672974068769 ) ) ;
#100462 = EDGE_CURVE ( 'NONE', #41837, #170487, #213314, .T. ) ;
#100461 = CARTESIAN_POINT ( 'NONE',  ( 8.748035429315576650, 11.22912730566677553, -1.599625672291255185 ) ) ;
#100463 = CARTESIAN_POINT ( 'NONE',  ( 4.216749469050096621, 4.878294787768598262, -1.199719254218452047 ) ) ;
#100464 = CARTESIAN_POINT ( 'NONE',  ( 6.373741612200171325, 7.569024981389272710, 1.082531754730549967 ) ) ;
#100465 = ORIENTED_EDGE ( 'NONE', *, *, #97582, .T. ) ;
#100467 = CARTESIAN_POINT ( 'NONE',  ( 0.3463400477153228407, 1.033117966650568986, -1.727632672016335080 ) ) ;
#100466 = CARTESIAN_POINT ( 'NONE',  ( 3.825598141381767903, 0.9817388958630569595, -1.557492293685861284 ) ) ;
#100468 = CARTESIAN_POINT ( 'NONE',  ( 3.497717624726462748, 2.241670729410083940, 0.5068476239948813689 ) ) ;
#100470 = CARTESIAN_POINT ( 'NONE',  ( 0.6548463511123479019, 1.551493821935068906, -1.027296181188163571 ) ) ;
#100469 = CARTESIAN_POINT ( 'NONE',  ( 1.220146605508150803E-14, 9.937500000000000000, -1.499999999999998446 ) ) ;
#100471 = CARTESIAN_POINT ( 'NONE',  ( 1.001543065824772753E-15, -3.871874999522043836, 3.793834371823811669 ) ) ;
#100472 = CARTESIAN_POINT ( 'NONE',  ( -5.066996723205291708, 6.934582148538044777, 1.599625672291267398 ) ) ;
#100473 = CYLINDRICAL_SURFACE ( 'NONE', #105630, 0.04999999999999991257 ) ;
#100474 = CARTESIAN_POINT ( 'NONE',  ( 4.904515063324526025, -1.898637117948184017, -0.2282459111111398431 ) ) ;
#100475 = CARTESIAN_POINT ( 'NONE',  ( -8.616370316684697883, 10.01118577667568132, -1.199719254218446718 ) ) ;
#100476 = CARTESIAN_POINT ( 'NONE',  ( 6.266472554743693912, 6.895788939045927712, 0.7740814723603481884 ) ) ;
#100477 = CARTESIAN_POINT ( 'NONE',  ( -5.966997003790228682, 8.054858819212300958, -1.443375672974066548 ) ) ;
#100479 = CARTESIAN_POINT ( 'NONE',  ( 2.852262661058731386, 0.6285613048715790185, 1.762029509812724992 ) ) ;
#100478 = CARTESIAN_POINT ( 'NONE',  ( 3.632441420962172263, 0.3087965321501208726, 2.067699918487746036 ) ) ;
#100480 = CARTESIAN_POINT ( 'NONE',  ( 6.480434237652121787, 9.543961796360731498, 1.082531754730558626 ) ) ;
#100481 = CARTESIAN_POINT ( 'NONE',  ( -1.364683531249997417, 5.321875000341417916, 1.214306433183764966E-14 ) ) ;
#100482 = CARTESIAN_POINT ( 'NONE',  ( 5.478019777291557979, -1.797689181224306321, -0.3974485807837144224 ) ) ;
#100483 = TOROIDAL_SURFACE ( 'NONE', #155855, 11.92000000000000171, 0.08000000000000000167 ) ;
#100484 = CARTESIAN_POINT ( 'NONE',  ( 2.683624340501134853, 5.218313266304903664, -1.199719254218446718 ) ) ;
#100486 = CARTESIAN_POINT ( 'NONE',  ( 5.678167406024951624, 5.518950149984223508, 0.7998128361456341429 ) ) ;
#100485 = DIRECTION ( 'NONE',  ( 0.6507913734559596097, 0.7592566023653043450, 0.000000000000000000 ) ) ;
#100487 = CARTESIAN_POINT ( 'NONE',  ( 3.668305164303451882, -1.157086425697685828, 1.279375231203205621 ) ) ;
#100488 = CARTESIAN_POINT ( 'NONE',  ( -6.958359152311683893, 9.141171649162195934, -1.599625672291263179 ) ) ;
#100489 = CARTESIAN_POINT ( 'NONE',  ( 0.000000000000000000, 4.518459255872631530, 0.000000000000000000 ) ) ;
#100490 = CARTESIAN_POINT ( 'NONE',  ( 1.436838838544731267, 7.449283400311756509, 4.203727439823562229 ) ) ;
#100491 =( BOUNDED_SURFACE ( )  B_SPLINE_SURFACE ( 3, 2, ( 
 ( #17845, #65534, #62364 ),
 ( #112254, #100190, #128526 ),
 ( #131680, #115444, #146845 ),
 ( #33064, #178267, #95962 ),
 ( #162016, #99142, #165191 ),
 ( #16785, #82868, #148946 ) ),
 .UNSPECIFIED., .F., .F., .T. ) 
 B_SPLINE_SURFACE_WITH_KNOTS ( ( 4, 2, 4 ),
 ( 3, 3 ),
 ( 0.000000000000000000, 0.0003831416164015018179, 0.0007662832328030036357 ),
 ( 0.000000000000000000, 1.000000000000000000 ),
 .UNSPECIFIED. ) 
 GEOMETRIC_REPRESENTATION_ITEM ( )  RATIONAL_B_SPLINE_SURFACE ( (
 ( 1.000000000000000000, 0.7071067811865399122, 1.000000000000000000),
 ( 1.000000000000000000, 0.6829713513653468127, 1.000000000000000000),
 ( 1.000000000000000000, 0.6534833722372194176, 1.000000000000000000),
 ( 1.000000000000000000, 0.6054027484662655167, 1.000000000000000000),
 ( 1.000000000000000000, 0.5875453974414891478, 1.000000000000000000),
 ( 1.000000000000000000, 0.5879095031487528988, 1.000000000000000000) ) ) 
 REPRESENTATION_ITEM ( '' )  SURFACE ( )  );
#100492 = CARTESIAN_POINT ( 'NONE',  ( 3.469446951953614189E-15, 6.180000000000019256, 1.214306433183764966E-14 ) ) ;
#100493 = CARTESIAN_POINT ( 'NONE',  ( 5.032167298026094748, 1.244454833084396306, 1.778855100471810280 ) ) ;
#100494 = CARTESIAN_POINT ( 'NONE',  ( 2.947667120405720986, 0.6567698719579934119, -1.703645827024417914 ) ) ;
#100495 = CARTESIAN_POINT ( 'NONE',  ( 0.2858946156298440844, -1.202361161835348025, -1.550730028719159215 ) ) ;
#100496 = CARTESIAN_POINT ( 'NONE',  ( 5.946512563314596100, -1.495626773323457170, 1.498989405617740189 ) ) ;
#100497 = ORIENTED_EDGE ( 'NONE', *, *, #28211, .T. ) ;
#100499 = CARTESIAN_POINT ( 'NONE',  ( 1.364683531249988535, 2.676041667008082214, 0.7879004041258500513 ) ) ;
#100498 = CARTESIAN_POINT ( 'NONE',  ( 5.794527259016318155, 1.876155144389481721, -1.316939630280162365 ) ) ;
#100500 = CARTESIAN_POINT ( 'NONE',  ( 9.053093885623066939, 11.58502883802551153, -1.599625672291262513 ) ) ;
#100501 = CIRCLE ( 'NONE', #211202, 0.08000000000000020983 ) ;
#100502 = CARTESIAN_POINT ( 'NONE',  ( 1.190261156817543631, 1.266008754425467897, 1.700926646755014593 ) ) ;
#100503 = CARTESIAN_POINT ( 'NONE',  ( -5.422898255786209099, 5.429062174613087599, -0.7216878364870207285 ) ) ;
#100504 = FACE_OUTER_BOUND ( 'NONE', #192814, .T. ) ;
#100505 = CARTESIAN_POINT ( 'NONE',  ( -4.555176424067209240, 8.258196894812975586, 1.040834085586084257E-14 ) ) ;
#100506 = CARTESIAN_POINT ( 'NONE',  ( 6.543812728621629660, 1.490886027097729105, 1.578480410219210928 ) ) ;
#100508 = CARTESIAN_POINT ( 'NONE',  ( 1.500000000000001332, 12.90625000068279604, 0.000000000000000000 ) ) ;
#100507 = CARTESIAN_POINT ( 'NONE',  ( -1.408750476333776369, 7.229967155397921452, 4.273289540530513797 ) ) ;
#100510 = ORIENTED_EDGE ( 'NONE', *, *, #106930, .F. ) ;
#100509 = CARTESIAN_POINT ( 'NONE',  ( 0.8212868038825784645, 1.678483586613238154, -1.455034836404971665 ) ) ;
#100511 = CARTESIAN_POINT ( 'NONE',  ( 6.434220164165640021, -1.621181005584397372, -1.198863592720422977 ) ) ;
#100513 = CARTESIAN_POINT ( 'NONE',  ( 4.135635188098309101, 1.943850041002512352, -0.6901024340064102480 ) ) ;
#100512 = CARTESIAN_POINT ( 'NONE',  ( 3.928111819657337911, 5.605883094398769195, 1.599625672291267398 ) ) ;
#100515 = CARTESIAN_POINT ( 'NONE',  ( -4.299344108864988634, 8.030002203735456590, -0.7216878364870615847 ) ) ;
#100514 = CARTESIAN_POINT ( 'NONE',  ( 4.993145711582793744, 9.047363440147082159, -0.7998128361456481317 ) ) ;
#100516 = CARTESIAN_POINT ( 'NONE',  ( 6.013923656113508542, 9.173938811177871244, -1.199719254218452047 ) ) ;
#100518 = EDGE_CURVE ( 'NONE', #39288, #87431, #55962, .T. ) ;
#100517 = CARTESIAN_POINT ( 'NONE',  ( 1.642778471875000035, -3.813541666188708490, -2.845375778867859751 ) ) ;
#100519 = CARTESIAN_POINT ( 'NONE',  ( 1.217323170181696002, 2.969494316908636300, 0.7750000000000100142 ) ) ;
#100520 = CARTESIAN_POINT ( 'NONE',  ( 1.060620546929908148, -1.890798925694850974, -0.8922787324358200101 ) ) ;
#100521 = CARTESIAN_POINT ( 'NONE',  ( 4.975232503164924935, -2.001511053420693020, -0.2440319332882301961 ) ) ;
#100522 = CARTESIAN_POINT ( 'NONE',  ( 4.968220237687512864, -1.735557695065930606, -0.6152675618510683453 ) ) ;
#100523 = CARTESIAN_POINT ( 'NONE',  ( 4.005544317833563461, 6.760553239859419250, -1.199719254218452047 ) ) ;
#100524 = CARTESIAN_POINT ( 'NONE',  ( 2.168594647197068070, -1.575507694510763335, -0.7022964154167319339 ) ) ;
#100525 = CARTESIAN_POINT ( 'NONE',  ( -0.1882626618336727398, -1.244567986390752390, -1.587255334073833790 ) ) ;
#100526 = CARTESIAN_POINT ( 'NONE',  ( 2.215865853697509102, 2.230823145726851475, 0.5541181435367804609 ) ) ;
#100527 = CARTESIAN_POINT ( 'NONE',  ( -5.225778143063529946, 8.184159369294361497, 1.199719254218452047 ) ) ;
#100528 = CARTESIAN_POINT ( 'NONE',  ( 1.739923964384773258, -1.638176463808267647, -1.560613564838263523 ) ) ;
#100529 = CARTESIAN_POINT ( 'NONE',  ( 3.035867697866540205, -1.414839191968674470, -1.560218430392734446 ) ) ;
#100530 = CARTESIAN_POINT ( 'NONE',  ( -5.309953438407606363, 6.223975762010839574, 1.199719254218452935 ) ) ;
#100532 = EDGE_CURVE ( 'NONE', #45344, #30079, #158004, .T. ) ;
#100531 = CARTESIAN_POINT ( 'NONE',  ( 6.959412922516382771, 7.013736585890911535, 0.7998128361456341429 ) ) ;
#100533 = CARTESIAN_POINT ( 'NONE',  ( 4.543390873910894356, 8.314723429622471684, 0.7216878364870317197 ) ) ;
#100534 = CARTESIAN_POINT ( 'NONE',  ( 5.593750000000004441, -1.895863743164200921, -0.7852924748296893354 ) ) ;
#100535 = CARTESIAN_POINT ( 'NONE',  ( -6.586563698140583512, 6.578745824119123675, 1.040834085586084257E-14 ) ) ;
#100536 = CARTESIAN_POINT ( 'NONE',  ( 0.7499999999999885647, 1.566666666666688412, -1.299038105676652899 ) ) ;
#100537 = CARTESIAN_POINT ( 'NONE',  ( -4.786191920824102830, 5.542644314838231168, 1.199719254218462483 ) ) ;
#100538 = CARTESIAN_POINT ( 'NONE',  ( 4.851916359752673991, -1.571614379473328160, -1.570179378767898370 ) ) ;
#100539 = CARTESIAN_POINT ( 'NONE',  ( 3.521585679250069045, -1.305302140894725627, -1.760141160621036649 ) ) ;
#100540 = CARTESIAN_POINT ( 'NONE',  ( -4.791917227426195858, 7.677988301050826969, -1.199719254218452047 ) ) ;
#100541 = CARTESIAN_POINT ( 'NONE',  ( -5.008811405605897882, 4.808311159487113073, 0.7998128361456281477 ) ) ;
#100542 = AXIS2_PLACEMENT_3D ( 'NONE', #174102, #142673, #43035 ) ;
#100543 = CARTESIAN_POINT ( 'NONE',  ( -0.6823417656250212460, 2.801041667008084879, 1.181850606188767472 ) ) ;
#100544 = CARTESIAN_POINT ( 'NONE',  ( 6.890000000000047642, 2.940278081043229186, 2.731889818495436995 ) ) ;
#100545 = CARTESIAN_POINT ( 'NONE',  ( -5.599154252763867134, 5.634694171087028636, 0.000000000000000000 ) ) ;
#100546 = CARTESIAN_POINT ( 'NONE',  ( 5.168275554957600271, 2.118074532352266282, -0.1063875075708180934 ) ) ;
#100547 = CARTESIAN_POINT ( 'NONE',  ( -6.617788377246193399, 8.814115421577600529, -1.443375672974066548 ) ) ;
#100548 = ORIENTED_EDGE ( 'NONE', *, *, #88421, .T. ) ;
#100550 = CARTESIAN_POINT ( 'NONE',  ( 6.807524309086420367, -0.4794501827766698421, 2.115671360755105646 ) ) ;
#100549 = CARTESIAN_POINT ( 'NONE',  ( -5.858531774880906262, 6.967946837850073294, 1.082531754730549078 ) ) ;
#100551 = CARTESIAN_POINT ( 'NONE',  ( 4.333802657862601215, 8.207853534148366492, 0.7998128361456462443 ) ) ;
#100552 = CARTESIAN_POINT ( 'NONE',  ( 1.284279953904119864, 3.046639714193936754, -0.7749999999999910294 ) ) ;
#100553 = UNCERTAINTY_MEASURE_WITH_UNIT (LENGTH_MEASURE( 1.000000000000000082E-05 ), #108866, 'distance_accuracy_value', 'NONE');
#100554 = DIRECTION ( 'NONE',  ( 0.000000000000000000, -1.000000000000000000, 0.000000000000000000 ) ) ;
#100555 = CARTESIAN_POINT ( 'NONE',  ( -0.6823417656250212460, 2.113541667008083991, 1.181850606188767472 ) ) ;
#100556 = CARTESIAN_POINT ( 'NONE',  ( 1.610509732637079638, -0.2130687159686726062, 1.727248725346673952 ) ) ;
#100557 = CARTESIAN_POINT ( 'NONE',  ( 3.871016551901614200, 4.474939717762034697, -1.199719254218446718 ) ) ;
#100558 = CARTESIAN_POINT ( 'NONE',  ( -10.39230484541323740, 3.447199233515621408, 6.000000000000048850 ) ) ;
#100559 = CARTESIAN_POINT ( 'NONE',  ( 1.364683531249986537, -0.07395833299191513499, 0.7879004041258500513 ) ) ;
#100560 = CARTESIAN_POINT ( 'NONE',  ( -1.510657702057710340E-15, 1.375000000682792267, 1.224999999999963229 ) ) ;
#100561 = CARTESIAN_POINT ( 'NONE',  ( 5.735289742212391850, -1.956171686333206816, 0.9202595734885756773 ) ) ;
#100562 = CARTESIAN_POINT ( 'NONE',  ( -3.327636637150278798, 5.969660945728899826, -1.199719254218452935 ) ) ;
#100563 = EDGE_CURVE ( 'NONE', #89282, #110706, #116604, .T. ) ;
#100564 = CARTESIAN_POINT ( 'NONE',  ( -7.334597914868741242, 8.619747657844088806, -1.082531754730543083 ) ) ;
#100565 = CARTESIAN_POINT ( 'NONE',  ( 5.102478102407745908, -0.7247817745383768884, -2.036717088958202471 ) ) ;
#100566 = CARTESIAN_POINT ( 'NONE',  ( 1.364683531249990311, 3.634375000341416584, 1.214306433183764966E-14 ) ) ;
#100567 = CARTESIAN_POINT ( 'NONE',  ( 5.887953105907347329, -0.8888255776743571035, 1.759709591642463433 ) ) ;
#100568 = CARTESIAN_POINT ( 'NONE',  ( 4.674945122873967129, -0.7415060156777570910, -1.567401138452922060 ) ) ;
#100570 = CARTESIAN_POINT ( 'NONE',  ( 2.015410700679621137, -2.124826835150806392, 0.5361769018528695918 ) ) ;
#100569 = CARTESIAN_POINT ( 'NONE',  ( -4.156403723172807449E-14, -1.046874999658554906, 1.570758158831744078 ) ) ;
#100571 = CARTESIAN_POINT ( 'NONE',  ( 2.520946605012349018, 1.507388781920895759, -1.747272692061818011 ) ) ;
#100572 = CARTESIAN_POINT ( 'NONE',  ( 5.220021542613917376, -1.098816822949649774, -1.743189258048108314 ) ) ;
#100573 = CARTESIAN_POINT ( 'NONE',  ( 0.1287130127310652239, -1.775900012335431155, 0.7861216482863192523 ) ) ;
#100574 = CARTESIAN_POINT ( 'NONE',  ( -6.521108698048779573, 8.631046119188804155, -1.443375672974058777 ) ) ;
#100575 = CARTESIAN_POINT ( 'NONE',  ( -4.573896719763875574, 6.429575154514868274, -1.599625672291271394 ) ) ;
#100576 = CARTESIAN_POINT ( 'NONE',  ( -9.608183788732286956, 15.11835436368665420, 7.189075342704710714 ) ) ;
#100577 = CARTESIAN_POINT ( 'NONE',  ( 3.357788437482766675, -1.608272433257527556, -1.382313803475518244 ) ) ;
#100578 = CARTESIAN_POINT ( 'NONE',  ( 5.113477980681966351, 7.841710745841885100, -1.181108758208327725 ) ) ;
#100579 = CARTESIAN_POINT ( 'NONE',  ( 1.354138928560550292, 0.1455316553338575902, -2.011204400906742240 ) ) ;
#100580 = CARTESIAN_POINT ( 'NONE',  ( -7.673551755210395342, 8.054824590608001600, 1.040834085586084257E-14 ) ) ;
#100581 = CARTESIAN_POINT ( 'NONE',  ( 4.243358471946375943, -1.921622210924242458, 1.084848892642875429 ) ) ;
#100582 = CARTESIAN_POINT ( 'NONE',  ( 3.285556943750000070, -2.821874999522043570, 0.000000000000000000 ) ) ;
#100583 = CARTESIAN_POINT ( 'NONE',  ( 2.096333906143353243, 1.839810448830980105, 0.2789567515945317600 ) ) ;
#100584 = CARTESIAN_POINT ( 'NONE',  ( -0.1290005225502675879, -0.006633637972621592160, -2.173875058097324064 ) ) ;
#100585 = CARTESIAN_POINT ( 'NONE',  ( 3.094265954482833703, 2.800000000000017586, -2.490342512183683965 ) ) ;
#100586 = DIRECTION ( 'NONE',  ( 0.000000000000000000, 0.000000000000000000, 1.000000000000000000 ) ) ;
#100588 = CARTESIAN_POINT ( 'NONE',  ( 6.925078400183553029, 0.5745968962584145912, 2.096956839219825230 ) ) ;
#100587 = CARTESIAN_POINT ( 'NONE',  ( -4.979135478818752958, 8.054126424104152804, -1.119915745145182440 ) ) ;
#100589 = VERTEX_POINT ( 'NONE', #71111 ) ;
#100590 = CARTESIAN_POINT ( 'NONE',  ( 3.063408159219972227, 0.3037436250956357386, -2.038260327603860222 ) ) ;
#100591 = CARTESIAN_POINT ( 'NONE',  ( 1.360316468749957597, 1.265625000341379147, -5.030698080332740574E-14 ) ) ;
#100592 = CARTESIAN_POINT ( 'NONE',  ( -7.054319997812058318, 7.124461507069184130, 1.040834085586084257E-14 ) ) ;
#100593 = CARTESIAN_POINT ( 'NONE',  ( 2.174478703267632707, 0.8655064541149575241, 1.824978016274068082 ) ) ;
#100594 = CARTESIAN_POINT ( 'NONE',  ( 0.7499999999999885647, -1.016666666666644847, 1.299038105676657340 ) ) ;
#100595 = CARTESIAN_POINT ( 'NONE',  ( 4.033714395265605823, 4.664753868353354704, -1.199719254218446718 ) ) ;
#100596 = CARTESIAN_POINT ( 'NONE',  ( 2.342715047087840397, 0.4503528687099351280, 2.010914609654746332 ) ) ;
#100598 = CARTESIAN_POINT ( 'NONE',  ( 0.6823417656249969321, 13.77604166700806232, -1.181850606188757036 ) ) ;
#100597 = CARTESIAN_POINT ( 'NONE',  ( 6.883263157960364254, -0.001323150302089577462, 1.953658984494696549 ) ) ;
#100599 = CARTESIAN_POINT ( 'NONE',  ( 6.328958779480917229, 6.278206752349526631, 0.7998128361456341429 ) ) ;
#100600 = CARTESIAN_POINT ( 'NONE',  ( -0.1411974294641837879, -0.0004739540254219963859, -1.900147702309516795 ) ) ;
#100601 = CARTESIAN_POINT ( 'NONE',  ( 1.341482821134845738, 1.838956754096718882, 0.09199767257135617327 ) ) ;
#100602 = CARTESIAN_POINT ( 'NONE',  ( 5.549527019956425278, -1.737703232767298545, -1.360318885177333570 ) ) ;
#100603 = CARTESIAN_POINT ( 'NONE',  ( 6.225128807330042591, 7.291680359087043151, -1.199719254218452047 ) ) ;
#100604 = CARTESIAN_POINT ( 'NONE',  ( 1.810078809455554438, -2.145489296895970011, 0.2626290421628638128 ) ) ;
#100605 = CARTESIAN_POINT ( 'NONE',  ( -4.528060117284246289, 6.305822774963486310, 1.443375672974064550 ) ) ;
#100606 = CARTESIAN_POINT ( 'NONE',  ( 2.079314900164643820, 1.561883299538204151, 1.275554356156020308 ) ) ;
#100607 = CARTESIAN_POINT ( 'NONE',  ( -1.734723475976807094E-15, -6.134628647623513231, -10.91970695577494332 ) ) ;
#100608 = CARTESIAN_POINT ( 'NONE',  ( -0.4768485052293973125, 6.608576083985783001, 3.444768111981479031 ) ) ;
#100609 = CARTESIAN_POINT ( 'NONE',  ( 1.890105089649192216, 8.991484090553308661, -0.7749999999999996891 ) ) ;
#100610 = CARTESIAN_POINT ( 'NONE',  ( 4.258636414635104117, -1.461677231104720143, 1.323132448414195528 ) ) ;
#100611 = CARTESIAN_POINT ( 'NONE',  ( 3.397672961473942266, -1.985868886743065609, 0.3494831190506141883 ) ) ;
#100613 = CARTESIAN_POINT ( 'NONE',  ( 8.378575743120986630, 12.71882943370911789, 1.040834085586084257E-14 ) ) ;
#100612 = CARTESIAN_POINT ( 'NONE',  ( -1.364683531250012516, 2.030208333674750953, 0.7879004041258379498 ) ) ;
#100615 = CARTESIAN_POINT ( 'NONE',  ( 6.621705515693503408, -2.043321748007483674, 0.5098342655636013410 ) ) ;
#100614 = CARTESIAN_POINT ( 'NONE',  ( -6.958359152311683893, 9.141171649162195934, -1.599625672291263179 ) ) ;
#100616 = B_SPLINE_CURVE_WITH_KNOTS ( 'NONE', 3,
 ( #67365, #148662, #46911, #97793 ),
 .UNSPECIFIED., .F., .F.,
 ( 4, 4 ),
 ( 0.000000000000000000, 8.505390838612159954E-05 ),
 .UNSPECIFIED. ) ;
#100617 = CARTESIAN_POINT ( 'NONE',  ( 5.916483165358986440, 0.8355632440216669288, 1.894440869009452300 ) ) ;
#100618 = CARTESIAN_POINT ( 'NONE',  ( 7.145310649601935182, 8.294949498412453437, -1.199719254218446718 ) ) ;
#100619 = CARTESIAN_POINT ( 'NONE',  ( -5.716734326456539783, 9.821273814174633188, -0.7998128361456231517 ) ) ;
#100620 = CARTESIAN_POINT ( 'NONE',  ( -1.566031286093755304, 8.750666943143144749, 2.469538363634797840 ) ) ;
#100621 = CARTESIAN_POINT ( 'NONE',  ( 4.711197416960428264, 1.676919581237258372, -1.125501318796730876 ) ) ;
#100622 = CARTESIAN_POINT ( 'NONE',  ( 1.499999999999987566, -0.9437499993171851731, 0.000000000000000000 ) ) ;
#100623 = CARTESIAN_POINT ( 'NONE',  ( 0.4970291366834606039, 0.3490122959711927098, 2.032667101136710563 ) ) ;
#100624 = CARTESIAN_POINT ( 'NONE',  ( 9.408995418203975447, 10.07950886410055524, 0.7216878364870438212 ) ) ;
#100625 = CARTESIAN_POINT ( 'NONE',  ( 7.517069824134078537, 7.734612647770044092, 0.000000000000000000 ) ) ;
#100626 = CARTESIAN_POINT ( 'NONE',  ( 5.899733120602060232, 6.912052057904395141, -1.199719254218452047 ) ) ;
#100627 = CARTESIAN_POINT ( 'NONE',  ( 1.364683531249986537, 0.6760416670080884316, 0.7879004041258500513 ) ) ;
#100628 = CARTESIAN_POINT ( 'NONE',  ( 5.041653019435334393, 6.975290837464928728, -1.599625672291269396 ) ) ;
#100629 = CARTESIAN_POINT ( 'NONE',  ( 7.144783764277405247, 8.398297815487545392, -1.082531754730543971 ) ) ;
#100631 = DIRECTION ( 'NONE',  ( 0.000000000000000000, 0.000000000000000000, 1.000000000000000000 ) ) ;
#100630 = CARTESIAN_POINT ( 'NONE',  ( 2.787735123443566110, -2.026669663610313865, 0.7793237752812106622 ) ) ;
#100632 = CARTESIAN_POINT ( 'NONE',  ( 6.626263010475290649, 1.250585457657760635, -1.762915812992614129 ) ) ;
#100634 = CARTESIAN_POINT ( 'NONE',  ( 3.263068207883256466, 1.795673413606920565, -0.4063787724192802209 ) ) ;
#100633 = CARTESIAN_POINT ( 'NONE',  ( -5.422898255786203769, 6.389431388914436738, -1.082531754730544860 ) ) ;
#100635 = CARTESIAN_POINT ( 'NONE',  ( 0.6823417656249917140, 4.342708333674755394, 1.181850606188765695 ) ) ;
#100636 = CARTESIAN_POINT ( 'NONE',  ( 4.634432875810733599, 0.3748786239917039631, 2.159109584303263940 ) ) ;
#100637 = CARTESIAN_POINT ( 'NONE',  ( 6.928203230280114866, 14.53133650447934144, 9.797958971139216544 ) ) ;
#100638 = CARTESIAN_POINT ( 'NONE',  ( 5.084992976345711568, -0.2718087151927280343, -2.246069130642995404 ) ) ;
#100639 = CARTESIAN_POINT ( 'NONE',  ( -5.392392409933270514, 7.314210449720692786, 1.599625672291269396 ) ) ;
#100640 = CARTESIAN_POINT ( 'NONE',  ( -5.470032677541931676, 6.438256155886466381, -1.298486150373518999 ) ) ;
#100641 = CARTESIAN_POINT ( 'NONE',  ( 4.613585901703492809, 8.466914752176691650, -0.2784627230535564046 ) ) ;
#100642 =( GEOMETRIC_REPRESENTATION_CONTEXT ( 3 ) GLOBAL_UNCERTAINTY_ASSIGNED_CONTEXT ( ( #91843 ) ) GLOBAL_UNIT_ASSIGNED_CONTEXT ( ( #145996, #98288, #97235 ) ) REPRESENTATION_CONTEXT ( 'NONE', 'WORKASPACE' ) );
#100643 = CARTESIAN_POINT ( 'NONE',  ( -4.611181641979265500, 8.393812659035525314, 0.000000000000000000 ) ) ;
#100644 = CARTESIAN_POINT ( 'NONE',  ( 4.367134877377630175, 7.148722219365612141, -1.082531754730548412 ) ) ;
#100645 = CARTESIAN_POINT ( 'NONE',  ( 6.925078400183545035, 0.003529629153843985134, 1.755452343125718073 ) ) ;
#100646 = CARTESIAN_POINT ( 'NONE',  ( 4.108068219531130438, -0.7683648849950328596, 1.860876229713221086 ) ) ;
#100647 = CARTESIAN_POINT ( 'NONE',  ( 6.877010230629674759, 9.046264573866535486, 1.599625672291281386 ) ) ;
#100648 = CARTESIAN_POINT ( 'NONE',  ( 3.540152450731326450, 0.9484212380423739930, -1.880392733946538719 ) ) ;
#100649 = CARTESIAN_POINT ( 'NONE',  ( 1.476048981871850518, -1.906537803873010084, -0.1858940877890648546 ) ) ;
#100651 = CARTESIAN_POINT ( 'NONE',  ( 1.499999999999989120, 2.754166666666688190, 0.8660254037844524744 ) ) ;
#100650 = CARTESIAN_POINT ( 'NONE',  ( -0.6823417656250039265, 12.56770833367473017, -1.181850606188755259 ) ) ;
#100652 = CARTESIAN_POINT ( 'NONE',  ( 1.539439451811152493, 1.821048954109681706, -0.7507764504887379786 ) ) ;
#100653 = CARTESIAN_POINT ( 'NONE',  ( 0.1978467685152424937, -1.870139902624564865, -0.05068021481659244765 ) ) ;
#100654 = CARTESIAN_POINT ( 'NONE',  ( 0.8890225878602634468, 0.1407106197201784259, 1.956863499422318631 ) ) ;
#100656 = ORIENTED_EDGE ( 'NONE', *, *, #48997, .T. ) ;
#100655 = CARTESIAN_POINT ( 'NONE',  ( 6.469024005207689498, -1.393930998056407189, 1.156871781951673395 ) ) ;
#100657 = CARTESIAN_POINT ( 'NONE',  ( 4.853455804012216213, 6.685451076146141425, 1.443375672974062551 ) ) ;
#100659 = EDGE_CURVE ( 'NONE', #121123, #119038, #161558, .T. ) ;
#100658 = VECTOR ( 'NONE', #87099, 1000.000000000000000 ) ;
#100660 = CARTESIAN_POINT ( 'NONE',  ( 1.364683531249986537, 0.9260416670080896528, 0.7879004041258500513 ) ) ;
#100661 = CARTESIAN_POINT ( 'NONE',  ( 5.700035372616791385, -1.870836310086241294, 0.001406584917262864625 ) ) ;
#100662 = CARTESIAN_POINT ( 'NONE',  ( 5.577033793921920335, 1.910671465402475677, 0.7975372692515870776 ) ) ;
#100663 = CARTESIAN_POINT ( 'NONE',  ( -4.136646265500964148, 6.879818838842817641, -1.082531754730551743 ) ) ;
#100664 = CARTESIAN_POINT ( 'NONE',  ( 2.494940289813108780, 3.447199233515649386, -11.73777120880564695 ) ) ;
#100665 = CARTESIAN_POINT ( 'NONE',  ( -1.201851678989727383E-14, 0.9625000000000237810, 1.732050807568877637 ) ) ;
#100666 = CARTESIAN_POINT ( 'NONE',  ( 5.601490020740366838, 9.686822124172440596, 1.040834085586084257E-14 ) ) ;
#100667 = CARTESIAN_POINT ( 'NONE',  ( -7.985916173649233230, 9.275655943134292869, -1.199719254218446718 ) ) ;
#100668 = CARTESIAN_POINT ( 'NONE',  ( 6.261886844665240481, 8.398896966899865646, 1.599625672291268286 ) ) ;
#100669 = CARTESIAN_POINT ( 'NONE',  ( -1.402160292154681736E-14, 0.6968750003414164729, -1.575800808251659024 ) ) ;
#100670 = CARTESIAN_POINT ( 'NONE',  ( -1.402160292154681736E-14, 2.087500000000021227, -1.732050807568863648 ) ) ;
#100672 = CARTESIAN_POINT ( 'NONE',  ( 5.020596955762157698, 4.751784624677624080, 1.040834085586084257E-14 ) ) ;
#100671 = CARTESIAN_POINT ( 'NONE',  ( 6.162552467866693640, -0.7048080804108979303, -1.831077584432870609 ) ) ;
#100673 = CARTESIAN_POINT ( 'NONE',  ( 2.811874868751465417, -1.677748492350576770, 1.117661080827489606 ) ) ;
#100674 = CARTESIAN_POINT ( 'NONE',  ( 3.538217205509861962, 0.6946294275822698649, 1.785521036047182486 ) ) ;
#100675 = EDGE_CURVE ( 'NONE', #24517, #3126, #96001, .T. ) ;
#100676 = DIRECTION ( 'NONE',  ( 0.000000000000000000, -1.000000000000000000, 0.000000000000000000 ) ) ;
#100677 = CARTESIAN_POINT ( 'NONE',  ( 1.523247060345904291, -2.062048068855956373, 0.7425582295156887280 ) ) ;
#100678 = CARTESIAN_POINT ( 'NONE',  ( 0.2333690889706682703, 0.003390530909083006028, -2.053566628440507635 ) ) ;
#100679 = CARTESIAN_POINT ( 'NONE',  ( 2.811613793402362393, -1.850737340378521223, 0.2705540153197931730 ) ) ;
#100680 = CARTESIAN_POINT ( 'NONE',  ( 1.499999999999987121, -1.214583332650518432, 0.8660254037844524744 ) ) ;
#100681 = CARTESIAN_POINT ( 'NONE',  ( 4.640889591357927557, 1.927823495868080439, 0.5801764560204000221 ) ) ;
#100682 = CARTESIAN_POINT ( 'NONE',  ( -7.857113714319432063, 9.125386407249497012, 1.199719254218462483 ) ) ;
#100684 = CARTESIAN_POINT ( 'NONE',  ( 4.060252369235962888, -1.217431538915053180, 1.732033588162092297 ) ) ;
#100683 = CARTESIAN_POINT ( 'NONE',  ( -5.612712406377534435, 5.650512016969639895, 0.7216878364870317197 ) ) ;
#100685 = FACE_OUTER_BOUND ( 'NONE', #69470, .T. ) ;
#100686 = CARTESIAN_POINT ( 'NONE',  ( 5.986797818411375260, 1.994257276370488219, 0.5558945855626205024 ) ) ;
#100688 = CARTESIAN_POINT ( 'NONE',  ( -5.753162853856577108, 6.626890507991352486, -1.008109661457639694 ) ) ;
#100687 = CARTESIAN_POINT ( 'NONE',  ( 2.314113491060950434, 1.363558105167931966, -1.585015408884550503 ) ) ;
#100690 = ORIENTED_EDGE ( 'NONE', *, *, #174144, .T. ) ;
#100689 = CARTESIAN_POINT ( 'NONE',  ( 1.096240241049123210, -0.4132495022837120446, -1.674402075930980338 ) ) ;
#100691 = CARTESIAN_POINT ( 'NONE',  ( 7.800018446563675489, 7.994443030612759848, -0.7998128361456281477 ) ) ;
#100692 = DIRECTION ( 'NONE',  ( 5.578564026256490882E-16, 1.000000000000000000, 9.066213480720158442E-32 ) ) ;
#100693 = CARTESIAN_POINT ( 'NONE',  ( 0.1333692844072559280, 0.001398348041498076455, -2.053671342968105051 ) ) ;
#100694 = PRESENTATION_STYLE_ASSIGNMENT (( #85510 ) ) ;
#100695 = CARTESIAN_POINT ( 'NONE',  ( 5.761852095683461350, 9.665985178365305686, -0.7216878364870267237 ) ) ;
#100696 = CARTESIAN_POINT ( 'NONE',  ( 8.966533317356120136, 1.405705671057797090, 7.975201661134141418 ) ) ;
#100697 = AXIS2_PLACEMENT_3D ( 'NONE', #63526, #177280, #14752 ) ;
#100699 = CARTESIAN_POINT ( 'NONE',  ( 0.1877650794145177826, 1.041282258498995361, 1.482055844031314518 ) ) ;
#100698 = CARTESIAN_POINT ( 'NONE',  ( 5.643937085038755797, 9.806620042512378177, -0.7998128361456481317 ) ) ;
#100700 = CARTESIAN_POINT ( 'NONE',  ( -7.477485413136760073, 8.682486722536401302, -1.199719254218446718 ) ) ;
#100701 = COLOUR_RGB ( '', 0.09019608, 0.27058824, 0.51372549) ;
#100702 = CARTESIAN_POINT ( 'NONE',  ( 4.273844736805816780, 6.009238164405336313, 1.599625672291267398 ) ) ;
#100703 = CARTESIAN_POINT ( 'NONE',  ( -5.710744021720588925, 7.310394840978843511, 1.216594670743395445 ) ) ;
#100704 = CARTESIAN_POINT ( 'NONE',  ( 6.363572996767764778, 8.517530811019446091, -1.599625672291283607 ) ) ;
#100705 = SURFACE_STYLE_FILL_AREA ( #129043 ) ;
#100706 = CARTESIAN_POINT ( 'NONE',  ( 3.994299746785815231, 7.604083813490793098, 0.004591788735710394809 ) ) ;
#100707 = CARTESIAN_POINT ( 'NONE',  ( 8.581948047770334043, 12.95609712246668899, 0.000000000000000000 ) ) ;
#100708 = ORIENTED_EDGE ( 'NONE', *, *, #91462, .T. ) ;
#100709 = ORIENTED_EDGE ( 'NONE', *, *, #50038, .F. ) ;
#100710 = CARTESIAN_POINT ( 'NONE',  ( 2.541259301162884121, 1.702954558545258346, -0.7510573925902948034 ) ) ;
#100711 = CARTESIAN_POINT ( 'NONE',  ( 0.3861688966736884776, -0.6463253627202453222, -1.803393044390422029 ) ) ;
#100712 = CARTESIAN_POINT ( 'NONE',  ( 0.2938078718510480081, 1.976988316466289142, -0.7672523047414223640 ) ) ;
#100713 = CARTESIAN_POINT ( 'NONE',  ( 2.274126960250456797, 5.663124471396743687, 0.4971758506561237412 ) ) ;
#100714 = CARTESIAN_POINT ( 'NONE',  ( -1.530509776559454860, 8.694755902745800569, -2.517145264428154672 ) ) ;
#100715 = CARTESIAN_POINT ( 'NONE',  ( -4.446711195602255806, 5.250546485366484717, -1.082531754730544860 ) ) ;
#100716 = CARTESIAN_POINT ( 'NONE',  ( 8.758204044747998296, 11.24099069033793974, 1.443375672974076540 ) ) ;
#100717 = CARTESIAN_POINT ( 'NONE',  ( 4.803538196489102852, -1.519661447750167982, -1.252675939642827529 ) ) ;
#100718 = CARTESIAN_POINT ( 'NONE',  ( 1.717596852896427606, 1.764750374324057347, 1.175337852406685535 ) ) ;
#100719 = CARTESIAN_POINT ( 'NONE',  ( -6.240830780992103755, 6.175390754112560110, 1.040834085586084257E-14 ) ) ;
#100720 = CARTESIAN_POINT ( 'NONE',  ( -11.13119402894544763, 7.260262539292284600, -4.367170956698847029 ) ) ;
#100721 = CARTESIAN_POINT ( 'NONE',  ( 0.000000000000000000, 0.02011834319527033843, -6.938893903907228378E-15 ) ) ;
#100722 = CARTESIAN_POINT ( 'NONE',  ( 6.070311387754347088, -2.079788119406985825, -0.6908379657195938828 ) ) ;
#100723 = SPHERICAL_SURFACE ( 'NONE', #12156, 0.08000000000000000167 ) ;
#100724 = CARTESIAN_POINT ( 'NONE',  ( 3.856402372034730686, 0.6923319331257683507, 1.797858303039111982 ) ) ;
#100725 = CARTESIAN_POINT ( 'NONE',  ( -8.290974629956718189, 9.631557475493025322, -1.199719254218446718 ) ) ;
#100726 = CARTESIAN_POINT ( 'NONE',  ( 0.6217474354073999621, -0.9722136304874777757, -1.544982199245432897 ) ) ;
#100727 = CARTESIAN_POINT ( 'NONE',  ( 0.4873205249028254027, -0.2742316277877173691, -2.189713876267186166 ) ) ;
#100728 = CARTESIAN_POINT ( 'NONE',  ( -0.5028141819148801428, 7.728236690828136801, 1.993924427468481309 ) ) ;
#100729 = ORIENTED_EDGE ( 'NONE', *, *, #28619, .T. ) ;
#100730 = EDGE_LOOP ( 'NONE', ( #46718, #104722, #200049, #162968 ) ) ;
#100731 = CARTESIAN_POINT ( 'NONE',  ( 6.684429667774410611, 1.136775344189003611, -1.608021923639752604 ) ) ;
#100732 = CARTESIAN_POINT ( 'NONE',  ( 0.6615421549095920062, 0.9584981283930308349, 1.688995467024148045 ) ) ;
#100733 = CARTESIAN_POINT ( 'NONE',  ( 6.679114621301890153, -1.074570768553984479, -2.031732957927368410 ) ) ;
#100735 = CARTESIAN_POINT ( 'NONE',  ( 4.592532296707762640, 1.824399381888962779, 0.3660411688805977337 ) ) ;
#100734 = CARTESIAN_POINT ( 'NONE',  ( -5.121948170912633991, 9.197632976031879792, -0.7998128361456362523 ) ) ;
#100736 = CARTESIAN_POINT ( 'NONE',  ( 5.742760583840166966, 8.857581893525663830, 1.199719254218452047 ) ) ;
#100737 = DIRECTION ( 'NONE',  ( 0.9998476951563912696, 0.000000000000000000, -0.01745240643728004568 ) ) ;
#100738 = CARTESIAN_POINT ( 'NONE',  ( -5.392392409933270514, 7.314210449720692786, 1.599625672291269396 ) ) ;
#100739 = CARTESIAN_POINT ( 'NONE',  ( -5.004368097219957789, 5.011053332944274352, 0.000000000000000000 ) ) ;
#100740 = CARTESIAN_POINT ( 'NONE',  ( 0.01162390915069450026, -2.148011843722149372, 0.4338911918742721641 ) ) ;
#100741 = CARTESIAN_POINT ( 'NONE',  ( 4.473827502829567315, 7.202920605734387749, -1.082531754730548412 ) ) ;
#100742 = CARTESIAN_POINT ( 'NONE',  ( 6.471393748265540147, 5.229711127717882491, 2.500000000000011102 ) ) ;
#100743 = DIRECTION ( 'NONE',  ( -1.000000000000000000, 0.000000000000000000, 1.478457507935137263E-17 ) ) ;
#100744 = CARTESIAN_POINT ( 'NONE',  ( 1.049113529465800054, -1.437755431736492673, -1.125068434497819680 ) ) ;
#100745 = CARTESIAN_POINT ( 'NONE',  ( -4.946027110887008860, 4.664786472323266153, -0.7998128361456221525 ) ) ;
#100746 = CARTESIAN_POINT ( 'NONE',  ( 3.287501071874948000, 1.364548152031169082, -1.070007228145404943 ) ) ;
#100747 = CARTESIAN_POINT ( 'NONE',  ( 11.33772463945036790, 10.90000000000000036, -3.600000000000002309 ) ) ;
#100748 = CARTESIAN_POINT ( 'NONE',  ( -6.138157471807708987, 5.995865026538652387, 1.148737437293850421E-12 ) ) ;
#100749 = CARTESIAN_POINT ( 'NONE',  ( 4.355419887332007356, 3.138961360799480627, -0.7749999999999935829 ) ) ;
#100750 = CARTESIAN_POINT ( 'NONE',  ( 6.656878040733529289, -1.407521694628325770, 1.162499734694094844 ) ) ;
#100751 = CARTESIAN_POINT ( 'NONE',  ( 4.592600981049492326, 1.923087700504518605, 0.3867253955378775476 ) ) ;
#100752 = CARTESIAN_POINT ( 'NONE',  ( -8.538937818508475885, 8.856515631215026829, 1.040834085586084257E-14 ) ) ;
#100753 = CARTESIAN_POINT ( 'NONE',  ( 6.823831386379729302, 6.855558127064808716, -0.7998128361456281477 ) ) ;
#100754 = CARTESIAN_POINT ( 'NONE',  ( 5.233110275169113201, 1.959380141031796585, 0.8112103084707968925 ) ) ;
#100755 = CARTESIAN_POINT ( 'NONE',  ( 5.993586425693011144, 9.150212042353954800, -1.199719254218452047 ) ) ;
#100756 = CARTESIAN_POINT ( 'NONE',  ( -10.14557902172788495, 10.73093036830436553, 1.040834085586084257E-14 ) ) ;
#100757 = AXIS2_PLACEMENT_3D ( 'NONE', #198374, #54285, #52148 ) ;
#100758 = CARTESIAN_POINT ( 'NONE',  ( 4.904298879841284098, 6.744767997946720328, 1.599625672291267175 ) ) ;
#100759 = CARTESIAN_POINT ( 'NONE',  ( 3.063400401570901543, 1.746483293306470674, 1.111379191485066364 ) ) ;
#100760 = CARTESIAN_POINT ( 'NONE',  ( -0.6823417656250246877, 0.3635416670080895973, 1.181850606188755259 ) ) ;
#100761 = VERTEX_POINT ( 'NONE', #77538 ) ;
#100762 = CARTESIAN_POINT ( 'NONE',  ( 3.287964078406432566, 1.811126957681759908, -1.415446460160358688 ) ) ;
#100763 = CARTESIAN_POINT ( 'NONE',  ( 7.443063144222396232, 11.62739806832741785, 1.040834085586084257E-14 ) ) ;
#100765 = CARTESIAN_POINT ( 'NONE',  ( -3.285556943749998737, -2.530208332855374831, 1.896917185911908499 ) ) ;
#100764 = CARTESIAN_POINT ( 'NONE',  ( 7.512626515748109135, 8.897724035528543851, 1.082531754730549967 ) ) ;
#100766 = CARTESIAN_POINT ( 'NONE',  ( 0.08888683327021307257, 6.492044364012829583, -3.106763327641859362 ) ) ;
#100767 = DIRECTION ( 'NONE',  ( -0.000000000000000000, -1.000000000000000000, -0.000000000000000000 ) ) ;
#100768 = ORIENTED_EDGE ( 'NONE', *, *, #108161, .T. ) ;
#100769 = CARTESIAN_POINT ( 'NONE',  ( 0.000000000000000000, 13.49999999999999822, 0.000000000000000000 ) ) ;
#100770 = CARTESIAN_POINT ( 'NONE',  ( 4.236511230858605259, 1.172298487584079396, -1.510895503047122945 ) ) ;
#100771 = DIRECTION ( 'NONE',  ( -0.000000000000000000, -1.000000000000000000, -0.000000000000000000 ) ) ;
#100772 = CARTESIAN_POINT ( 'NONE',  ( 5.508750344372229435, 1.303470515519134842, -1.129639352617429537 ) ) ;
#100773 = CARTESIAN_POINT ( 'NONE',  ( 3.169157936054858293, 1.820986098869777470, -0.8666075021629695563 ) ) ;
#100774 = CARTESIAN_POINT ( 'NONE',  ( 4.658965222740456547, 1.322560505849355694, 1.879950767321969529 ) ) ;
#100775 = CARTESIAN_POINT ( 'NONE',  ( 0.000000000000000000, 7.999999999999992895, 0.000000000000000000 ) ) ;
#100776 = CARTESIAN_POINT ( 'NONE',  ( 1.067327838873022516, -1.996528553209110379, -0.9406146916221403975 ) ) ;
#100777 = CARTESIAN_POINT ( 'NONE',  ( -4.828112100242283766, 7.686528979374367410, -1.082531754730549967 ) ) ;
#100778 = CARTESIAN_POINT ( 'NONE',  ( 5.378098658424382172, -0.9825891054615911724, 1.471664417823245197 ) ) ;
#100779 = EDGE_CURVE ( 'NONE', #58688, #80644, #85602, .T. ) ;
#100781 = CARTESIAN_POINT ( 'NONE',  ( 1.482826411003408840, -0.3401602582979300626, -2.266773921731002339 ) ) ;
#100780 = CARTESIAN_POINT ( 'NONE',  ( 5.956828388357757298, 8.042995434541133193, 1.599625672291269396 ) ) ;
#100782 = CARTESIAN_POINT ( 'NONE',  ( 6.650350966976619205, -1.419654684173769166, 1.172063944840713523 ) ) ;
#100783 = CARTESIAN_POINT ( 'NONE',  ( -5.935437387732586778, 10.14670372898850381, -0.7998128361456362523 ) ) ;
#100784 = CARTESIAN_POINT ( 'NONE',  ( -1.154700538379266339, -2.500000000000002220, 2.602085213965210642E-15 ) ) ;
#100785 = CARTESIAN_POINT ( 'NONE',  ( -4.842197138736131556, 5.678260079060780008, 1.199719254218452935 ) ) ;
#100786 = CARTESIAN_POINT ( 'NONE',  ( -1.360316468750002894, -0.3072916663252554526, 0.7853790794158901356 ) ) ;
#100787 = DIRECTION ( 'NONE',  ( 1.000000000000000000, 0.000000000000000000, 0.000000000000000000 ) ) ;
#100788 = CARTESIAN_POINT ( 'NONE',  ( 0.4851436980863755299, 2.077851564382672933, 0.6296362999115376891 ) ) ;
#100789 = CARTESIAN_POINT ( 'NONE',  ( 1.253139057289072822, 0.1435168058863903473, -2.011451928166609893 ) ) ;
#100790 = CARTESIAN_POINT ( 'NONE',  ( 1.499999999999987121, 0.8270833340161471980, -0.8660254037844253849 ) ) ;
#100791 = CARTESIAN_POINT ( 'NONE',  ( 5.074797080785846681, -1.814676937445957039, -0.6471642872378483569 ) ) ;
#100792 = CARTESIAN_POINT ( 'NONE',  ( 1.364683531249997417, 11.73437500034139802, 2.602085213965210642E-15 ) ) ;
#100793 = CARTESIAN_POINT ( 'NONE',  ( 2.320824347369263574, -0.8547976213506520704, -2.050556073580122707 ) ) ;
#100794 = ORIENTED_EDGE ( 'NONE', *, *, #166654, .F. ) ;
#100796 = DIRECTION ( 'NONE',  ( -1.000000000000000000, 0.000000000000000000, -5.551115123125765446E-17 ) ) ;
#100795 = FACE_OUTER_BOUND ( 'NONE', #200379, .T. ) ;
#100797 = CARTESIAN_POINT ( 'NONE',  ( -0.3898781600097490641, 2.718687676624831351, -1.963392457971794514 ) ) ;
#100798 = CARTESIAN_POINT ( 'NONE',  ( 8.727698198895078363, 11.20540053684285553, -1.599625672291257406 ) ) ;
#100799 = CARTESIAN_POINT ( 'NONE',  ( 1.499999999999990896, 5.306250000682820378, 1.214306433183764966E-14 ) ) ;
#100800 = CARTESIAN_POINT ( 'NONE',  ( 4.739680933654325301, 1.736262504677583474, 0.1214163294094624396 ) ) ;
#100802 = CARTESIAN_POINT ( 'NONE',  ( 2.892962425504439050, 0.2373818416543191645, 1.947367909387688112 ) ) ;
#100801 = AXIS2_PLACEMENT_3D ( 'NONE', #126387, #205399, #40805 ) ;
#100804 = CARTESIAN_POINT ( 'NONE',  ( -7.700668062882078502, 9.046829497192987901, -1.082531754730543971 ) ) ;
#100803 = CARTESIAN_POINT ( 'NONE',  ( 4.578903193113299963, 6.365139696764064325, 1.599625672291267398 ) ) ;
#100805 =( NAMED_UNIT ( * ) PLANE_ANGLE_UNIT ( ) SI_UNIT ( $, .RADIAN. ) );
#100806 = CARTESIAN_POINT ( 'NONE',  ( 9.622536337397022521, 12.24937836509514710, 1.599625672291281386 ) ) ;
#100807 = CARTESIAN_POINT ( 'NONE',  ( 0.5024796060203519099, 2.057031790779086045, 0.1535979213492833784 ) ) ;
#100808 = CARTESIAN_POINT ( 'NONE',  ( -7.640183256500752584, 8.872300873127729304, -1.199719254218446718 ) ) ;
#100809 = EDGE_CURVE ( 'NONE', #194999, #175582, #111182, .T. ) ;
#100810 = CARTESIAN_POINT ( 'NONE',  ( -3.429849674132948500, 5.024577257953626308, -1.443375672974051449 ) ) ;
#100811 = CARTESIAN_POINT ( 'NONE',  ( 1.411376899827078368, 1.996129479730743617, 1.065132602888875457 ) ) ;
#100812 = ORIENTED_EDGE ( 'NONE', *, *, #2389, .T. ) ;
#100813 = CARTESIAN_POINT ( 'NONE',  ( 1.499999999999985123, -0.1729166659838496101, -0.8660254037844323793 ) ) ;
#100814 = CARTESIAN_POINT ( 'NONE',  ( 2.565516880305099612, 1.835255434019352094, -0.3607447438512822457 ) ) ;
#100815 = CARTESIAN_POINT ( 'NONE',  ( 1.230678901735713593, 1.732143722507371475, 0.08558704247295551015 ) ) ;
#100816 = CARTESIAN_POINT ( 'NONE',  ( 5.425378541715013547, -1.389685604419872655, -1.694579525865948844 ) ) ;
#100817 = CARTESIAN_POINT ( 'NONE',  ( 5.702268328713489431, -2.307758713666784534, -0.007378162171353326235 ) ) ;
#100818 = CARTESIAN_POINT ( 'NONE',  ( 0.9540633210794751129, 2.058568143186993105, -0.1002533246910724124 ) ) ;
#100819 = CARTESIAN_POINT ( 'NONE',  ( 3.187375889530741802, -0.7864489302777454283, 1.775747734548535961 ) ) ;
#100820 = CARTESIAN_POINT ( 'NONE',  ( -4.080641047588907888, 6.744203074620265248, -1.082531754730548412 ) ) ;
#100821 = CARTESIAN_POINT ( 'NONE',  ( 5.993391575003323091, 1.416176893967495687, 1.222094818194748189 ) ) ;
#100822 = CARTESIAN_POINT ( 'NONE',  ( 0.8750000000000005551, 2.052068128417951609, -5.168192407616667353E-14 ) ) ;
#100823 = CARTESIAN_POINT ( 'NONE',  ( 4.019038269249470829, 7.568960612331900428, -0.3200009682147019752 ) ) ;
#100824 = CARTESIAN_POINT ( 'NONE',  ( 0.4558326304775248139, 1.278721518017480685, 1.171137906463788347 ) ) ;
#100825 = CARTESIAN_POINT ( 'NONE',  ( 5.248414862265931902, 5.295774558831261913, 0.000000000000000000 ) ) ;
#100826 = CARTESIAN_POINT ( 'NONE',  ( -3.755786496842899057E-14, 1.703125000341434214, 1.570758158831776052 ) ) ;
#100827 = CARTESIAN_POINT ( 'NONE',  ( 4.834611377684539413, 0.6298767044488963185, -1.915599524792414465 ) ) ;
#100828 = CARTESIAN_POINT ( 'NONE',  ( -4.568734577680894304, 5.392907097791561633, -1.082531754730543971 ) ) ;
#100829 = CARTESIAN_POINT ( 'NONE',  ( 7.736899214892750010, 12.17813285068358020, 1.040834085586084257E-14 ) ) ;
#100830 = CARTESIAN_POINT ( 'NONE',  ( 3.040771591214902259, 6.769593633051179005, -0.7998128361456362523 ) ) ;
#100832 = DIRECTION ( 'NONE',  ( 0.000000000000000000, 0.000000000000000000, -1.000000000000000000 ) ) ;
#100831 = CARTESIAN_POINT ( 'NONE',  ( 2.174178736149934732, -1.123764393468742684, 1.438770255985911684 ) ) ;
#100833 = CARTESIAN_POINT ( 'NONE',  ( -6.445975688654487001, 6.485002823043819475, -0.7998128361456362523 ) ) ;
#100834 = CARTESIAN_POINT ( 'NONE',  ( 11.01135777277262306, 10.90000000000000036, -1.400000000000001910 ) ) ;
#100835 = CARTESIAN_POINT ( 'NONE',  ( -10.62873463776380056, 9.799999999999998934, -3.200000000000001510 ) ) ;
#100836 = ORIENTED_EDGE ( 'NONE', *, *, #203422, .F. ) ;
#100837 = CARTESIAN_POINT ( 'NONE',  ( -4.895902867866254837, 7.765618208269001066, 1.082531754730549967 ) ) ;
#100838 = CARTESIAN_POINT ( 'NONE',  ( 0.4800000000000000933, 2.999999999999999112, -2.500000000000000444 ) ) ;
#100839 = CARTESIAN_POINT ( 'NONE',  ( -8.779068160048691283, 10.20099992726700933, -1.199719254218446718 ) ) ;
#100840 = CARTESIAN_POINT ( 'NONE',  ( 6.569012466128139494, -1.559778377529440929, 1.282785893457456750 ) ) ;
#100842 = ORIENTED_EDGE ( 'NONE', *, *, #53099, .F. ) ;
#100841 = CARTESIAN_POINT ( 'NONE',  ( 0.5926325054007793858, -1.174586488569592690, 1.765252418913294319 ) ) ;
#100843 = CARTESIAN_POINT ( 'NONE',  ( -6.720001414228860881, 7.869031733802326123, -1.199719254218452047 ) ) ;
#100844 = CARTESIAN_POINT ( 'NONE',  ( 4.168242161197552420, 6.950367390450747251, -1.199719254218452047 ) ) ;
#100845 = CARTESIAN_POINT ( 'NONE',  ( 5.014554672588167783, 1.422794387333496946, -1.491179163509145811 ) ) ;
#100846 = CARTESIAN_POINT ( 'NONE',  ( 5.432267593368638181, -1.591316862017605471, -1.238322901282742805 ) ) ;
#100847 = ORIENTED_EDGE ( 'NONE', *, *, #208563, .F. ) ;
#100848 = ORIENTED_EDGE ( 'NONE', *, *, #136119, .T. ) ;
#100849 = CARTESIAN_POINT ( 'NONE',  ( -5.908535366263027555, 4.807949608181242951, 2.499999999999999112 ) ) ;
#100850 = CARTESIAN_POINT ( 'NONE',  ( -1.225000000000030065, 0.3333333340161496738, 0.7072540797572656190 ) ) ;
#100851 = AXIS2_PLACEMENT_3D ( 'NONE', #75804, #195963, #45456 ) ;
#100853 = VERTEX_POINT ( 'NONE', #143660 ) ;
#100852 = CARTESIAN_POINT ( 'NONE',  ( -6.414942957921379474, 7.513130201443591005, -1.199719254218452047 ) ) ;
#100854 = CARTESIAN_POINT ( 'NONE',  ( 4.614865537624940117, 8.465324746759504748, 0.2878883051726736086 ) ) ;
#100855 = CARTESIAN_POINT ( 'NONE',  ( 4.903672622533055581, 0.3418847601762939337, 1.986741992616162245 ) ) ;
#100856 = CARTESIAN_POINT ( 'NONE',  ( 5.191278274421009975, -0.6593680717656666967, 1.719199333795925710 ) ) ;
#100857 = AXIS2_PLACEMENT_3D ( 'NONE', #132458, #59686, #72732 ) ;
#100858 = CARTESIAN_POINT ( 'NONE',  ( -0.02338929933905046013, 4.099262448077650944, -2.266018688142543258 ) ) ;
#100859 = CARTESIAN_POINT ( 'NONE',  ( 2.666999619196269045, -1.590435880060107499, 1.672335932400937253 ) ) ;
#100860 = CARTESIAN_POINT ( 'NONE',  ( 5.332099551924443404, 9.442809587212341427, 0.000000000000000000 ) ) ;
#100861 = CARTESIAN_POINT ( 'NONE',  ( 5.220075184997099882, -1.151474455836385857, -1.829185309946822713 ) ) ;
#100862 = CARTESIAN_POINT ( 'NONE',  ( 7.633404179693907388, 8.864391950186421454, -1.199719254218441611 ) ) ;
#100863 = CARTESIAN_POINT ( 'NONE',  ( 6.462460624273299814, -1.686435539877573220, -0.7394478613861471539 ) ) ;
#100864 = CARTESIAN_POINT ( 'NONE',  ( -5.111587607552082524, 5.922272616020886282, 1.199719254218450271 ) ) ;
#100865 = CARTESIAN_POINT ( 'NONE',  ( 4.130415602100383943, 0.2865403768554532493, -2.280420282979139124 ) ) ;
#100866 = CARTESIAN_POINT ( 'NONE',  ( -9.549485338617042629, 15.20529649091228919, -7.267374014294610163 ) ) ;
#100867 = CARTESIAN_POINT ( 'NONE',  ( -3.820365424000704557, 7.679119771301277098, -0.7998128361456481317 ) ) ;
#100868 = CARTESIAN_POINT ( 'NONE',  ( 3.238977024203249400, -1.650389259550872456, 0.8806316622528218563 ) ) ;
#100871 = CARTESIAN_POINT ( 'NONE',  ( -6.961185525973791144, 7.086080966583015339, 0.7998128361456341429 ) ) ;
#100870 = CARTESIAN_POINT ( 'NONE',  ( -0.7500000000000249800, -0.7770833326505161009, 1.299038105676659116 ) ) ;
#100869 = CARTESIAN_POINT ( 'NONE',  ( 1.212987991671743204, 1.561712320281399835, -1.103468303573502673 ) ) ;
#100872 = CARTESIAN_POINT ( 'NONE',  ( 3.352369063006555905, 2.207063162671081713, 4.936380160885933677E-05 ) ) ;
#100873 = CARTESIAN_POINT ( 'NONE',  ( 6.620655732516614655, 0.0004550665019913459623, 2.073887158236030093 ) ) ;
#100874 = CARTESIAN_POINT ( 'NONE',  ( 3.948449050077836642, 5.629609863222681199, 1.599625672291267398 ) ) ;
#100875 = CARTESIAN_POINT ( 'NONE',  ( 7.146556367734771875, 8.470642196179646533, 1.082531754730549967 ) ) ;
#100876 = CARTESIAN_POINT ( 'NONE',  ( -3.276266675996675204, 6.974061555304760240, -0.7998128361456281477 ) ) ;
#100877 = CARTESIAN_POINT ( 'NONE',  ( -7.282137903871469753, 8.628820655005750240, 1.082531754730549078 ) ) ;
#100878 = CARTESIAN_POINT ( 'NONE',  ( 0.7199194774221047144, -1.050951492028269874, -1.667678589039832904 ) ) ;
#100879 = CARTESIAN_POINT ( 'NONE',  ( 6.445943507803128192, 0.8898977879068777908, -2.129411633396756098 ) ) ;
#100880 = CARTESIAN_POINT ( 'NONE',  ( 1.170277241841523264, -0.8789641444944886750, -1.754005360843587047 ) ) ;
#100881 = CARTESIAN_POINT ( 'NONE',  ( 4.118078732422246979, 2.047561256575948452, -0.2476526470514497091 ) ) ;
#100882 = CARTESIAN_POINT ( 'NONE',  ( 5.422898255786183341, 7.349800603215774331, -1.443375672974051449 ) ) ;
#100883 = CARTESIAN_POINT ( 'NONE',  ( 5.155843554946782703, 9.237177590738404831, -0.7998128361456481317 ) ) ;
#100884 = EDGE_LOOP ( 'NONE', ( #68128, #48416, #89355, #31084 ) ) ;
#100885 = CARTESIAN_POINT ( 'NONE',  ( 7.415946836550714849, 9.675023947441092176, 1.443375672974076540 ) ) ;
#100886 = CARTESIAN_POINT ( 'NONE',  ( 1.364683531249990311, 4.196875000341417028, 1.214306433183764966E-14 ) ) ;
#100887 = CARTESIAN_POINT ( 'NONE',  ( 11.80248046418316044, 12.30000000000000071, -1.695421849633145017 ) ) ;
#100888 = CARTESIAN_POINT ( 'NONE',  ( 2.846849068745292755, 6.265148313604064434, 0.000000000000000000 ) ) ;
#100889 = CARTESIAN_POINT ( 'NONE',  ( 6.162576015390932582, -0.7755629475397389783, -2.028117739495437277 ) ) ;
#100891 = CARTESIAN_POINT ( 'NONE',  ( 6.392148736875968851, -0.4980823202534767624, -1.772533436741857260 ) ) ;
#100890 = LINE ( 'NONE', #16426, #77099 ) ;
#100892 = CARTESIAN_POINT ( 'NONE',  ( -1.387358672527334136, 7.251968950354660493, -4.302625267139479348 ) ) ;
#100893 = CARTESIAN_POINT ( 'NONE',  ( 1.826099658462914777, 3.981846818258164777, 0.3999999999999847566 ) ) ;
#100894 = CARTESIAN_POINT ( 'NONE',  ( 1.088877184111051832, 1.652420591378001014, -0.8765777015899288704 ) ) ;
#100895 = CARTESIAN_POINT ( 'NONE',  ( -5.937252720508472414, 6.122620518184580973, 0.7955437839095025332 ) ) ;
#100896 = CARTESIAN_POINT ( 'NONE',  ( 6.546060204425600659, 6.805396270974036987, -0.4351356575816138772 ) ) ;
#100897 = CARTESIAN_POINT ( 'NONE',  ( -1.364683531250012516, 4.801041667008083991, -0.7879004041258300672 ) ) ;
#100898 = CARTESIAN_POINT ( 'NONE',  ( 1.014147342612067737, -1.912461472154961317, 0.0006945104691555297090 ) ) ;
#100899 = CARTESIAN_POINT ( 'NONE',  ( 3.150976108479891735, -1.446007784402236318, -1.020181273144848744 ) ) ;
#100900 = CARTESIAN_POINT ( 'NONE',  ( 0.4164788467995067522, -0.6444665046171775824, -1.800526059235994403 ) ) ;
#100902 = CARTESIAN_POINT ( 'NONE',  ( 4.833546035289306708, 0.5969252065377036454, -1.820314225251006945 ) ) ;
#100901 = DIRECTION ( 'NONE',  ( 0.000000000000000000, 1.000000000000000000, 0.000000000000000000 ) ) ;
#100903 = CARTESIAN_POINT ( 'NONE',  ( -3.511198596259299087, 6.271927390929313617, -7.499999999999997335 ) ) ;
#100904 = CARTESIAN_POINT ( 'NONE',  ( 5.934039001034627780, 1.171926208273272207, 1.582800714458313385 ) ) ;
#100905 = CARTESIAN_POINT ( 'NONE',  ( 0.7562902151678205787, 0.8540304730459827853, -1.941197329821432227 ) ) ;
#100906 = CYLINDRICAL_SURFACE ( 'NONE', #162210, 1.000000000000000222 ) ;
#100907 = CARTESIAN_POINT ( 'NONE',  ( 3.977312496258199825, 1.761605600429091201, -0.6297503393934977822 ) ) ;
#100909 = VERTEX_POINT ( 'NONE', #94884 ) ;
#100908 = CARTESIAN_POINT ( 'NONE',  ( 0.9964003531478006215, -0.4411313887022934033, -1.771462291394958255 ) ) ;
#100911 = CARTESIAN_POINT ( 'NONE',  ( -1.876320386020336795, -0.7120587666045246067, 0.8722162550184210383 ) ) ;
#100910 = CARTESIAN_POINT ( 'NONE',  ( 3.914836437932368796, 1.561248537261412883, -1.560010120355350471 ) ) ;
#100912 = EDGE_CURVE ( 'NONE', #204354, #141010, #189216, .T. ) ;
#100913 = CARTESIAN_POINT ( 'NONE',  ( -0.6823417656249969321, 4.530208333674755394, -1.181850606188749264 ) ) ;
#100914 = CARTESIAN_POINT ( 'NONE',  ( 0.6958484739430546018, -1.457389369856504358, -1.459923026165359516 ) ) ;
#100915 = CARTESIAN_POINT ( 'NONE',  ( 5.991813822235618758, 9.077867661661846554, 1.199719254218462483 ) ) ;
#100916 = CARTESIAN_POINT ( 'NONE',  ( -8.992082194361570302, 11.51384853155376220, 1.599625672291269396 ) ) ;
#100917 = CARTESIAN_POINT ( 'NONE',  ( 1.445103857048100515, 8.688264192037886247, 2.625611233228254182 ) ) ;
#100918 = CARTESIAN_POINT ( 'NONE',  ( -3.433841370118181580, -0.01667935949903331938, -0.3944899663380890265 ) ) ;
#100919 = CARTESIAN_POINT ( 'NONE',  ( 0.1753634416057497647, 2.004068818557998011, -2.558292918872175914 ) ) ;
#100920 = ORIENTED_EDGE ( 'NONE', *, *, #20260, .T. ) ;
#100921 = CARTESIAN_POINT ( 'NONE',  ( 3.191909353267761151, -1.388477207968623839, -1.535938721777901472 ) ) ;
#100922 = CARTESIAN_POINT ( 'NONE',  ( 0.7499999999999902300, 3.983333333333352488, 1.299038105676669330 ) ) ;
#100923 = CARTESIAN_POINT ( 'NONE',  ( 1.071799524545346216, 2.083542002058445863, -0.5754571431841256635 ) ) ;
#100924 = CARTESIAN_POINT ( 'NONE',  ( -6.005252172667468358, 7.091917859149008407, -1.064983193601161338 ) ) ;
#100925 = CARTESIAN_POINT ( 'NONE',  ( 1.998700280430569576, -1.981126291604264233, -0.3917822458236255301 ) ) ;
#100926 = CARTESIAN_POINT ( 'NONE',  ( 6.938893903907228378E-15, 10.64264068711930733, 1.214306433183764966E-14 ) ) ;
#100928 = CARTESIAN_POINT ( 'NONE',  ( 8.270110514656034084, 9.711179024262627024, 1.082531754730558626 ) ) ;
#100927 = CARTESIAN_POINT ( 'NONE',  ( 1.737499999999999378, -3.966666666666666785, -3.009438278150925683 ) ) ;
#100929 = CARTESIAN_POINT ( 'NONE',  ( 6.573592277014387975, 1.495820547097841846, -1.351949839681468868 ) ) ;
#100930 = CARTESIAN_POINT ( 'NONE',  ( 0.7433754753295095385, 0.3886281223182270761, -1.978556061772406505 ) ) ;
#100931 = CARTESIAN_POINT ( 'NONE',  ( 0.000000000000000000, 1.000000000000000888, 0.000000000000000000 ) ) ;
#100932 = CARTESIAN_POINT ( 'NONE',  ( 5.337503337980974649, 0.8888059580158399475, -2.003405333693850654 ) ) ;
#100933 = CARTESIAN_POINT ( 'NONE',  ( -1.500000000000011324, 2.952083334016149418, 0.8660254037844403729 ) ) ;
#100934 = CARTESIAN_POINT ( 'NONE',  ( 3.304848191199673213, -0.3775801424153284458, -1.874573493127674961 ) ) ;
#100935 = CARTESIAN_POINT ( 'NONE',  ( -5.253948220495577637, 6.088359997788290734, 1.199719254218450271 ) ) ;
#100936 = CARTESIAN_POINT ( 'NONE',  ( 3.945059511452237100, 6.586024615794168646, -1.082531754730548412 ) ) ;
#100938 = CARTESIAN_POINT ( 'NONE',  ( 0.5797041155359906606, -0.7231210598357665775, 1.882482590253447663 ) ) ;
#100937 = CARTESIAN_POINT ( 'NONE',  ( -8.961576348508637935, 12.43862759236002269, -1.082531754730543083 ) ) ;
#100939 = CARTESIAN_POINT ( 'NONE',  ( 1.364683531249996529, 11.77604166700806410, 0.7879004041258405033 ) ) ;
#100941 = CARTESIAN_POINT ( 'NONE',  ( -6.168033539574333979, 6.160736982450306876, 0.7998128361456281477 ) ) ;
#100940 = CARTESIAN_POINT ( 'NONE',  ( 0.8203738007961014489, 1.359819376615223785, -1.845384199244608947 ) ) ;
#100942 = CARTESIAN_POINT ( 'NONE',  ( 4.594587176762323644, -0.3796550294026636574, -1.682289508650273602 ) ) ;
#100943 = CARTESIAN_POINT ( 'NONE',  ( -0.1399997263889820043, 5.722209607272843002, -2.594334538518060729 ) ) ;
#100944 = CARTESIAN_POINT ( 'NONE',  ( 4.681643115420508039, 4.356338477612361260, 0.7998128361456341429 ) ) ;
#100945 = CARTESIAN_POINT ( 'NONE',  ( -0.02264175331115856823, -0.002534049983801976106, -2.089079740194143220 ) ) ;
#100946 = CARTESIAN_POINT ( 'NONE',  ( 1.486689167417578394, 1.889818972856545987, 0.5264814339432166701 ) ) ;
#100947 = CARTESIAN_POINT ( 'NONE',  ( 3.469446951953614189E-15, 6.400000000000023448, 1.214306433183764966E-14 ) ) ;
#100948 = CARTESIAN_POINT ( 'NONE',  ( 4.168242161197552420, 6.950367390450747251, -1.199719254218452047 ) ) ;
#100949 = CARTESIAN_POINT ( 'NONE',  ( 0.07556134207192634344, 1.307170157424314638, -2.493659143521540500 ) ) ;
#100950 = FILL_AREA_STYLE_COLOUR ( '', #165397 ) ;
#100951 = VERTEX_POINT ( 'NONE', #91692 ) ;
#100952 = CARTESIAN_POINT ( 'NONE',  ( 4.354050602105923318, 0.7703955181818689102, -1.639620356061684436 ) ) ;
#100953 = ORIENTED_EDGE ( 'NONE', *, *, #78317, .F. ) ;
#100954 = CARTESIAN_POINT ( 'NONE',  ( 6.367489420273535039, 7.457767740854454708, -1.199719254218452047 ) ) ;
#100955 = FACE_OUTER_BOUND ( 'NONE', #14433, .T. ) ;
#100956 = CARTESIAN_POINT ( 'NONE',  ( 5.285751626526108637, 1.744147384919532140, -0.4889748023358466145 ) ) ;
#100957 = CARTESIAN_POINT ( 'NONE',  ( 5.519577934094840543, 9.453608333170423705, 0.7216878364870317197 ) ) ;
#100958 = CARTESIAN_POINT ( 'NONE',  ( 2.276274698451039580, 5.633392974947595278, -0.5486624834757477531 ) ) ;
#100959 = CARTESIAN_POINT ( 'NONE',  ( 5.283544098290614777, 6.372568566219670494, -1.132182188465682859 ) ) ;
#100960 = COLOUR_RGB ( '', 0.40784314, 0.44705882, 0.49803922) ;
#100962 = CARTESIAN_POINT ( 'NONE',  ( 9.297140650669039275, 11.86975006391249643, 1.599625672291281386 ) ) ;
#100961 = CARTESIAN_POINT ( 'NONE',  ( 5.916418678859147740, 0.7547467877644217227, 1.701316312257817875 ) ) ;
#100963 = CARTESIAN_POINT ( 'NONE',  ( 3.866719127221716512, -0.1911932653220274059, -1.906053554140298756 ) ) ;
#100964 = CARTESIAN_POINT ( 'NONE',  ( -6.745710774231114648, -7.818797203689479502, -6.689804758640219617 ) ) ;
#100965 = CARTESIAN_POINT ( 'NONE',  ( -11.65681998539108655, 6.358950688113277572, -4.978640985104797245 ) ) ;
#100966 = EDGE_CURVE ( 'NONE', #178226, #178739, #59155, .T. ) ;
#100967 = FACE_OUTER_BOUND ( 'NONE', #105150, .T. ) ;
#100968 = PRESENTATION_STYLE_ASSIGNMENT (( #133520 ) ) ;
#100969 = CARTESIAN_POINT ( 'NONE',  ( 5.450014563013511726, 8.341805509282339770, -1.082531754730543083 ) ) ;
#100970 = CARTESIAN_POINT ( 'NONE',  ( -8.188761592974033832, 12.49737959187099179, -0.7216878364870267237 ) ) ;
#100971 = CARTESIAN_POINT ( 'NONE',  ( 1.024558638192473170, 1.287004556549703693, -1.736669753874709343 ) ) ;
#100972 = CARTESIAN_POINT ( 'NONE',  ( -5.581116510680924847, 6.540332679663050541, -1.199719254218453823 ) ) ;
#100973 = CARTESIAN_POINT ( 'NONE',  ( 5.529746549527311039, 7.544733289238903851, -1.599625672291281386 ) ) ;
#100974 = CARTESIAN_POINT ( 'NONE',  ( 0.8678470384533981674, 0.8956018474440343713, 1.590720368640268001 ) ) ;
#100975 = CARTESIAN_POINT ( 'NONE',  ( -5.603597561149804562, 5.431951997629870910, 0.7998128361456341429 ) ) ;
#100976 = CARTESIAN_POINT ( 'NONE',  ( 3.311362000969253039, -0.3573404788377898544, 1.790086433339547201 ) ) ;
#100977 = CARTESIAN_POINT ( 'NONE',  ( 9.963343620504341303, 12.35838256557349979, -7.799456358664951239 ) ) ;
#100978 = CARTESIAN_POINT ( 'NONE',  ( 1.599720133015330337, 1.321132142916726204, 1.382909031182079307 ) ) ;
#100979 = ORIENTED_EDGE ( 'NONE', *, *, #193834, .T. ) ;
#100980 = CARTESIAN_POINT ( 'NONE',  ( 2.805082309988204514, -1.639025760435019130, 1.091792480472515647 ) ) ;
#100981 = CARTESIAN_POINT ( 'NONE',  ( 5.284693219347969873, 1.710810618512406789, -0.9191280305995457311 ) ) ;
#100982 = CARTESIAN_POINT ( 'NONE',  ( -3.492107083971660586, 6.231819477012331632, 1.199719254218452935 ) ) ;
#100984 = CARTESIAN_POINT ( 'NONE',  ( 4.658503719480325600, 2.115088938745744329, 0.1532479335744421078 ) ) ;
#100983 = CARTESIAN_POINT ( 'NONE',  ( 5.083381250481017410, 4.895309311841474553, 0.7998128361456352531 ) ) ;
#100985 = CARTESIAN_POINT ( 'NONE',  ( -7.006746397889348721, 6.052176462752765218, -2.500000000000000000 ) ) ;
#100986 = CARTESIAN_POINT ( 'NONE',  ( 9.043452155515161905, 10.50944792197790889, 1.199719254218453823 ) ) ;
#100987 = CARTESIAN_POINT ( 'NONE',  ( 5.980536202102920917, 6.100347882654393317, -0.6550157475838751520 ) ) ;
#100988 = DIRECTION ( 'NONE',  ( 0.000000000000000000, 0.000000000000000000, 1.000000000000000000 ) ) ;
#100989 = ORIENTED_EDGE ( 'NONE', *, *, #207178, .F. ) ;
#100990 = CARTESIAN_POINT ( 'NONE',  ( -1.364683531250010740, 13.13020833367472839, 0.7879004041258445001 ) ) ;
#100991 = CARTESIAN_POINT ( 'NONE',  ( 3.230585741806197841, 6.991043475407723307, 0.7998128361456271485 ) ) ;
#100992 = CARTESIAN_POINT ( 'NONE',  ( 3.486418057008484617, 7.219238166485217434, 1.040834085586084257E-14 ) ) ;
#100993 = CARTESIAN_POINT ( 'NONE',  ( 6.384963997392946844, 6.413822516572072807, 0.7998128361456352531 ) ) ;
#100994 = CARTESIAN_POINT ( 'NONE',  ( 0.000000000000000000, 4.000007913748540922, 0.000000000000000000 ) ) ;
#100995 = CARTESIAN_POINT ( 'NONE',  ( 5.320859459983126705, 1.688362619374352613, 0.6951667914897319278 ) ) ;
#100996 = CARTESIAN_POINT ( 'NONE',  ( 10.99950989413227909, -9.915617157791128733, -0.1038368378055223862 ) ) ;
#100997 = CARTESIAN_POINT ( 'NONE',  ( -9.381879110976678149, 11.00824238663667565, 1.082531754730558626 ) ) ;
#100998 = VECTOR ( 'NONE', #154901, 1000.000000000000227 ) ;
#100999 = CARTESIAN_POINT ( 'NONE',  ( -6.454776619733716636, 6.787828609132271929, -0.3692292702514640146 ) ) ;
#101000 = CARTESIAN_POINT ( 'NONE',  ( 7.011678565220082149, -6.606405293530973388, -6.580818069395332870 ) ) ;
#101001 = CARTESIAN_POINT ( 'NONE',  ( 5.963714631206167738, 1.842656449598079060, -0.3214700631931910468 ) ) ;
#101002 = CARTESIAN_POINT ( 'NONE',  ( 6.479907352327590964, 9.647310113435821677, 1.199719254218462483 ) ) ;
#101003 = CARTESIAN_POINT ( 'NONE',  ( 3.264201069286599477, 0.8669165009558920110, 1.720499056138290683 ) ) ;
#101004 = CARTESIAN_POINT ( 'NONE',  ( -4.786191920824102830, 5.542644314838231168, 1.199719254218462483 ) ) ;
#101005 = CARTESIAN_POINT ( 'NONE',  ( 4.891794496432329886, 4.601515088792824670, -0.7998128361456211532 ) ) ;
#101006 = CARTESIAN_POINT ( 'NONE',  ( -1.402160292154681736E-14, 9.234375000341398021, 1.575800808251682339 ) ) ;
#101007 = CARTESIAN_POINT ( 'NONE',  ( -4.737684612971557740, 7.614716917520386374, 1.199719254218464037 ) ) ;
#101008 = CARTESIAN_POINT ( 'NONE',  ( 4.708759422647839976, 4.387974169377582001, -0.7998128361456211532 ) ) ;
#101009 = CARTESIAN_POINT ( 'NONE',  ( -3.485854892044994102, 7.080931450778859215, -0.7216878364870458196 ) ) ;
#101010 =( BOUNDED_CURVE ( )  B_SPLINE_CURVE ( 2, ( #121, #31609, #66188, #97684, #117170, #198339, #64103, #116097, #18529 ),
 .UNSPECIFIED., .F., .T. ) 
 B_SPLINE_CURVE_WITH_KNOTS ( ( 3, 2, 2, 2, 3 ),
 ( 0.1875000000000000000, 0.1944444444444444475, 0.2083333333333333426, 0.2222222222222222099, 0.2291666666666666574 ),
 .UNSPECIFIED. ) 
 CURVE ( )  GEOMETRIC_REPRESENTATION_ITEM ( )  RATIONAL_B_SPLINE_CURVE ( ( 0.9330127018922194093, 0.9330127018922194093, 1.000000000000000000, 0.8660254037844387076, 1.000000000000000000, 0.8660254037844387076, 1.000000000000000000, 0.9330127018922194093, 0.9330127018922194093 ) ) 
 REPRESENTATION_ITEM ( '' )  );
#101011 = CARTESIAN_POINT ( 'NONE',  ( 1.564221677423253798, -1.129412574612179920, 1.790659096458546706 ) ) ;
#101012 = CARTESIAN_POINT ( 'NONE',  ( 9.077347539549325717, 10.54899253668443393, -1.199719254218446718 ) ) ;
#101013 = CARTESIAN_POINT ( 'NONE',  ( -0.7499999999999972244, 3.608333333333359150, -1.299038105676652011 ) ) ;
#101014 = CARTESIAN_POINT ( 'NONE',  ( 6.719590346122157776, 0.3599300073104904074, -2.038585587018165945 ) ) ;
#101016 = CARTESIAN_POINT ( 'NONE',  ( 4.012431654125413694, 7.810675627703163038, 0.2615036927465386740 ) ) ;
#101015 = CARTESIAN_POINT ( 'NONE',  ( 1.821575194732877545, 1.059174331173462935, -1.505913648122420900 ) ) ;
#101017 = CARTESIAN_POINT ( 'NONE',  ( 4.826339496784873617, 8.574553812983598533, -0.7216878364870257245 ) ) ;
#101018 = CARTESIAN_POINT ( 'NONE',  ( 4.095971805104288599, 5.871996087412059140, 1.443375672974058777 ) ) ;
#101019 = CARTESIAN_POINT ( 'NONE',  ( 1.834309667284042433, 2.267783887084608097, 0.3333485250246841503 ) ) ;
#101020 = CARTESIAN_POINT ( 'NONE',  ( 0.1174333910212103232, -1.791171220025630895, 0.3524246893974944395 ) ) ;
#101021 = B_SPLINE_CURVE_WITH_KNOTS ( 'NONE', 3,
 ( #47806, #161541, #78135, #162603, #131223, #180965 ),
 .UNSPECIFIED., .F., .F.,
 ( 4, 2, 4 ),
 ( 0.000000000000000000, 0.0003845013059668467856, 0.0007690026119336935712 ),
 .UNSPECIFIED. ) ;
#101022 = ORIENTED_EDGE ( 'NONE', *, *, #182167, .T. ) ;
#101023 = CARTESIAN_POINT ( 'NONE',  ( 6.900736999231407154, 10.99468423250458038, -0.7216878364870267237 ) ) ;
#101024 = CARTESIAN_POINT ( 'NONE',  ( 0.5627444733627232631, 0.5882401669465211480, 1.925320163072720359 ) ) ;
#101025 = CARTESIAN_POINT ( 'NONE',  ( 0.5847188370675902025, 1.875566754216885013, 0.5750099747552291918 ) ) ;
#101026 = CARTESIAN_POINT ( 'NONE',  ( -8.462260433223891098, 13.02438760540324481, -0.7998128361456281477 ) ) ;
#101028 = CARTESIAN_POINT ( 'NONE',  ( -3.469446951953614189E-15, 8.920000000000001705, -2.420000000000000373 ) ) ;
#101027 = CARTESIAN_POINT ( 'NONE',  ( -7.232384877886063990, 10.52520055992070525, -1.199719254218446718 ) ) ;
#101029 = CARTESIAN_POINT ( 'NONE',  ( 3.285556943750000070, -0.7218749995220423710, 0.000000000000000000 ) ) ;
#101031 = CARTESIAN_POINT ( 'NONE',  ( 2.658786778619155022, -1.538754371767250495, -0.8742638447295988380 ) ) ;
#101030 = CARTESIAN_POINT ( 'NONE',  ( 3.802746959959231177, 1.793210335683467216, 1.074525653306056316 ) ) ;
#101032 = DIRECTION ( 'NONE',  ( 0.000000000000000000, 0.000000000000000000, 1.000000000000000000 ) ) ;
#101033 = ADVANCED_FACE ( 'NONE', ( #125313 ), #191272, .F. ) ;
#101035 = CARTESIAN_POINT ( 'NONE',  ( 5.015721488424509822, -1.223180480392561886, -1.938471153541870384 ) ) ;
#101034 = DIRECTION ( 'NONE',  ( 0.000000000000000000, 1.000000000000000000, 0.000000000000000000 ) ) ;
#101036 = CARTESIAN_POINT ( 'NONE',  ( 2.993823619545363801, -0.5058645990140339110, -1.665172204756032448 ) ) ;
#101037 = CARTESIAN_POINT ( 'NONE',  ( 8.353795204314554468, 12.89784483834236184, -0.7998128361456352531 ) ) ;
#101038 = AXIS2_PLACEMENT_3D ( 'NONE', #42112, #192579, #108224 ) ;
#101039 = CARTESIAN_POINT ( 'NONE',  ( 4.549643065837591038, 7.465611455855944101, -1.199719254218452047 ) ) ;
#101040 = CARTESIAN_POINT ( 'NONE',  ( 2.758840240711700531, -1.728971274941538017, -0.1308756186972348801 ) ) ;
#101041 = CARTESIAN_POINT ( 'NONE',  ( 3.315042099977282497, -1.646035655820307309, 1.415953490726479469 ) ) ;
#101042 = CARTESIAN_POINT ( 'NONE',  ( 5.847644326195776010, 5.716673223516856694, -0.7998128361456281477 ) ) ;
#101043 = CARTESIAN_POINT ( 'NONE',  ( 4.751185534883737738, 0.1928377863454934504, -2.007255887737584121 ) ) ;
#101044 = CARTESIAN_POINT ( 'NONE',  ( 1.187500000000001110, -1.451031289061072815, 1.451031289061169183 ) ) ;
#101045 = CARTESIAN_POINT ( 'NONE',  ( 1.499999999999990896, 4.056250000682819490, 1.214306433183764966E-14 ) ) ;
#101046 = CARTESIAN_POINT ( 'NONE',  ( 1.852440960305309137, 0.6018503411110776025, 1.830038407220703656 ) ) ;
#101047 = CARTESIAN_POINT ( 'NONE',  ( 0.7500000000000006661, 9.114583334016129967, 1.299038105676657340 ) ) ;
#101048 = CARTESIAN_POINT ( 'NONE',  ( 5.115582552657226501, 1.816446842268246931, 1.278514946224351689 ) ) ;
#101049 = ORIENTED_EDGE ( 'NONE', *, *, #125678, .F. ) ;
#101050 = CARTESIAN_POINT ( 'NONE',  ( -0.1108833634136975610, 0.7331455517814323697, -1.980187714524218823 ) ) ;
#101051 = B_SPLINE_CURVE_WITH_KNOTS ( 'NONE', 3,
 ( #10753, #175420, #110474, #59512 ),
 .UNSPECIFIED., .F., .F.,
 ( 4, 4 ),
 ( 1.910166083080831124E-17, 0.002003498272494318600 ),
 .UNSPECIFIED. ) ;
#101052 = CARTESIAN_POINT ( 'NONE',  ( -0.7500000000000006661, 2.358333333333358262, -1.299038105676652011 ) ) ;
#101053 = CARTESIAN_POINT ( 'NONE',  ( 7.623762449586013901, 7.788811034138823253, 1.040834085586084257E-14 ) ) ;
#101054 = CARTESIAN_POINT ( 'NONE',  ( 3.673896439178911066, 7.230036912443299713, 0.7216878364870317197 ) ) ;
#101055 = CARTESIAN_POINT ( 'NONE',  ( -3.285556943750000514, -1.888541666188711110, -1.896917185911906722 ) ) ;
#101056 = CARTESIAN_POINT ( 'NONE',  ( 6.057081135787192316, 1.604708697955498087, -1.128374156723031430 ) ) ;
#101057 = CARTESIAN_POINT ( 'NONE',  ( 8.270110514656034084, 9.711179024262627024, 1.082531754730558626 ) ) ;
#101058 = ADVANCED_FACE ( 'NONE', ( #158799 ), #61861, .T. ) ;
#101059 = CARTESIAN_POINT ( 'NONE',  ( 6.573497657123517079, 2.167905964706399846, -0.6471699410235329797 ) ) ;
#101060 = AXIS2_PLACEMENT_3D ( 'NONE', #109480, #191699, #91044 ) ;
#101061 = CARTESIAN_POINT ( 'NONE',  ( 4.366607992053101128, 7.252070536440704096, -1.199719254218448494 ) ) ;
#101063 = AXIS2_PLACEMENT_3D ( 'NONE', #160418, #7748, #10946 ) ;
#101062 = CARTESIAN_POINT ( 'NONE',  ( -4.285785955695645910, 7.053815144069948140, 1.082531754730549967 ) ) ;
#101064 = CARTESIAN_POINT ( 'NONE',  ( 3.947761307511790552, 1.492003129663575622, 1.424497906600069363 ) ) ;
#101065 = CARTESIAN_POINT ( 'NONE',  ( -3.730464822054482710, 7.503959392372201442, 1.040834085586084257E-14 ) ) ;
#101066 = CARTESIAN_POINT ( 'NONE',  ( -1.001543065824772872E-14, 4.493750000682820378, 1.732050807568877637 ) ) ;
#101067 = CARTESIAN_POINT ( 'NONE',  ( -1.364683531250000748, 0.009375000341420303140, 0.000000000000000000 ) ) ;
#101068 = CARTESIAN_POINT ( 'NONE',  ( 6.327412175546781370, -1.761338861328298089, 0.6302073946208713862 ) ) ;
#101069 = CARTESIAN_POINT ( 'NONE',  ( 4.658689525625823613, 1.003974855541647004, 1.413729434382102079 ) ) ;
#101070 = CARTESIAN_POINT ( 'NONE',  ( 4.809955069398625938, 1.195453170786121788, -1.265177307932338513 ) ) ;
#101071 = DIRECTION ( 'NONE',  ( 0.000000000000000000, 8.546850786086437571E-32, 1.000000000000000000 ) ) ;
#101072 = CARTESIAN_POINT ( 'NONE',  ( 2.226505721922732661, 2.224568380592424344, 0.5530147644091478742 ) ) ;
#101073 = CARTESIAN_POINT ( 'NONE',  ( -1.364683531249997417, 4.071875000341417028, 1.214306433183764966E-14 ) ) ;
#101074 = CARTESIAN_POINT ( 'NONE',  ( 5.724191925653110857, 2.015179739716387974, 0.5568145835738461669 ) ) ;
#101075 = CARTESIAN_POINT ( 'NONE',  ( 0.02305342982030639601, -1.130023889514218505, -1.454075609423427728 ) ) ;
#101076 = CARTESIAN_POINT ( 'NONE',  ( -1.299038105676632915, 7.500000000000000000, -0.7500000000000006661 ) ) ;
#101077 = CARTESIAN_POINT ( 'NONE',  ( 1.072888940501380839, -0.9041080511620370741, 1.802418165037560138 ) ) ;
#101078 = CARTESIAN_POINT ( 'NONE',  ( 8.655961103042326243, 13.72543968248328561, -9.385390936148914065 ) ) ;
#101079 = CARTESIAN_POINT ( 'NONE',  ( -9.189729191964438826, 9.615772233580322848, 1.040834085586084257E-14 ) ) ;
#101080 = CARTESIAN_POINT ( 'NONE',  ( 5.144429221381498607, 8.089252293998699272, -1.199719254218452047 ) ) ;
#101081 = CARTESIAN_POINT ( 'NONE',  ( 3.686284471605893120, 1.179319764668992576, 1.762089746328721507 ) ) ;
#101082 = CARTESIAN_POINT ( 'NONE',  ( 0.6823417656249864960, -0.5739583329919112353, -1.181850606188749264 ) ) ;
#101083 = CARTESIAN_POINT ( 'NONE',  ( 5.162654993523497993, -1.319871331358621669, 1.261628347558927166 ) ) ;
#101084 = EDGE_LOOP ( 'NONE', ( #123482, #176091, #164128, #117173, #153395, #91103, #116210, #144172, #158966, #11044, #195630, #83408, #28308, #152946, #121010, #186382 ) ) ;
#101085 = CARTESIAN_POINT ( 'NONE',  ( -7.144220599758281054, 7.299621885998258897, 0.7998128361456341429 ) ) ;
#101086 = CARTESIAN_POINT ( 'NONE',  ( 2.272730219304121668, 5.707593880249651086, 0.2947169286177344638 ) ) ;
#101087 = CARTESIAN_POINT ( 'NONE',  ( 6.739811759324814133, 8.956476034002680109, -1.443375672974078761 ) ) ;
#101088 = CARTESIAN_POINT ( 'NONE',  ( 0.000000000000000000, -0.9843749995220403282, -3.793834371823813001 ) ) ;
#101089 = CARTESIAN_POINT ( 'NONE',  ( -7.379715684540041565, 7.504089808251839244, 1.040834085586084257E-14 ) ) ;
#101090 = CARTESIAN_POINT ( 'NONE',  ( 2.918227964375613048, -2.017298000423489501, 0.1032239234411459483 ) ) ;
#101091 = CARTESIAN_POINT ( 'NONE',  ( 6.704147062870869256, -2.206433763861126884, 0.04732420095975712476 ) ) ;
#101092 = VECTOR ( 'NONE', #202544, 1000.000000000000000 ) ;
#101093 = CARTESIAN_POINT ( 'NONE',  ( 9.673906298550626559, 11.24497775551929557, 1.199719254218452047 ) ) ;
#101094 = CARTESIAN_POINT ( 'NONE',  ( 3.590524784426767813, 1.814595775041549564, 0.4119230038364861679 ) ) ;
#101095 = CARTESIAN_POINT ( 'NONE',  ( 7.730120138085914583, 12.17022392774227768, 0.7998128361456462443 ) ) ;
#101096 = CARTESIAN_POINT ( 'NONE',  ( 11.88172094500853504, 13.87999994398406045, -1.685553348215862446 ) ) ;
#101097 = CARTESIAN_POINT ( 'NONE',  ( -3.521367211247373508, 5.131347717920458962, -1.599625672291256295 ) ) ;
#101098 =( BOUNDED_SURFACE ( )  B_SPLINE_SURFACE ( 3, 2, ( 
 ( #73825, #89028, #142062 ),
 ( #6669, #75959, #7738 ),
 ( #27198, #191822, #122675 ),
 ( #60773, #139919, #22912 ),
 ( #57581, #109605, #126932 ),
 ( #175610, #41353, #157224 ) ),
 .UNSPECIFIED., .F., .F., .T. ) 
 B_SPLINE_SURFACE_WITH_KNOTS ( ( 4, 2, 4 ),
 ( 3, 3 ),
 ( 0.000000000000000000, 0.0003754689591423960443, 0.0007509379182847920886 ),
 ( 0.000000000000000000, 1.000000000000000000 ),
 .UNSPECIFIED. ) 
 GEOMETRIC_REPRESENTATION_ITEM ( )  RATIONAL_B_SPLINE_SURFACE ( (
 ( 1.000000000000000000, 0.7071067811865551223, 1.000000000000000000),
 ( 1.000000000000000000, 0.7018599272026829761, 1.000000000000000000),
 ( 1.000000000000000000, 0.6927733177256546471, 1.000000000000000000),
 ( 1.000000000000000000, 0.6772007068877438085, 1.000000000000000000),
 ( 1.000000000000000000, 0.6709974581634302604, 1.000000000000000000),
 ( 1.000000000000000000, 0.6711954675835395401, 1.000000000000000000) ) ) 
 REPRESENTATION_ITEM ( '' )  SURFACE ( )  );
#101099 = CARTESIAN_POINT ( 'NONE',  ( -6.496328159242330536, 10.73079995242472862, 0.000000000000000000 ) ) ;
#101101 = CARTESIAN_POINT ( 'NONE',  ( -4.377387467589398007, 7.366231944554199274, 1.201952607213795821 ) ) ;
#101100 = CARTESIAN_POINT ( 'NONE',  ( -7.099629715411508890, 8.311931418515415615, 1.199719254218452047 ) ) ;
#101102 = CARTESIAN_POINT ( 'NONE',  ( 0.6823417656249864960, -1.073958332991911568, -1.181850606188749264 ) ) ;
#101103 = ADVANCED_FACE ( 'NONE', ( #144723 ), #102789, .F. ) ;
#101104 = CARTESIAN_POINT ( 'NONE',  ( 1.915017753259074862, 0.5389909111754992432, 1.648018863455216643 ) ) ;
#101105 = CARTESIAN_POINT ( 'NONE',  ( 0.9018503542332901857, 1.320273433284512521, -1.133937880871397796 ) ) ;
#101107 = CARTESIAN_POINT ( 'NONE',  ( 6.941411460516762943, 11.04213777067082702, -0.7216878364870267237 ) ) ;
#101106 = CARTESIAN_POINT ( 'NONE',  ( 0.1656154469977044186, -2.063490973871735967, -1.033197247175041467 ) ) ;
#101108 = CARTESIAN_POINT ( 'NONE',  ( 6.222152418221221559, 7.023474430343600083, -1.033429630759775675 ) ) ;
#101109 = CARTESIAN_POINT ( 'NONE',  ( 1.880222553438152033, -1.104958259108330898, 1.739320704499922154 ) ) ;
#101110 = CARTESIAN_POINT ( 'NONE',  ( 0.1927366488196740335, -1.238295061544148812, -1.591656064170659191 ) ) ;
#101111 = DIRECTION ( 'NONE',  ( 0.000000000000000000, 0.000000000000000000, -1.000000000000000000 ) ) ;
#101112 = CARTESIAN_POINT ( 'NONE',  ( -4.423703259808839938, 8.383013913077441259, 0.7998128361456352531 ) ) ;
#101113 = CARTESIAN_POINT ( 'NONE',  ( 0.4089732319989903275, 1.714023354001862787, 0.9739579164984181192 ) ) ;
#101115 = CARTESIAN_POINT ( 'NONE',  ( -6.617788377246193399, 8.814115421577600529, -1.443375672974066548 ) ) ;
#101114 = CARTESIAN_POINT ( 'NONE',  ( 5.150612376422202487, 1.885107930906554152, 0.3209214958604587054 ) ) ;
#101116 = CARTESIAN_POINT ( 'NONE',  ( 5.953802724510455668, 0.6443607167232848765, -2.110727517106169682 ) ) ;
#101117 = CARTESIAN_POINT ( 'NONE',  ( -1.225000000000036060, 2.291666667349470998, -0.7072540797573277915 ) ) ;
#101118 = CARTESIAN_POINT ( 'NONE',  ( -7.362820735710029041, -5.796536394784445712, -7.362820735712818809 ) ) ;
#101119 = CARTESIAN_POINT ( 'NONE',  ( 5.045042557616584489, 5.058506870073687267, 0.000000000000000000 ) ) ;
#101120 = CARTESIAN_POINT ( 'NONE',  ( -3.133342898089680695, 6.669667457830990465, 0.7216878364870338292 ) ) ;
#101121 = CARTESIAN_POINT ( 'NONE',  ( -0.1048592448738161903, -0.1538584160990438265, -1.986454975908092058 ) ) ;
#101122 = ORIENTED_EDGE ( 'NONE', *, *, #190752, .F. ) ;
#101123 = CARTESIAN_POINT ( 'NONE',  ( 3.680997481958053541, -2.223193225534472628, -0.6181044232122161475 ) ) ;
#101124 = CARTESIAN_POINT ( 'NONE',  ( 4.422284181769401634, 0.9229163912191931107, 1.731201473044993167 ) ) ;
#101125 = CARTESIAN_POINT ( 'NONE',  ( 1.112071775475082402, 1.959765382314464732, -0.09068415226199526280 ) ) ;
#101126 = CARTESIAN_POINT ( 'NONE',  ( 3.714570900464285064, 4.396382807705524698, 1.082531754730560403 ) ) ;
#101127 = CARTESIAN_POINT ( 'NONE',  ( 6.761669295867161367, -7.008190897455697232, 6.673079560224753237 ) ) ;
#101128 = ORIENTED_EDGE ( 'NONE', *, *, #71473, .F. ) ;
#101129 = CARTESIAN_POINT ( 'NONE',  ( -0.1704767588886099972, -1.641208087572191276, -1.337381612054800772 ) ) ;
#101131 = CARTESIAN_POINT ( 'NONE',  ( -9.020252271793614440, 9.418049160047695878, 0.7998128361456462443 ) ) ;
#101130 = CARTESIAN_POINT ( 'NONE',  ( -4.599240423533815125, 6.388866465587984322, 1.599625672291267398 ) ) ;
#101132 = CARTESIAN_POINT ( 'NONE',  ( 0.000000000000000000, 11.29999999999999893, 0.000000000000000000 ) ) ;
#101133 = CARTESIAN_POINT ( 'NONE',  ( 3.186559800492471783, 1.209906992153013894, -1.802498320862821579 ) ) ;
#101134 = CARTESIAN_POINT ( 'NONE',  ( 0.1024722964814587939, 2.599067505215466589, 1.999601597966877309 ) ) ;
#101135 = CARTESIAN_POINT ( 'NONE',  ( 1.301209403646291118, -0.3165094942152619772, -2.096747597609450953 ) ) ;
#101136 = CARTESIAN_POINT ( 'NONE',  ( -0.7500000000000006661, 3.139583334016149418, -1.299038105676652011 ) ) ;
#101137 = CARTESIAN_POINT ( 'NONE',  ( 10.06423010004587759, 10.63602329300870153, 0.000000000000000000 ) ) ;
#101138 = CARTESIAN_POINT ( 'NONE',  ( 11.86145017031113902, 13.50581953513848710, -1.100000000000000533 ) ) ;
#101139 = CARTESIAN_POINT ( 'NONE',  ( 6.580239226864286195, 6.782991656975736028, -0.2881480849740332140 ) ) ;
#101140 = CARTESIAN_POINT ( 'NONE',  ( 1.845067233098520942, -1.742569257963645146, 1.099794920586109725 ) ) ;
#101142 = CARTESIAN_POINT ( 'NONE',  ( 10.38614328979755719, 3.507114751586604129, -5.996442624206805405 ) ) ;
#101141 = CARTESIAN_POINT ( 'NONE',  ( -9.989660255170729641, 10.54902514065433827, -0.7998128361456291469 ) ) ;
#101143 = CARTESIAN_POINT ( 'NONE',  ( -0.6823417656250212460, 2.301041667008084435, 1.181850606188767472 ) ) ;
#101144 = CARTESIAN_POINT ( 'NONE',  ( 0.07755575628181145265, 6.946778278137147211, -2.783982195446454533 ) ) ;
#101145 = CARTESIAN_POINT ( 'NONE',  ( 10.51568781791557328, 11.11256730203912468, 3.554797817682051164 ) ) ;
#101146 = ORIENTED_EDGE ( 'NONE', *, *, #76635, .T. ) ;
#101147 = CARTESIAN_POINT ( 'NONE',  ( 4.881465217424630687, 0.1836680969147832243, -1.903426456924644183 ) ) ;
#101148 = VECTOR ( 'NONE', #116673, 1000.000000000000000 ) ;
#101149 = CARTESIAN_POINT ( 'NONE',  ( -6.972266317189433020E-16, 1.750000000682810475, -1.225000000000013634 ) ) ;
#101150 = CARTESIAN_POINT ( 'NONE',  ( 1.353188757747030957, -1.783583821274600911, 1.391813662893444548 ) ) ;
#101151 = CIRCLE ( 'NONE', #132278, 0.08000000000000027922 ) ;
#101152 = CARTESIAN_POINT ( 'NONE',  ( -2.415323921528888196, 5.969628341758991930, 0.7998128361456341429 ) ) ;
#101153 = CARTESIAN_POINT ( 'NONE',  ( 1.423755586445039745, -1.797672382977614669, 0.2236433623570739382 ) ) ;
#101154 = CARTESIAN_POINT ( 'NONE',  ( 1.147507391605587568, 1.886754179610318438, -0.3309440326291489542 ) ) ;
#101155 = CARTESIAN_POINT ( 'NONE',  ( 2.066927875543830950, 1.535623996113824496, -1.388825173883188713 ) ) ;
#101156 = CARTESIAN_POINT ( 'NONE',  ( 0.6823417656249882723, 1.488541667008083547, -1.181850606188749264 ) ) ;
#101157 = CARTESIAN_POINT ( 'NONE',  ( 0.2859245228041712439, -0.9316758688886862538, 1.737439158343912382 ) ) ;
#101158 = CARTESIAN_POINT ( 'NONE',  ( 5.918570133321236604, 1.291915522740747502, -1.429275465086258246 ) ) ;
#101160 = CARTESIAN_POINT ( 'NONE',  ( 6.435429789636040177, 6.784273175954743884, -0.4071148367965071735 ) ) ;
#101159 = CARTESIAN_POINT ( 'NONE',  ( 6.533804136697315634, -1.437950210024591780, -1.674183229976949905 ) ) ;
#101161 = EDGE_CURVE ( 'NONE', #154836, #72912, #168492, .T. ) ;
#101162 = CARTESIAN_POINT ( 'NONE',  ( 1.364683531249988757, 1.134375000341421247, 0.000000000000000000 ) ) ;
#101163 = CARTESIAN_POINT ( 'NONE',  ( 4.527816470857299436, 2.001556401900002058, -0.4979991880497411372 ) ) ;
#101164 = CARTESIAN_POINT ( 'NONE',  ( -5.391338639728555648, 9.441645512991978961, -0.7998128361456231517 ) ) ;
#101165 = CARTESIAN_POINT ( 'NONE',  ( 8.589254009457354400, 9.979550084910457031, -1.199719254218446718 ) ) ;
#101166 = CARTESIAN_POINT ( 'NONE',  ( -1.420000000000021911, 8.627523663848661428, 2.580000000000011173 ) ) ;
#101167 = CARTESIAN_POINT ( 'NONE',  ( 4.496500501226593727, 8.397667684739696270, 0.7998128361456462443 ) ) ;
#101169 = CARTESIAN_POINT ( 'NONE',  ( 1.499999999999987121, 3.295833333333354709, -0.8660254037844262731 ) ) ;
#101168 = CARTESIAN_POINT ( 'NONE',  ( 5.174884205284945082, -1.981925234046210571, -0.7124256662833851061 ) ) ;
#101170 = CARTESIAN_POINT ( 'NONE',  ( 0.5378411956755309031, 2.025704276806821191, -0.7818309977141599809 ) ) ;
#101171 = CARTESIAN_POINT ( 'NONE',  ( -0.6823417656250003738, 1.030208333674752286, -1.181850606188749264 ) ) ;
#101172 = CARTESIAN_POINT ( 'NONE',  ( 4.921240491056324551, -0.1114908479964340365, 2.158860929761210912 ) ) ;
#101173 = CARTESIAN_POINT ( 'NONE',  ( 5.848308768596990781, 0.9934667122631580805, -1.758341319078795761 ) ) ;
#101174 = CARTESIAN_POINT ( 'NONE',  ( 1.284279953904126748, 10.64264068711930733, -0.7749999999999874767 ) ) ;
#101175 = EDGE_CURVE ( 'NONE', #72492, #49868, #199548, .T. ) ;
#101178 = CARTESIAN_POINT ( 'NONE',  ( 6.209271165378815738, 7.306866450105836464, -1.082531754730543083 ) ) ;
#101177 = CARTESIAN_POINT ( 'NONE',  ( 1.642778471875000035, -1.626041666188710044, -2.845375778867859751 ) ) ;
#101176 = CARTESIAN_POINT ( 'NONE',  ( 7.095713291905693332, 9.371694488680407886, 1.599625672291268286 ) ) ;
#101179 = CARTESIAN_POINT ( 'NONE',  ( -6.642568916052639771, 6.714361588341672515, 0.000000000000000000 ) ) ;
#101180 = CARTESIAN_POINT ( 'NONE',  ( 3.221888912838869690, 0.9023448338944944913, -1.803416113280359445 ) ) ;
#101181 = CARTESIAN_POINT ( 'NONE',  ( -7.641992139597101108, 12.06740792950531649, 0.7998128361456481317 ) ) ;
#101183 = CARTESIAN_POINT ( 'NONE',  ( -1.045839947578414805E-15, 1.812499999999992673, 1.224999999999988987 ) ) ;
#101182 = CARTESIAN_POINT ( 'NONE',  ( -3.358669367883384105, 4.941533567329135401, -1.599625672291262513 ) ) ;
#101185 = CARTESIAN_POINT ( 'NONE',  ( 0.07933194154487546723, -7.609852571077992067, -9.499668754385622194 ) ) ;
#101184 = CARTESIAN_POINT ( 'NONE',  ( 5.278265135069068137, -1.204163492603943064, 1.795060720813673738 ) ) ;
#101186 = CARTESIAN_POINT ( 'NONE',  ( -1.123270288250318494, 3.297697346350006331, -0.7749999999993560929 ) ) ;
#101187 = DIRECTION ( 'NONE',  ( -1.000000000000000000, 0.000000000000000000, 0.000000000000000000 ) ) ;
#101189 = CARTESIAN_POINT ( 'NONE',  ( 5.817982510940042040, 0.9913841921252890543, -1.755779027446252138 ) ) ;
#101188 = CARTESIAN_POINT ( 'NONE',  ( -5.870317324592805086, 9.792527945426188651, -0.7216878364870197293 ) ) ;
#101190 = CARTESIAN_POINT ( 'NONE',  ( 1.499999999999989120, 5.004166666666691299, 0.8660254037844524744 ) ) ;
#101191 = CARTESIAN_POINT ( 'NONE',  ( 0.8380132626705768528, 1.698558605200460869, 0.2991625477344951323 ) ) ;
#101192 = CARTESIAN_POINT ( 'NONE',  ( 6.737475991348287785, 6.825086509519945999, -0.7998128361456481317 ) ) ;
#101193 = CIRCLE ( 'NONE', #90868, 0.08000000000000014044 ) ;
#101195 = CARTESIAN_POINT ( 'NONE',  ( 7.842465510862060896, 8.114240948952696542, 0.000000000000000000 ) ) ;
#101194 = CARTESIAN_POINT ( 'NONE',  ( 7.402388683381404988, 10.61957531637824204, -1.082531754730537976 ) ) ;
#101196 = DIRECTION ( 'NONE',  ( -5.578564026256490882E-16, -1.000000000000000000, -9.066213480720158442E-32 ) ) ;
#101197 = CARTESIAN_POINT ( 'NONE',  ( 5.307814152003552444, -1.861618091082300808, 0.1822119596564600597 ) ) ;
#101198 = CARTESIAN_POINT ( 'NONE',  ( -0.05795285570054254515, -1.240470478354677164, -1.586248892985191006 ) ) ;
#101199 = CARTESIAN_POINT ( 'NONE',  ( -10.83760360872516060, 4.885615726745599297, 4.963138928152970308 ) ) ;
#101200 = CARTESIAN_POINT ( 'NONE',  ( 4.500943809612556024, 4.353448654077163305, 1.214306433183764966E-14 ) ) ;
#101201 = CARTESIAN_POINT ( 'NONE',  ( -5.112833325684904118, 8.979072956692109031, -0.7216878364870338292 ) ) ;
#101202 = ORIENTED_EDGE ( 'NONE', *, *, #207506, .T. ) ;
#101203 = CARTESIAN_POINT ( 'NONE',  ( 8.717529583462633624, 13.11427558077437894, 0.7216878364870438212 ) ) ;
#101206 = EDGE_CURVE ( 'NONE', #29321, #114168, #171288, .T. ) ;
#101205 = CARTESIAN_POINT ( 'NONE',  ( 0.8961114988408731552, -0.9091644883451601711, -1.799914091915676639 ) ) ;
#101204 = CARTESIAN_POINT ( 'NONE',  ( 2.139458383197485603, 0.002846582261652879763, 2.120667954922689002 ) ) ;
#101207 = CARTESIAN_POINT ( 'NONE',  ( 6.526270840131753737, 8.707344961610770540, -1.599625672291283607 ) ) ;
#101208 = CARTESIAN_POINT ( 'NONE',  ( 6.280167721515548251, -1.160692707240444710, 1.823489969145650313 ) ) ;
#101209 = CARTESIAN_POINT ( 'NONE',  ( 7.019370843573166319, 9.212351955633947043, 1.599625672291281386 ) ) ;
#101210 = CIRCLE ( 'NONE', #104644, 7.424569270082293393 ) ;
#101212 = CARTESIAN_POINT ( 'NONE',  ( 0.5498253489954890716, 0.9468162992772524156, 1.665335589065963129 ) ) ;
#101211 = CARTESIAN_POINT ( 'NONE',  ( -5.766295404513795297, 5.621766148221195358, 0.7998128361456341429 ) ) ;
#101213 = VECTOR ( 'NONE', #77852, 1000.000000000000000 ) ;
#101214 = CARTESIAN_POINT ( 'NONE',  ( 0.7499999999999902300, 5.066666666666684193, -1.299038105676658228 ) ) ;
#101215 = CARTESIAN_POINT ( 'NONE',  ( -1.292658234375052784, 2.851562500512133447, -3.816391647148975608E-14 ) ) ;
#101216 = CARTESIAN_POINT ( 'NONE',  ( 6.493992390821439642, 7.639041213122241381, -1.082531754730543971 ) ) ;
#101217 = EDGE_CURVE ( 'NONE', #135745, #12495, #50987, .T. ) ;
#101218 = CARTESIAN_POINT ( 'NONE',  ( -1.364683531250014514, -0.9072916663252470482, 0.7879004041258379498 ) ) ;
#101219 = CARTESIAN_POINT ( 'NONE',  ( 3.768803514918948938, 4.459654191235965293, -1.082531754730543083 ) ) ;
#101220 = CARTESIAN_POINT ( 'NONE',  ( -4.081167932913447594, 4.720116328942494555, -1.199719254218452047 ) ) ;
#101221 = CARTESIAN_POINT ( 'NONE',  ( 4.012696165952275962, 1.530467462299599735, -1.526897427004340280 ) ) ;
#101222 = ADVANCED_FACE ( 'NONE', ( #209280 ), #54896, .T. ) ;
#101223 = CARTESIAN_POINT ( 'NONE',  ( -4.638297949650955765, 8.425448351319163365, 0.7216878364870267237 ) ) ;
#101224 = CARTESIAN_POINT ( 'NONE',  ( 4.719646871332936477, 8.520355426614829142, -0.7216878364870357165 ) ) ;
#101225 = CARTESIAN_POINT ( 'NONE',  ( 1.459403507577087700, -1.788631592985808538, 1.138920039206146928 ) ) ;
#101226 = CARTESIAN_POINT ( 'NONE',  ( 3.147653791585693028, 8.920000000000001705, 2.419999999999999485 ) ) ;
#101227 = CIRCLE ( 'NONE', #194629, 0.2000000000000005107 ) ;
#101228 = CARTESIAN_POINT ( 'NONE',  ( 2.723849342626927239, -1.131982996307562273, -1.613792087129195085 ) ) ;
#101229 = CARTESIAN_POINT ( 'NONE',  ( 4.640819915729988310, 1.831716588661407963, 0.5496940206762624959 ) ) ;
#101230 = EDGE_LOOP ( 'NONE', ( #170417, #11352, #206497, #53942 ) ) ;
#101231 = DIRECTION ( 'NONE',  ( 0.000000000000000000, 8.546850786086437571E-32, 1.000000000000000000 ) ) ;
#101232 = CARTESIAN_POINT ( 'NONE',  ( 6.355907380368630122, -0.6650989860433678125, 1.853973344504164622 ) ) ;
#101233 = CARTESIAN_POINT ( 'NONE',  ( 0.9900592867461569524, -0.4711592545371501295, -1.883805795384153381 ) ) ;
#101234 = ORIENTED_EDGE ( 'NONE', *, *, #34519, .T. ) ;
#101235 = CARTESIAN_POINT ( 'NONE',  ( -4.716257332707368910, 6.595662536282280719, -1.599625672291271394 ) ) ;
#101236 = CARTESIAN_POINT ( 'NONE',  ( -5.171509248969888617, 4.998125310078441075, 0.7998128361456281477 ) ) ;
#101237 = CARTESIAN_POINT ( 'NONE',  ( 5.957918438201454059, 9.038323046955323292, -1.199719254218440723 ) ) ;
#101239 = CARTESIAN_POINT ( 'NONE',  ( 5.356880090730863131, 7.343055753976412525, 1.443375672974064550 ) ) ;
#101238 = CARTESIAN_POINT ( 'NONE',  ( 5.960781091502512119, 10.10599504006161986, 0.7998128361456462443 ) ) ;
#101241 = ORIENTED_EDGE ( 'NONE', *, *, #148232, .T. ) ;
#101240 = CARTESIAN_POINT ( 'NONE',  ( 6.322915745023367506, 1.413667134151237459, -1.287952294376143447 ) ) ;
#101242 = CARTESIAN_POINT ( 'NONE',  ( 3.405080638938757343, 1.739790774466195789, -1.357627211771177178 ) ) ;
#101243 = AXIS2_PLACEMENT_3D ( 'NONE', #3472, #181182, #100988 ) ;
#101244 = CARTESIAN_POINT ( 'NONE',  ( 2.468050989216635127, 2.164326253657654853, -0.4298898877757306725 ) ) ;
#101245 = CARTESIAN_POINT ( 'NONE',  ( -11.92619526913700057, 19.00000000000000000, -1.328859060402686199 ) ) ;
#101246 = CARTESIAN_POINT ( 'NONE',  ( 0.2231138172586397683, 1.663799575440491285, 0.9424754157791456199 ) ) ;
#101247 = CARTESIAN_POINT ( 'NONE',  ( -2.279673327430177476, 5.603443282069742182, 1.040551764627347231E-14 ) ) ;
#101248 = CARTESIAN_POINT ( 'NONE',  ( -6.729185449012799580, -6.864242550357221972, -6.701130152864378076 ) ) ;
#101249 = CARTESIAN_POINT ( 'NONE',  ( 3.086448098943677998, 1.152334561581969785, -1.719836228861029603 ) ) ;
#101250 = CARTESIAN_POINT ( 'NONE',  ( -6.084912014434944894, 5.993485526462540847, -0.7998128361456291469 ) ) ;
#101251 = CARTESIAN_POINT ( 'NONE',  ( -5.773214272755326171, 7.262619621122762048, 1.194638459467006530 ) ) ;
#101253 = CARTESIAN_POINT ( 'NONE',  ( 1.376082401959723089, 1.288024388040419632, 1.735935173841046675 ) ) ;
#101252 = CARTESIAN_POINT ( 'NONE',  ( -5.115504031057831469, 4.862509545855891346, 0.7998128361456341429 ) ) ;
#101254 = CARTESIAN_POINT ( 'NONE',  ( 3.579775959861815515, -1.078688530630707243, 1.907616655872627964 ) ) ;
#101255 = CARTESIAN_POINT ( 'NONE',  ( -1.081945585493433448, -0.9830613892718149671, 3.305300248233959515 ) ) ;
#101256 = CARTESIAN_POINT ( 'NONE',  ( 4.475600106286968582, 5.354526557823810151, -1.082531754730548412 ) ) ;
#101257 = CARTESIAN_POINT ( 'NONE',  ( 1.408440994508643129, 7.230285460703517408, 4.273713947604631080 ) ) ;
#101258 = CARTESIAN_POINT ( 'NONE',  ( 0.6823417656249934904, 15.00520833367473195, 1.181850606188764807 ) ) ;
#101259 = CARTESIAN_POINT ( 'NONE',  ( -5.387385936583832802, 7.378645907471495846, -1.599625672291271394 ) ) ;
#101260 = CARTESIAN_POINT ( 'NONE',  ( 6.469374514269041754, -1.702674068921444572, -0.3278888851577909658 ) ) ;
#101261 = CARTESIAN_POINT ( 'NONE',  ( -2.252626078164912560, 5.779814191167667481, 0.7998128361456341429 ) ) ;
#101262 = CARTESIAN_POINT ( 'NONE',  ( 4.118080132427735407, 2.055207691244304691, -0.2483996215696740451 ) ) ;
#101263 = CARTESIAN_POINT ( 'NONE',  ( 5.044581972647897317, -1.532752649812264778, 1.460808053437604226 ) ) ;
#101264 = CARTESIAN_POINT ( 'NONE',  ( 7.311924916471702396, 7.425000578838787391, -0.7998128361456281477 ) ) ;
#101265 = CARTESIAN_POINT ( 'NONE',  ( -1.364683531250010740, 4.280208333674753618, 0.7879004041258379498 ) ) ;
#101266 = CARTESIAN_POINT ( 'NONE',  ( 2.571101405699018017, 1.757081157110135017, 0.8898057773328130748 ) ) ;
#101267 = CARTESIAN_POINT ( 'NONE',  ( 0.3516297456669579269, -1.353986107606550471, -1.350798769753497552 ) ) ;
#101268 = CARTESIAN_POINT ( 'NONE',  ( 5.367208288505312730, 2.210367218987763671, -0.6069939957479841830 ) ) ;
#101269 = CARTESIAN_POINT ( 'NONE',  ( 2.683998146737070378, -0.9385614705539682134, 1.565816405032012470 ) ) ;
#101270 = CARTESIAN_POINT ( 'NONE',  ( 3.553118775233146120, 6.302999783484076524, -1.199719254218453823 ) ) ;
#101271 = CARTESIAN_POINT ( 'NONE',  ( 5.138177029454836564, 7.977995053463880382, 1.082531754730558626 ) ) ;
#101272 = CARTESIAN_POINT ( 'NONE',  ( -5.181187258716735577, 9.196468901811520880, 0.7998128361456481317 ) ) ;
#101274 = VERTEX_POINT ( 'NONE', #44701 ) ;
#101273 =( BOUNDED_CURVE ( )  B_SPLINE_CURVE ( 2, ( #68054, #32396, #31337, #116900, #35577, #81142, #166663, #162406, #113716 ),
 .UNSPECIFIED., .F., .T. ) 
 B_SPLINE_CURVE_WITH_KNOTS ( ( 3, 2, 2, 2, 3 ),
 ( 0.2031250000000001388, 0.2083333333333333426, 0.2187500000000000000, 0.2291666666666666574, 0.2343749999999997780 ),
 .UNSPECIFIED. ) 
 CURVE ( )  GEOMETRIC_REPRESENTATION_ITEM ( )  RATIONAL_B_SPLINE_CURVE ( ( 0.9330127018922194093, 0.9330127018922211857, 1.000000000000000000, 0.8660254037844387076, 1.000000000000000000, 0.8660254037844387076, 1.000000000000000000, 0.9330127018922221849, 0.9330127018922194093 ) ) 
 REPRESENTATION_ITEM ( '' )  );
#101275 = CARTESIAN_POINT ( 'NONE',  ( 3.463142787923169763, -1.643428793820296718, 1.162544664348450496 ) ) ;
#101276 = CARTESIAN_POINT ( 'NONE',  ( 3.994932754639446859, 0.2835094185691371393, 1.941019531709553103 ) ) ;
#101277 = CARTESIAN_POINT ( 'NONE',  ( -6.157374318900681764, 10.33535380535947290, 0.7998128361456481317 ) ) ;
#101278 = B_SPLINE_CURVE_WITH_KNOTS ( 'NONE', 3,
 ( #164847, #16439, #51098, #198392 ),
 .UNSPECIFIED., .F., .F.,
 ( 4, 4 ),
 ( 2.941991273438700769E-15, 0.0007499567245562745437 ),
 .UNSPECIFIED. ) ;
#101279 = CARTESIAN_POINT ( 'NONE',  ( -5.225778143063529946, 8.184159369294361497, 1.199719254218452047 ) ) ;
#101280 = DIRECTION ( 'NONE',  ( 1.000000000000000000, 0.000000000000000000, 0.000000000000000000 ) ) ;
#101282 = CARTESIAN_POINT ( 'NONE',  ( 5.787929806067755756, -0.7924508370336593721, 1.582612139130882278 ) ) ;
#101281 = CARTESIAN_POINT ( 'NONE',  ( 0.3454080995960371325, 0.6521308015206389586, -1.986527616087286452 ) ) ;
#101283 = FACE_OUTER_BOUND ( 'NONE', #27133, .T. ) ;
#101284 = EDGE_CURVE ( 'NONE', #145502, #99491, #158431, .T. ) ;
#101285 = CARTESIAN_POINT ( 'NONE',  ( 1.675987266036529366, -1.170314894790158933, 1.852603040092117848 ) ) ;
#101286 = CARTESIAN_POINT ( 'NONE',  ( 6.632745071352946553, -1.550850273991890127, 0.7898216520882040959 ) ) ;
#101287 = CARTESIAN_POINT ( 'NONE',  ( 8.423693512792301163, 8.722063941212843119, 0.7998128361456481317 ) ) ;
#101288 = CARTESIAN_POINT ( 'NONE',  ( 0.1333692844072801587, 4.087911462428309051, -2.608372271572469092 ) ) ;
#101289 = CARTESIAN_POINT ( 'NONE',  ( 1.031410063161166013, -1.091267733730487466, -1.335775140220570201 ) ) ;
#101290 = CARTESIAN_POINT ( 'NONE',  ( 0.7382080005397623212, -2.165046367600947708, -0.7717227881791683952 ) ) ;
#101291 = CARTESIAN_POINT ( 'NONE',  ( 0.3631484714031462668, 0.2087870660046411420, -2.181583536649676525 ) ) ;
#101292 = CARTESIAN_POINT ( 'NONE',  ( 6.362590153729421161, -0.5805357501837383749, 1.633877867761362124 ) ) ;
#101293 = CARTESIAN_POINT ( 'NONE',  ( 2.526237079854487089, -1.271617311931704686, -1.803507373242494438 ) ) ;
#101294 = AXIS2_PLACEMENT_3D ( 'NONE', #61623, #130703, #196694 ) ;
#101295 = CARTESIAN_POINT ( 'NONE',  ( 6.602019255160630706, 0.8372048429528687885, -2.003470777635954381 ) ) ;
#101296 = DIRECTION ( 'NONE',  ( 0.000000000000000000, 1.000000000000000000, 0.000000000000000000 ) ) ;
#101297 = CARTESIAN_POINT ( 'NONE',  ( 2.202504513770195516, 1.378945901905674232, -1.606877091071600816 ) ) ;
#101298 = CARTESIAN_POINT ( 'NONE',  ( 6.727182134110168299, 1.217656702865956397, 2.400974650093392171 ) ) ;
#101299 = CARTESIAN_POINT ( 'NONE',  ( 5.069325366411169931, 0.1891801624123757852, -1.917091172425288370 ) ) ;
#101300 = ORIENTED_EDGE ( 'NONE', *, *, #36782, .T. ) ;
#101302 = CARTESIAN_POINT ( 'NONE',  ( -1.201851678989727383E-14, 5.337500000000020783, -1.732050807568863648 ) ) ;
#101301 = CARTESIAN_POINT ( 'NONE',  ( 2.050677904428706455, -1.769283327057631805, 1.457584778241685974 ) ) ;
#101303 = CARTESIAN_POINT ( 'NONE',  ( 5.034155109375821446, 4.767602470560229122, -0.7998128361456221525 ) ) ;
#101304 = CARTESIAN_POINT ( 'NONE',  ( 4.469384193999260901, 8.366031992974468423, -0.7998128361456231517 ) ) ;
#101305 = CARTESIAN_POINT ( 'NONE',  ( 4.530067796519579026, -2.178530490643998174, 0.4330045798939685109 ) ) ;
#101306 = CARTESIAN_POINT ( 'NONE',  ( -7.158341918335454857, 10.33485409049125003, 1.082531754730549967 ) ) ;
#101307 = CARTESIAN_POINT ( 'NONE',  ( -1.140665321753059347, 3.300000000000025135, -0.7542256614604591070 ) ) ;
#101308 = CARTESIAN_POINT ( 'NONE',  ( 4.338245966692901412, 8.005111361209628740, -0.7216878364870197293 ) ) ;
#101309 = CARTESIAN_POINT ( 'NONE',  ( -6.819388077549415783, 10.89977715720891815, 0.7216878364870458196 ) ) ;
#101310 = CARTESIAN_POINT ( 'NONE',  ( 5.777182853198898904, 6.873039762554409293, -1.082531754730548412 ) ) ;
#101311 = ORIENTED_EDGE ( 'NONE', *, *, #160649, .F. ) ;
#101312 = CARTESIAN_POINT ( 'NONE',  ( 3.393204081532863459, -0.8197727808607684352, -1.842447475547980495 ) ) ;
#101314 = CARTESIAN_POINT ( 'NONE',  ( 0.8310137546357538874, -1.940837517380919808, -0.6983779148895614686 ) ) ;
#101313 = CARTESIAN_POINT ( 'NONE',  ( 6.265839547809997079, 10.46189657242035587, 0.7998128361456462443 ) ) ;
#101315 = CARTESIAN_POINT ( 'NONE',  ( -11.89321938400720491, 13.76255278360659062, 1.599605898944226334 ) ) ;
#101316 = CARTESIAN_POINT ( 'NONE',  ( 5.926322542504858681, 8.007405281046052536, -1.443375672974078761 ) ) ;
#101317 = CARTESIAN_POINT ( 'NONE',  ( 0.000000000000000000, 3.481548657788671619, 0.000000000000000000 ) ) ;
#101318 = CARTESIAN_POINT ( 'NONE',  ( -1.364683531250012516, 3.030208333674755394, 0.7879004041258379498 ) ) ;
#101319 = CARTESIAN_POINT ( 'NONE',  ( 4.453197812796324762, 0.4814713343750369190, -2.137748681182354726 ) ) ;
#101320 = CARTESIAN_POINT ( 'NONE',  ( 0.8267963299631932994, 0.8146243292815741333, -1.844710905833810255 ) ) ;
#101321 = CARTESIAN_POINT ( 'NONE',  ( 1.540310226958538475, -1.555040833713853710, 0.9856339240054690087 ) ) ;
#101322 = CARTESIAN_POINT ( 'NONE',  ( 4.722401423535961484, 2.193339426362813871, 0.6665824366990577010 ) ) ;
#101323 = CARTESIAN_POINT ( 'NONE',  ( 3.855264089065893351, 1.827008581971893530, -0.2271198879545410221 ) ) ;
#101324 = CARTESIAN_POINT ( 'NONE',  ( 9.610031953988080744, 10.10612545594124967, -0.7998128361456281477 ) ) ;
#101325 = SHAPE_REPRESENTATION_RELATIONSHIP ( 'NONE' , 'NONE' ,  #121983, #156107 ) ;
#101326 = CARTESIAN_POINT ( 'NONE',  ( 4.489149150750438189, 1.630474666268775685, -0.8212668906743822994 ) ) ;
#101327 = CARTESIAN_POINT ( 'NONE',  ( 5.010388774477189777, -1.913804350592800629, 0.6351971752796632398 ) ) ;
#101328 = CARTESIAN_POINT ( 'NONE',  ( -9.501566725078754772, 9.979582688880366703, -0.7998128361456291469 ) ) ;
#101330 = CARTESIAN_POINT ( 'NONE',  ( -7.065734331377342414, 8.272386803808890576, -1.199719254218452047 ) ) ;
#101329 = CARTESIAN_POINT ( 'NONE',  ( 4.979486748501788185, 2.112903116282875082, -0.8095491994110515233 ) ) ;
#101331 = CARTESIAN_POINT ( 'NONE',  ( 0.1355649208573142805, -1.924581242375450030, 0.8557158107796616342 ) ) ;
#101332 =( NAMED_UNIT ( * ) SI_UNIT ( $, .STERADIAN. ) SOLID_ANGLE_UNIT ( ) );
#101333 = CARTESIAN_POINT ( 'NONE',  ( 3.367693471486675083, -0.4065805204805824635, 2.029877954327436118 ) ) ;
#101334 = CARTESIAN_POINT ( 'NONE',  ( 2.866659414285625651, 5.431854185720147221, -1.199719254218446718 ) ) ;
#101335 = CARTESIAN_POINT ( 'NONE',  ( -1.360316468750011332, 2.421875000341397577, -1.387778780781445676E-14 ) ) ;
#101336 = SHAPE_DEFINITION_REPRESENTATION ( #109439, #40301 ) ;
#101338 = CARTESIAN_POINT ( 'NONE',  ( 1.787598692544673851, 1.328180555690385845, 1.395690353023341101 ) ) ;
#101337 = CARTESIAN_POINT ( 'NONE',  ( -9.189729191964438826, 9.615772233580322848, 1.040834085586084257E-14 ) ) ;
#101339 = UNCERTAINTY_MEASURE_WITH_UNIT (LENGTH_MEASURE( 1.000000000000000082E-05 ), #45689, 'distance_accuracy_value', 'NONE');
#101340 = DIRECTION ( 'NONE',  ( 0.000000000000000000, 0.000000000000000000, 1.000000000000000000 ) ) ;
#101341 = CARTESIAN_POINT ( 'NONE',  ( 6.977413706903823787, -0.1529601955215283693, 1.936277946061695898 ) ) ;
#101342 = CARTESIAN_POINT ( 'NONE',  ( 5.085717018457579286, 6.066329622022862189, -1.082531754730548412 ) ) ;
#101343 = CARTESIAN_POINT ( 'NONE',  ( 5.766360146646302809, 6.053989883630594981, 0.5864573027323967125 ) ) ;
#101344 = CARTESIAN_POINT ( 'NONE',  ( -3.253066792275140173, 5.882662793374543675, 1.199719254218462483 ) ) ;
#101346 = CARTESIAN_POINT ( 'NONE',  ( 1.512303732575480675, -0.7424040314494853021, 2.093836701676012879 ) ) ;
#101345 = CARTESIAN_POINT ( 'NONE',  ( 0.5277791401020451856, -0.3051165123582540994, 2.098401203810342786 ) ) ;
#101347 = CIRCLE ( 'NONE', #84029, 0.1000000000000000472 ) ;
#101348 = CARTESIAN_POINT ( 'NONE',  ( 2.837057662192625340, 0.2562861413469962879, 2.090225181913709207 ) ) ;
#101349 = CARTESIAN_POINT ( 'NONE',  ( -7.937372586157736443, 8.224965870130965584, 0.7998128361456341429 ) ) ;
#101350 = CARTESIAN_POINT ( 'NONE',  ( 6.531277313481192337, 8.642909503859968368, 1.599625672291281386 ) ) ;
#101351 = CARTESIAN_POINT ( 'NONE',  ( 0.3087543870234563115, -1.498283157731963966, 1.103738804280843366 ) ) ;
#101352 = CARTESIAN_POINT ( 'NONE',  ( 6.262976894508937242, 9.394224579314053969, -1.199719254218440723 ) ) ;
#101353 = CARTESIAN_POINT ( 'NONE',  ( -4.356251871828045630, 7.199010410547511007, -1.027643995846918790 ) ) ;
#101354 = CARTESIAN_POINT ( 'NONE',  ( 5.820528018968444961, 5.685037531751635953, 0.7998128361456341429 ) ) ;
#101355 = CARTESIAN_POINT ( 'NONE',  ( -5.261973015879593873, 8.192700047617899273, 1.082531754730549967 ) ) ;
#101356 = CARTESIAN_POINT ( 'NONE',  ( -8.676855123066030018, 9.225345186439589895, -0.7216878364870267237 ) ) ;
#101357 = CARTESIAN_POINT ( 'NONE',  ( 1.318772358905948794, -0.7683209907942339933, -1.976687055281033611 ) ) ;
#101358 = CARTESIAN_POINT ( 'NONE',  ( -6.774234028683526532, 7.932303117332766718, 1.199719254218452047 ) ) ;
#101360 = CARTESIAN_POINT ( 'NONE',  ( 4.562918044398325712, 1.517878595006398212, -1.242988302126393441 ) ) ;
#101359 = CARTESIAN_POINT ( 'NONE',  ( 1.224999999999994982, 1.145833333333333481, -0.7072540797572898219 ) ) ;
#101361 = CARTESIAN_POINT ( 'NONE',  ( 2.958072429731006370, 2.151414462573512765, -0.2105227563667099733 ) ) ;
#101362 = CARTESIAN_POINT ( 'NONE',  ( 1.241482983173985533, 1.839155304979672501, 0.08999620058360720265 ) ) ;
#101363 = CARTESIAN_POINT ( 'NONE',  ( -4.088066877127150001, 7.522549914775793489, 0.5433784229755319606 ) ) ;
#101364 = CARTESIAN_POINT ( 'NONE',  ( -0.2582262029270495085, -8.187798858731225593, -9.496816297611141877 ) ) ;
#101365 = CARTESIAN_POINT ( 'NONE',  ( 4.839680888265717407, 1.736017449284636527, 0.1234091131117609486 ) ) ;
#101366 = CARTESIAN_POINT ( 'NONE',  ( 0.3554123170487776817, 16.00000000000087397, -12.67999999502907649 ) ) ;
#101367 = CARTESIAN_POINT ( 'NONE',  ( 5.097502569058200983, 6.970172302033127210, -1.443375672974051449 ) ) ;
#101368 = CARTESIAN_POINT ( 'NONE',  ( -10.48266952940149466, 5.268049057482275366, -5.154014898524191146 ) ) ;
#101369 = CARTESIAN_POINT ( 'NONE',  ( 1.639762333045853726, -1.565812861550972324, -1.490595759849028035 ) ) ;
#101370 = EDGE_CURVE ( 'NONE', #40935, #112763, #2407, .T. ) ;
#101371 = AXIS2_PLACEMENT_3D ( 'NONE', #4099, #3032, #55021 ) ;
#101372 = CARTESIAN_POINT ( 'NONE',  ( 3.339220083777879378, -1.203169880011810022, 1.617570133648409847 ) ) ;
#101373 = CARTESIAN_POINT ( 'NONE',  ( 0.4019237886466847653, 12.85491455036742892, 1.499999999999997113 ) ) ;
#101375 = VECTOR ( 'NONE', #90484, 1000.000000000000000 ) ;
#101374 = CARTESIAN_POINT ( 'NONE',  ( 0.9894095316701527754, 1.906041449620498929, -1.019753361306941386 ) ) ;
#101376 = CARTESIAN_POINT ( 'NONE',  ( 3.203940287746226634, -1.969268756981055635, 0.09538867180547243307 ) ) ;
#101377 = CARTESIAN_POINT ( 'NONE',  ( 6.609000000000047059, 2.429201845222619394, 2.481963755843877628 ) ) ;
#101378 = CARTESIAN_POINT ( 'NONE',  ( 3.614730616327064716, -0.1400294986239834782, 1.937054734790619293 ) ) ;
#101381 = VERTEX_POINT ( 'NONE', #79313 ) ;
#101380 = CARTESIAN_POINT ( 'NONE',  ( -3.851925040058345573, 5.587274861525073355, -1.443375672974078761 ) ) ;
#101379 = CARTESIAN_POINT ( 'NONE',  ( -9.612367721964606204, 12.23751498042398289, -1.443375672974058777 ) ) ;
#101382 = CARTESIAN_POINT ( 'NONE',  ( -4.462041952228944730, 7.259447140025469203, -1.082531754730549967 ) ) ;
#101383 = CARTESIAN_POINT ( 'NONE',  ( -0.2106854629475062024, 1.349218558350977260, -2.248994321313985800 ) ) ;
#101384 = CARTESIAN_POINT ( 'NONE',  ( 4.817943484809818600, 6.714296380401858499, 1.599625672291269396 ) ) ;
#101385 = CARTESIAN_POINT ( 'NONE',  ( -3.793249116773374396, 7.647484079536056356, 0.7998128361456352531 ) ) ;
#101386 = CARTESIAN_POINT ( 'NONE',  ( -4.620296487206990932, 8.612372678375294299, 0.000000000000000000 ) ) ;
#101387 = CARTESIAN_POINT ( 'NONE',  ( -10.42585693878457853, 11.26584730477792284, -0.7216878364870267237 ) ) ;
#101388 = CARTESIAN_POINT ( 'NONE',  ( 0.09513611692719620150, -0.4880922032983874281, -2.160105283315365998 ) ) ;
#101389 = CARTESIAN_POINT ( 'NONE',  ( 1.642778471875000035, -2.676041666188708756, -2.845375778867859751 ) ) ;
#101390 = CONICAL_SURFACE ( 'NONE', #70283, 3.999999999999998224, 0.8621700546672330656 ) ;
#101391 = CARTESIAN_POINT ( 'NONE',  ( 4.592600981049492326, 1.923087700504518605, 0.3867253955378775476 ) ) ;
#101392 = CARTESIAN_POINT ( 'NONE',  ( 1.969375177810539945, -1.978050944945686673, -0.3905967402937361443 ) ) ;
#101393 = VERTEX_POINT ( 'NONE', #94522 ) ;
#101394 = CARTESIAN_POINT ( 'NONE',  ( 3.555961197718297218, 1.179765190368966321, 1.758020836099948747 ) ) ;
#101395 = CARTESIAN_POINT ( 'NONE',  ( -1.499999999999997780, 3.431250000682818602, 1.214306433183764966E-14 ) ) ;
#101397 = CARTESIAN_POINT ( 'NONE',  ( -6.338600509588822263, 7.353787668397130162, -1.199719254218446718 ) ) ;
#101396 = CARTESIAN_POINT ( 'NONE',  ( 0.1745949693968693039, 7.629137130509094256, -2.355306170041113756 ) ) ;
#101398 = CARTESIAN_POINT ( 'NONE',  ( 2.818100271072515817, 1.733748696238574416, 0.6199764264002775027 ) ) ;
#101399 = ORIENTED_EDGE ( 'NONE', *, *, #61843, .F. ) ;
#101400 = CARTESIAN_POINT ( 'NONE',  ( -7.160677686311960777, 11.50587440067263678, -0.7998128361456291469 ) ) ;
#101401 = CARTESIAN_POINT ( 'NONE',  ( 0.4032277238576092993, 3.019957635004406171, 0.4115402804777972268 ) ) ;
#101402 = CARTESIAN_POINT ( 'NONE',  ( 5.115537534566190203, 1.735013203181461350, 1.219038288318145646 ) ) ;
#101403 = DIRECTION ( 'NONE',  ( 5.551115123125764213E-17, 0.000000000000000000, -1.000000000000000000 ) ) ;
#101404 = CARTESIAN_POINT ( 'NONE',  ( 6.612626235163189925, 8.737816579155630592, -1.599625672291262513 ) ) ;
#101405 = EDGE_CURVE ( 'NONE', #62943, #133392, #161645, .T. ) ;
#101406 = STYLED_ITEM ( 'NONE', ( #156264 ), #179324 ) ;
#101407 = CARTESIAN_POINT ( 'NONE',  ( 4.921196286130338216, -0.1051130969715245306, 2.058245376175421804 ) ) ;
#101410 = CARTESIAN_POINT ( 'NONE',  ( 2.507154105146496725, -1.820902139252629448, 0.2722148935128121394 ) ) ;
#101409 = CARTESIAN_POINT ( 'NONE',  ( 0.4493573998385214652, 1.374985906440568506, 1.254353302672887693 ) ) ;
#101408 = CARTESIAN_POINT ( 'NONE',  ( 0.000000000000000000, 12.30000000000000071, 0.000000000000000000 ) ) ;
#101411 = CARTESIAN_POINT ( 'NONE',  ( 8.992082194361556091, 11.51384853155376220, 1.599625672291279388 ) ) ;
#101412 = DIRECTION ( 'NONE',  ( 0.000000000000000000, 0.000000000000000000, -1.000000000000000000 ) ) ;
#101413 = CARTESIAN_POINT ( 'NONE',  ( -11.86145016429273191, 10.19999999999999929, 1.099999999999996758 ) ) ;
#101414 = DIRECTION ( 'NONE',  ( 5.578564026256287751E-16, 1.000000000000000000, 0.000000000000000000 ) ) ;
#101415 = CARTESIAN_POINT ( 'NONE',  ( 2.016531038934398445, -1.041976349804032420, -1.945408382319254503 ) ) ;
#101416 = CARTESIAN_POINT ( 'NONE',  ( 5.290393965937395748, -2.244422280358076005, -0.2844362755431028567 ) ) ;
#101417 = CARTESIAN_POINT ( 'NONE',  ( 3.538296236868877731, 0.7303062672313584969, 1.879804216660937666 ) ) ;
#101418 = CARTESIAN_POINT ( 'NONE',  ( -6.507550544879489252, 9.575597488125954015, 1.082531754730548412 ) ) ;
#101419 = CARTESIAN_POINT ( 'NONE',  ( 5.045072953846708508, 0.1408599011454790551, 1.806194821104394777 ) ) ;
#101420 = CARTESIAN_POINT ( 'NONE',  ( 4.399565145148922163, -1.877536364458038065, 0.3796658851462595408 ) ) ;
#101421 = CARTESIAN_POINT ( 'NONE',  ( 0.6823417656249917140, 5.655208333674749177, 1.181850606188765695 ) ) ;
#101422 = CARTESIAN_POINT ( 'NONE',  ( 3.485194120740982449, 1.782821823783652837, -0.8418218905394663221 ) ) ;
#101423 = CARTESIAN_POINT ( 'NONE',  ( 4.715616592392388284, -1.834479983729628616, 0.3652084810651031743 ) ) ;
#101424 = CARTESIAN_POINT ( 'NONE',  ( 5.230833165924736683, -1.752262279689630553, -0.6273003976000991466 ) ) ;
#101425 = CARTESIAN_POINT ( 'NONE',  ( 1.364683531249990311, 5.363541667008086655, 0.7879004041258500513 ) ) ;
#101426 = CARTESIAN_POINT ( 'NONE',  ( 0.1105650446291406575, 1.931126588553159884, 0.5807481968119408977 ) ) ;
#101428 = CARTESIAN_POINT ( 'NONE',  ( 2.192140752285096639, -0.8994906754480420652, 1.904460908831892008 ) ) ;
#101427 = CARTESIAN_POINT ( 'NONE',  ( -3.348500752450953577, 4.929670182657964084, 1.443375672974062551 ) ) ;
#101429 = CARTESIAN_POINT ( 'NONE',  ( 8.550388431712704573, 13.12720360364021133, 0.000000000000000000 ) ) ;
#101431 = LINE ( 'NONE', #4959, #101148 ) ;
#101430 = DIRECTION ( 'NONE',  ( -0.2150645590070936197, 0.8781765503997437383, 0.4272624273056206401 ) ) ;
#101432 = CARTESIAN_POINT ( 'NONE',  ( 2.995319178684289430, 6.412246817072642102, -0.4997136395867556868 ) ) ;
#101433 = CARTESIAN_POINT ( 'NONE',  ( 1.969016121511291795, -1.558499072447929956, 1.284715733913702085 ) ) ;
#101434 = CARTESIAN_POINT ( 'NONE',  ( -1.201851678989727383E-14, 1.571875000341420581, 1.575800808251672791 ) ) ;
#101435 = CARTESIAN_POINT ( 'NONE',  ( -2.467220768007014176, 5.822248629409386922, 0.7216878364870317197 ) ) ;
#101436 = CARTESIAN_POINT ( 'NONE',  ( 3.174580523894166006, 6.855427711185178019, 0.7998128361456341429 ) ) ;
#101437 = ADVANCED_FACE ( 'NONE', ( #13240 ), #44053, .T. ) ;
#101438 = CARTESIAN_POINT ( 'NONE',  ( 2.425270691926324051, -0.002641788883844811090, 2.161773191836775521 ) ) ;
#101439 = CARTESIAN_POINT ( 'NONE',  ( 6.889999999999997016, 3.693514451062899884, 2.514185260296258217 ) ) ;
#101442 = PLANE ( 'NONE',  #172979 ) ;
#101441 = CARTESIAN_POINT ( 'NONE',  ( -5.335766472694951190, 4.384919054141811046, -2.499999999999995115 ) ) ;
#101440 = CARTESIAN_POINT ( 'NONE',  ( 3.061108821635398769, 6.793320401875094561, -0.7998128361456362523 ) ) ;
#101443 = CARTESIAN_POINT ( 'NONE',  ( 8.717529583462633624, 13.11427558077437894, 0.7216878364870438212 ) ) ;
#101444 = CARTESIAN_POINT ( 'NONE',  ( 6.438686429976131720, -1.555646628146038157, 1.282773817382940384 ) ) ;
#101445 = CARTESIAN_POINT ( 'NONE',  ( -6.887178846062109727, 10.01849717283904262, -1.082531754730537976 ) ) ;
#101446 = CARTESIAN_POINT ( 'NONE',  ( 1.031118135130421498, -1.979082047791239418, 0.9416876394413642437 ) ) ;
#101447 = CARTESIAN_POINT ( 'NONE',  ( -1.084202172485504434E-15, -6.124285368610756564, -10.93005900551661114 ) ) ;
#101449 = CARTESIAN_POINT ( 'NONE',  ( -0.6823417656250003738, 12.15104166700806054, 1.181850606188754593 ) ) ;
#101448 = CARTESIAN_POINT ( 'NONE',  ( 1.481717434351536244, 2.089849803356018221, -0.8673477522002839279 ) ) ;
#101450 = CARTESIAN_POINT ( 'NONE',  ( -8.296699936558862731, 11.76690146170562201, 1.199719254218453823 ) ) ;
#101451 = CARTESIAN_POINT ( 'NONE',  ( 4.276577519141481432, -0.4465006364167342645, -1.966305148836451577 ) ) ;
#101452 = CARTESIAN_POINT ( 'NONE',  ( -3.755245360860919757, 7.324943987738961049, -0.7216878364870257245 ) ) ;
#101453 = CARTESIAN_POINT ( 'NONE',  ( -1.402160292154681736E-14, 2.259375000341416140, -1.575800808251660134 ) ) ;
#101454 = CARTESIAN_POINT ( 'NONE',  ( 4.594558193676899549, 8.374302254291812631, 0.02480325318809234458 ) ) ;
#101455 = CARTESIAN_POINT ( 'NONE',  ( -1.500000000000015099, 9.229166666666667851, -0.8660254037844309360 ) ) ;
#101456 = CARTESIAN_POINT ( 'NONE',  ( 4.178129962880992920, -0.9906059873891288614, 1.411843326160647782 ) ) ;
#101457 = CARTESIAN_POINT ( 'NONE',  ( 6.861835142292135536, 9.098836647464588978, 1.443375672974065660 ) ) ;
#101458 = EDGE_CURVE ( 'NONE', #164652, #81936, #165098, .T. ) ;
#101459 = CARTESIAN_POINT ( 'NONE',  ( 1.633702333402654361, 0.8778187100713531477, -1.536624053347920071 ) ) ;
#101460 = VECTOR ( 'NONE', #135222, 1000.000000000000000 ) ;
#101461 = CARTESIAN_POINT ( 'NONE',  ( 5.227635310461984375, -2.096914331502324647, 0.6878394029543041244 ) ) ;
#101462 = AXIS2_PLACEMENT_3D ( 'NONE', #133243, #199248, #45221 ) ;
#101463 = ORIENTED_EDGE ( 'NONE', *, *, #184050, .T. ) ;
#101464 = CARTESIAN_POINT ( 'NONE',  ( -5.478376588373717659, 8.549133898814758936, -1.199719254218452047 ) ) ;
#101465 = CARTESIAN_POINT ( 'NONE',  ( 4.745720352911135365, 1.994069623535676961, -0.2986464557954356946 ) ) ;
#101467 = ORIENTED_EDGE ( 'NONE', *, *, #165594, .T. ) ;
#101466 = CARTESIAN_POINT ( 'NONE',  ( 4.728658910183288988, 1.244086218232887120, -1.317109676944823393 ) ) ;
#101468 = CARTESIAN_POINT ( 'NONE',  ( 3.028041890241763401, 1.040506211802554981, -1.554362669439563360 ) ) ;
#101469 = CARTESIAN_POINT ( 'NONE',  ( 6.639283661800273961, -1.628176093627232479, 0.8261057939347238310 ) ) ;
#101470 = CARTESIAN_POINT ( 'NONE',  ( 1.652457426684301955, 1.892030339952909035, 0.2773405859870237133 ) ) ;
#101471 = CARTESIAN_POINT ( 'NONE',  ( -6.199677282185614757, 6.647997080169443684, 0.6295152255529173901 ) ) ;
#101472 = CARTESIAN_POINT ( 'NONE',  ( -10.96415609372974131, 4.387140345944800401, -6.371816014364277692 ) ) ;
#101473 = CARTESIAN_POINT ( 'NONE',  ( 10.99943592164172657, -9.999999999999994671, -0.1113975120798811613 ) ) ;
#101474 = EDGE_CURVE ( 'NONE', #130628, #31895, #13499, .T. ) ;
#101475 = CARTESIAN_POINT ( 'NONE',  ( 0.6823417656249917140, 4.155208333674755394, 1.181850606188765695 ) ) ;
#101476 = CARTESIAN_POINT ( 'NONE',  ( 0.5098338327763075606, -0.6861045072398126443, 1.785269576063217345 ) ) ;
#101477 = CARTESIAN_POINT ( 'NONE',  ( 6.387299765813869712, 6.624473612970537495, 0.000000000000000000 ) ) ;
#101478 = CARTESIAN_POINT ( 'NONE',  ( 1.346068015636435522, -0.8851805579040676886, 1.750911360861057142 ) ) ;
#101479 = ADVANCED_FACE ( 'NONE', ( #159492 ), #152560, .T. ) ;
#101480 = FACE_OUTER_BOUND ( 'NONE', #173876, .T. ) ;
#101481 = CARTESIAN_POINT ( 'NONE',  ( -5.483346782084204563, 5.361935765378481378, 0.000000000000000000 ) ) ;
#101482 = CARTESIAN_POINT ( 'NONE',  ( 4.887034483293543730, -1.997634423138573867, -0.7120497732875651353 ) ) ;
#101484 = CARTESIAN_POINT ( 'NONE',  ( 1.004302930252164871E-16, 4.400000000000001243, 1.500000000000000222 ) ) ;
#101483 = CARTESIAN_POINT ( 'NONE',  ( 8.398386088661320414, 11.88553530582519357, -1.199719254218446718 ) ) ;
#101485 = CARTESIAN_POINT ( 'NONE',  ( 6.678986255646885972, -0.09454399199107686724, -1.969188304806670287 ) ) ;
#101486 = CARTESIAN_POINT ( 'NONE',  ( 1.364683531249990311, 2.634375000341422801, 1.214306433183764966E-14 ) ) ;
#101487 = CARTESIAN_POINT ( 'NONE',  ( 1.371341259694250247, -1.728764894987804057, -1.031425992479652720 ) ) ;
#101488 = VERTEX_POINT ( 'NONE', #117995 ) ;
#101490 = CARTESIAN_POINT ( 'NONE',  ( 0.6853559850922884555, 1.733544695350475395, 1.215283626663875793 ) ) ;
#101489 = CARTESIAN_POINT ( 'NONE',  ( -8.242994207428740339, 9.679543332497402730, 1.082531754730558626 ) ) ;
#101491 = CARTESIAN_POINT ( 'NONE',  ( 9.977304178207173635, 9.828474135482244023, 6.693966201985774411 ) ) ;
#101492 = CARTESIAN_POINT ( 'NONE',  ( 2.893098739488662030, 0.2508700648995808025, 2.055025655848155886 ) ) ;
#101493 = CARTESIAN_POINT ( 'NONE',  ( 3.555981428534177091, 7.370671776590375757, 0.7998128361456271485 ) ) ;
#101494 = CARTESIAN_POINT ( 'NONE',  ( 3.562760505341037831, 7.378580699531681830, -1.734723475976807094E-15 ) ) ;
#101495 = EDGE_LOOP ( 'NONE', ( #48914, #206194, #111320, #39595, #195132, #124836 ) ) ;
#101497 = CARTESIAN_POINT ( 'NONE',  ( 5.542585869888291938, 5.360771691158120689, -0.7998128361456211532 ) ) ;
#101496 = CARTESIAN_POINT ( 'NONE',  ( 4.664062431145298504, -1.365975323770602268, 1.582769587995744853 ) ) ;
#101500 = ORIENTED_EDGE ( 'NONE', *, *, #147855, .T. ) ;
#101499 = CARTESIAN_POINT ( 'NONE',  ( 2.912559398657811549, -0.5280806737378342941, -1.732764662445994919 ) ) ;
#101498 = CARTESIAN_POINT ( 'NONE',  ( 3.153144192703428939, -1.491587519860730238, -1.052284964708279258 ) ) ;
#101501 = CARTESIAN_POINT ( 'NONE',  ( 9.083072846151447166, 12.68433652289702884, 1.199719254218450271 ) ) ;
#101502 = LINE ( 'NONE', #151334, #168349 ) ;
#101503 = CARTESIAN_POINT ( 'NONE',  ( 9.273181387935053976, 13.51005744372143091, 6.801679163151792551 ) ) ;
#101504 = CARTESIAN_POINT ( 'NONE',  ( 5.087059579022827904, -0.2656672225294122169, -2.190654145894948890 ) ) ;
#101505 = CARTESIAN_POINT ( 'NONE',  ( 1.364683531249997417, 9.796875000341396245, 2.602085213965210642E-15 ) ) ;
#101506 = ORIENTED_EDGE ( 'NONE', *, *, #140892, .F. ) ;
#101507 = CARTESIAN_POINT ( 'NONE',  ( 3.773993364719562926, 1.897484654492180400, -0.2369724479281897500 ) ) ;
#101508 = CARTESIAN_POINT ( 'NONE',  ( -4.783329267523015460, 4.474972321731942593, -0.7998128361456221525 ) ) ;
#101509 = CARTESIAN_POINT ( 'NONE',  ( 8.782984583554449998, 9.141236857102018831, 1.040834085586084257E-14 ) ) ;
#101510 = CARTESIAN_POINT ( 'NONE',  ( -0.6801582343750282034, 0.4635416670080716450, 1.178068619123793015 ) ) ;
#101511 = CARTESIAN_POINT ( 'NONE',  ( 5.138177029454852551, 5.096887410559856946, 0.7216878364870317197 ) ) ;
#101512 = CARTESIAN_POINT ( 'NONE',  ( -11.86145016429273014, 13.40000000000000036, -1.100000000000002087 ) ) ;
#101513 = CARTESIAN_POINT ( 'NONE',  ( 7.129428853186368542, 14.53091783984007357, -9.655670968535163823 ) ) ;
#101514 = DIRECTION ( 'NONE',  ( 0.7927788072560210120, 0.000000000000000000, 0.6095094443613819912 ) ) ;
#101515 = CARTESIAN_POINT ( 'NONE',  ( -6.830415307812264025, -7.473374494058229622, -6.717278222822378630 ) ) ;
#101516 = CARTESIAN_POINT ( 'NONE',  ( 3.532352470753961082, 1.824241569866682289, 0.4128566369710484629 ) ) ;
#101517 = CARTESIAN_POINT ( 'NONE',  ( 11.81905481421901705, 11.25735655617266673, -1.592167362352180149 ) ) ;
#101518 = CARTESIAN_POINT ( 'NONE',  ( -0.2409995289980038091, 6.947781193150415646, -2.595509233728268583 ) ) ;
#101519 = CIRCLE ( 'NONE', #63498, 3.000000000000010214 ) ;
#101520 = AXIS2_PLACEMENT_3D ( 'NONE', #40349, #174628, #39264 ) ;
#101521 = CARTESIAN_POINT ( 'NONE',  ( -6.182154858151506893, 9.195969186943299789, 1.082531754730548412 ) ) ;
#101522 = CARTESIAN_POINT ( 'NONE',  ( 6.411931881972196610E-05, -0.8997486769052507327, 1.687471195204979457 ) ) ;
#101523 = CARTESIAN_POINT ( 'NONE',  ( 5.820528018968444961, 5.685037531751635953, 0.7998128361456341429 ) ) ;
#101524 = CARTESIAN_POINT ( 'NONE',  ( 0.3034763168169403169, -1.518637222489120919, -1.253724199518479354 ) ) ;
#101525 = CARTESIAN_POINT ( 'NONE',  ( 1.001577623981730891, -1.966640429010723112, 0.4445266750975271353 ) ) ;
#101526 = AXIS2_PLACEMENT_3D ( 'NONE', #58550, #210110, #160317 ) ;
#101527 = CARTESIAN_POINT ( 'NONE',  ( -8.350932551013499960, 11.83017284523606172, -1.199719254218446718 ) ) ;
#101528 = CARTESIAN_POINT ( 'NONE',  ( 4.830447868218803897, 8.857549289555754157, -0.7998128361456481317 ) ) ;
#101529 =( LENGTH_UNIT ( ) NAMED_UNIT ( * ) SI_UNIT ( .MILLI., .METRE. ) );
#101530 = CARTESIAN_POINT ( 'NONE',  ( 1.500213180713722450, -0.7911926984936793472, -2.043816727864488314 ) ) ;
#101531 = CARTESIAN_POINT ( 'NONE',  ( -15.75000000000000000, 10.19999999999999929, 0.6999999999999992895 ) ) ;
#101532 = CARTESIAN_POINT ( 'NONE',  ( -4.308793891044708779, 3.921347715840572956, 1.214306433183764966E-14 ) ) ;
#101533 = CARTESIAN_POINT ( 'NONE',  ( 5.885648082108200896, 6.039213315313952002, 0.7216878364870328300 ) ) ;
#101534 = CARTESIAN_POINT ( 'NONE',  ( 8.503988664269582998, 10.94440607977979063, 1.599625672291281386 ) ) ;
#101535 = AXIS2_PLACEMENT_3D ( 'NONE', #108755, #159569, #90311 ) ;
#101536 = CARTESIAN_POINT ( 'NONE',  ( 3.623053363349855172, 5.249981562040033189, 1.599625672291267398 ) ) ;
#101537 = CARTESIAN_POINT ( 'NONE',  ( 7.512626515748109135, 8.897724035528543851, 1.082531754730549967 ) ) ;
#101538 = ORIENTED_EDGE ( 'NONE', *, *, #42750, .F. ) ;
#101540 = CARTESIAN_POINT ( 'NONE',  ( 0.5572895418005788803, -1.725428541193659182, 1.036833936551822655 ) ) ;
#101539 = CARTESIAN_POINT ( 'NONE',  ( 3.667381569930192597, 1.025862638139760419, 1.528780434079744843 ) ) ;
#101541 = CARTESIAN_POINT ( 'NONE',  ( 3.111036021816812713, 0.8295677418227834776, -2.143598788741421401 ) ) ;
#101543 = CARTESIAN_POINT ( 'NONE',  ( 0.7954780101973528694, -1.310620071111982421, -1.321417528198569613 ) ) ;
#101542 = CARTESIAN_POINT ( 'NONE',  ( 4.216222584169931231, 4.021273891060765493, 1.214306433183764966E-14 ) ) ;
#101544 = CARTESIAN_POINT ( 'NONE',  ( 1.642778471875000035, -3.376041666188708046, -2.845375778867859751 ) ) ;
#101545 = CARTESIAN_POINT ( 'NONE',  ( -5.590039407536138150, 5.416134151747256986, 0.000000000000000000 ) ) ;
#101546 = CARTESIAN_POINT ( 'NONE',  ( 4.394721148579957770, -1.856311205515799312, -0.4593126252911489127 ) ) ;
#101548 = CARTESIAN_POINT ( 'NONE',  ( -7.974166903131914452, 12.45494515362926435, -0.7998128361456281477 ) ) ;
#101547 = B_SPLINE_CURVE_WITH_KNOTS ( 'NONE', 3,
 ( #173162, #208815, #24743, #123424 ),
 .UNSPECIFIED., .F., .F.,
 ( 4, 4 ),
 ( 0.000000000000000000, 0.0005936488266206346861 ),
 .UNSPECIFIED. ) ;
#101549 = CARTESIAN_POINT ( 'NONE',  ( 6.396603524444617328, 6.809554808131969672, -0.5206029305389828776 ) ) ;
#101550 = CARTESIAN_POINT ( 'NONE',  ( -5.966997003790221576, 9.015228033513643879, -1.082531754730549967 ) ) ;
#101552 = CARTESIAN_POINT ( 'NONE',  ( 1.938157646728836614, 1.849873822469105145, 0.2772664081076986475 ) ) ;
#101551 = CARTESIAN_POINT ( 'NONE',  ( 3.755486520148888729, 2.074727465276064997, -0.2578676962887976321 ) ) ;
#101553 = CARTESIAN_POINT ( 'NONE',  ( 6.127922243696800386, 10.09306701771420656, -0.7216878364870267237 ) ) ;
#101554 = CARTESIAN_POINT ( 'NONE',  ( -6.773376349083143566, -7.473374494058229622, -6.661184041420940005 ) ) ;
#101555 = CARTESIAN_POINT ( 'NONE',  ( 2.770765728838171960, 1.651868531079144553, -0.5482889651245922424 ) ) ;
#101556 = CARTESIAN_POINT ( 'NONE',  ( 4.521807925357579805, 5.234196320127330715, -1.199719254218452047 ) ) ;
#101558 = CARTESIAN_POINT ( 'NONE',  ( 4.599240423533799138, 6.388866465587984322, 1.599625672291267398 ) ) ;
#101557 = DIRECTION ( 'NONE',  ( -0.000000000000000000, -1.000000000000000000, -0.000000000000000000 ) ) ;
#101559 = CARTESIAN_POINT ( 'NONE',  ( 4.125434265850294047, -1.649698657028845883, 0.5036723037128154612 ) ) ;
#101560 = CARTESIAN_POINT ( 'NONE',  ( -6.028571859570855729, 10.18508426947466816, 0.000000000000000000 ) ) ;
#101561 = CARTESIAN_POINT ( 'NONE',  ( 6.129534211984397629, -2.079372889712034489, 0.7396383780838566846 ) ) ;
#101562 = DIRECTION ( 'NONE',  ( 0.000000000000000000, 0.000000000000000000, -1.000000000000000000 ) ) ;
#101563 = PRESENTATION_STYLE_ASSIGNMENT (( #117880 ) ) ;
#101564 = CARTESIAN_POINT ( 'NONE',  ( 3.801787986034934619, -1.640574847700679628, -1.422045332411596474 ) ) ;
#101565 = CARTESIAN_POINT ( 'NONE',  ( 2.121465551170404140, -1.771062468586531047, 0.4427346646293239818 ) ) ;
#101566 = CARTESIAN_POINT ( 'NONE',  ( 0.4440980561614648603, -0.9299495107331550159, 1.727370323332158897 ) ) ;
#101567 = CARTESIAN_POINT ( 'NONE',  ( 5.682842148387160286, 1.729519065878544426, -1.221158300678204300 ) ) ;
#101568 = ORIENTED_EDGE ( 'NONE', *, *, #112518, .F. ) ;
#101570 = CARTESIAN_POINT ( 'NONE',  ( -0.6823417656250212460, 2.863541667008084879, 1.181850606188767472 ) ) ;
#101569 = CARTESIAN_POINT ( 'NONE',  ( 6.128533286225700039, 0.2205342988230532264, 2.281768524910554596 ) ) ;
#101571 = CARTESIAN_POINT ( 'NONE',  ( 4.241003122976366058, 3.842258486427521103, -0.7998128361456211532 ) ) ;
#101572 = CARTESIAN_POINT ( 'NONE',  ( 1.735180256192244919, 1.979698633766859395, 0.7602586827493148514 ) ) ;
#101573 = CARTESIAN_POINT ( 'NONE',  ( -4.555176424511596878, 7.297827681030051750, 1.082531754730560403 ) ) ;
#101574 = CARTESIAN_POINT ( 'NONE',  ( 3.877268743828276243, 4.586196958296845594, 1.082531754730560403 ) ) ;
#101575 = CARTESIAN_POINT ( 'NONE',  ( -5.002595493318215070, 7.819816594637776674, 1.082531754730560403 ) ) ;
#101577 = CARTESIAN_POINT ( 'NONE',  ( -1.500000000000001110, 13.05208333401612997, 0.8660254037844419273 ) ) ;
#101576 = CARTESIAN_POINT ( 'NONE',  ( 6.883263157960367806, 6.035304072343574688, 2.648703854151325032 ) ) ;
#101579 = ORIENTED_EDGE ( 'NONE', *, *, #212713, .T. ) ;
#101578 = CARTESIAN_POINT ( 'NONE',  ( 1.225557454335997054, 1.961257301181002388, 1.042886780478131215 ) ) ;
#101580 = CARTESIAN_POINT ( 'NONE',  ( 6.117814597332064785, 0.2004318333163370436, 2.006446488866588496 ) ) ;
#101582 = CARTESIAN_POINT ( 'NONE',  ( 3.924720150778399752, -1.388762634255924500, 1.525101558930273660 ) ) ;
#101581 = CARTESIAN_POINT ( 'NONE',  ( 4.684505768721569652, 5.424010470718658716, -1.199719254218452047 ) ) ;
#101584 = CARTESIAN_POINT ( 'NONE',  ( 1.737500000000001155, -3.733333333333331616, 3.009438278150922130 ) ) ;
#101583 = CARTESIAN_POINT ( 'NONE',  ( 5.668190738965027897, 8.770583741171307679, -1.199719254218452047 ) ) ;
#101585 = CARTESIAN_POINT ( 'NONE',  ( 7.147083253059300922, 8.367293879104554577, 1.199719254218452935 ) ) ;
#101586 = CARTESIAN_POINT ( 'NONE',  ( 0.000000000000000000, -1.596874999522041705, -3.793834371823813001 ) ) ;
#101587 = CARTESIAN_POINT ( 'NONE',  ( -1.500000000000001110, 12.77083333333333215, 0.8660254037844418162 ) ) ;
#101588 = CARTESIAN_POINT ( 'NONE',  ( 0.8321122680391360715, 2.060015930055682620, 0.3555243805062404117 ) ) ;
#101589 = CARTESIAN_POINT ( 'NONE',  ( 4.746720300533005421, 1.994071680685698400, -0.2986252114312442640 ) ) ;
#101590 = CARTESIAN_POINT ( 'NONE',  ( 4.774869596704574448, 1.716175909155163382, -0.6674964387535023969 ) ) ;
#101591 = CARTESIAN_POINT ( 'NONE',  ( 6.063521013809720195, 8.097193820909906137, 1.599625672291281386 ) ) ;
#101592 = CARTESIAN_POINT ( 'NONE',  ( 0.5512174377280190107, 0.5480947683692177774, -1.635447244754190788 ) ) ;
#101593 = CARTESIAN_POINT ( 'NONE',  ( 0.2687680251878405424, -0.2516378192510167477, -2.000730910237565663 ) ) ;
#101594 = CARTESIAN_POINT ( 'NONE',  ( 1.301886090224623205, 1.538925899722990431, -1.707713671238730635 ) ) ;
#101595 = CARTESIAN_POINT ( 'NONE',  ( -6.762819695118240659, 6.784377820593065600, 0.7998128361456341429 ) ) ;
#101596 = CARTESIAN_POINT ( 'NONE',  ( 1.441102657128832121, 0.4411821743415585417, 2.218815533503415871 ) ) ;
#101597 = CARTESIAN_POINT ( 'NONE',  ( 2.877667905955140437, 1.999614821268459020, -0.6613089454029356107 ) ) ;
#101598 = CARTESIAN_POINT ( 'NONE',  ( -5.795184315198522285, 5.725746220678519904, -0.7998128361456362523 ) ) ;
#101599 = CARTESIAN_POINT ( 'NONE',  ( 7.298366762858032430, 7.409182732956175244, 1.040834085586084257E-14 ) ) ;
#101600 = CARTESIAN_POINT ( 'NONE',  ( 5.004368096775565711, 8.852530189631227842, -0.7216878364870458196 ) ) ;
#101601 = CARTESIAN_POINT ( 'NONE',  ( 5.812500000000003553, 1.451031289061346818, 1.451031289060879637 ) ) ;
#101602 = CARTESIAN_POINT ( 'NONE',  ( -6.600121851754250812, 6.594563670001734046, 0.7998128361456341429 ) ) ;
#101603 = CARTESIAN_POINT ( 'NONE',  ( 5.572037945092146671, 8.484166121707415797, -1.082531754730543971 ) ) ;
#101604 = CARTESIAN_POINT ( 'NONE',  ( 4.314144046604536875, 7.442532859859907646, 1.092782195075291396 ) ) ;
#101605 = EDGE_CURVE ( 'NONE', #18526, #80644, #59917, .T. ) ;
#101606 = CARTESIAN_POINT ( 'NONE',  ( -4.436542580169821726, 6.199052314996659874, 1.599625672291267398 ) ) ;
#101607 = CARTESIAN_POINT ( 'NONE',  ( 5.326523995474015116, -0.9991460305027520805, -1.984133879135864920 ) ) ;
#101608 = CARTESIAN_POINT ( 'NONE',  ( 3.943468035136340255, 0.7389761752502190806, -2.063229655756371628 ) ) ;
#101609 = CARTESIAN_POINT ( 'NONE',  ( -4.401593425930945713, 8.286942763561420122, 1.040834085586084257E-14 ) ) ;
#101610 = CARTESIAN_POINT ( 'NONE',  ( -11.89942855770813956, 9.799999999999998934, 0.6999999999999992895 ) ) ;
#101611 = CARTESIAN_POINT ( 'NONE',  ( 4.932062528313536198, 1.127988425013145779, 1.604980062286972542 ) ) ;
#101612 = CIRCLE ( 'NONE', #73948, 0.04999999999999883010 ) ;
#101613 = CARTESIAN_POINT ( 'NONE',  ( -0.6823417656250212460, 2.301041667008084435, 1.181850606188767472 ) ) ;
#101614 = CARTESIAN_POINT ( 'NONE',  ( 6.890000000000005898, 7.052460701731090076, 2.598152593539102551 ) ) ;
#101615 = CARTESIAN_POINT ( 'NONE',  ( -4.229780737783618072, 6.918199379847403740, 1.082531754730560403 ) ) ;
#101616 = CARTESIAN_POINT ( 'NONE',  ( 4.781546299372162245, 0.2051969522943071500, -2.110614603223801122 ) ) ;
#101617 = CARTESIAN_POINT ( 'NONE',  ( -7.932929277771797238, 8.427708043588125975, 0.000000000000000000 ) ) ;
#101618 = ORIENTED_EDGE ( 'NONE', *, *, #184338, .T. ) ;
#101621 = AXIS2_PLACEMENT_3D ( 'NONE', #53472, #19892, #119609 ) ;
#101620 = CARTESIAN_POINT ( 'NONE',  ( 6.174726448494309849, -2.051094451480539149, -0.6828207641706719455 ) ) ;
#101619 = CARTESIAN_POINT ( 'NONE',  ( -6.631346530859867805, 6.909194838857525944, 0.000000000000000000 ) ) ;
#101622 = CARTESIAN_POINT ( 'NONE',  ( 5.301401758143367893, 6.143722458377430584, 1.199719254218462483 ) ) ;
#101623 = CARTESIAN_POINT ( 'NONE',  ( 5.337399561049260832, 0.7408347518493042516, -1.685818907712175019 ) ) ;
#101624 = CARTESIAN_POINT ( 'NONE',  ( -0.6823417656250003738, 2.780208333674753618, -1.181850606188749264 ) ) ;
#101625 = CARTESIAN_POINT ( 'NONE',  ( 1.276469996339978819, 1.608456030955440541, -0.6653204537699786147 ) ) ;
#101627 = EDGE_CURVE ( 'NONE', #199688, #44672, #21127, .T. ) ;
#101626 = CARTESIAN_POINT ( 'NONE',  ( -11.94105721237523277, 19.00000000000000000, -1.187919463087249827 ) ) ;
#101628 = CARTESIAN_POINT ( 'NONE',  ( -0.6823417656250246877, -1.136458332991911790, 1.181850606188755259 ) ) ;
#101629 = CARTESIAN_POINT ( 'NONE',  ( 9.283847064513500058, 11.43438320747982750, -7.606630335864923431 ) ) ;
#101630 = CARTESIAN_POINT ( 'NONE',  ( 5.541917325712655717, 0.8799508658935292216, -1.974686638939105343 ) ) ;
#101631 = ADVANCED_FACE ( 'NONE', ( #202348 ), #170940, .F. ) ;
#101632 = CARTESIAN_POINT ( 'NONE',  ( -3.704402285031864306, 5.344888637335695414, -1.599625672291256295 ) ) ;
#101633 = CARTESIAN_POINT ( 'NONE',  ( -6.182154857707119255, 10.15633840072622363, 0.000000000000000000 ) ) ;
#101634 = CARTESIAN_POINT ( 'NONE',  ( 5.032170685167933755, 1.114402916724830161, -1.852182961850391774 ) ) ;
#101635 = CARTESIAN_POINT ( 'NONE',  ( -1.201851678989727383E-14, 3.071875000341420137, 1.575800808251672791 ) ) ;
#101636 = CARTESIAN_POINT ( 'NONE',  ( 4.833256578820930294, -1.803536663746601709, 0.7962986557112069486 ) ) ;
#101637 = CARTESIAN_POINT ( 'NONE',  ( 4.305767739847966347, -1.508829150093475180, 0.8539562774845139703 ) ) ;
#101638 = B_SPLINE_CURVE_WITH_KNOTS ( 'NONE', 3,
 ( #87836, #133420, #199426, #83555, #184247, #18550 ),
 .UNSPECIFIED., .F., .F.,
 ( 4, 2, 4 ),
 ( 0.000000000000000000, 0.0003767011250903908558, 0.0007534022501807817115 ),
 .UNSPECIFIED. ) ;
#101639 = CARTESIAN_POINT ( 'NONE',  ( 1.382659466718983543, -0.3261178763579902218, -2.167053615394160637 ) ) ;
#101640 = CARTESIAN_POINT ( 'NONE',  ( 2.679136956247138546, -2.208066087050132520, -0.6703273527271095267 ) ) ;
#101641 = CARTESIAN_POINT ( 'NONE',  ( 4.762995170230669650, -1.839058295199582638, -0.9300793793675359300 ) ) ;
#101642 = CARTESIAN_POINT ( 'NONE',  ( 0.1814471035007196309, -0.9164790359779145801, 1.712077929913154328 ) ) ;
#101643 = CARTESIAN_POINT ( 'NONE',  ( -8.161645285302366659, 8.624267042381978499, 1.040834085586084257E-14 ) ) ;
#101644 = CARTESIAN_POINT ( 'NONE',  ( -4.847922445338252118, 7.813604065273374921, -1.199719254218453823 ) ) ;
#101645 = CARTESIAN_POINT ( 'NONE',  ( 11.89942855770814312, 12.30000000000000071, -0.7000000000000009548 ) ) ;
#101646 = SURFACE_SIDE_STYLE ('',( #35565 ) ) ;
#101647 = CARTESIAN_POINT ( 'NONE',  ( 1.442029965644067158, -1.730867108953790590, -1.034163949609874233 ) ) ;
#101648 = CARTESIAN_POINT ( 'NONE',  ( -5.694061327615147050, 9.586895948952255608, 0.000000000000000000 ) ) ;
#101649 = CARTESIAN_POINT ( 'NONE',  ( 3.592985822966657583, -0.4282699184722462693, -2.164648485658649868 ) ) ;
#101650 = CARTESIAN_POINT ( 'NONE',  ( -1.642778471875000035, -2.005208332855376696, -2.845375778867859751 ) ) ;
#101651 = CARTESIAN_POINT ( 'NONE',  ( 1.322862136463611504, -1.679459703857703268, -0.8019484745323454122 ) ) ;
#101652 = CARTESIAN_POINT ( 'NONE',  ( -0.02880301295722555166, 0.6711181056864559125, -2.353869138803561079 ) ) ;
#101653 = LINE ( 'NONE', #18249, #180339 ) ;
#101654 = CARTESIAN_POINT ( 'NONE',  ( 2.300251978943730791, 2.674522988693084358, -2.456405383529883135 ) ) ;
#101656 = CARTESIAN_POINT ( 'NONE',  ( 6.925078400183566352, 7.051505795288234957, 2.842497989238515821 ) ) ;
#101655 = CARTESIAN_POINT ( 'NONE',  ( -5.526470424545159688, 7.552361116859303891, -1.349762019914104272 ) ) ;
#101657 = CARTESIAN_POINT ( 'NONE',  ( 6.105383947169263692, -1.826632712061267094, 0.2301338403083788009 ) ) ;
#101658 = ORIENTED_EDGE ( 'NONE', *, *, #186479, .T. ) ;
#101659 = CARTESIAN_POINT ( 'NONE',  ( 3.028252848896676674, 1.146099369071330143, -1.712595011064410366 ) ) ;
#101660 = CARTESIAN_POINT ( 'NONE',  ( -1.360316468750040642, 2.161458333674780352, 0.7853790794158861388 ) ) ;
#101661 = CARTESIAN_POINT ( 'NONE',  ( -6.501298352952815662, 7.543601818988450169, -1.199719254218446718 ) ) ;
#101662 = CARTESIAN_POINT ( 'NONE',  ( 1.805337931753002501, 1.756199045189226204, -0.9973023101699033388 ) ) ;
#101663 = CARTESIAN_POINT ( 'NONE',  ( 1.499999999999987121, -0.2458333333333099502, 0.8660254037844524744 ) ) ;
#101664 = CARTESIAN_POINT ( 'NONE',  ( 2.849184837166184536, 6.475799410002530898, 0.7998128361456362523 ) ) ;
#101665 = CARTESIAN_POINT ( 'NONE',  ( 2.061468863205512925, 0.3533766173234990093, -2.030202010101101795 ) ) ;
#101667 = CARTESIAN_POINT ( 'NONE',  ( 1.364683531250000303, 13.00520833367473550, -0.7879004041258355073 ) ) ;
#101666 = DIRECTION ( 'NONE',  ( 0.000000000000000000, 0.000000000000000000, 1.000000000000000000 ) ) ;
#101668 = CARTESIAN_POINT ( 'NONE',  ( 6.277588818327314080, 7.282607361925381717, 1.199719254218462483 ) ) ;
#101669 = CARTESIAN_POINT ( 'NONE',  ( -0.1411974294641968053, 0.7397609206469482057, -1.984549174418163808 ) ) ;
#101670 = CARTESIAN_POINT ( 'NONE',  ( 5.795608111622330583, 1.668732747960173235, 1.444295198399044855 ) ) ;
#101671 = CARTESIAN_POINT ( 'NONE',  ( 6.550524494058025837, 7.671308660269694712, -1.199719254218452047 ) ) ;
#101672 = CARTESIAN_POINT ( 'NONE',  ( 1.089409339093825979, 1.906878951332368954, -1.017924135055588541 ) ) ;
#101673 = CARTESIAN_POINT ( 'NONE',  ( -5.585596099150199834, 5.618876325204420930, -0.7216878364870207285 ) ) ;
#101674 = CARTESIAN_POINT ( 'NONE',  ( 1.516814941429758701, 0.2024661778830244008, 2.006371303556075958 ) ) ;
#101675 = SURFACE_STYLE_FILL_AREA ( #117993 ) ;
#101676 = CARTESIAN_POINT ( 'NONE',  ( -0.5987733972867143040, 6.693213315561105325, 3.557617754081424888 ) ) ;
#101677 = CARTESIAN_POINT ( 'NONE',  ( 9.305047017613615523, 3.481540744127370690, 7.450000000000001954 ) ) ;
#101678 = AXIS2_PLACEMENT_3D ( 'NONE', #117114, #99738, #83477 ) ;
#101679 = CARTESIAN_POINT ( 'NONE',  ( 2.236979667955760309, -1.672073921526989748, 0.8388852543278202401 ) ) ;
#101680 = CARTESIAN_POINT ( 'NONE',  ( 3.204314817619222211, 1.275555974797081049, -1.561881975048397209 ) ) ;
#101682 = CARTESIAN_POINT ( 'NONE',  ( -15.75000000000000000, 13.79999999999998295, 3.199999999999997957 ) ) ;
#101681 = CARTESIAN_POINT ( 'NONE',  ( 1.364683531249986537, 1.655208333674748955, -0.7879004041258239610 ) ) ;
#101684 = CARTESIAN_POINT ( 'NONE',  ( 5.479168138989118475, -0.05037515785718051087, -2.105640702651077945 ) ) ;
#101683 = CARTESIAN_POINT ( 'NONE',  ( -8.688077508258798431, 9.030511935923748013, -0.7998128361456291469 ) ) ;
#101685 = COLOUR_RGB ( '', 0.66274510, 0.83137255, 0.94901961) ;
#101686 = CARTESIAN_POINT ( 'NONE',  ( 6.337546739384100292, 9.481222731668410120, 1.199719254218460707 ) ) ;
#101687 = CARTESIAN_POINT ( 'NONE',  ( -6.042130013184518589, 10.20090211535728031, -0.7998128361456291469 ) ) ;
#101688 = CARTESIAN_POINT ( 'NONE',  ( 6.539320575229276677, 6.035451701470580410, 2.698157228745074576 ) ) ;
#101689 = CARTESIAN_POINT ( 'NONE',  ( 5.449475261934634496, -1.824267568868439771, 0.8672911397697125047 ) ) ;
#101690 = CARTESIAN_POINT ( 'NONE',  ( 0.6823417656249917140, 5.592708333674749177, 1.181850606188765695 ) ) ;
#101691 = CARTESIAN_POINT ( 'NONE',  ( 0.5849265108320426121, 1.972682758258193392, 0.6021488627185996867 ) ) ;
#101692 = CARTESIAN_POINT ( 'NONE',  ( 7.131225611108079399, 11.26358761302737754, 0.7216878364870438212 ) ) ;
#101693 = EDGE_CURVE ( 'NONE', #31452, #157630, #175475, .T. ) ;
#101694 = CARTESIAN_POINT ( 'NONE',  ( 6.692885107001518286, 7.837396042037102717, -1.199719254218452047 ) ) ;
#101695 = CARTESIAN_POINT ( 'NONE',  ( 4.199993725183334803, 8.122019456014369254, -0.7998128361456362523 ) ) ;
#101696 = CARTESIAN_POINT ( 'NONE',  ( -1.364683531250014514, 0.05104166700808546175, -0.7879004041258359514 ) ) ;
#101698 = DIRECTION ( 'NONE',  ( 0.000000000000000000, 0.000000000000000000, 1.000000000000000000 ) ) ;
#101697 = CARTESIAN_POINT ( 'NONE',  ( 6.364626766972446781, 6.390095747748157251, 0.7998128361456352531 ) ) ;
#101699 = CARTESIAN_POINT ( 'NONE',  ( 8.568389893712330618, 9.098802418860289620, 1.040834085586084257E-14 ) ) ;
#101700 = CARTESIAN_POINT ( 'NONE',  ( 3.649033395009869452, -0.4203537998966280220, -2.129940419224036763 ) ) ;
#101702 = CARTESIAN_POINT ( 'NONE',  ( 1.944624168438695566, -1.479605912621816621, -1.095697124569312564 ) ) ;
#101701 = CARTESIAN_POINT ( 'NONE',  ( -4.690757960648240577, 6.495636925554817864, 1.443375672974064550 ) ) ;
#101703 = CARTESIAN_POINT ( 'NONE',  ( 1.364683531249988535, 3.905208333674751842, -0.7879004041258239610 ) ) ;
#101704 = CARTESIAN_POINT ( 'NONE',  ( 3.913774547416096095, -1.127657808996849198, -1.879056921112078893 ) ) ;
#101705 = CARTESIAN_POINT ( 'NONE',  ( 6.983263157960330147, 7.051826758666251749, 2.751962080009969114 ) ) ;
#101706 = CARTESIAN_POINT ( 'NONE',  ( 5.331070463540595661, 0.1608317336210095816, 2.256856606938316023 ) ) ;
#101707 = CARTESIAN_POINT ( 'NONE',  ( -5.856232286098998152, 8.919689202835742847, 1.199719254218452047 ) ) ;
#101708 = CARTESIAN_POINT ( 'NONE',  ( 9.499668754385636404, 7.849261790823902629, 0.07933194154488391880 ) ) ;
#101709 = CARTESIAN_POINT ( 'NONE',  ( 4.745935331938881951, 8.308991367555595531, -0.7587592799198628057 ) ) ;
#101710 = CARTESIAN_POINT ( 'NONE',  ( -7.078765599666485997, 7.431183752465250869, 0.000000000000000000 ) ) ;
#101711 = CARTESIAN_POINT ( 'NONE',  ( 3.445180431648313224, 7.033477913649446300, 0.7216878364870257245 ) ) ;
#101712 =( BOUNDED_CURVE ( )  B_SPLINE_CURVE ( 2, ( #77438, #209549, #172825, #128422, #194389, #66483, #111075, #177081, #31906 ),
 .UNSPECIFIED., .F., .T. ) 
 B_SPLINE_CURVE_WITH_KNOTS ( ( 3, 2, 2, 2, 3 ),
 ( 0.04687499999999993755, 0.05208333333333333565, 0.06250000000000000000, 0.07291666666666667129, 0.07812500000000022204 ),
 .UNSPECIFIED. ) 
 CURVE ( )  GEOMETRIC_REPRESENTATION_ITEM ( )  RATIONAL_B_SPLINE_CURVE ( ( 0.9330127018922192983, 0.9330127018922185211, 1.000000000000000000, 0.8660254037844387076, 1.000000000000000000, 0.8660254037844387076, 1.000000000000000000, 0.9330127018922165227, 0.9330127018922194093 ) ) 
 REPRESENTATION_ITEM ( '' )  );
#101713 = EDGE_CURVE ( 'NONE', #181174, #112981, #96011, .T. ) ;
#101714 = CARTESIAN_POINT ( 'NONE',  ( 6.643818817254954823, 0.6745290893846628277, -1.636350436104140327 ) ) ;
#101715 = CARTESIAN_POINT ( 'NONE',  ( 3.299479658734363330, 1.818928663852859451, -0.8628815382619985375 ) ) ;
#101716 = CARTESIAN_POINT ( 'NONE',  ( 8.444030743212801227, 8.745790710036752458, 0.7998128361456462443 ) ) ;
#101717 = CARTESIAN_POINT ( 'NONE',  ( 1.782391780347460486, -1.127077160282144552, 1.778786634185139270 ) ) ;
#101718 = CARTESIAN_POINT ( 'NONE',  ( 1.370553398973891390, -0.2825970708170088552, -1.894525755544463008 ) ) ;
#101720 = CARTESIAN_POINT ( 'NONE',  ( 0.7499999999999902300, 2.483333333333351156, 1.299038105676669330 ) ) ;
#101719 = CARTESIAN_POINT ( 'NONE',  ( -1.364683531250000748, 12.60937500034139980, 0.000000000000000000 ) ) ;
#101721 = CARTESIAN_POINT ( 'NONE',  ( 1.785543415971390102, -1.855581397249297382, 0.6606886831301524987 ) ) ;
#101722 = CARTESIAN_POINT ( 'NONE',  ( 0.5845639792326964290, -0.2246964894469481722, -1.857040431621145959 ) ) ;
#101723 = CARTESIAN_POINT ( 'NONE',  ( 1.539427311113782837, 1.813978416018032558, -0.7477436361984082236 ) ) ;
#101725 = ORIENTED_EDGE ( 'NONE', *, *, #109311, .F. ) ;
#101724 = CARTESIAN_POINT ( 'NONE',  ( 0.4570967503451648373, -1.639016809899789040, 0.9851245988263114262 ) ) ;
#101726 = CARTESIAN_POINT ( 'NONE',  ( 6.643132081016124069, 7.813037518349371879, 1.082531754730558626 ) ) ;
#101727 = CARTESIAN_POINT ( 'NONE',  ( -1.402160292154681736E-14, 0.3843750003414230232, 1.575800808251672791 ) ) ;
#101728 = CARTESIAN_POINT ( 'NONE',  ( 6.051601594667257444, 0.5412791183288803154, -1.790613848972313349 ) ) ;
#101729 = CARTESIAN_POINT ( 'NONE',  ( 8.920375002787457319, 12.49452237230570084, 1.199719254218450271 ) ) ;
#101730 = CARTESIAN_POINT ( 'NONE',  ( 6.983263157960403866, -0.005959781318053494932, 2.045923054782183392 ) ) ;
#101731 = CARTESIAN_POINT ( 'NONE',  ( 6.086797785588474063, 1.993605056338519699, 0.5577928598018768724 ) ) ;
#101732 = CARTESIAN_POINT ( 'NONE',  ( 10.30923643716952576, 0.9706168436483885165, 5.952040432139194870 ) ) ;
#101733 = CARTESIAN_POINT ( 'NONE',  ( -3.485854892044994102, 7.080931450778859215, -0.7216878364870458196 ) ) ;
#101735 =( NAMED_UNIT ( * ) SI_UNIT ( $, .STERADIAN. ) SOLID_ANGLE_UNIT ( ) );
#101734 = AXIS2_PLACEMENT_3D ( 'NONE', #77703, #207702, #143823 ) ;
#101736 = CARTESIAN_POINT ( 'NONE',  ( -1.500000000000001332, 0.6500000000000255573, 0.000000000000000000 ) ) ;
#101737 = CARTESIAN_POINT ( 'NONE',  ( 6.591235234537977661, 10.84152487360300299, 0.7998128361456462443 ) ) ;
#101738 = CARTESIAN_POINT ( 'NONE',  ( -7.967387826325084355, 12.44703623068796361, 0.7998128361456481317 ) ) ;
#101739 = CARTESIAN_POINT ( 'NONE',  ( 5.505492895601038938, 8.580769590579979678, -1.199719254218452047 ) ) ;
#101740 = EDGE_CURVE ( 'NONE', #63230, #53115, #70247, .T. ) ;
#101741 = CARTESIAN_POINT ( 'NONE',  ( 1.364683531249986537, 1.155208333674754728, -0.7879004041258239610 ) ) ;
#101742 = CARTESIAN_POINT ( 'NONE',  ( -1.500000000000011324, 2.670833333333352044, 0.8660254037844403729 ) ) ;
#101744 = CARTESIAN_POINT ( 'NONE',  ( 5.671388329218120639, 5.511041227042920099, 1.040834085586084257E-14 ) ) ;
#101743 = CARTESIAN_POINT ( 'NONE',  ( 5.002378505967388200, 1.956489882415031190, 0.1462272935644214900 ) ) ;
#101745 = EDGE_CURVE ( 'NONE', #37534, #61789, #109099, .T. ) ;
#101746 = CARTESIAN_POINT ( 'NONE',  ( 3.620470095612156047, 0.4925664443866035191, -1.954873191151076162 ) ) ;
#101747 = CARTESIAN_POINT ( 'NONE',  ( 2.975699994382564828, -0.7717752754876210375, 1.753554302899827277 ) ) ;
#101748 = CARTESIAN_POINT ( 'NONE',  ( -1.913201741516678434, 3.249623237789960761, -0.4478572873796636822 ) ) ;
#101749 = CARTESIAN_POINT ( 'NONE',  ( 0.3807642395799658575, -0.2741851280289032688, -2.174293136291181483 ) ) ;
#101750 = CARTESIAN_POINT ( 'NONE',  ( 0.1333692844072559280, 0.001398348041498076455, -2.053671342968105051 ) ) ;
#101751 = CARTESIAN_POINT ( 'NONE',  ( 3.374138713240721454, -1.116850685118627728, 1.500355210514233262 ) ) ;
#101752 = CARTESIAN_POINT ( 'NONE',  ( -1.500000000000015099, -0.7979166659838445863, 0.8660254037844403729 ) ) ;
#101753 = CARTESIAN_POINT ( 'NONE',  ( -6.333630315878337136, 10.54098580183340772, 0.000000000000000000 ) ) ;
#101755 = CARTESIAN_POINT ( 'NONE',  ( 4.851218673320928154, 0.2063579389092398131, -2.107127644889031703 ) ) ;
#101754 = CARTESIAN_POINT ( 'NONE',  ( -4.256897045010916258, 7.910204285913967404, 0.7216878364870317197 ) ) ;
#101756 = CARTESIAN_POINT ( 'NONE',  ( 0.000000000000000000, 0.08000000000000020983, -2.000000000000000000 ) ) ;
#101757 = CARTESIAN_POINT ( 'NONE',  ( 5.494608840674215955, 2.039112051642687717, 0.3575134270455831986 ) ) ;
#101758 = CARTESIAN_POINT ( 'NONE',  ( 0.8200051061889235271, 1.242435332701301132, -1.681397122352365603 ) ) ;
#101760 = ORIENTED_EDGE ( 'NONE', *, *, #203182, .T. ) ;
#101759 = CARTESIAN_POINT ( 'NONE',  ( 5.983392046985362533, 1.685759371660649375, -0.7011634845648377912 ) ) ;
#101761 = B_SPLINE_CURVE_WITH_KNOTS ( 'NONE', 3,
 ( #113625, #14956, #30172, #161244, #96261, #78905, #195874 ),
 .UNSPECIFIED., .F., .F.,
 ( 4, 3, 4 ),
 ( 3.315837474970529026E-05, 0.0009000000035470258212, 0.001929259801299062485 ),
 .UNSPECIFIED. ) ;
#101762 = CARTESIAN_POINT ( 'NONE',  ( 6.252281394196331554, 10.44607872653774372, 1.040834085586084257E-14 ) ) ;
#101763 = CARTESIAN_POINT ( 'NONE',  ( -0.07933194151890057833, -9.902237888914269703, -9.499668754386311420 ) ) ;
#101764 = CARTESIAN_POINT ( 'NONE',  ( -9.970593900173907898, 5.552053933461305490, 5.997145116287158295 ) ) ;
#101765 = CARTESIAN_POINT ( 'NONE',  ( 5.951666246274784910, 9.887435020721849099, 0.7216878364870438212 ) ) ;
#101766 = CARTESIAN_POINT ( 'NONE',  ( -1.904329973710278789, 3.286760881231344467, 0.4119279214152820612 ) ) ;
#101768 = CARTESIAN_POINT ( 'NONE',  ( 0.1701768659465550948, 0.6913354060617262764, 1.674562877054022625 ) ) ;
#101767 = CARTESIAN_POINT ( 'NONE',  ( 5.806634928402749196, 9.996434193103704402, -0.7998128361456481317 ) ) ;
#101769 = CARTESIAN_POINT ( 'NONE',  ( -6.482770005628665011, 10.71498210654212002, 0.7998128361456481317 ) ) ;
#101770 = CARTESIAN_POINT ( 'NONE',  ( 4.517891501851804215, 6.293959390292322986, -1.599625672291255185 ) ) ;
#101771 = CARTESIAN_POINT ( 'NONE',  ( -5.171754443046126859, 7.767122556988016235, 1.178735681042131667 ) ) ;
#101772 = CARTESIAN_POINT ( 'NONE',  ( 6.984385409695311964, 8.177479728513226576, 1.199719254218452935 ) ) ;
#101773 = CARTESIAN_POINT ( 'NONE',  ( -7.228805602686602327, -7.003075417673644054, -7.884707905546937567 ) ) ;
#101774 = CARTESIAN_POINT ( 'NONE',  ( -11.48243876534946040, 11.29999999999998117, 3.199999999999997957 ) ) ;
#101775 = CARTESIAN_POINT ( 'NONE',  ( 10.24960094225127172, 11.06021530882240356, -0.7216878364870257245 ) ) ;
#101776 = ORIENTED_EDGE ( 'NONE', *, *, #46152, .T. ) ;
#101777 = CARTESIAN_POINT ( 'NONE',  ( 5.800407700000974387, 1.352143934286989868, -1.496062775417882129 ) ) ;
#101778 = CARTESIAN_POINT ( 'NONE',  ( 0.1004478525090373164, -0.9956121213324088393, 1.872212410442177566 ) ) ;
#101779 = CARTESIAN_POINT ( 'NONE',  ( 10.96314634606097016, -7.723163831703883986, -0.5532327639488858750 ) ) ;
#101780 = EDGE_CURVE ( 'NONE', #212421, #191425, #123606, .T. ) ;
#101781 = CLOSED_SHELL ( 'NONE', ( #148919, #189311, #90966, #39481, #57658, #36169, #206348, #182303, #116512, #26308, #120033, #32992, #24949, #34930, #53647, #96650, #157529, #95724, #143463, #27472, #16348, #113298, #71547, #16562, #167322, #123897, #12395, #155788, #131203, #184348, #61624, #134784, #147965, #151618, #210185, #46402, #140206, #15092, #187801, #159622, #212994, #131789 ) ) ;
#101782 = CARTESIAN_POINT ( 'NONE',  ( -0.1399997263889820043, 5.722209607272843002, -2.594334538518060729 ) ) ;
#101783 = CARTESIAN_POINT ( 'NONE',  ( -1.501328131443588232, 8.653248444470658995, -2.562127481693517783 ) ) ;
#101784 = CARTESIAN_POINT ( 'NONE',  ( -4.799223189557577207, 4.701441264013013210, 0.7216878364870317197 ) ) ;
#101785 = CARTESIAN_POINT ( 'NONE',  ( 8.093854517678360949, 12.38665467069271386, 1.040834085586084257E-14 ) ) ;
#101786 = CARTESIAN_POINT ( 'NONE',  ( 3.309381622104785148, -1.607321225346239668, -1.137771303188861660 ) ) ;
#101787 = CARTESIAN_POINT ( 'NONE',  ( 1.348456458401224412, 1.042098076042829780, -1.846665823592225975 ) ) ;
#101788 = CARTESIAN_POINT ( 'NONE',  ( -6.230135280679522936, 7.227244901336242755, 1.199719254218450271 ) ) ;
#101789 = CARTESIAN_POINT ( 'NONE',  ( -11.94311415714975588, 8.978930693142787689, 0.6090307097988665319 ) ) ;
#101790 = CARTESIAN_POINT ( 'NONE',  ( -9.496912337248829772, -9.201070920843589462, 0.2456386449429323604 ) ) ;
#101791 = CARTESIAN_POINT ( 'NONE',  ( 5.613277516225614328, -2.138688192980051639, 0.4772630486022874652 ) ) ;
#101792 = FACE_OUTER_BOUND ( 'NONE', #159593, .T. ) ;
#101793 = CARTESIAN_POINT ( 'NONE',  ( 3.909137014540211119, 1.651653515444248876, 0.9912706138347370244 ) ) ;
#101794 = CARTESIAN_POINT ( 'NONE',  ( -6.886651960737580680, 10.12184548991413457, -1.199719254218440723 ) ) ;
#101795 = CARTESIAN_POINT ( 'NONE',  ( -0.02988540731095785247, 0.7668091516429014209, -1.812018377701756888 ) ) ;
#101796 = CARTESIAN_POINT ( 'NONE',  ( 0.9794701899953797142, -0.05759512415488829418, -2.206297691287119722 ) ) ;
#101797 = DIRECTION ( 'NONE',  ( 0.000000000000000000, 0.000000000000000000, -1.000000000000000000 ) ) ;
#101798 = ORIENTED_EDGE ( 'NONE', *, *, #125041, .F. ) ;
#101799 = CARTESIAN_POINT ( 'NONE',  ( 3.553645660557675612, 6.199651466408984568, -1.082531754730549967 ) ) ;
#101800 = CARTESIAN_POINT ( 'NONE',  ( 6.227403457816463650, 0.1483525144864000778, -1.963943935631215165 ) ) ;
#101801 = CARTESIAN_POINT ( 'NONE',  ( 0.4505971019186795212, -1.641227270844529018, -1.037965677199135017 ) ) ;
#101802 = CARTESIAN_POINT ( 'NONE',  ( 6.503268925837763170, 2.271904311083965844, 0.3474358185819835798 ) ) ;
#101804 = CARTESIAN_POINT ( 'NONE',  ( 4.117883143796479573, 1.847306362133010360, -0.2240370018555241372 ) ) ;
#101803 = CARTESIAN_POINT ( 'NONE',  ( -5.108390017298964914, 9.181815130149269422, 0.000000000000000000 ) ) ;
#101805 = CARTESIAN_POINT ( 'NONE',  ( 6.444921918449731280, 8.612437886315108315, 1.599625672291268286 ) ) ;
#101806 = CARTESIAN_POINT ( 'NONE',  ( 0.000000000000000000, 13.49999999999999822, 0.000000000000000000 ) ) ;
#101807 = CARTESIAN_POINT ( 'NONE',  ( 0.000000000000000000, 6.161115872820241535, 0.000000000000000000 ) ) ;
#101808 = CARTESIAN_POINT ( 'NONE',  ( -5.880485940025243607, 7.883652901494672349, 1.599625672291269396 ) ) ;
#101809 = CARTESIAN_POINT ( 'NONE',  ( 6.720655732516647163, 2.082321177337285167, 2.135279995619132620 ) ) ;
#101810 = CARTESIAN_POINT ( 'NONE',  ( 0.6971427418834205136, 1.794861059153027627, 1.257291590721874686 ) ) ;
#101811 = CARTESIAN_POINT ( 'NONE',  ( 5.341549334104200852, 5.334155099317434257, 0.7216878364870317197 ) ) ;
#101812 = ORIENTED_EDGE ( 'NONE', *, *, #11694, .T. ) ;
#101813 = CARTESIAN_POINT ( 'NONE',  ( 9.242574560015899721, -9.438200158419393304, -0.5964493340168087743 ) ) ;
#101814 = CARTESIAN_POINT ( 'NONE',  ( 1.500000000000035971, 7.000000000000000000, 9.886859966642587594 ) ) ;
#101815 = CARTESIAN_POINT ( 'NONE',  ( 0.4514209555319322331, 0.5758240286459560542, -1.732582669633643047 ) ) ;
#101816 = CARTESIAN_POINT ( 'NONE',  ( -5.596818484342970912, 5.424043074688562172, -0.7998128361456221525 ) ) ;
#101817 = CARTESIAN_POINT ( 'NONE',  ( 2.355775467714062543, 0.08314403793566874090, -1.732266345623443948 ) ) ;
#101818 = FACE_OUTER_BOUND ( 'NONE', #25296, .T. ) ;
#101819 = CARTESIAN_POINT ( 'NONE',  ( -1.225000000000060263, 2.729166666666693164, -0.7072540797573217963 ) ) ;
#101820 = EDGE_CURVE ( 'NONE', #84638, #79740, #82046, .T. ) ;
#101821 = CARTESIAN_POINT ( 'NONE',  ( -5.438229012412903352, 6.477593614970734492, -1.082531754730549967 ) ) ;
#101822 = CARTESIAN_POINT ( 'NONE',  ( 5.180226163740526246, -1.011166736308216629, 1.519887457628710248 ) ) ;
#101823 = CARTESIAN_POINT ( 'NONE',  ( 3.871884822249270108, -1.933460040528666379, 0.3310023857948928838 ) ) ;
#101824 = CARTESIAN_POINT ( 'NONE',  ( 1.224999999999938805, -1.041666665983848938, -0.7072540797573197979 ) ) ;
#101825 = CARTESIAN_POINT ( 'NONE',  ( -8.642432853707342488, 12.17025653171218558, 1.199719254218462483 ) ) ;
#101826 = CARTESIAN_POINT ( 'NONE',  ( 5.503720292143644777, 8.508425209887878538, 1.199719254218462483 ) ) ;
#101827 = CARTESIAN_POINT ( 'NONE',  ( 4.863993733624056404, 0.6645719631460760279, -2.013739200842738608 ) ) ;
#101828 = CARTESIAN_POINT ( 'NONE',  ( 6.318982112420993502, 9.529840343536603697, -1.199719254218452047 ) ) ;
#101829 = CIRCLE ( 'NONE', #198743, 9.499999999999992895 ) ;
#101830 = CARTESIAN_POINT ( 'NONE',  ( -9.110189153378817295, 12.71597221466224603, 1.199719254218462483 ) ) ;
#101831 = CARTESIAN_POINT ( 'NONE',  ( 3.379797469122407083, -1.996479967689598789, 0.5476083754193948883 ) ) ;
#101833 = CARTESIAN_POINT ( 'NONE',  ( -0.6823417656250246877, -0.3864583329919110688, 1.181850606188755259 ) ) ;
#101832 = CARTESIAN_POINT ( 'NONE',  ( 6.827182134110226563, 2.468179810210658243, 2.195371296381436022 ) ) ;
#101836 = ORIENTED_EDGE ( 'NONE', *, *, #214379, .T. ) ;
#101835 = CARTESIAN_POINT ( 'NONE',  ( 4.793709693897413082, 2.072883653632663137, -0.7987435787581667057 ) ) ;
#101834 = AXIS2_PLACEMENT_3D ( 'NONE', #63150, #80465, #96748 ) ;
#101837 = CARTESIAN_POINT ( 'NONE',  ( 2.461953032136819264, -2.200924886027255667, -0.6633417334961901890 ) ) ;
#101838 = CARTESIAN_POINT ( 'NONE',  ( 7.280365300858406385, 11.43758391773608984, 1.040834085586084257E-14 ) ) ;
#101840 = CARTESIAN_POINT ( 'NONE',  ( -3.285556943750000514, -2.588541666188707513, -1.896917185911906500 ) ) ;
#101839 = CARTESIAN_POINT ( 'NONE',  ( 5.872089928494542477, 9.864872326636710653, 0.000000000000000000 ) ) ;
#101841 = DIRECTION ( 'NONE',  ( 0.000000000000000000, 0.000000000000000000, -1.000000000000000000 ) ) ;
#101842 = CARTESIAN_POINT ( 'NONE',  ( 0.000000000000000000, 2.800000000000024691, -0.7749999999999935829 ) ) ;
#101843 = CARTESIAN_POINT ( 'NONE',  ( -5.478522506877910203, 6.271832789251446272, -1.004670684072657583 ) ) ;
#101844 = CARTESIAN_POINT ( 'NONE',  ( 4.588094604188536429, 1.105678411722615051, 1.560157546714964871 ) ) ;
#101845 = CARTESIAN_POINT ( 'NONE',  ( 0.08888683327021046354, 6.492044364012832247, -3.106763327641855810 ) ) ;
#101846 = CARTESIAN_POINT ( 'NONE',  ( 3.698037441923990087, -1.722821800119245683, -0.08474311298608917797 ) ) ;
#101847 = CARTESIAN_POINT ( 'NONE',  ( 3.626185617424377838, 2.007256095728218614, 0.1928357053486499384 ) ) ;
#101848 = CARTESIAN_POINT ( 'NONE',  ( 3.657115705757322477, 1.277955821227232613, 1.910552683106376382 ) ) ;
#101849 = CIRCLE ( 'NONE', #8460, 1.249999999999999778 ) ;
#101850 = CARTESIAN_POINT ( 'NONE',  ( 0.6124999999999723999, 1.145833334016146843, 1.060881119635889380 ) ) ;
#101851 = CARTESIAN_POINT ( 'NONE',  ( 0.03028722099337673168, -1.361824662662258767, -1.737358624739212543 ) ) ;
#101852 = CARTESIAN_POINT ( 'NONE',  ( -5.641601317062248988, 6.714861303728305586, -1.082531754730549967 ) ) ;
#101853 = ORIENTED_EDGE ( 'NONE', *, *, #10962, .F. ) ;
#101854 = CARTESIAN_POINT ( 'NONE',  ( 4.727684277059563733, -1.088367244632810094, -1.395429379651995649 ) ) ;
#101856 = CARTESIAN_POINT ( 'NONE',  ( 0.8852319118969053102, 2.019148884293726631, -1.085135299617467020 ) ) ;
#101855 = CARTESIAN_POINT ( 'NONE',  ( 6.398522151006641678, 6.429640362454684954, 0.000000000000000000 ) ) ;
#101857 = CARTESIAN_POINT ( 'NONE',  ( 0.4095771458324704573, 1.203761932438538462, -1.257115261623420022 ) ) ;
#101858 = CARTESIAN_POINT ( 'NONE',  ( -5.921879234118920365, 10.13088588310589699, 0.000000000000000000 ) ) ;
#101859 = CARTESIAN_POINT ( 'NONE',  ( 6.685463922536254877, -0.9407050535897142352, 1.977304495687677521 ) ) ;
#101860 = CARTESIAN_POINT ( 'NONE',  ( -3.709037541790315640, 6.484905011134099340, -1.199719254218450271 ) ) ;
#101861 = CARTESIAN_POINT ( 'NONE',  ( -0.6801582343750022241, -0.6197916663252672764, -1.178068619123841643 ) ) ;
#101862 = CARTESIAN_POINT ( 'NONE',  ( 3.927105836647628134, 7.326788671016230658, -0.8738547742103716098 ) ) ;
#101863 = CARTESIAN_POINT ( 'NONE',  ( 0.3444781036854955847, -1.022991162849467228, 1.915094836987745630 ) ) ;
#101864 = CARTESIAN_POINT ( 'NONE',  ( 1.323454262349360144, -1.463929862531298198, -1.387097294446784090 ) ) ;
#101865 = CARTESIAN_POINT ( 'NONE',  ( -1.500000000000001332, -0.3187499993171846735, 0.000000000000000000 ) ) ;
#101866 = CARTESIAN_POINT ( 'NONE',  ( 4.934167778409569216, 0.9889366926784399769, -1.653171546959011140 ) ) ;
#101867 = CARTESIAN_POINT ( 'NONE',  ( 0.6823417656249969321, 11.77604166700806054, -1.181850606188757036 ) ) ;
#101868 = MECHANICAL_DESIGN_GEOMETRIC_PRESENTATION_REPRESENTATION (  '', ( #5044 ), #147352 ) ;
#101869 = CARTESIAN_POINT ( 'NONE',  ( 1.477127009259255219, -1.566406750307091533, 1.575387012651897622 ) ) ;
#101870 = ORIENTED_EDGE ( 'NONE', *, *, #179626, .F. ) ;
#101872 = CARTESIAN_POINT ( 'NONE',  ( 0.4914377447849272440, 7.519435632882160547, -2.014015809874914797 ) ) ;
#101871 = CARTESIAN_POINT ( 'NONE',  ( 1.419999999067300234, 7.203691543881690862, -4.238255391842187692 ) ) ;
#101873 = DIRECTION ( 'NONE',  ( 5.551115123125766062E-17, 0.000000000000000000, -1.000000000000000000 ) ) ;
#101874 = CARTESIAN_POINT ( 'NONE',  ( 9.725276259704228821, 10.24057714594344048, 0.7998128361456462443 ) ) ;
#101875 = DIRECTION ( 'NONE',  ( 0.000000000000000000, 1.000000000000000000, 0.000000000000000000 ) ) ;
#101876 = DIRECTION ( 'NONE',  ( 0.000000000000000000, 0.000000000000000000, -1.000000000000000000 ) ) ;
#101877 = CARTESIAN_POINT ( 'NONE',  ( 3.772797691900576567, 1.637269354731695881, -0.5906731273508105673 ) ) ;
#101879 = EDGE_CURVE ( 'NONE', #166808, #207703, #192753, .T. ) ;
#101878 = CARTESIAN_POINT ( 'NONE',  ( 2.840232074097197579, -1.010955899468408248, 1.681206195012739046 ) ) ;
#101881 = CARTESIAN_POINT ( 'NONE',  ( -1.364683531250012516, 2.301041667008087988, -0.7879004041258289570 ) ) ;
#101880 = CARTESIAN_POINT ( 'NONE',  ( 4.684505768721569652, 5.424010470718658716, -1.199719254218452047 ) ) ;
#101882 = CARTESIAN_POINT ( 'NONE',  ( -5.906232603126833958, 6.003624899985508634, 0.1331734367991978252 ) ) ;
#101883 = CARTESIAN_POINT ( 'NONE',  ( -0.9311234436981514762, -2.128119629485601738, -3.474999999999999645 ) ) ;
#101884 = CARTESIAN_POINT ( 'NONE',  ( 6.812952578306354035, -1.517200236233799071, 1.243500037895750143 ) ) ;
#101885 = CARTESIAN_POINT ( 'NONE',  ( -7.320512876374914768, 10.62801655815766999, 1.199719254218453823 ) ) ;
#101886 = CARTESIAN_POINT ( 'NONE',  ( -5.219525951136862574, 5.191794485855519170, -0.7216878364870197293 ) ) ;
#101887 = AXIS2_PLACEMENT_3D ( 'NONE', #164517, #117961, #182888 ) ;
#101888 = CARTESIAN_POINT ( 'NONE',  ( 1.710245752144876619, -2.245277845785878412, 0.2781651023185549021 ) ) ;
#101889 = ORIENTED_EDGE ( 'NONE', *, *, #154559, .T. ) ;
#101890 = CARTESIAN_POINT ( 'NONE',  ( -1.500000000000015099, -0.5479166659838513587, 0.8660254037844403729 ) ) ;
#101891 = CARTESIAN_POINT ( 'NONE',  ( 2.653401028632852654, 0.5028369177751991215, -1.801603059227441239 ) ) ;
#101892 = CARTESIAN_POINT ( 'NONE',  ( 0.8263334968928169877, 0.7041814825227004082, -1.584920328518927279 ) ) ;
#101893 = CARTESIAN_POINT ( 'NONE',  ( 4.915667883426772633, -1.172277214026868464, -1.851500752446763709 ) ) ;
#101894 = CARTESIAN_POINT ( 'NONE',  ( 5.139818204295112380, -1.627507941656263002, -1.636155730761083227 ) ) ;
#101895 = CARTESIAN_POINT ( 'NONE',  ( 0.8661736431406670267, 1.015005012832224329, 1.793514120848164195 ) ) ;
#101896 = CARTESIAN_POINT ( 'NONE',  ( 3.626839189636944738, -1.793926730891879151, 0.7440942006126953778 ) ) ;
#101897 = CARTESIAN_POINT ( 'NONE',  ( -5.382223794500852421, 5.381608636446842731, -0.7216878364870197293 ) ) ;
#101898 = VECTOR ( 'NONE', #175042, 1000.000000000000000 ) ;
#101899 = CARTESIAN_POINT ( 'NONE',  ( 6.221928862670094595, -1.039020359566013907, -1.555222851818117924 ) ) ;
#101900 = CARTESIAN_POINT ( 'NONE',  ( 1.239108386966929265, 13.33839687343696490, -0.6814443383427297718 ) ) ;
#101901 = CARTESIAN_POINT ( 'NONE',  ( 0.1452960159114678740, -0.1365383601019970750, -1.704228001402931625 ) ) ;
#101902 = ADVANCED_FACE ( 'NONE', ( #16369 ), #49962, .T. ) ;
#101903 = CARTESIAN_POINT ( 'NONE',  ( 1.360316468749963592, 1.244791667008120051, 0.7853790794158761468 ) ) ;
#101904 = CARTESIAN_POINT ( 'NONE',  ( 4.606092368833686557, -0.09613688574180989654, 2.014232646917232916 ) ) ;
#101905 = CARTESIAN_POINT ( 'NONE',  ( -4.080641047588918546, 4.823464646017586510, -1.082531754730548412 ) ) ;
#101906 = CARTESIAN_POINT ( 'NONE',  ( 8.422639742587595180, 10.84949900448412130, -1.599625672291268286 ) ) ;
#101907 = CARTESIAN_POINT ( 'NONE',  ( 4.472210567661338843, 6.310941310395290493, 1.599625672291261402 ) ) ;
#101909 = CARTESIAN_POINT ( 'NONE',  ( 7.778383330260339790, -5.907420853759298041, -7.778383330260368211 ) ) ;
#101908 = CARTESIAN_POINT ( 'NONE',  ( 1.822601884235462766, 1.703052241681313861, 0.6583118566880485911 ) ) ;
#101910 = CARTESIAN_POINT ( 'NONE',  ( -3.800028193580205382, 7.655393002477360653, -0.7998128361456481317 ) ) ;
#101911 = CARTESIAN_POINT ( 'NONE',  ( -4.899292406491859708, 6.809203455697520724, -1.599625672291271394 ) ) ;
#101912 = CARTESIAN_POINT ( 'NONE',  ( -9.706334639731263536, 5.108299517166001280, 6.477055075394225092 ) ) ;
#101913 = ORIENTED_EDGE ( 'NONE', *, *, #65438, .F. ) ;
#101914 = CARTESIAN_POINT ( 'NONE',  ( -5.926322542504872892, 8.007405281046052536, -1.443375672974066548 ) ) ;
#101915 = CARTESIAN_POINT ( 'NONE',  ( -4.464712657601869417, 4.103252943490596216, 0.7998128361456341429 ) ) ;
#101916 = CARTESIAN_POINT ( 'NONE',  ( 2.969881706132979637, 6.595290641185153291, 0.3483476683807932295 ) ) ;
#101917 = CARTESIAN_POINT ( 'NONE',  ( 5.725262222419306823, 1.782257655895511661, 0.9500345275383536015 ) ) ;
#101919 = EDGE_LOOP ( 'NONE', ( #197709, #38911, #189222, #106315 ) ) ;
#101918 = CARTESIAN_POINT ( 'NONE',  ( 6.604121268705382519, -0.9518609934017449037, 2.004712419625443776 ) ) ;
#101920 = CARTESIAN_POINT ( 'NONE',  ( -5.586841817283045408, 8.675676665875643678, 1.199719254218454489 ) ) ;
#101921 = CARTESIAN_POINT ( 'NONE',  ( 3.832150974156964818, 7.622593236491780999, 1.040834085586084257E-14 ) ) ;
#101922 = CARTESIAN_POINT ( 'NONE',  ( 5.506733764336206427, 1.562011470896901288, -1.344504574768749627 ) ) ;
#101923 = CARTESIAN_POINT ( 'NONE',  ( 4.904922738988922504, -1.081064280317966420, -1.701948707654332704 ) ) ;
#101924 = VERTEX_POINT ( 'NONE', #163726 ) ;
#101925 = VERTEX_POINT ( 'NONE', #162664 ) ;
#101926 = CARTESIAN_POINT ( 'NONE',  ( -5.000000000000013323, 11.39843543023555661, 0.7750000000000004663 ) ) ;
#101927 = CARTESIAN_POINT ( 'NONE',  ( 4.162516854595432747, 4.815023404238158555, 1.199719254218464037 ) ) ;
#101929 = ORIENTED_EDGE ( 'NONE', *, *, #34246, .F. ) ;
#101928 = CARTESIAN_POINT ( 'NONE',  ( -6.642568916052639771, 6.714361588341672515, 0.000000000000000000 ) ) ;
#101930 = CARTESIAN_POINT ( 'NONE',  ( 4.616554244727909762, 8.463227371007752353, -0.2998622348379786362 ) ) ;
#101931 = CARTESIAN_POINT ( 'NONE',  ( 5.184922634274871989, -1.076153828860962225, -1.704676470440001701 ) ) ;
#101932 = CARTESIAN_POINT ( 'NONE',  ( 3.292734131499192252, 1.452021927685825275, 1.131891246899892289 ) ) ;
#101933 = CARTESIAN_POINT ( 'NONE',  ( -6.520158902582635640, 5.290451655907115303, 2.438235897557452514 ) ) ;
#101934 = CARTESIAN_POINT ( 'NONE',  ( 2.614278096488438674, -2.282406316997650286, 0.3399710349294912115 ) ) ;
#101936 = CARTESIAN_POINT ( 'NONE',  ( 7.354371980770088690, 7.544798497178720531, 0.000000000000000000 ) ) ;
#101935 = B_SPLINE_CURVE_WITH_KNOTS ( 'NONE', 3,
 ( #82297, #165693, #108752, #194194, #59926, #115934 ),
 .UNSPECIFIED., .F., .F.,
 ( 4, 2, 4 ),
 ( 0.000000000000000000, 0.0003844267940947825469, 0.0007688535881895650938 ),
 .UNSPECIFIED. ) ;
#101937 = CARTESIAN_POINT ( 'NONE',  ( 4.622454487542248636, 1.333869025858843704, -1.700861402727947391 ) ) ;
#101938 = CARTESIAN_POINT ( 'NONE',  ( 7.964525173024008531, 11.37936423758166526, 1.199719254218460707 ) ) ;
#101939 = CARTESIAN_POINT ( 'NONE',  ( 0.3099700162084629285, 1.338387961458173070, -1.407469107711552425 ) ) ;
#101940 = CARTESIAN_POINT ( 'NONE',  ( -4.089755892816631544, 7.923132308261379819, -0.7998128361456281477 ) ) ;
#101941 = CARTESIAN_POINT ( 'NONE',  ( -9.333041836229964971, 15.44694763438214125, -7.472413793098273693 ) ) ;
#101942 = CARTESIAN_POINT ( 'NONE',  ( -6.252245114557387851, 7.323316050852266557, -1.199719254218453823 ) ) ;
#101943 = CLOSED_SHELL ( 'NONE', ( #40744, #157979, #72324, #124284, #192369, #171348, #44684, #109706, #102444, #178835, #90483, #113804, #42102, #79631, #66279, #104742, #146474, #119184, #140120, #182391, #164270, #199667, #172838, #105427, #154242, #66003, #197875, #177196, #16748, #7315 ) ) ;
#101944 = CARTESIAN_POINT ( 'NONE',  ( 3.186256133050053840, -1.842714570631575510, -0.3211874441736498054 ) ) ;
#101945 = CARTESIAN_POINT ( 'NONE',  ( 6.315303677655929704, -0.2418685481465185916, 1.956520841371222952 ) ) ;
#101947 = CARTESIAN_POINT ( 'NONE',  ( -7.422162748838431412, 7.623887726591770608, -0.7998128361456362523 ) ) ;
#101946 = CARTESIAN_POINT ( 'NONE',  ( 1.364683531249992088, 5.384375000341417916, 1.214306433183764966E-14 ) ) ;
#101948 = CARTESIAN_POINT ( 'NONE',  ( 1.998912159191484905, -0.5904864226158462737, -2.126349760018491963 ) ) ;
#101949 = CARTESIAN_POINT ( 'NONE',  ( 4.516274566683618374, 8.283087737857229627, -0.7216878364870552565 ) ) ;
#101950 = CARTESIAN_POINT ( 'NONE',  ( 4.059776932288224671, 6.823824623389866950, 1.199719254218462483 ) ) ;
#101951 = CARTESIAN_POINT ( 'NONE',  ( -3.815730167242251003, 6.539103397502874948, -1.199719254218452047 ) ) ;
#101952 = CARTESIAN_POINT ( 'NONE',  ( -6.577113915960828727, 9.727031097712693253, -1.082531754730549967 ) ) ;
#101953 = CARTESIAN_POINT ( 'NONE',  ( 0.5617156953909893113, 1.950523934018918659, -0.2849811346736507156 ) ) ;
#101954 = CARTESIAN_POINT ( 'NONE',  ( 6.270204019816865149, 1.180490267363063062, 1.982795515311958079 ) ) ;
#101955 = CARTESIAN_POINT ( 'NONE',  ( 0.9593383959572501229, 1.601786533887459507, 1.132500672181527168 ) ) ;
#101956 = CARTESIAN_POINT ( 'NONE',  ( 3.995030872118944032, 0.2978362323166737213, 2.040820773513659425 ) ) ;
#101957 = CARTESIAN_POINT ( 'NONE',  ( 4.826339496784873617, 8.574553812983598533, -0.7216878364870257245 ) ) ;
#101958 = EDGE_CURVE ( 'NONE', #21610, #86388, #193431, .T. ) ;
#101959 = CARTESIAN_POINT ( 'NONE',  ( 6.801350335910821165, 7.963938809097990124, 1.199719254218452047 ) ) ;
#101960 = VERTEX_POINT ( 'NONE', #213499 ) ;
#101961 = CARTESIAN_POINT ( 'NONE',  ( 8.392133896734671694, 8.893170422386358354, 0.7216878364870458196 ) ) ;
#101962 = CARTESIAN_POINT ( 'NONE',  ( -1.364683531249997417, 4.071875000341417028, 1.214306433183764966E-14 ) ) ;
#101963 = CYLINDRICAL_SURFACE ( 'NONE', #100757, 11.10000000000000142 ) ;
#101964 = CARTESIAN_POINT ( 'NONE',  ( 4.161989969270895706, 5.878740935614591656, 1.443375672974062551 ) ) ;
#101965 = CARTESIAN_POINT ( 'NONE',  ( 6.109878594781020134, 0.6360665949224998394, -2.075910194261113784 ) ) ;
#101967 = CARTESIAN_POINT ( 'NONE',  ( 5.987831981441136264, -1.833028718050220940, -0.1737628300680846560 ) ) ;
#101966 = DIRECTION ( 'NONE',  ( -0.000000000000000000, 1.000000000000000000, -0.000000000000000000 ) ) ;
#101968 = CARTESIAN_POINT ( 'NONE',  ( 5.405874916910509143, 6.287787029864440491, -1.050246922354510559 ) ) ;
#101969 = LINE ( 'NONE', #52155, #111972 ) ;
#101970 = CARTESIAN_POINT ( 'NONE',  ( 1.792056902697708454, -1.861051795492570049, -0.1884349046137670514 ) ) ;
#101971 = CARTESIAN_POINT ( 'NONE',  ( -4.549609453380520030, 7.192579769413725010, 1.336992641046318875 ) ) ;
#101972 = CARTESIAN_POINT ( 'NONE',  ( 1.734723475976807094E-15, -7.105553651663779391, 0.000000000000000000 ) ) ;
#101973 = CARTESIAN_POINT ( 'NONE',  ( 6.480989489388473856, 6.848452138476523565, -0.6157061703677743081 ) ) ;
#101974 = CARTESIAN_POINT ( 'NONE',  ( 1.364683531249990311, 4.926041667008083991, 0.7879004041258500513 ) ) ;
#101975 = CARTESIAN_POINT ( 'NONE',  ( 0.5922591856823838929, -1.062013159134197693, 1.590055880637729402 ) ) ;
#101976 = CARTESIAN_POINT ( 'NONE',  ( 2.693947877954734338, -1.764960265255947736, -0.1323486908471616652 ) ) ;
#101977 = CARTESIAN_POINT ( 'NONE',  ( 0.9965660710522583621, -1.865815080690262917, -0.4182784585613218420 ) ) ;
#101979 = CARTESIAN_POINT ( 'NONE',  ( 4.587445725801254426, -0.5070264450876013074, 1.847228357985892577 ) ) ;
#101978 = CARTESIAN_POINT ( 'NONE',  ( -8.157201976916404362, 12.66848607304450702, -0.7998128361456281477 ) ) ;
#101980 = CARTESIAN_POINT ( 'NONE',  ( 0.3999999999999906408, 3.949999999999988187, -0.8338124244295798126 ) ) ;
#101981 = CARTESIAN_POINT ( 'NONE',  ( 5.512145389550558328, 1.967385609537531277, -0.09471018678799088264 ) ) ;
#101982 = CARTESIAN_POINT ( 'NONE',  ( 1.406653384705614629, -2.110883996484512970, -0.2024971186788473154 ) ) ;
#101983 = DIRECTION ( 'NONE',  ( 0.000000000000000000, -1.000000000000000000, 0.000000000000000000 ) ) ;
#101984 = CARTESIAN_POINT ( 'NONE',  ( 3.397188523315307407, 1.473948685399184333, 1.151750840393983344 ) ) ;
#101986 = VERTEX_POINT ( 'NONE', #178915 ) ;
#101985 = CARTESIAN_POINT ( 'NONE',  ( 6.445920802586958764, 0.6525945181424031016, -1.596887126696917791 ) ) ;
#101988 = CARTESIAN_POINT ( 'NONE',  ( 3.470524135418292300, 5.072030796119872953, -1.443375672974057666 ) ) ;
#101987 = CARTESIAN_POINT ( 'NONE',  ( 3.018423772948013006, -1.088090592406821155, -1.919924466345590108 ) ) ;
#101989 = CARTESIAN_POINT ( 'NONE',  ( 1.364683531249988535, 4.176041667008081326, 0.7879004041258500513 ) ) ;
#101990 = CARTESIAN_POINT ( 'NONE',  ( 1.188016131547619647, -1.306928873568227623, -1.595823035580832272 ) ) ;
#101991 = CARTESIAN_POINT ( 'NONE',  ( 6.612626235163189925, 8.737816579155630592, -1.599625672291262513 ) ) ;
#101993 = CARTESIAN_POINT ( 'NONE',  ( -8.130085669689073313, 12.63685038127928806, 0.7998128361456481317 ) ) ;
#101992 = AXIS2_PLACEMENT_3D ( 'NONE', #162306, #193722, #97316 ) ;
#101994 = CARTESIAN_POINT ( 'NONE',  ( -8.830779531597137577, 3.974415841077566292, -7.430925027917930414 ) ) ;
#101995 = CARTESIAN_POINT ( 'NONE',  ( -3.422577805355617730, -0.02192484962740117241, -0.4179650480824659842 ) ) ;
#101996 = CARTESIAN_POINT ( 'NONE',  ( -1.499999999999960476, 7.378742179571331938, 10.87908636427991205 ) ) ;
#101997 = VERTEX_POINT ( 'NONE', #145383 ) ;
#101998 = CARTESIAN_POINT ( 'NONE',  ( 3.631357695093720750, 0.05367941694835526995, -2.069842578854002468 ) ) ;
#102000 = CARTESIAN_POINT ( 'NONE',  ( -1.201851678989727383E-14, 4.087500000000022560, -1.732050807568863648 ) ) ;
#101999 = VECTOR ( 'NONE', #197157, 1000.000000000000000 ) ;
#102001 = CARTESIAN_POINT ( 'NONE',  ( 1.528841242883504981, 2.082761121880230881, 0.5781018612496248155 ) ) ;
#102002 = CARTESIAN_POINT ( 'NONE',  ( -6.429665931644899857, 6.880618766637560668, 0.7446329532827021813 ) ) ;
#102003 = CARTESIAN_POINT ( 'NONE',  ( 1.154951149459724880, 0.3962062163746901677, 1.980246309512444070 ) ) ;
#102004 = DIRECTION ( 'NONE',  ( 0.000000000000000000, 0.000000000000000000, -1.000000000000000000 ) ) ;
#102005 = EDGE_CURVE ( 'NONE', #115335, #199311, #137435, .T. ) ;
#102007 = CARTESIAN_POINT ( 'NONE',  ( 9.083599731475992201, 9.699880562917908122, 0.7216878364870438212 ) ) ;
#102006 = CARTESIAN_POINT ( 'NONE',  ( 0.1747926744264660381, 7.629137130509078268, -2.455305974604498953 ) ) ;
#102008 = CARTESIAN_POINT ( 'NONE',  ( 6.854846703925609575, -0.8643618726141141240, 1.819651424301058418 ) ) ;
#102009 = CARTESIAN_POINT ( 'NONE',  ( 6.051949806467664672, 0.9910487912591151582, 1.639330874965704732 ) ) ;
#102010 = CARTESIAN_POINT ( 'NONE',  ( 6.639320575229248789, 2.413637632230402286, 2.584074196137386092 ) ) ;
#102011 = CARTESIAN_POINT ( 'NONE',  ( 3.491892070630482348, -2.189115664112693871, -0.1057334378413293807 ) ) ;
#102012 = VECTOR ( 'NONE', #172053, 1000.000000000000000 ) ;
#102013 = CARTESIAN_POINT ( 'NONE',  ( 1.499999999999989120, 3.056250000682818158, 1.214306433183764966E-14 ) ) ;
#102014 = CARTESIAN_POINT ( 'NONE',  ( 3.463059065379544776, -1.560675823418774533, 1.104941681961457256 ) ) ;
#102015 = CARTESIAN_POINT ( 'NONE',  ( -4.446184310277715213, 7.274633231044262516, -1.199719254218452047 ) ) ;
#102016 = EDGE_CURVE ( 'NONE', #117162, #57811, #41509, .T. ) ;
#102017 = CARTESIAN_POINT ( 'NONE',  ( 2.846849068745292755, 6.265148313604064434, 0.000000000000000000 ) ) ;
#102019 = CARTESIAN_POINT ( 'NONE',  ( 0.9312678054614745848, -1.591333336790928366, -1.238303555203337458 ) ) ;
#102018 = CARTESIAN_POINT ( 'NONE',  ( -8.459924664802993988, 12.81373650900478189, 1.040834085586084257E-14 ) ) ;
#102020 = CARTESIAN_POINT ( 'NONE',  ( -1.364683531250010295, 11.69270833367473017, 0.7879004041258445001 ) ) ;
#102022 = CARTESIAN_POINT ( 'NONE',  ( -5.764151584465413869, 6.753873599078290546, -1.199719254218453823 ) ) ;
#102021 = CARTESIAN_POINT ( 'NONE',  ( 0.8027370721926800901, 1.731296644042874755, -1.502618532894074876 ) ) ;
#102024 = ORIENTED_EDGE ( 'NONE', *, *, #174354, .F. ) ;
#102023 = CARTESIAN_POINT ( 'NONE',  ( 4.453923018928796829, 1.724380149092176850, -0.04373908735122617603 ) ) ;
#102025 = DIRECTION ( 'NONE',  ( 0.000000000000000000, 1.000000000000000000, 0.000000000000000000 ) ) ;
#102026 = CARTESIAN_POINT ( 'NONE',  ( 7.958799866421889746, 9.244020251369077457, -1.199719254218441611 ) ) ;
#102027 = CARTESIAN_POINT ( 'NONE',  ( 5.183294799126148433, 4.941598775268944976, 1.040834085586084257E-14 ) ) ;
#102028 = CARTESIAN_POINT ( 'NONE',  ( 6.381095703207991576, -8.233137084989849086, 7.037870247915948063 ) ) ;
#102029 = CARTESIAN_POINT ( 'NONE',  ( 1.539427311113782837, 1.813978416018032558, -0.7477436361984082236 ) ) ;
#102030 = CARTESIAN_POINT ( 'NONE',  ( 4.273844736805816780, 6.009238164405336313, 1.599625672291267398 ) ) ;
#102031 = CARTESIAN_POINT ( 'NONE',  ( 0.07556134207191073093, 7.629137130509040077, -2.844199257382596269 ) ) ;
#102032 = ORIENTED_EDGE ( 'NONE', *, *, #121074, .T. ) ;
#102033 = DIRECTION ( 'NONE',  ( -0.000000000000000000, 1.000000000000000000, 0.000000000000000000 ) ) ;
#102034 = ORIENTED_EDGE ( 'NONE', *, *, #60236, .F. ) ;
#102035 = CARTESIAN_POINT ( 'NONE',  ( 3.861793950654641261, 0.6069239149280086787, -1.706917045096454366 ) ) ;
#102036 = AXIS2_PLACEMENT_3D ( 'NONE', #198944, #103620, #53798 ) ;
#102037 = VERTEX_POINT ( 'NONE', #33703 ) ;
#102038 = CARTESIAN_POINT ( 'NONE',  ( 6.313256805818848960, 7.394496357324014113, 1.199719254218452047 ) ) ;
#102039 = PLANE ( 'NONE',  #153028 ) ;
#102040 = CARTESIAN_POINT ( 'NONE',  ( 5.215404452620196807, 1.484227587358154077, 1.038217761341611922 ) ) ;
#102041 = CARTESIAN_POINT ( 'NONE',  ( 4.868786560638878491, 8.694351730805124134, 0.7216878364870317197 ) ) ;
#102042 = CARTESIAN_POINT ( 'NONE',  ( -4.792515913634093623E-13, -7.868798029037626485, 9.500000000000001776 ) ) ;
#102043 = CARTESIAN_POINT ( 'NONE',  ( 4.708705726121224622, 6.822254573549790813, -1.234111767277449534 ) ) ;
#102045 = CARTESIAN_POINT ( 'NONE',  ( 9.083072846151447166, 12.68433652289702884, 1.199719254218450271 ) ) ;
#102044 = CARTESIAN_POINT ( 'NONE',  ( 6.092234697878679661, 0.9164522128973868753, -1.619700000576968391 ) ) ;
#102046 = CARTESIAN_POINT ( 'NONE',  ( 4.253473425383147877, 1.857088099111468216, -0.4692844457289280236 ) ) ;
#102047 = CARTESIAN_POINT ( 'NONE',  ( 1.500000000000039524, 7.564371094685074404, 10.87018506808106899 ) ) ;
#102048 = CARTESIAN_POINT ( 'NONE',  ( -12.93621305287376089, 7.735084883283615653, -1.079074430401041118 ) ) ;
#102049 = EDGE_CURVE ( 'NONE', #177991, #91101, #57796, .T. ) ;
#102050 = CARTESIAN_POINT ( 'NONE',  ( -1.499999999999997780, 5.681250000682820378, 1.214306433183764966E-14 ) ) ;
#102051 = CARTESIAN_POINT ( 'NONE',  ( 1.270994156678442596E-16, -6.530144695498194096, -11.00000000000000178 ) ) ;
#102052 = CARTESIAN_POINT ( 'NONE',  ( 6.805829924380114804, 8.002851668940699881, 1.082531754730558626 ) ) ;
#102053 = B_SPLINE_CURVE_WITH_KNOTS ( 'NONE', 3,
 ( #154059, #71706, #121637, #187606, #105325, #173531 ),
 .UNSPECIFIED., .F., .F.,
 ( 4, 2, 4 ),
 ( 0.000000000000000000, 0.0002821277059972537317, 0.0005642554119945074635 ),
 .UNSPECIFIED. ) ;
#102054 = CARTESIAN_POINT ( 'NONE',  ( -9.002250809793991948, 12.48608113052627289, -1.082531754730543971 ) ) ;
#102055 = CARTESIAN_POINT ( 'NONE',  ( 1.305796196612363902, -0.5247483525172501606, 2.096912610238470975 ) ) ;
#102056 = CARTESIAN_POINT ( 'NONE',  ( -5.424143973919053785, 8.485862515284315677, 1.199719254218454489 ) ) ;
#102057 = CIRCLE ( 'NONE', #198807, 11.92000000000000171 ) ;
#102058 = CARTESIAN_POINT ( 'NONE',  ( 5.879395890181562834, 6.888325289080478697, -1.199719254218452047 ) ) ;
#102059 = CARTESIAN_POINT ( 'NONE',  ( 0.7272432748211544729, -1.735090175422876246, 0.5678700757711930835 ) ) ;
#102060 = CARTESIAN_POINT ( 'NONE',  ( -4.608882153641705059, 7.464447381635583412, -1.199719254218452047 ) ) ;
#102061 = CARTESIAN_POINT ( 'NONE',  ( 3.996943106591983597, 1.542326501817241180, -0.9764022233923684846 ) ) ;
#102062 = CARTESIAN_POINT ( 'NONE',  ( 10.79929312474867942, -8.526088927970997489, -0.1885023626713021039 ) ) ;
#102063 = CARTESIAN_POINT ( 'NONE',  ( 1.546972149855216472, 0.1906517044060058730, 1.902890584052991940 ) ) ;
#102064 = CARTESIAN_POINT ( 'NONE',  ( 2.664455434096600683, -0.7511504341344789060, -1.820894044046962534 ) ) ;
#102065 = CARTESIAN_POINT ( 'NONE',  ( 4.212401414637350072, 1.776917926058638963, 0.7840673734914437309 ) ) ;
#102066 = CARTESIAN_POINT ( 'NONE',  ( -3.923105346307911745, 5.670318552149568703, -1.599625672291283607 ) ) ;
#102068 = CARTESIAN_POINT ( 'NONE',  ( 4.043311264919998038, 0.1072909356813686182, 2.118029240109862155 ) ) ;
#102067 = CARTESIAN_POINT ( 'NONE',  ( 7.856023664475727308, 8.130058794835305136, -0.7998128361456341429 ) ) ;
#102069 = CARTESIAN_POINT ( 'NONE',  ( 0.1899713450103265033, -8.048696291100959854, 9.532262708098286907 ) ) ;
#102070 = CARTESIAN_POINT ( 'NONE',  ( 9.097684769969825780, 10.57271930550834860, -1.199719254218446718 ) ) ;
#102071 = CARTESIAN_POINT ( 'NONE',  ( 6.029390871727402512, 6.069343164222702924, -0.5281050654588164139 ) ) ;
#102072 = CARTESIAN_POINT ( 'NONE',  ( 0.4019237886466816012, 11.70758545099816494, -1.499999999999998668 ) ) ;
#102073 = CARTESIAN_POINT ( 'NONE',  ( 6.333594036239346359, 7.418223126147930557, 1.199719254218453823 ) ) ;
#102074 = CARTESIAN_POINT ( 'NONE',  ( 11.94980361723080264, 12.59761943414562957, -1.099999926404445771 ) ) ;
#102075 = CARTESIAN_POINT ( 'NONE',  ( 3.580510235063854019, -1.759844519496515325, -0.4856381957471164745 ) ) ;
#102076 = CARTESIAN_POINT ( 'NONE',  ( 0.3866937364864087567, 3.956598013261175772, -11.53692321988872926 ) ) ;
#102077 = CARTESIAN_POINT ( 'NONE',  ( -8.595506201384022660, 11.05117653974661529, 1.443375672974064550 ) ) ;
#102078 = CARTESIAN_POINT ( 'NONE',  ( -5.337921042252067316, 7.714266718146587820, 1.325459453385816833 ) ) ;
#102079 = PLANE ( 'NONE',  #129600 ) ;
#102080 = CARTESIAN_POINT ( 'NONE',  ( 5.014452206985246185, 1.289541220462528504, -1.355370375751355105 ) ) ;
#102081 = CARTESIAN_POINT ( 'NONE',  ( 6.913768267964901071, 10.15348118167935709, -1.199719254218441611 ) ) ;
#102082 = CARTESIAN_POINT ( 'NONE',  ( 3.193887106011963350, -0.7802878698427909709, 1.761581285093082982 ) ) ;
#102083 = CARTESIAN_POINT ( 'NONE',  ( 6.930524233185828997, -1.209519613549964845, 1.545115813350018241 ) ) ;
#102084 = CARTESIAN_POINT ( 'NONE',  ( 3.867100128395839942, 5.534702787927018974, -1.599625672291255185 ) ) ;
#102085 = CARTESIAN_POINT ( 'NONE',  ( -0.6823417656250003738, 9.463541667008065872, 1.181850606188754593 ) ) ;
#102086 = CARTESIAN_POINT ( 'NONE',  ( -6.551614543901706611, 8.666636272683888365, 1.599625672291283607 ) ) ;
#102087 = CARTESIAN_POINT ( 'NONE',  ( 2.822068529938852155, 6.444163718237301275, -0.7998128361456291469 ) ) ;
#102088 = CARTESIAN_POINT ( 'NONE',  ( -4.055297343818976330, 5.824542549245813383, 1.443375672974065660 ) ) ;
#102089 = CARTESIAN_POINT ( 'NONE',  ( 1.511481539699152776, -1.992283995360244253, 0.7168839309619617906 ) ) ;
#102090 = CARTESIAN_POINT ( 'NONE',  ( 8.594979316059474073, 12.11489407112305372, 1.199719254218450271 ) ) ;
#102091 = CARTESIAN_POINT ( 'NONE',  ( 0.4426559099768930805, 6.562653563187502925, 3.383538084249848144 ) ) ;
#102092 = CARTESIAN_POINT ( 'NONE',  ( 6.315297747118990834, -1.772576088781053327, -1.069364167438614732 ) ) ;
#102094 = CARTESIAN_POINT ( 'NONE',  ( 4.291716407524416077, 7.230775179981989709, -0.9765121647202840149 ) ) ;
#102093 = CARTESIAN_POINT ( 'NONE',  ( 0.7844012160764175512, 1.623964078452419857, -0.8677550623670119423 ) ) ;
#102095 = CARTESIAN_POINT ( 'NONE',  ( 6.609999999999973674, -0.005249217919313375023, 2.280159464062641916 ) ) ;
#102096 = CARTESIAN_POINT ( 'NONE',  ( 5.287316719649520991, 8.151991358691011769, -1.082531754730549078 ) ) ;
#102097 = CARTESIAN_POINT ( 'NONE',  ( 5.424670859243587273, 5.501406555305196733, -0.7216878364870458196 ) ) ;
#102098 = CARTESIAN_POINT ( 'NONE',  ( 1.359778343217881602, 2.257671611795939004, -0.3959128255837316979 ) ) ;
#102099 = CARTESIAN_POINT ( 'NONE',  ( 0.06470675514189982991, -1.629034059718449834, -0.8243793580787887043 ) ) ;
#102100 = CARTESIAN_POINT ( 'NONE',  ( -6.622231685632140596, 6.690634819517756959, 0.000000000000000000 ) ) ;
#102101 = CARTESIAN_POINT ( 'NONE',  ( 6.052673674419667194, -1.666704710846309112, -0.9964068823852706425 ) ) ;
#102102 = ORIENTED_EDGE ( 'NONE', *, *, #198854, .T. ) ;
#102103 = CARTESIAN_POINT ( 'NONE',  ( 8.880227426826641235, 10.42298208846167284, 1.082531754730549967 ) ) ;
#102104 = CARTESIAN_POINT ( 'NONE',  ( 0.3166526355253923009, -0.6820779544549429030, -1.894243553402875202 ) ) ;
#102105 = CARTESIAN_POINT ( 'NONE',  ( 6.421112215724263272, -1.799107166270615732, 0.9110519380226205222 ) ) ;
#102107 = DIRECTION ( 'NONE',  ( 0.1510067114093955887, 0.000000000000000000, -0.9885327375000383388 ) ) ;
#102106 = CARTESIAN_POINT ( 'NONE',  ( -7.004758919754800139, 11.32396917302262018, 0.000000000000000000 ) ) ;
#102108 = DIRECTION ( 'NONE',  ( -1.000000000000000000, 5.578564026256503701E-16, -1.972152263052529514E-31 ) ) ;
#102111 = B_SPLINE_CURVE_WITH_KNOTS ( 'NONE', 3,
 ( #129745, #180534, #32156, #162170, #66741, #213015, #81962, #164289, #148047, #214055 ),
 .UNSPECIFIED., .F., .F.,
 ( 4, 2, 2, 2, 4 ),
 ( 1.904249188897462635E-17, 0.0002021113321160430986, 0.0004042226642320671153, 0.0006063339963480911862, 0.0008084453284641152570 ),
 .UNSPECIFIED. ) ;
#102110 = CARTESIAN_POINT ( 'NONE',  ( 2.465387952175815744, 1.736178859682969700, -0.3425752158293988159 ) ) ;
#102109 = CARTESIAN_POINT ( 'NONE',  ( 2.625039678221803729, -1.950394636745816701, 0.7532777691767779116 ) ) ;
#102112 = CARTESIAN_POINT ( 'NONE',  ( 0.7500000000000006661, 12.16666666666666607, -1.299038105676657340 ) ) ;
#102113 = VECTOR ( 'NONE', #173403, 1000.000000000000000 ) ;
#102115 = CARTESIAN_POINT ( 'NONE',  ( 4.875077803184670877, 2.140050280577758812, -0.8218066810307764758 ) ) ;
#102114 = CARTESIAN_POINT ( 'NONE',  ( -11.32753564352527675, 6.357177643255160326, -3.964828284308058226 ) ) ;
#102116 = CARTESIAN_POINT ( 'NONE',  ( 3.292619090915947844, 1.372597323508369715, 1.069791993016102172 ) ) ;
#102117 = CARTESIAN_POINT ( 'NONE',  ( 8.543609354905870035, 13.11929468069890525, 0.7998128361456462443 ) ) ;
#102118 = CARTESIAN_POINT ( 'NONE',  ( 4.899292406491845497, 6.809203455697520724, -1.599625672291273393 ) ) ;
#102119 = CARTESIAN_POINT ( 'NONE',  ( 3.708057520534962848, -1.311595775785476148, -1.134043610401070712 ) ) ;
#102120 = CARTESIAN_POINT ( 'NONE',  ( 3.350208609569472529, -0.8826205156595956502, 1.983864470818137660 ) ) ;
#102121 = CARTESIAN_POINT ( 'NONE',  ( 3.147464216666835402, 6.823792019419957278, -0.7998128361456291469 ) ) ;
#102122 = CARTESIAN_POINT ( 'NONE',  ( 4.206267736153862735, 1.236801365491456028, -1.592660703826812352 ) ) ;
#102123 = CARTESIAN_POINT ( 'NONE',  ( 1.406250000000001332, 1.895863743164055926, -0.7852924748300647018 ) ) ;
#102124 = CARTESIAN_POINT ( 'NONE',  ( 0.7499999999999920064, 4.014583334016149863, 1.299038105676669330 ) ) ;
#102125 = CARTESIAN_POINT ( 'NONE',  ( 1.834862671528534994, 0.1865727292883790633, 1.917327306167202261 ) ) ;
#102126 = CARTESIAN_POINT ( 'NONE',  ( 1.499999999999993117, 9.135416667349463893, 0.8660254037844409281 ) ) ;
#102127 = CARTESIAN_POINT ( 'NONE',  ( 5.660436988733716035, 2.218808146451553220, 0.1093606849192785280 ) ) ;
#102128 = EDGE_LOOP ( 'NONE', ( #4409, #163429, #31444, #206205 ) ) ;
#102129 = CARTESIAN_POINT ( 'NONE',  ( 6.883263157960367806, 0.5819222519044697783, 1.998722019247618276 ) ) ;
#102130 = CARTESIAN_POINT ( 'NONE',  ( -1.201851678989727383E-14, 1.462500000000018119, 1.732050807568877637 ) ) ;
#102131 = CARTESIAN_POINT ( 'NONE',  ( 5.615048174354031474, 9.702639970055050966, 0.7998128361456462443 ) ) ;
#102132 = CARTESIAN_POINT ( 'NONE',  ( 5.151735183068521629, 5.112705256442466428, 1.040834085586084257E-14 ) ) ;
#102133 = CARTESIAN_POINT ( 'NONE',  ( 1.001543065824772753E-15, -1.421874999522042549, 3.793834371823810780 ) ) ;
#102134 = CARTESIAN_POINT ( 'NONE',  ( 0.8212868038825784645, 1.678483586613238154, -1.455034836404971665 ) ) ;
#102136 = EDGE_CURVE ( 'NONE', #200016, #119366, #90615, .T. ) ;
#102135 = CARTESIAN_POINT ( 'NONE',  ( 5.652778587040098834, -0.4750822840141955550, -1.903360745478323901 ) ) ;
#102137 = CARTESIAN_POINT ( 'NONE',  ( 8.188761592974039161, 10.57664116326830595, -1.443375672974063439 ) ) ;
#102138 = CARTESIAN_POINT ( 'NONE',  ( -0.3565558069077310321, 3.212289187162292503, 1.969079779732920032 ) ) ;
#102139 = CARTESIAN_POINT ( 'NONE',  ( 6.380173838452511959, -1.218392737502610013, 1.906166127322491910 ) ) ;
#102140 = AXIS2_PLACEMENT_3D ( 'NONE', #11999, #161482, #147354 ) ;
#102141 = CARTESIAN_POINT ( 'NONE',  ( 5.065906673361608270, 5.939254536123854677, -1.199719254218450271 ) ) ;
#102142 = CARTESIAN_POINT ( 'NONE',  ( -5.966997003790240228, 6.134120390609613338, -0.7216878364870338292 ) ) ;
#102143 = CARTESIAN_POINT ( 'NONE',  ( 4.703617135414410733, -1.592502274362836978, -1.310920101374695168 ) ) ;
#102144 = CARTESIAN_POINT ( 'NONE',  ( -3.744022975668147790, 7.519777238254810925, -0.7998128361456281477 ) ) ;
#102145 = PRESENTATION_LAYER_ASSIGNMENT (  '', '', ( #195542 ) ) ;
#102146 = CARTESIAN_POINT ( 'NONE',  ( 1.499999999999989120, 4.035416667349482012, 0.8660254037844524744 ) ) ;
#102147 = CARTESIAN_POINT ( 'NONE',  ( -0.6823417656250212460, 5.363541667008087543, 1.181850606188767472 ) ) ;
#102148 = CARTESIAN_POINT ( 'NONE',  ( 5.782452155351484713, -1.824793809246130438, -0.4103911052399379367 ) ) ;
#102149 = CARTESIAN_POINT ( 'NONE',  ( 4.254371668973718990, 1.680547194560323643, -0.4271837243535313022 ) ) ;
#102150 = CARTESIAN_POINT ( 'NONE',  ( 2.911345607792231949, -0.8600081332746039031, -1.513042209403854699 ) ) ;
#102151 = CARTESIAN_POINT ( 'NONE',  ( 8.825994812371966702, 12.28044913353391898, -1.082531754730543083 ) ) ;
#102152 = CARTESIAN_POINT ( 'NONE',  ( 2.068323803795060645, -1.406806521851681424, 1.809881060044524093 ) ) ;
#102153 = CARTESIAN_POINT ( 'NONE',  ( 1.364683531249990311, 3.446875000341416584, 1.214306433183764966E-14 ) ) ;
#102154 = CARTESIAN_POINT ( 'NONE',  ( 6.110894567773135222, -0.2550301881006194482, 2.075043241552937179 ) ) ;
#102155 = CARTESIAN_POINT ( 'NONE',  ( 0.07576575995338691305, -1.785066692240460551, -0.4505573523648154222 ) ) ;
#102156 = CARTESIAN_POINT ( 'NONE',  ( -0.3870735955438814879, 1.000000000000000888, 11.88799243440809050 ) ) ;
#102157 = SURFACE_SIDE_STYLE ('',( #66418 ) ) ;
#102158 = CARTESIAN_POINT ( 'NONE',  ( 1.547500230860882287, -1.423960469535384465, 1.427938386157491246 ) ) ;
#102159 = DIRECTION ( 'NONE',  ( 0.7592566023652971285, -0.6507913734559680474, 0.000000000000000000 ) ) ;
#102160 = CARTESIAN_POINT ( 'NONE',  ( 7.536566823016115357, 13.99512261572719929, -10.19722028184718532 ) ) ;
#102161 = CARTESIAN_POINT ( 'NONE',  ( -7.232384877886063990, 10.52520055992070525, -1.199719254218446718 ) ) ;
#102162 = CARTESIAN_POINT ( 'NONE',  ( 7.169564303528210836, 7.258913197071374945, -0.7998128361456281477 ) ) ;
#102163 = CARTESIAN_POINT ( 'NONE',  ( 2.701940546545733568, 1.501232083741442125, 1.497845299259780827 ) ) ;
#102164 = CARTESIAN_POINT ( 'NONE',  ( -0.6823417656250003738, -0.2822916663252489355, -1.181850606188749264 ) ) ;
#102165 = CARTESIAN_POINT ( 'NONE',  ( 5.830640656690653678, 1.760721658632548037, 0.4824517239352192344 ) ) ;
#102166 = EDGE_LOOP ( 'NONE', ( #22917, #24620 ) ) ;
#102167 = CARTESIAN_POINT ( 'NONE',  ( -5.108390017298964914, 9.181815130149269422, 0.000000000000000000 ) ) ;
#102168 = CARTESIAN_POINT ( 'NONE',  ( -4.909104350095669034, 4.829635951307452046, 0.07536873999081075692 ) ) ;
#102169 = CARTESIAN_POINT ( 'NONE',  ( -3.285556943750000514, -1.276041666188709511, -1.896917185911906500 ) ) ;
#102170 = CARTESIAN_POINT ( 'NONE',  ( -5.096975683733680818, 8.033889833409558534, -1.199719254218452047 ) ) ;
#102171 = CARTESIAN_POINT ( 'NONE',  ( 2.531515522815621200, -0.1936091499190935594, 2.010454966646264552 ) ) ;
#102172 = CARTESIAN_POINT ( 'NONE',  ( 6.264705869774118696, -1.564926740429407603, 1.556175991035801287 ) ) ;
#102173 = CARTESIAN_POINT ( 'NONE',  ( 10.16199982864259788, 11.81442020729326536, 1.199719254218452047 ) ) ;
#102174 = CARTESIAN_POINT ( 'NONE',  ( 3.994834637159989654, 0.2691826048217076384, 1.841218289905453664 ) ) ;
#102175 = CARTESIAN_POINT ( 'NONE',  ( 9.752392566931574081, 10.27221283770866300, -0.7998128361456281477 ) ) ;
#102176 = CARTESIAN_POINT ( 'NONE',  ( 11.86239285000045918, 13.88000000000000078, -1.812080536912753059 ) ) ;
#102177 = ORIENTED_EDGE ( 'NONE', *, *, #117997, .T. ) ;
#102178 = CARTESIAN_POINT ( 'NONE',  ( -4.009460741339347045, 5.700790169694431420, -1.599625672291256295 ) ) ;
#102179 = CARTESIAN_POINT ( 'NONE',  ( -9.006694118179950692, 9.402231314165087284, 1.040834085586084257E-14 ) ) ;
#102180 = AXIS2_PLACEMENT_3D ( 'NONE', #187535, #108497, #209098 ) ;
#102182 = CARTESIAN_POINT ( 'NONE',  ( -4.867404985860277478, 6.905081695904778272, 1.445136279841979121 ) ) ;
#102181 = CARTESIAN_POINT ( 'NONE',  ( -7.449279056065764237, 7.655523418356991350, 0.7998128361456341429 ) ) ;
#102183 = CARTESIAN_POINT ( 'NONE',  ( 1.364683531249988757, -0.3656249996585800299, 0.000000000000000000 ) ) ;
#102184 = CARTESIAN_POINT ( 'NONE',  ( 1.616079437515309136, 0.5095893236424541284, -1.657241410798731440 ) ) ;
#102185 = CARTESIAN_POINT ( 'NONE',  ( 1.306181984371343585, 1.533458449073618057, 0.8229166363448844335 ) ) ;
#102187 = CARTESIAN_POINT ( 'NONE',  ( 7.456621297836067086, 10.68284669990868174, 1.082531754730558626 ) ) ;
#102186 = CARTESIAN_POINT ( 'NONE',  ( 6.076872578159392191, -2.189301982996785245, -0.7299270095633101363 ) ) ;
#102188 = CARTESIAN_POINT ( 'NONE',  ( 6.590425141155737521, 6.776330403399432711, -0.3092786388759184990 ) ) ;
#102189 = CARTESIAN_POINT ( 'NONE',  ( 1.915377802959626230, -0.2551614870064948803, 2.044872660591416480 ) ) ;
#102190 = CARTESIAN_POINT ( 'NONE',  ( 5.656776405399742025, 7.622658444431597680, -1.599625672291262513 ) ) ;
#102191 = CARTESIAN_POINT ( 'NONE',  ( 6.503268925837763170, 2.271904311083965844, 0.3474358185819835798 ) ) ;
#102192 = CARTESIAN_POINT ( 'NONE',  ( 6.902720183911293717, 15.44694763437295570, -9.761920501353824164 ) ) ;
#102193 = CARTESIAN_POINT ( 'NONE',  ( -5.261446130555064826, 8.296048364692991228, 1.199719254218452935 ) ) ;
#102194 = CARTESIAN_POINT ( 'NONE',  ( 0.3210827503922530357, -0.09932373348091848297, 1.969089571372897085 ) ) ;
#102195 = AXIS2_PLACEMENT_3D ( 'NONE', #192605, #74615, #161196 ) ;
#102197 = CARTESIAN_POINT ( 'NONE',  ( -7.431277594066152403, 8.802816960232885179, -1.082531754730549967 ) ) ;
#102196 = CARTESIAN_POINT ( 'NONE',  ( 3.181800181368432678, 1.864768544494728175, -0.4233684943922080834 ) ) ;
#102198 = CARTESIAN_POINT ( 'NONE',  ( 5.830760709146560750, 2.125890151018691832, 0.5921790101122563765 ) ) ;
#102199 = CARTESIAN_POINT ( 'NONE',  ( 1.224999999999955014, 1.958333334016108873, -0.7072540797573237947 ) ) ;
#102200 = CARTESIAN_POINT ( 'NONE',  ( -8.068510813464099485, 8.585886501895810596, 0.7216878364870317197 ) ) ;
#102201 = CARTESIAN_POINT ( 'NONE',  ( 4.787437638956922648, 6.678706226906775179, -1.443375672974068769 ) ) ;
#102202 = AXIS2_PLACEMENT_3D ( 'NONE', #117864, #19213, #135136 ) ;
#102203 = CARTESIAN_POINT ( 'NONE',  ( -5.139949632912262700, 5.169231791251960750, 0.7216878364870257245 ) ) ;
#102204 = CARTESIAN_POINT ( 'NONE',  ( 6.516280388114966904, -2.120036885061008292, 0.05137064186952475936 ) ) ;
#102205 = VERTEX_POINT ( 'NONE', #200451 ) ;
#102206 = CARTESIAN_POINT ( 'NONE',  ( 3.241587113499379669, -2.035928198617407592, 1.086232460313860892 ) ) ;
#102207 = CARTESIAN_POINT ( 'NONE',  ( 4.334394203492665909, -1.131343785558375226, 1.602600411086833931 ) ) ;
#102208 = CARTESIAN_POINT ( 'NONE',  ( 0.9714493606215730548, -0.2934177832072166758, 1.939591667560663035 ) ) ;
#102209 = CARTESIAN_POINT ( 'NONE',  ( 7.979500612418553906, 15.27321092523385104, 8.904723856824006134 ) ) ;
#102210 = CARTESIAN_POINT ( 'NONE',  ( -11.89835103415199313, 13.82893085832464131, 1.561208891256346876 ) ) ;
#102211 = ORIENTED_EDGE ( 'NONE', *, *, #110606, .F. ) ;
#102212 = CARTESIAN_POINT ( 'NONE',  ( 6.421112215724263272, -1.799107166270615732, 0.9110519380226205222 ) ) ;
#102213 = CARTESIAN_POINT ( 'NONE',  ( -6.821723845970312894, 11.11042825360738284, 0.000000000000000000 ) ) ;
#102214 = CARTESIAN_POINT ( 'NONE',  ( 1.419999999999989049, 6.280000000000042881, -2.579999999999995630 ) ) ;
#102215 = CARTESIAN_POINT ( 'NONE',  ( 3.608415011292832819, 2.171239808225163159, 0.005094884836047069293 ) ) ;
#102216 = CARTESIAN_POINT ( 'NONE',  ( 0.4999999999999761302, 3.172938907704328404, 0.3999999999999750422 ) ) ;
#102217 = CARTESIAN_POINT ( 'NONE',  ( 1.055114822555893728, 0.4192091730233596381, 2.078585086915801128 ) ) ;
#102218 = CARTESIAN_POINT ( 'NONE',  ( 1.499999999999989120, 1.556250000682817047, 0.000000000000000000 ) ) ;
#102219 = CARTESIAN_POINT ( 'NONE',  ( 10.38962578677386084, 11.01565159419135043, 0.000000000000000000 ) ) ;
#102220 = CARTESIAN_POINT ( 'NONE',  ( -4.909853179035948756, 4.660783761091170874, 0.1377329554490049068 ) ) ;
#102221 = CARTESIAN_POINT ( 'NONE',  ( 6.576141308597898139, 6.785670920958930985, -0.3094590540993913952 ) ) ;
#102222 = CARTESIAN_POINT ( 'NONE',  ( 1.827488212121135769, -1.941439008138484246, 0.6915448510415463934 ) ) ;
#102224 = CARTESIAN_POINT ( 'NONE',  ( 4.650083499807235121, 5.295740330745369207, 1.082471891955963716 ) ) ;
#102223 = CARTESIAN_POINT ( 'NONE',  ( -9.480175724453545172, 12.08329098332774265, 1.599625672291281386 ) ) ;
#102225 = CARTESIAN_POINT ( 'NONE',  ( -1.364683531250014514, 1.738541667008085545, -0.7879004041258289570 ) ) ;
#102226 = DIRECTION ( 'NONE',  ( 0.000000000000000000, 0.000000000000000000, 1.000000000000000000 ) ) ;
#102227 = ORIENTED_EDGE ( 'NONE', *, *, #14726, .T. ) ;
#102228 = CARTESIAN_POINT ( 'NONE',  ( 4.670513044250029999, 0.7352163052343118066, 1.765496816765201649 ) ) ;
#102229 = CARTESIAN_POINT ( 'NONE',  ( 6.666858444607468570, -2.065188582200903955, -0.9245386165244884324 ) ) ;
#102230 = CARTESIAN_POINT ( 'NONE',  ( -4.627410500965859264, 4.293067094081919777, 0.7998128361456341429 ) ) ;
#102231 = CARTESIAN_POINT ( 'NONE',  ( 0.8963918696095014571, -1.767652434117328308, -0.3957652751337119024 ) ) ;
#102232 = CARTESIAN_POINT ( 'NONE',  ( 0.7783702408986278298, -0.4687143430282306733, -1.857332652546606733 ) ) ;
#102233 = CARTESIAN_POINT ( 'NONE',  ( 2.207561477879273593, -1.661462528888792090, -1.235070534849058266 ) ) ;
#102234 = CARTESIAN_POINT ( 'NONE',  ( -0.6823417656250246877, 0.1135416670080893753, 1.181850606188755259 ) ) ;
#102235 = CARTESIAN_POINT ( 'NONE',  ( 0.7605432175010603535, -1.429589592961340028, 1.357792370201470256 ) ) ;
#102236 = CARTESIAN_POINT ( 'NONE',  ( 5.443948574151852959, 0.7788650187186187956, -1.762213160536057144 ) ) ;
#102238 = CARTESIAN_POINT ( 'NONE',  ( 6.474762296362193581, 6.758873339713582062, -0.2294044474360455721 ) ) ;
#102237 = CARTESIAN_POINT ( 'NONE',  ( 6.709632191794143274, -0.4886956906769434061, 2.160084693451309601 ) ) ;
#102239 = CARTESIAN_POINT ( 'NONE',  ( -0.6823417656250003738, 1.717708333674752730, -1.181850606188749264 ) ) ;
#102240 = CARTESIAN_POINT ( 'NONE',  ( 4.352046829380719295, -0.7922827022245787498, 1.904640004429495326 ) ) ;
#102241 = CARTESIAN_POINT ( 'NONE',  ( -6.226218857173722476, 8.287007971501239467, 1.599625672291283607 ) ) ;
#102242 = CARTESIAN_POINT ( 'NONE',  ( 8.586391356156291010, 8.911878091804165791, 0.7998128361456481317 ) ) ;
#102243 = CARTESIAN_POINT ( 'NONE',  ( 4.813308228051395687, 5.574280006603454574, 1.199719254218462483 ) ) ;
#102244 = CARTESIAN_POINT ( 'NONE',  ( 5.331380718671758778, 7.243030143248949670, -1.599625672291256295 ) ) ;
#102246 = CARTESIAN_POINT ( 'NONE',  ( -1.499999999999997780, 3.900000000000021672, 1.214306433183764966E-14 ) ) ;
#102245 = CARTESIAN_POINT ( 'NONE',  ( 5.737368847912779124, -1.905360455185100887, 0.8973202462331535401 ) ) ;
#102247 = CARTESIAN_POINT ( 'NONE',  ( 6.812946544903684121, -1.603000239855886466, 1.309962327488790157 ) ) ;
#102248 = CARTESIAN_POINT ( 'NONE',  ( -1.364683531250012516, 1.342708333674755616, 0.7879004041258379498 ) ) ;
#102249 = CARTESIAN_POINT ( 'NONE',  ( 5.220075184997099882, -1.151474455836385857, -1.829185309946822713 ) ) ;
#102250 = CARTESIAN_POINT ( 'NONE',  ( 4.037763967290787903, -1.932009543340426072, 0.5885129382087511685 ) ) ;
#102251 = CARTESIAN_POINT ( 'NONE',  ( 6.620655732516649294, 2.950034989283246478, 2.626075342966327497 ) ) ;
#102254 = CARTESIAN_POINT ( 'NONE',  ( 5.287316719649520991, 8.151991358691011769, -1.082531754730549078 ) ) ;
#102253 = CARTESIAN_POINT ( 'NONE',  ( 1.642778471875001811, -1.392708332855374653, 2.845375778867859751 ) ) ;
#102252 = FACE_OUTER_BOUND ( 'NONE', #6255, .T. ) ;
#102255 = CARTESIAN_POINT ( 'NONE',  ( -4.956387674247580755, 7.940146832334256111, 1.199719254218452935 ) ) ;
#102256 = CARTESIAN_POINT ( 'NONE',  ( 2.553923023464285347, 1.082840749376843270, 1.700961377887353798 ) ) ;
#102257 = CARTESIAN_POINT ( 'NONE',  ( -7.666245793523398078, 11.03137162816423356, 1.199719254218453823 ) ) ;
#102258 = CARTESIAN_POINT ( 'NONE',  ( -5.576481253922474401, 5.400316305864651056, -0.7998128361456221525 ) ) ;
#102259 = CARTESIAN_POINT ( 'NONE',  ( -11.97185388258315086, 12.22000009279607546, -0.8311143155443164732 ) ) ;
#102260 = CARTESIAN_POINT ( 'NONE',  ( 6.595517585942704208, -7.896420114628012854, 7.253242555595321051 ) ) ;
#102261 = ADVANCED_FACE ( 'NONE', ( #118224 ), #3311, .T. ) ;
#102263 = CARTESIAN_POINT ( 'NONE',  ( 4.816029892389546596, 1.034148959857810190, -1.730877356967218894 ) ) ;
#102262 = CARTESIAN_POINT ( 'NONE',  ( -6.466876083594135238, 9.528143949959703818, 1.082531754730548412 ) ) ;
#102264 = CARTESIAN_POINT ( 'NONE',  ( -1.201851678989727383E-14, 5.587500000000021672, -1.732050807568863648 ) ) ;
#102265 = CARTESIAN_POINT ( 'NONE',  ( 1.171983892495536805, -1.097183398155553435, 1.330944738974817243 ) ) ;
#102266 = CARTESIAN_POINT ( 'NONE',  ( 5.631432701629774051, 7.663367133358481631, 1.599625672291269396 ) ) ;
#102268 = CARTESIAN_POINT ( 'NONE',  ( 1.814759087649938429, 3.975067388631681187, 0.4606438099578180068 ) ) ;
#102267 = CARTESIAN_POINT ( 'NONE',  ( 7.619319141200057821, 10.87266085050000974, 1.082531754730557072 ) ) ;
#102269 = LINE ( 'NONE', #53522, #171587 ) ;
#102270 = CARTESIAN_POINT ( 'NONE',  ( 5.923093557443566581, -0.04637014295935313474, 1.870147476527424635 ) ) ;
#102271 = CARTESIAN_POINT ( 'NONE',  ( 6.328391183068679204, -0.9529656412403487709, -1.773404795463069838 ) ) ;
#102272 = CARTESIAN_POINT ( 'NONE',  ( -5.546694241322218666, 8.524874810634301525, 1.082531754730550855 ) ) ;
#102273 = ORIENTED_EDGE ( 'NONE', *, *, #82128, .T. ) ;
#102274 = CARTESIAN_POINT ( 'NONE',  ( 8.703971429848968100, 13.09845773489176679, 0.000000000000000000 ) ) ;
#102275 = CARTESIAN_POINT ( 'NONE',  ( 0.9488424731869498086, -1.824129051820524205, -0.8596123018156722750 ) ) ;
#102276 = CARTESIAN_POINT ( 'NONE',  ( 1.265540092975623088, 0.5243090560775253151, -1.734071359953066382 ) ) ;
#102277 = CARTESIAN_POINT ( 'NONE',  ( 7.550965208168244125, 7.774157262476569130, -0.7998128361456341429 ) ) ;
#102278 = CARTESIAN_POINT ( 'NONE',  ( 5.823154874416164084, -0.05760400987671504547, 2.161107263091876618 ) ) ;
#102279 = AXIS2_PLACEMENT_3D ( 'NONE', #66440, #20893, #115295 ) ;
#102280 = CARTESIAN_POINT ( 'NONE',  ( 6.317209508963599340, 9.457495962844502557, 1.199719254218462483 ) ) ;
#102282 = CARTESIAN_POINT ( 'NONE',  ( -0.2060670157024322158, -0.8220983527124374746, -1.729069022899624164 ) ) ;
#102281 = CARTESIAN_POINT ( 'NONE',  ( -4.985647801523292344, 6.839675073242382553, -1.599625672291256295 ) ) ;
#102283 = CARTESIAN_POINT ( 'NONE',  ( 1.850900803405173489, 8.952907405788534945, 0.7750000000000004663 ) ) ;
#102284 = FACE_OUTER_BOUND ( 'NONE', #26455, .T. ) ;
#102286 = EDGE_CURVE ( 'NONE', #14247, #14615, #188803, .T. ) ;
#102285 =( BOUNDED_CURVE ( )  B_SPLINE_CURVE ( 2, ( #117415, #70699, #120632, #102168, #200704 ),
 .UNSPECIFIED., .F., .T. ) 
 B_SPLINE_CURVE_WITH_KNOTS ( ( 3, 2, 3 ),
 ( 0.1122816501277887347, 0.1125000000000000028, 0.1129944696182164920 ),
 .UNSPECIFIED. ) 
 CURVE ( )  GEOMETRIC_REPRESENTATION_ITEM ( )  RATIONAL_B_SPLINE_CURVE ( ( 0.9866942343795583881, 0.9929791993688261709, 1.000000000000000000, 0.9841008718140600298, 0.9719753288332768637 ) ) 
 REPRESENTATION_ITEM ( '' )  );
#102287 = CIRCLE ( 'NONE', #1914, 0.04999999999999991257 ) ;
#102288 = CARTESIAN_POINT ( 'NONE',  ( 5.626270559546810546, 8.547437505237857280, 1.082531754730558626 ) ) ;
#102289 = CARTESIAN_POINT ( 'NONE',  ( -1.364683531250014514, -0.9489583329919112353, -0.7879004041258359514 ) ) ;
#102291 = ORIENTED_EDGE ( 'NONE', *, *, #66894, .T. ) ;
#102290 = CARTESIAN_POINT ( 'NONE',  ( 2.738383840280320669, 6.138605547061593448, 0.7216878364870338292 ) ) ;
#102292 = CARTESIAN_POINT ( 'NONE',  ( -4.485049888022365927, 4.126979712314507331, 0.7998128361456341429 ) ) ;
#102293 = CARTESIAN_POINT ( 'NONE',  ( 3.801785103514757846, -0.6297183656660889639, 2.067937956787009757 ) ) ;
#102294 = CARTESIAN_POINT ( 'NONE',  ( -5.289089323106922258, 9.184704953684462936, 0.7216878364870267237 ) ) ;
#102295 = CARTESIAN_POINT ( 'NONE',  ( 6.563555762791525972, 6.830105609444471426, -0.7216878364870458196 ) ) ;
#102296 = CARTESIAN_POINT ( 'NONE',  ( 0.8441712343106638761, -1.349783269286155996, -1.635521010841307410 ) ) ;
#102297 = CARTESIAN_POINT ( 'NONE',  ( 0.000000000000000000, 3.500000000000003109, 0.000000000000000000 ) ) ;
#102298 = CARTESIAN_POINT ( 'NONE',  ( 2.073447407941295673, 1.887670557785134928, -0.5683696268203948243 ) ) ;
#102299 = CARTESIAN_POINT ( 'NONE',  ( 4.992401499097729456, -1.057410677138232780, 1.593263788312593743 ) ) ;
#102300 = ORIENTED_EDGE ( 'NONE', *, *, #82643, .F. ) ;
#102301 = PLANE ( 'NONE',  #28545 ) ;
#102302 = CARTESIAN_POINT ( 'NONE',  ( 6.250452387334210158, -1.959941389959872549, -0.1944618805250642457 ) ) ;
#102303 = CARTESIAN_POINT ( 'NONE',  ( 0.7263842893957738189, 0.1423072432159468159, 1.936797167885440096 ) ) ;
#102304 = EDGE_LOOP ( 'NONE', ( #94404, #142148, #115106, #85853 ) ) ;
#102305 = CARTESIAN_POINT ( 'NONE',  ( -3.786470039966538970, 7.639575156594750283, 0.000000000000000000 ) ) ;
#102306 = CARTESIAN_POINT ( 'NONE',  ( -3.311934663488232733, 7.085950550703385531, -0.7998128361456481317 ) ) ;
#102308 = CARTESIAN_POINT ( 'NONE',  ( 5.167065940139554669, 9.042344340222555843, -0.7216878364870458196 ) ) ;
#102307 = CARTESIAN_POINT ( 'NONE',  ( 7.145310649601935182, 8.294949498412453437, -1.199719254218446718 ) ) ;
#102310 = ORIENTED_EDGE ( 'NONE', *, *, #91921, .T. ) ;
#102309 = CARTESIAN_POINT ( 'NONE',  ( 4.582611755193141789, -1.246403352314252810, 1.450376384258989182 ) ) ;
#102311 = CARTESIAN_POINT ( 'NONE',  ( 3.229339687698820072, 0.05429069646168545316, 2.206380697113208722 ) ) ;
#102312 = CARTESIAN_POINT ( 'NONE',  ( 1.958336283151569157, 2.200835622443702011, -0.1624582802550941507 ) ) ;
#102313 = CARTESIAN_POINT ( 'NONE',  ( 6.518203450479811423, 5.167241622962441383, -2.437504649502886256 ) ) ;
#102314 = CARTESIAN_POINT ( 'NONE',  ( 0.2055213853429035953, 1.417038256915002181, 1.284265443176696442 ) ) ;
#102315 = CARTESIAN_POINT ( 'NONE',  ( 3.834746474454188013E-15, 8.812500000000000000, 1.500000000000001554 ) ) ;
#102316 = CARTESIAN_POINT ( 'NONE',  ( -0.008622056139523381901, 15.44694768828586540, 11.95585894197802013 ) ) ;
#102317 = CARTESIAN_POINT ( 'NONE',  ( -6.653311379900198830, -6.675176078274440705, -6.940534579975141227 ) ) ;
#102318 = CARTESIAN_POINT ( 'NONE',  ( 2.980987059868036138, 1.948563265827065960, 0.6999735360200682877 ) ) ;
#102319 = CARTESIAN_POINT ( 'NONE',  ( -5.708146366553361162, 6.618257834855742594, -1.199719254218446718 ) ) ;
#102320 = AXIS2_PLACEMENT_3D ( 'NONE', #163844, #127149, #96730 ) ;
#102321 = CARTESIAN_POINT ( 'NONE',  ( -4.807049873888117553, 8.139959938814184781, 0.8294007104595437774 ) ) ;
#102323 = CARTESIAN_POINT ( 'NONE',  ( 0.7257156204387126275, -2.052300050329861847, 0.6792298617422781737 ) ) ;
#102322 = CARTESIAN_POINT ( 'NONE',  ( -3.415764635639130020, 6.072476943965863683, 1.199719254218462483 ) ) ;
#102324 = CARTESIAN_POINT ( 'NONE',  ( 2.929422067023911502, -1.473737196803912797, -1.622193633833472814 ) ) ;
#102325 = CARTESIAN_POINT ( 'NONE',  ( -1.499999999999946709, 7.750000000000000000, 15.75000000000000711 ) ) ;
#102326 = CARTESIAN_POINT ( 'NONE',  ( 3.933273961740298752, 5.682181936820735579, 1.443375672974058777 ) ) ;
#102327 = CARTESIAN_POINT ( 'NONE',  ( 1.499999999999996891, 12.89583333333333215, -0.8660254037844378194 ) ) ;
#102328 = CARTESIAN_POINT ( 'NONE',  ( 1.364683531250000303, 13.31770833367472839, -0.7879004041258355073 ) ) ;
#102329 = CARTESIAN_POINT ( 'NONE',  ( -4.444040490229335560, 8.406740681901359480, 0.7998128361456352531 ) ) ;
#102330 = UNCERTAINTY_MEASURE_WITH_UNIT (LENGTH_MEASURE( 1.000000000000000082E-05 ), #77369, 'distance_accuracy_value', 'NONE');
#102331 = CARTESIAN_POINT ( 'NONE',  ( 6.012339335674446339, -1.629552802491928354, 0.5935831289462877303 ) ) ;
#102332 = MECHANICAL_DESIGN_GEOMETRIC_PRESENTATION_REPRESENTATION (  '', ( #8954 ), #12500 ) ;
#102333 = CARTESIAN_POINT ( 'NONE',  ( -3.765413976293358278, 5.416068943807445635, 1.599625672291267398 ) ) ;
#102334 = CARTESIAN_POINT ( 'NONE',  ( 3.467693386974544545, -0.4085244671708112008, 2.029378838279243258 ) ) ;
#102335 = CARTESIAN_POINT ( 'NONE',  ( 4.218443861432810138, 2.076744001477859314, 0.4112613105302816430 ) ) ;
#102336 = CARTESIAN_POINT ( 'NONE',  ( 6.449928391799196525, 8.548002428564306143, -1.599625672291262513 ) ) ;
#102337 = CARTESIAN_POINT ( 'NONE',  ( -1.201851678989727383E-14, 4.446875000341417916, -1.575800808251660134 ) ) ;
#102338 = CARTESIAN_POINT ( 'NONE',  ( 3.397268178914572889, -1.739110600408208196, 0.9241587964883835049 ) ) ;
#102339 = CARTESIAN_POINT ( 'NONE',  ( 0.5977379272000953314, 1.286164058678052946, 1.415416067018962165 ) ) ;
#102340 = CARTESIAN_POINT ( 'NONE',  ( 5.384854118993849248, 2.023671607873143152, -1.076698936902406922 ) ) ;
#102341 = CARTESIAN_POINT ( 'NONE',  ( 2.824607995650964209, 1.719152210223941601, 0.6149139946348626262 ) ) ;
#102342 = CIRCLE ( 'NONE', #50402, 11.09999999999999964 ) ;
#102343 = CARTESIAN_POINT ( 'NONE',  ( 5.578253857379852576, 5.472660686556754861, -0.7998128361456481317 ) ) ;
#102344 = CARTESIAN_POINT ( 'NONE',  ( 6.005898860729467437, 7.069598761348265370, -1.082531754730543083 ) ) ;
#102345 = CARTESIAN_POINT ( 'NONE',  ( -7.369020184227459858, 8.555943955475521889, 1.199719254218450271 ) ) ;
#102346 = CARTESIAN_POINT ( 'NONE',  ( 4.060795210881157580, 0.5408870827437872730, 1.939095388008914345 ) ) ;
#102347 = CARTESIAN_POINT ( 'NONE',  ( 4.856279117655732058, -1.961245242753749674, -0.05215834203427943683 ) ) ;
#102348 = CARTESIAN_POINT ( 'NONE',  ( -7.157815033010924921, 10.43820240756634199, 1.199719254218453823 ) ) ;
#102349 = CARTESIAN_POINT ( 'NONE',  ( -5.331380718671772101, 7.243030143248949670, -1.599625672291256295 ) ) ;
#102350 = CARTESIAN_POINT ( 'NONE',  ( 0.1753634416057497925, 6.947017063990798214, -2.739087685391654148 ) ) ;
#102352 = CARTESIAN_POINT ( 'NONE',  ( 5.823074959372767090, -0.03971387110058427483, 1.769581062106811986 ) ) ;
#102351 = CARTESIAN_POINT ( 'NONE',  ( 0.8903107040577078468, -0.5117213476562210150, -2.027015703535272717 ) ) ;
#102353 = DIRECTION ( 'NONE',  ( 0.000000000000000000, 8.546850786086437571E-32, 1.000000000000000000 ) ) ;
#102354 = CARTESIAN_POINT ( 'NONE',  ( 1.939652437182255662, 0.8368340126228106524, -2.025574644071465258 ) ) ;
#102355 = CARTESIAN_POINT ( 'NONE',  ( 6.544851825567233661, -1.402524398529688021, -1.030163739638074727 ) ) ;
#102356 = CARTESIAN_POINT ( 'NONE',  ( 6.588372581236919601, 9.773852880496709972, -1.199719254218440723 ) ) ;
#102357 = CARTESIAN_POINT ( 'NONE',  ( 0.1333692844072767447, 1.351132181276387678, -2.308013766563504987 ) ) ;
#102358 = CARTESIAN_POINT ( 'NONE',  ( 0.8555558213108410692, 1.723155885897029282, -0.08016331026279581440 ) ) ;
#102359 = CARTESIAN_POINT ( 'NONE',  ( 0.9315567102232256147, 1.134920720140248251, 1.998545780126102844 ) ) ;
#102360 = CARTESIAN_POINT ( 'NONE',  ( 0.1698123575781598782, 1.266975945507025081, 1.788028528876134393 ) ) ;
#102361 = CARTESIAN_POINT ( 'NONE',  ( 6.485661447747480324, 1.619333758318822536, 0.6201139256068515238 ) ) ;
#102362 = CARTESIAN_POINT ( 'NONE',  ( 2.420803835572300500, 1.440536793087299205, -1.671967039616916617 ) ) ;
#102363 =( BOUNDED_SURFACE ( )  B_SPLINE_SURFACE ( 3, 2, ( 
 ( #165375, #32183, #33242 ),
 ( #201048, #69979, #83049 ),
 ( #101441, #182682, #136090 ),
 ( #149124, #48456, #85190 ),
 ( #20174, #66770, #152332 ),
 ( #3909, #132911, #135035 ) ),
 .UNSPECIFIED., .F., .F., .T. ) 
 B_SPLINE_SURFACE_WITH_KNOTS ( ( 4, 2, 4 ),
 ( 3, 3 ),
 ( 0.000000000000000000, 0.002122857551078454266, 0.004245715102156908533 ),
 ( 0.000000000000000000, 1.000000000000000000 ),
 .UNSPECIFIED. ) 
 GEOMETRIC_REPRESENTATION_ITEM ( )  RATIONAL_B_SPLINE_SURFACE ( (
 ( 1.000000000000000000, 0.7806433624857567199, 1.000000000000000000),
 ( 1.000000000000000000, 0.7860453980259759499, 1.000000000000000000),
 ( 1.000000000000000000, 0.7924770197564218188, 1.000000000000000000),
 ( 1.000000000000000000, 0.8094762427233131996, 1.000000000000000000),
 ( 1.000000000000000000, 0.8200718518785214961, 1.000000000000000000),
 ( 1.000000000000000000, 0.8343063410434347071, 1.000000000000000000) ) ) 
 REPRESENTATION_ITEM ( '' )  SURFACE ( )  );
#102364 = CARTESIAN_POINT ( 'NONE',  ( 0.6730172731169652423, 1.498246551899045098, -1.571433807820749706 ) ) ;
#102365 = CARTESIAN_POINT ( 'NONE',  ( -1.499999999999997780, 3.900000000000021672, 1.214306433183764966E-14 ) ) ;
#102366 = CARTESIAN_POINT ( 'NONE',  ( 1.165409582065090266, 1.953992404094638591, -0.8159742408818432269 ) ) ;
#102367 = CARTESIAN_POINT ( 'NONE',  ( 6.827182134110230116, 2.398703475977175703, 2.668604416072619223 ) ) ;
#102368 = CARTESIAN_POINT ( 'NONE',  ( 5.930678043039342207, 1.856691256794128053, 0.5132231078649931444 ) ) ;
#102369 = ORIENTED_EDGE ( 'NONE', *, *, #21723, .T. ) ;
#102371 = CARTESIAN_POINT ( 'NONE',  ( -1.402160292154681736E-14, -1.115624999658584082, 1.575800808251672791 ) ) ;
#102370 = CARTESIAN_POINT ( 'NONE',  ( 1.839794590071419211, 0.8728355696882350578, -2.119893007042342958 ) ) ;
#102372 = CARTESIAN_POINT ( 'NONE',  ( 3.440018289565364817, 5.036440642624797626, 1.599625672291267398 ) ) ;
#102373 = CARTESIAN_POINT ( 'NONE',  ( 6.006425746053997372, 6.966250444273174303, -1.199719254218445830 ) ) ;
#102374 = CARTESIAN_POINT ( 'NONE',  ( 3.703960633009816483, 1.609604546992912999, 1.531039788047829253 ) ) ;
#102375 = CARTESIAN_POINT ( 'NONE',  ( -6.832946231607472498, 9.955225789308602913, 1.082531754730549967 ) ) ;
#102377 = EDGE_CURVE ( 'NONE', #152468, #30835, #171171, .T. ) ;
#102376 =( LENGTH_UNIT ( ) NAMED_UNIT ( * ) SI_UNIT ( .MILLI., .METRE. ) );
#102378 = CARTESIAN_POINT ( 'NONE',  ( 4.853455804012212660, 7.645820290447483458, 1.082531754730558626 ) ) ;
#102379 = CARTESIAN_POINT ( 'NONE',  ( -7.741342523278709642, 10.05465224862374285, 1.443375672974090751 ) ) ;
#102380 = CARTESIAN_POINT ( 'NONE',  ( 5.153507786970260796, 7.105788066255672497, -1.443375672974078761 ) ) ;
#102381 = ORIENTED_EDGE ( 'NONE', *, *, #54983, .T. ) ;
#102382 = ORIENTED_EDGE ( 'NONE', *, *, #25508, .F. ) ;
#102383 = CARTESIAN_POINT ( 'NONE',  ( 2.074842474778653134, -0.8596299393073093542, 1.824119475507138821 ) ) ;
#102385 = CARTESIAN_POINT ( 'NONE',  ( 1.024372331059967056, 1.013329571420513053, 1.796381585629814426 ) ) ;
#102384 = CARTESIAN_POINT ( 'NONE',  ( 8.776205506747620788, 9.133327934160710981, -0.7998128361456221525 ) ) ;
#102386 = PRESENTATION_STYLE_ASSIGNMENT (( #50446 ) ) ;
#102387 = CARTESIAN_POINT ( 'NONE',  ( 5.844973620822835336, 7.912498205750389424, 1.443375672974064550 ) ) ;
#102388 = CARTESIAN_POINT ( 'NONE',  ( 10.23203630735456393, -6.594478602028841507, -1.760317133499381158E-15 ) ) ;
#102389 = CARTESIAN_POINT ( 'NONE',  ( 1.364683531249988535, 4.113541667008088432, 0.7879004041258500513 ) ) ;
#102390 = CARTESIAN_POINT ( 'NONE',  ( 4.171962795014371395, -1.262591954434747921, 1.790989659139609724 ) ) ;
#102391 = CARTESIAN_POINT ( 'NONE',  ( 1.582657950916711131, -0.6767122143778031562, 1.899619169727875700 ) ) ;
#102392 = CARTESIAN_POINT ( 'NONE',  ( -0.04178991631376138827, -1.644041690304678616, -0.8291446804715857377 ) ) ;
#102393 = CARTESIAN_POINT ( 'NONE',  ( 5.812145867431055102, 1.542159960141289199, -1.696276722712148688 ) ) ;
#102394 = CARTESIAN_POINT ( 'NONE',  ( 3.486116527793288178, -0.3603757036649730128, -1.805346353211812804 ) ) ;
#102395 = CARTESIAN_POINT ( 'NONE',  ( 8.235688245297327015, 11.69572115523387268, -1.199719254218446718 ) ) ;
#102396 = CARTESIAN_POINT ( 'NONE',  ( 4.014527796464135712, 1.291161025869846712, -1.290856679043244970 ) ) ;
#102397 = CARTESIAN_POINT ( 'NONE',  ( 5.326796142270829648, 0.8146286751641409474, -1.844708973168760924 ) ) ;
#102398 = CARTESIAN_POINT ( 'NONE',  ( -9.677822722056413696, 10.18521468535430685, 1.040834085586084257E-14 ) ) ;
#102400 = CARTESIAN_POINT ( 'NONE',  ( -6.903036488013351679, 8.082572653217566128, -1.199719254218452047 ) ) ;
#102399 = CARTESIAN_POINT ( 'NONE',  ( 4.399490234458226290, 1.814852776126129497, 1.350843829522253792 ) ) ;
#102401 = CARTESIAN_POINT ( 'NONE',  ( 6.124072230051534227, -1.166888049220366597, -1.752910934067633875 ) ) ;
#102402 = DIRECTION ( 'NONE',  ( -0.1510067114093955887, 0.000000000000000000, 0.9885327375000383388 ) ) ;
#102403 = CARTESIAN_POINT ( 'NONE',  ( 4.141125838365485201, -0.1998502692034490602, -2.060677327190631569 ) ) ;
#102404 = CARTESIAN_POINT ( 'NONE',  ( 4.054051625686104998, 4.688480637177271149, -1.199719254218446718 ) ) ;
#102405 = CARTESIAN_POINT ( 'NONE',  ( -0.6801582343750265380, 1.463541667008072533, 1.178068619123799898 ) ) ;
#102406 = PRODUCT_CONTEXT ( 'NONE', #49107, 'mechanical' ) ;
#102407 = B_SPLINE_CURVE_WITH_KNOTS ( 'NONE', 3,
 ( #31759, #99943, #128277, #29621, #50130, #33865, #12275, #78351, #178005, #132483, #114140, #162827, #97830, #163895, #144474, #148698 ),
 .UNSPECIFIED., .F., .F.,
 ( 4, 3, 3, 3, 3, 4 ),
 ( 0.000000000000000000, 4.381999914579370578E-06, 1.110488615493398738E-05, 1.784390311306881054E-05, 2.460054645147356366E-05, 3.136851507421863007E-05 ),
 .UNSPECIFIED. ) ;
#102409 = CARTESIAN_POINT ( 'NONE',  ( 2.367692237863534555, 1.889325326408105576, -0.3758258368516536052 ) ) ;
#102408 = CARTESIAN_POINT ( 'NONE',  ( -9.450196763925152510, 10.98398329845622001, -1.199719254218441611 ) ) ;
#102410 = CARTESIAN_POINT ( 'NONE',  ( 4.800089777832203808, 5.120415418395356077, -0.7784788408505428636 ) ) ;
#102411 = CARTESIAN_POINT ( 'NONE',  ( 0.4320049508096295288, 1.131045402950446199, 1.612214446364314213 ) ) ;
#102412 = CARTESIAN_POINT ( 'NONE',  ( 4.326460416092276162, 7.101268681199365496, -1.082531754730548412 ) ) ;
#102413 = CARTESIAN_POINT ( 'NONE',  ( 5.886424920137334205, 5.980649323864647648, 0.1385726864747312270 ) ) ;
#102414 = CARTESIAN_POINT ( 'NONE',  ( 10.42995565840374184, 1.000000000000000888, -5.797106512947759249 ) ) ;
#102415 = CARTESIAN_POINT ( 'NONE',  ( -2.767835915484202047, 6.380892334706859792, -0.7998128361456281477 ) ) ;
#102416 = CARTESIAN_POINT ( 'NONE',  ( 1.793536179914383188, -0.1149406603053771958, -2.218580859979270681 ) ) ;
#102417 = CARTESIAN_POINT ( 'NONE',  ( 2.960101939890079858, 2.095960298449873971, -0.2048252169620876917 ) ) ;
#102418 = CARTESIAN_POINT ( 'NONE',  ( -6.587282531393266360, 8.778525268082516320, 1.599625672291269396 ) ) ;
#102419 = CARTESIAN_POINT ( 'NONE',  ( 5.926885707468349196, 10.06645042535509660, 1.040834085586084257E-14 ) ) ;
#102420 = CARTESIAN_POINT ( 'NONE',  ( 0.9239872072115723478, 0.9125040393608827571, 1.621899335316509649 ) ) ;
#102421 = CARTESIAN_POINT ( 'NONE',  ( 5.829115978871627135, 8.888053511070525659, 1.199719254218462483 ) ) ;
#102422 = CARTESIAN_POINT ( 'NONE',  ( 4.497554271431305040, 6.270232621468402989, -1.599625672291256295 ) ) ;
#102423 = CARTESIAN_POINT ( 'NONE',  ( -5.126391479742927970, 8.994890803093138487, 0.7216878364870267237 ) ) ;
#102424 = CARTESIAN_POINT ( 'NONE',  ( -7.036318535812428721, 11.15286269184909784, 0.000000000000000000 ) ) ;
#102425 = CARTESIAN_POINT ( 'NONE',  ( 1.723052270212792836, 1.567896913533245229, -1.427966198690698851 ) ) ;
#102426 = CARTESIAN_POINT ( 'NONE',  ( -7.761116589180078407, 8.019333873657032541, 0.000000000000000000 ) ) ;
#102428 = CARTESIAN_POINT ( 'NONE',  ( 4.492601031306558745, 1.923586649950057792, 0.3847822903023030428 ) ) ;
#102427 = CARTESIAN_POINT ( 'NONE',  ( -3.555477883677943599E-14, 1.187500000000005773, -1.414508159514621610 ) ) ;
#102429 = CARTESIAN_POINT ( 'NONE',  ( 3.274459119871219848, -1.289031633699176949, 1.735169069618908821 ) ) ;
#102430 = CARTESIAN_POINT ( 'NONE',  ( 2.050122339901743196, -1.422379512129726908, 1.169167124061460949 ) ) ;
#102431 = CARTESIAN_POINT ( 'NONE',  ( -4.016817522127867690, 7.623078265842172740, -0.1143880650965305862 ) ) ;
#102432 = EDGE_CURVE ( 'NONE', #31312, #94484, #129432, .T. ) ;
#102433 = CARTESIAN_POINT ( 'NONE',  ( 5.033026810027643627, -1.234204449110408053, -1.227257546430237989 ) ) ;
#102434 = CARTESIAN_POINT ( 'NONE',  ( 4.044555541517573793, 7.746237447724527492, 0.4662041258270445132 ) ) ;
#102435 = CARTESIAN_POINT ( 'NONE',  ( 5.016153647376201619, 7.835634441038803466, 1.082531754730558626 ) ) ;
#102436 = CARTESIAN_POINT ( 'NONE',  ( -10.12885446735897510, 6.153639267710001803, -5.673676530672286944 ) ) ;
#102437 = CARTESIAN_POINT ( 'NONE',  ( 1.499129196564863209, 1.767075381950654611, -1.244890797856931686 ) ) ;
#102438 = AXIS2_PLACEMENT_3D ( 'NONE', #188570, #42350, #208012 ) ;
#102439 = CARTESIAN_POINT ( 'NONE',  ( 3.286482353612128815, -1.943773746517188039, 0.5350062169211177165 ) ) ;
#102440 = CARTESIAN_POINT ( 'NONE',  ( -8.609064354553318310, 12.98773281371349775, 0.7216878364870317197 ) ) ;
#102441 = CARTESIAN_POINT ( 'NONE',  ( 0.7608789386071808103, -1.564954856162886765, 1.491513986042219297 ) ) ;
#102442 = CARTESIAN_POINT ( 'NONE',  ( 3.836761837097919070, 0.2881357685159210424, 1.950175340126619306 ) ) ;
#102443 =( GEOMETRIC_REPRESENTATION_CONTEXT ( 3 ) GLOBAL_UNCERTAINTY_ASSIGNED_CONTEXT ( ( #182863 ) ) GLOBAL_UNIT_ASSIGNED_CONTEXT ( ( #183635, #87207, #51518 ) ) REPRESENTATION_CONTEXT ( 'NONE', 'WORKASPACE' ) );
#102444 = ADVANCED_FACE ( 'NONE', ( #134448 ), #36897, .T. ) ;
#102445 = CARTESIAN_POINT ( 'NONE',  ( 6.609000000000052388, 1.285212548570794588, 2.017169166534539038 ) ) ;
#102446 = CARTESIAN_POINT ( 'NONE',  ( 2.999484396081523396, -1.939716604588328508, 0.09806999327347488971 ) ) ;
#102449 = VERTEX_POINT ( 'NONE', #22761 ) ;
#102448 = CARTESIAN_POINT ( 'NONE',  ( -3.689227196694346400, 6.357829925235092716, -1.082531754730546636 ) ) ;
#102447 = CARTESIAN_POINT ( 'NONE',  ( -8.785320351530977234, 13.19336481018743079, 1.040834085586084257E-14 ) ) ;
#102451 = EDGE_CURVE ( 'NONE', #201520, #173093, #200359, .T. ) ;
#102450 = CARTESIAN_POINT ( 'NONE',  ( -3.797692425159308716, 7.444741906078900406, 0.000000000000000000 ) ) ;
#102452 = CARTESIAN_POINT ( 'NONE',  ( -0.1110810684432622653, 2.888487728959455936, -2.285870655067727242 ) ) ;
#102453 = CARTESIAN_POINT ( 'NONE',  ( 5.411639590510088027, 6.342609606130419131, -1.199719254218452047 ) ) ;
#102454 = CARTESIAN_POINT ( 'NONE',  ( -4.630991987519598396, 7.560518531151607213, 1.199719254218452935 ) ) ;
#102456 = ORIENTED_EDGE ( 'NONE', *, *, #170447, .T. ) ;
#102455 = CARTESIAN_POINT ( 'NONE',  ( -7.781453819600577582, 8.043060642480948985, 0.000000000000000000 ) ) ;
#102457 = CARTESIAN_POINT ( 'NONE',  ( -9.612367721964613310, 11.27714576612263997, -1.082531754730537976 ) ) ;
#102458 = CARTESIAN_POINT ( 'NONE',  ( 6.739320262688799801, -2.065560010629815313, 1.029036360498974068 ) ) ;
#102459 = CARTESIAN_POINT ( 'NONE',  ( 0.000000000000000000, -4.046874999522043659, -3.793834371823813001 ) ) ;
#102460 = CARTESIAN_POINT ( 'NONE',  ( 3.854310441289869882, -1.959320932037407426, -0.1006921081871253454 ) ) ;
#102461 = CARTESIAN_POINT ( 'NONE',  ( 8.769426429940780920, 9.125419011219408461, 0.7998128361456462443 ) ) ;
#102462 = CARTESIAN_POINT ( 'NONE',  ( 1.723279953462612202, 1.994870059565261755, 0.2930690452552578429 ) ) ;
#102463 = VERTEX_POINT ( 'NONE', #157075 ) ;
#102464 = CARTESIAN_POINT ( 'NONE',  ( 3.397769718358482738, -2.085282637925215177, 0.3663039253445389276 ) ) ;
#102465 = CARTESIAN_POINT ( 'NONE',  ( 0.7499999999999902300, 1.264583334016147642, 1.299038105676657340 ) ) ;
#102467 = CARTESIAN_POINT ( 'NONE',  ( -6.392833124043511894, 7.417059051927569868, 1.199719254218450271 ) ) ;
#102466 = CARTESIAN_POINT ( 'NONE',  ( 0.1747926744264712562, 2.889263262932476817, -2.344248796821886138 ) ) ;
#102468 = CARTESIAN_POINT ( 'NONE',  ( 2.659893383946440260, -1.269561761542839617, 1.333649727802692198 ) ) ;
#102469 = VERTEX_POINT ( 'NONE', #142981 ) ;
#102470 = CARTESIAN_POINT ( 'NONE',  ( -7.700141177557535244, 11.07091624287075859, -1.199719254218446718 ) ) ;
#102471 = DIRECTION ( 'NONE',  ( -1.000000000000000000, -1.276756478318932585E-15, -3.330669073875474552E-16 ) ) ;
#102472 = CARTESIAN_POINT ( 'NONE',  ( 3.990573222356631256, -1.218298518170106925, 1.735533685479621502 ) ) ;
#102473 = CARTESIAN_POINT ( 'NONE',  ( 0.000000000000000000, 0.5000000000000004441, -3.475000000000000089 ) ) ;
#102474 = CARTESIAN_POINT ( 'NONE',  ( 7.772902139336337335, 7.962807338847539107, 0.7998128361456341429 ) ) ;
#102475 = VERTEX_POINT ( 'NONE', #139769 ) ;
#102476 = CARTESIAN_POINT ( 'NONE',  ( 5.325487547722469905, -1.958136382931666031, 0.6425617224121594750 ) ) ;
#102478 = CARTESIAN_POINT ( 'NONE',  ( 2.085277916773973228, -0.7859315772556186852, 1.665205719185464561 ) ) ;
#102477 = CARTESIAN_POINT ( 'NONE',  ( -6.632963465583701534, 8.761543347979550589, -1.599625672291263179 ) ) ;
#102479 = CARTESIAN_POINT ( 'NONE',  ( 8.341290820905593151, 10.75459192918846618, 1.599625672291281386 ) ) ;
#102480 = DIRECTION ( 'NONE',  ( -0.3502638921866464417, 1.953969548649013931E-16, 0.9366510587354618389 ) ) ;
#102481 = DIRECTION ( 'NONE',  ( 0.000000000000000000, 1.000000000000000000, 0.000000000000000000 ) ) ;
#102482 = CARTESIAN_POINT ( 'NONE',  ( -0.9398415344193471466, 7.435109595052176168, 4.383649807226260187 ) ) ;
#102483 = DIRECTION ( 'NONE',  ( 0.000000000000000000, 0.000000000000000000, -1.000000000000000000 ) ) ;
#102484 =( GEOMETRIC_REPRESENTATION_CONTEXT ( 3 ) GLOBAL_UNCERTAINTY_ASSIGNED_CONTEXT ( ( #77125 ) ) GLOBAL_UNIT_ASSIGNED_CONTEXT ( ( #69234, #165699, #17288 ) ) REPRESENTATION_CONTEXT ( 'NONE', 'WORKASPACE' ) );
#102485 = CARTESIAN_POINT ( 'NONE',  ( 2.121956728516772639, -2.140194184088719531, 0.5379336890513550795 ) ) ;
#102486 = CARTESIAN_POINT ( 'NONE',  ( 4.798257751182677389, -2.261729152689537781, -0.06211711723675371333 ) ) ;
#102487 = CARTESIAN_POINT ( 'NONE',  ( -8.215877900201387973, 8.687538426430837291, 0.7216878364870578100 ) ) ;
#102488 = CARTESIAN_POINT ( 'NONE',  ( 4.922017755325088118, -1.802143800875387614, 0.1849416998233286979 ) ) ;
#102489 = CARTESIAN_POINT ( 'NONE',  ( 3.942530958389865781, -1.415603592240498365, 1.290913190617749118 ) ) ;
#102490 = CARTESIAN_POINT ( 'NONE',  ( -0.6823417656249969321, 3.530208333674754506, -1.181850606188749264 ) ) ;
#102491 = CARTESIAN_POINT ( 'NONE',  ( 3.836761837097919070, 0.2881357685159210424, 1.950175340126619306 ) ) ;
#102492 = CARTESIAN_POINT ( 'NONE',  ( 5.612129163471575310, -0.8422657237196762292, -1.670366365510121742 ) ) ;
#102493 = CARTESIAN_POINT ( 'NONE',  ( 5.318752605461887661, -1.348013374683079135, 1.283375817886179826 ) ) ;
#102494 = CARTESIAN_POINT ( 'NONE',  ( 1.364683531249988535, 5.655208333674751842, -0.7879004041258300672 ) ) ;
#102495 = CARTESIAN_POINT ( 'NONE',  ( 0.005092704479254389627, -0.09411098085002241043, 2.014433268766747887 ) ) ;
#102497 = CARTESIAN_POINT ( 'NONE',  ( 2.033940956955893498, -1.376631898319637726, -1.593950314443808969 ) ) ;
#102496 = CARTESIAN_POINT ( 'NONE',  ( -4.243338890952916387, 4.052909582307567149, -0.7216878364870207285 ) ) ;
#102498 = CARTESIAN_POINT ( 'NONE',  ( 10.40996301719436090, 11.03937836301526687, 0.000000000000000000 ) ) ;
#102500 = CARTESIAN_POINT ( 'NONE',  ( 0.07479286986303290696, 5.725009232006174287, -2.449550298930736059 ) ) ;
#102499 = CARTESIAN_POINT ( 'NONE',  ( -0.6823417656250212460, 5.613541667008087543, 1.181850606188767472 ) ) ;
#102501 = CARTESIAN_POINT ( 'NONE',  ( 3.164422831683691761, 2.120778211551369807, -0.003951117757632071313 ) ) ;
#102502 = CARTESIAN_POINT ( 'NONE',  ( 0.000000000000000000, 13.49999999999999822, 0.000000000000000000 ) ) ;
#102503 = CARTESIAN_POINT ( 'NONE',  ( 2.056904690034748739, 0.4466968674397324701, 1.969590803855451933 ) ) ;
#102504 = CARTESIAN_POINT ( 'NONE',  ( -1.402160292154681736E-14, 1.696875000341421469, -1.575800808251659024 ) ) ;
#102505 = AXIS2_PLACEMENT_3D ( 'NONE', #156968, #20536, #4268 ) ;
#102506 = CARTESIAN_POINT ( 'NONE',  ( -3.389175213736311587, 4.977123720824209840, 1.443375672974064550 ) ) ;
#102507 = CARTESIAN_POINT ( 'NONE',  ( 4.578903193113299963, 6.365139696764064325, 1.599625672291267398 ) ) ;
#102508 = EDGE_LOOP ( 'NONE', ( #63315, #55490, #139621, #151607 ) ) ;
#102509 = CARTESIAN_POINT ( 'NONE',  ( 2.020999711022552159, 2.016103727727487804, 0.7800470891412072394 ) ) ;
#102510 = CARTESIAN_POINT ( 'NONE',  ( -5.229199737892074420E-15, 0.06250000000001598721, 1.224999999999961009 ) ) ;
#102512 = CARTESIAN_POINT ( 'NONE',  ( 4.216222584169931231, 4.021273891060765493, 1.214306433183764966E-14 ) ) ;
#102511 = CARTESIAN_POINT ( 'NONE',  ( 4.224247379109608680, 7.085983154673295203, -1.199719254218452047 ) ) ;
#102513 = CARTESIAN_POINT ( 'NONE',  ( -10.87339650836132776, 5.131772588966429183, -5.487095527168452058 ) ) ;
#102514 = CARTESIAN_POINT ( 'NONE',  ( -7.985752187169337546, -6.863172033215962031, 7.565242077046661073 ) ) ;
#102515 = CARTESIAN_POINT ( 'NONE',  ( -8.405692050792730186, 9.869357483088723626, 1.082531754730558626 ) ) ;
#102516 = CARTESIAN_POINT ( 'NONE',  ( 0.6443834720083198020, 0.6415979653194536780, 2.095529601600601755 ) ) ;
#102517 = CARTESIAN_POINT ( 'NONE',  ( -10.34545848478754593, -8.336144560139965520, 0.6172425113790593887 ) ) ;
#102519 = CARTESIAN_POINT ( 'NONE',  ( 0.6823417656249934904, 11.94270833367473017, 1.181850606188764807 ) ) ;
#102518 = CARTESIAN_POINT ( 'NONE',  ( 1.622331739061450007, -1.257988004683800787, -1.880359251820800104 ) ) ;
#102520 = CARTESIAN_POINT ( 'NONE',  ( -8.995998617867369873, 10.45408546138876993, 1.199719254218462483 ) ) ;
#102521 = EDGE_CURVE ( 'NONE', #158436, #167173, #83973, .T. ) ;
#102522 = CARTESIAN_POINT ( 'NONE',  ( -3.904385050611244079, 7.498940292447679568, 1.040834085586084257E-14 ) ) ;
#102523 = CARTESIAN_POINT ( 'NONE',  ( 1.364683531249988535, 1.926041667008086211, 0.7879004041258500513 ) ) ;
#102524 = CARTESIAN_POINT ( 'NONE',  ( 4.611577566919329740, 8.352668595566711929, -0.2595669225248058432 ) ) ;
#102525 = CARTESIAN_POINT ( 'NONE',  ( -1.500000000000008216, 9.500000000000001776, 3.469446951953614189E-15 ) ) ;
#102526 = CARTESIAN_POINT ( 'NONE',  ( 4.248488654339817927, 0.4632642123635377640, 1.661427155677893674 ) ) ;
#102527 = CARTESIAN_POINT ( 'NONE',  ( 3.366167277942881064, 7.149221934233827014, -0.7998128361456362523 ) ) ;
#102528 = CARTESIAN_POINT ( 'NONE',  ( 1.862210123611393708, -1.255811410660602867, 1.247235970127296811 ) ) ;
#102529 = CARTESIAN_POINT ( 'NONE',  ( 2.772137614628172653, 2.003179168937582855, -0.1996775111661793500 ) ) ;
#102530 = CARTESIAN_POINT ( 'NONE',  ( 8.563946585326370098, 13.14302144952281814, 0.7998128361456462443 ) ) ;
#102531 = CARTESIAN_POINT ( 'NONE',  ( 5.245248717291847385, -1.895131572898335115, 1.130396782059706950 ) ) ;
#102532 = ORIENTED_EDGE ( 'NONE', *, *, #65647, .F. ) ;
#102533 = CARTESIAN_POINT ( 'NONE',  ( 4.008073073761713623, -0.7691326184188684856, 1.867817587601346307 ) ) ;
#102534 = CARTESIAN_POINT ( 'NONE',  ( -7.598418745816086783, 7.829519723065708092, 0.000000000000000000 ) ) ;
#102535 = CARTESIAN_POINT ( 'NONE',  ( 4.077750037130567939, -0.7691059624741981571, 1.864175985064358665 ) ) ;
#102536 = EDGE_LOOP ( 'NONE', ( #75147, #111577, #146975, #81358 ) ) ;
#102537 = VERTEX_POINT ( 'NONE', #205795 ) ;
#102538 = CARTESIAN_POINT ( 'NONE',  ( 2.518242125168220102, 1.223528130051700025, -1.415109699333151561 ) ) ;
#102539 = CARTESIAN_POINT ( 'NONE',  ( 3.147653791585717453, 8.920000000000001705, -2.420000000000002149 ) ) ;
#102540 = CARTESIAN_POINT ( 'NONE',  ( 2.425908952446104827, -1.891012092455180760, 0.2844710172774585488 ) ) ;
#102541 = CARTESIAN_POINT ( 'NONE',  ( 1.506454395378251805E-16, 4.500000000000003553, 2.250000000000006661 ) ) ;
#102542 = CARTESIAN_POINT ( 'NONE',  ( -10.14891672641957499, 5.000029895416906456, -7.601366607803407227 ) ) ;
#102543 = CARTESIAN_POINT ( 'NONE',  ( -1.364683531250012516, 2.551041667008089320, -0.7879004041258289570 ) ) ;
#102544 = CARTESIAN_POINT ( 'NONE',  ( 0.4922593472763935329, -1.060406550076501642, 1.591262010887870115 ) ) ;
#102545 = CARTESIAN_POINT ( 'NONE',  ( 5.234856708652222856, 8.161064355852680308, 1.082531754730549078 ) ) ;
#102546 = CARTESIAN_POINT ( 'NONE',  ( 1.574581288703358339, 1.320057194528483135, -1.451483715152704246 ) ) ;
#102547 = EDGE_CURVE ( 'NONE', #141689, #105686, #33813, .T. ) ;
#102548 = DIRECTION ( 'NONE',  ( -1.000000000000000000, 1.014813233446432150E-15, 1.972152263052529514E-31 ) ) ;
#102549 = CARTESIAN_POINT ( 'NONE',  ( -4.990283058281743678, 7.979691447040783814, -1.199719254218453823 ) ) ;
#102550 = CARTESIAN_POINT ( 'NONE',  ( 3.762070191281779774, 0.7111978290502696254, -1.997938288694045550 ) ) ;
#102552 = LINE ( 'NONE', #21272, #164501 ) ;
#102551 = CARTESIAN_POINT ( 'NONE',  ( 9.097684769969825780, 10.57271930550834860, -1.199719254218446718 ) ) ;
#102553 = B_SPLINE_CURVE_WITH_KNOTS ( 'NONE', 1,
 ( #189623, #188556 ),
 .UNSPECIFIED., .F., .F.,
 ( 2, 2 ),
 ( 0.000000000000000000, 0.5165575204427501621 ),
 .UNSPECIFIED. ) ;
#102554 =( BOUNDED_SURFACE ( )  B_SPLINE_SURFACE ( 3, 2, ( 
 ( #30685, #100985, #149759 ),
 ( #181179, #260, #66330 ),
 ( #198478, #50123, #67397 ),
 ( #133538, #199545, #14396 ),
 ( #51187, #117310, #96768 ),
 ( #211534, #63169, #129335 ) ),
 .UNSPECIFIED., .F., .F., .T. ) 
 B_SPLINE_SURFACE_WITH_KNOTS ( ( 4, 2, 4 ),
 ( 3, 3 ),
 ( 6.938893903907228378E-18, 0.002403677751102689057, 0.004807355502205371174 ),
 ( 0.000000000000000000, 1.000000000000000000 ),
 .UNSPECIFIED. ) 
 GEOMETRIC_REPRESENTATION_ITEM ( )  RATIONAL_B_SPLINE_SURFACE ( (
 ( 1.000000000000000000, 0.7789607113619948509, 1.000000000000000000),
 ( 1.000000000000000000, 0.7844575505954939354, 1.000000000000000000),
 ( 1.000000000000000000, 0.7910273759756237810, 1.000000000000000000),
 ( 1.000000000000000000, 0.8087931444444614870, 1.000000000000000000),
 ( 1.000000000000000000, 0.8199986536752678079, 1.000000000000000000),
 ( 1.000000000000000000, 0.8356624583022104202, 1.000000000000000000) ) ) 
 REPRESENTATION_ITEM ( '' )  SURFACE ( )  );
#102555 = CARTESIAN_POINT ( 'NONE',  ( 5.343030940550726804, -1.692140053440434277, 1.011138898101251016 ) ) ;
#102556 = CARTESIAN_POINT ( 'NONE',  ( -1.364683531250000748, 1.009375000341421247, 0.000000000000000000 ) ) ;
#102557 = CARTESIAN_POINT ( 'NONE',  ( 1.283448800676566970, 0.1440664973490720091, -2.008080635846798856 ) ) ;
#102558 = EDGE_LOOP ( 'NONE', ( #180161, #173900, #161311, #89807, #199007, #20825, #98871, #140040, #176590 ) ) ;
#102559 = CIRCLE ( 'NONE', #40435, 0.08000000000000020983 ) ;
#102560 = CARTESIAN_POINT ( 'NONE',  ( 1.441172756004579947, -1.817888344413360668, -1.085095524780084864 ) ) ;
#102561 = CARTESIAN_POINT ( 'NONE',  ( 11.76011352416511535, 6.974713285862789824, 2.433019384783116745 ) ) ;
#102562 = CARTESIAN_POINT ( 'NONE',  ( 2.541538742049511246, 1.893869637037654208, -0.8368498079355383146 ) ) ;
#102563 = CARTESIAN_POINT ( 'NONE',  ( 3.366167277942881064, 7.149221934233827014, -0.7998128361456362523 ) ) ;
#102564 = CARTESIAN_POINT ( 'NONE',  ( 5.254667053748194760, 8.288139441751686931, 1.199719254218452047 ) ) ;
#102565 = ORIENTED_EDGE ( 'NONE', *, *, #179202, .F. ) ;
#102567 = CARTESIAN_POINT ( 'NONE',  ( 5.352771719296971042, 5.139321848801576387, 0.7998128361456341429 ) ) ;
#102566 = CARTESIAN_POINT ( 'NONE',  ( 4.242189115703227209, 0.5575990197337198362, 2.014825664747122769 ) ) ;
#102570 = ORIENTED_EDGE ( 'NONE', *, *, #189072, .F. ) ;
#102569 = CARTESIAN_POINT ( 'NONE',  ( 1.101899038012419174, -0.8149344392366760781, 1.617857622727811862 ) ) ;
#102568 = CARTESIAN_POINT ( 'NONE',  ( 3.223480179809079971, -1.759765543241718966, 0.4855387900214308550 ) ) ;
#102571 = CARTESIAN_POINT ( 'NONE',  ( 6.709632191794143274, -0.4886956906769434061, 2.160084693451309601 ) ) ;
#102572 = CARTESIAN_POINT ( 'NONE',  ( -8.044078759455166150, -6.893137084989842123, 7.385065802799744894 ) ) ;
#102573 = CARTESIAN_POINT ( 'NONE',  ( 10.16132735305258628, 13.50054059766859993, 7.251518808614104472 ) ) ;
#102574 = CARTESIAN_POINT ( 'NONE',  ( 5.174942826180319422, -2.076333920960464763, -0.7478091396579674699 ) ) ;
#102575 = CARTESIAN_POINT ( 'NONE',  ( -8.012344526598182026E-15, 9.609375000341398021, -1.575800808251669460 ) ) ;
#102576 = VERTEX_POINT ( 'NONE', #140848 ) ;
#102577 = CARTESIAN_POINT ( 'NONE',  ( 3.844317892072905973, 1.020479721125296280, -1.617037373464407457 ) ) ;
#102578 = CARTESIAN_POINT ( 'NONE',  ( -3.460355519985875983, 5.060167411448709629, 1.599625672291267398 ) ) ;
#102579 = CARTESIAN_POINT ( 'NONE',  ( 6.584456157731144899, 10.83361595066169514, -0.7998128361456291469 ) ) ;
#102581 = CARTESIAN_POINT ( 'NONE',  ( -5.181758602633715682, 4.945385036406048762, 2.499999999999998668 ) ) ;
#102580 = B_SPLINE_CURVE_WITH_KNOTS ( 'NONE', 3,
 ( #203579, #9666, #173265, #157012, #73603, #189490 ),
 .UNSPECIFIED., .F., .F.,
 ( 4, 2, 4 ),
 ( 0.000000000000000000, 0.0003129201390360506364, 0.0006258402780721015980 ),
 .UNSPECIFIED. ) ;
#102582 = CARTESIAN_POINT ( 'NONE',  ( -2.353626204688216217E-14, 0.1093750003414345612, -1.570758158831782048 ) ) ;
#102583 = CARTESIAN_POINT ( 'NONE',  ( 5.056828107772846082, 6.922718763866881453, -1.443375672974051449 ) ) ;
#102584 = EDGE_CURVE ( 'NONE', #120769, #187511, #9731, .T. ) ;
#102585 = CARTESIAN_POINT ( 'NONE',  ( 6.585463931165095985, -0.9389328202267492873, 1.978239266594773671 ) ) ;
#102586 = CARTESIAN_POINT ( 'NONE',  ( 6.127784903196001665, 7.091900248975262500, -1.102264294108054266 ) ) ;
#102587 = CARTESIAN_POINT ( 'NONE',  ( -4.379492900960898716, 15.46945218216220219, -11.18131077117918792 ) ) ;
#102588 = ORIENTED_EDGE ( 'NONE', *, *, #121327, .F. ) ;
#102589 = ORIENTED_EDGE ( 'NONE', *, *, #59134, .F. ) ;
#102590 = CARTESIAN_POINT ( 'NONE',  ( 1.499999999999821032, 7.360305807095781638, -4.205660139708353285 ) ) ;
#102591 = EDGE_CURVE ( 'NONE', #198330, #702, #209495, .T. ) ;
#102592 = CARTESIAN_POINT ( 'NONE',  ( 4.077312411328878561, 1.762187477035919603, -0.6278270876356045749 ) ) ;
#102593 = CARTESIAN_POINT ( 'NONE',  ( -3.285556943750000514, -1.626041666188708046, -1.896917185911906722 ) ) ;
#102594 = CIRCLE ( 'NONE', #99200, 4.022469383779238683 ) ;
#102595 = CARTESIAN_POINT ( 'NONE',  ( 7.334597915313080918, 9.580116872663850813, 1.040834085586084257E-14 ) ) ;
#102596 = CARTESIAN_POINT ( 'NONE',  ( -5.883875478650828050, 9.808345791827219884, 0.7216878364870458196 ) ) ;
#102598 = CARTESIAN_POINT ( 'NONE',  ( 3.953084306836263995, 6.769626237021087789, 1.199719254218452047 ) ) ;
#102597 = AXIS2_PLACEMENT_3D ( 'NONE', #163962, #129406, #145613 ) ;
#102599 = CARTESIAN_POINT ( 'NONE',  ( 6.484877546038077867, 6.460111979999551224, 1.040834085586084257E-14 ) ) ;
#102600 = CARTESIAN_POINT ( 'NONE',  ( 6.578973861349465935, 1.929489650308688464, 0.7507879531711419974 ) ) ;
#102602 = CARTESIAN_POINT ( 'NONE',  ( 1.089470510105726708, -0.4871801946146369078, 1.956568126268923846 ) ) ;
#102601 = B_SPLINE_CURVE_WITH_KNOTS ( 'NONE', 3,
 ( #43813, #41679, #140252, #109926, #110987, #112064 ),
 .UNSPECIFIED., .F., .F.,
 ( 4, 2, 4 ),
 ( 1.978668964786020170E-18, 0.0002104102383275119543, 0.0004208204766550219028 ),
 .UNSPECIFIED. ) ;
#102603 = CARTESIAN_POINT ( 'NONE',  ( -8.134002093194872884, 11.57708731111429401, 1.199719254218453823 ) ) ;
#102604 = CARTESIAN_POINT ( 'NONE',  ( 6.964048179274811012, 8.153752959689313684, 1.199719254218452047 ) ) ;
#102605 = DIRECTION ( 'NONE',  ( 0.000000000000000000, 0.000000000000000000, -1.000000000000000000 ) ) ;
#102606 = CARTESIAN_POINT ( 'NONE',  ( 1.957222284144799929, 0.3726435881295561692, -2.159377063894574622 ) ) ;
#102607 = CARTESIAN_POINT ( 'NONE',  ( 5.918537399722813674, 1.222626809077583587, -1.356019982345892050 ) ) ;
#102608 = CARTESIAN_POINT ( 'NONE',  ( -4.485049888022365927, 4.126979712314507331, 0.7998128361456341429 ) ) ;
#102609 = CARTESIAN_POINT ( 'NONE',  ( 4.746763178560254204, 6.631252689777363152, 1.443375672974065660 ) ) ;
#102610 = CARTESIAN_POINT ( 'NONE',  ( 10.42352117080803708, 11.05519620889787724, -0.7998128361456281477 ) ) ;
#102611 = CARTESIAN_POINT ( 'NONE',  ( 2.679707916995359263, 6.278076336469897711, -0.7998128361456291469 ) ) ;
#102612 = CARTESIAN_POINT ( 'NONE',  ( 4.523580528814945545, 5.306540700819438960, 1.199719254218452047 ) ) ;
#102613 = ORIENTED_EDGE ( 'NONE', *, *, #120570, .F. ) ;
#102615 = CARTESIAN_POINT ( 'NONE',  ( 1.067042177248921364, -1.585704042599777264, 1.240073755948613243 ) ) ;
#102614 = CARTESIAN_POINT ( 'NONE',  ( 3.421284184235491743, -1.099380227797893905, -1.476844927387373163 ) ) ;
#102616 = CARTESIAN_POINT ( 'NONE',  ( 2.126706441246130286, 0.3935840842550219487, -2.264316624754546314 ) ) ;
#102618 = CARTESIAN_POINT ( 'NONE',  ( 1.129495572712395646, 1.795378659943444033, -0.4894723102292392047 ) ) ;
#102617 = CARTESIAN_POINT ( 'NONE',  ( 3.212919216758630014, 6.692230152952963529, 0.000000000000000000 ) ) ;
#102619 = CARTESIAN_POINT ( 'NONE',  ( -3.475000000000000533, -0.7291666666666675178, -2.006292185433948827 ) ) ;
#102620 = CARTESIAN_POINT ( 'NONE',  ( -3.391510981712833939, 7.108513245306943062, 0.7998128361456341429 ) ) ;
#102621 = CARTESIAN_POINT ( 'NONE',  ( -9.367496997901325173, 14.48154074412966175, -7.499999999620646562 ) ) ;
#102622 = CARTESIAN_POINT ( 'NONE',  ( 4.939673314881130040, -1.814047719456039154, 0.6055163330952323397 ) ) ;
#102623 = CARTESIAN_POINT ( 'NONE',  ( -10.08065090696061716, 11.71951313199760136, -1.199719254218441611 ) ) ;
#102624 = CARTESIAN_POINT ( 'NONE',  ( 6.486339200172205999, 6.751434215916642501, 0.1376000389162572446 ) ) ;
#102625 = CARTESIAN_POINT ( 'NONE',  ( -7.024532985656169792, 9.288650798055913427, 1.443375672974064550 ) ) ;
#102627 = CARTESIAN_POINT ( 'NONE',  ( 1.744777856283234785, -1.581906188472384400, 0.9981555316627908070 ) ) ;
#102626 = CARTESIAN_POINT ( 'NONE',  ( 3.403930425450612418, -0.8493818440679711257, -1.910634358282743417 ) ) ;
#102628 = CARTESIAN_POINT ( 'NONE',  ( 8.622622508611357262, 9.162073802909148412, -0.7216878364870197293 ) ) ;
#102629 = CARTESIAN_POINT ( 'NONE',  ( -0.6823417656250212460, 5.363541667008087543, 1.181850606188767472 ) ) ;
#102630 = CARTESIAN_POINT ( 'NONE',  ( 2.981702274927648944, -1.715113757222336721, -0.2947475401101228853 ) ) ;
#102631 = CARTESIAN_POINT ( 'NONE',  ( 5.834086172582112262, 5.700855377634248100, 1.040834085586084257E-14 ) ) ;
#102632 = CARTESIAN_POINT ( 'NONE',  ( 11.86687934130374522, 13.60951949616558565, -1.056332641424308827 ) ) ;
#102633 = CARTESIAN_POINT ( 'NONE',  ( 4.248488654339817927, 0.4632642123635377640, 1.661427155677893674 ) ) ;
#102634 = CARTESIAN_POINT ( 'NONE',  ( 3.579775959861815515, -1.078688530630707243, 1.907616655872627964 ) ) ;
#102635 = CARTESIAN_POINT ( 'NONE',  ( 5.971336403843030105, 0.1662174427981797931, -2.200672837095698497 ) ) ;
#102636 = CARTESIAN_POINT ( 'NONE',  ( 0.7500000000000006661, 8.583333333333332149, 1.299038105676657340 ) ) ;
#102637 = TOROIDAL_SURFACE ( 'NONE', #61200, 9.580000000000001847, 0.08000000000000000167 ) ;
#102638 = CARTESIAN_POINT ( 'NONE',  ( 3.713894982949633050, 0.5324762967815239723, -2.104625409411722270 ) ) ;
#102639 = CARTESIAN_POINT ( 'NONE',  ( 1.840199252755945425, 1.805614550920462635, 0.2691313018618191055 ) ) ;
#102640 = CARTESIAN_POINT ( 'NONE',  ( 0.2507196182260813533, -0.4238382354822354259, -1.922440920834954436 ) ) ;
#102641 = CARTESIAN_POINT ( 'NONE',  ( 4.716069161646245789, 1.085680477651463915, -1.817652797078447735 ) ) ;
#102642 = EDGE_CURVE ( 'NONE', #94956, #135209, #145114, .T. ) ;
#102643 = ORIENTED_EDGE ( 'NONE', *, *, #129790, .T. ) ;
#102645 = CARTESIAN_POINT ( 'NONE',  ( 1.364683531249988535, 3.176041667008084435, 0.7879004041258500513 ) ) ;
#102644 = CARTESIAN_POINT ( 'NONE',  ( 4.406014021519581547, -0.9797006336973247409, -2.072624738501188446 ) ) ;
#102646 = CARTESIAN_POINT ( 'NONE',  ( 6.720655732516681802, 2.481091636469245021, 2.111593894264688132 ) ) ;
#102647 = CARTESIAN_POINT ( 'NONE',  ( 9.622536337397022521, 12.24937836509514710, 1.599625672291281386 ) ) ;
#102648 = CARTESIAN_POINT ( 'NONE',  ( 0.8914570141239013257, -0.05588796005432519753, -2.119924415460701983 ) ) ;
#102649 = CARTESIAN_POINT ( 'NONE',  ( -5.151735183512911043, 6.073074471262228435, 1.082531754730548412 ) ) ;
#102650 = CARTESIAN_POINT ( 'NONE',  ( 0.000000000000000000, 0.000000000000000000, 0.000000000000000000 ) ) ;
#102651 = CARTESIAN_POINT ( 'NONE',  ( -5.924549939047510705, 6.974691686052601369, 1.082531754730549967 ) ) ;
#102653 = CARTESIAN_POINT ( 'NONE',  ( -0.7500000000000006661, 12.48958333401613352, -1.299038105676657340 ) ) ;
#102652 = CARTESIAN_POINT ( 'NONE',  ( 6.883263157960367806, 2.959656548886806071, 2.506466465954690914 ) ) ;
#102654 = ORIENTED_EDGE ( 'NONE', *, *, #207872, .T. ) ;
#102655 = CARTESIAN_POINT ( 'NONE',  ( 5.238907797441370029, 2.013986022392059816, -0.1017483359899013229 ) ) ;
#102657 = CARTESIAN_POINT ( 'NONE',  ( 4.610253265130005218, 2.062215687086375038, -0.04552280787792003375 ) ) ;
#102656 = CARTESIAN_POINT ( 'NONE',  ( 6.173040012923759257, 6.096301524699504704, -0.7998128361456281477 ) ) ;
#102659 = CARTESIAN_POINT ( 'NONE',  ( -0.2409995289980245703, 0.2355275985303668385, -2.034371242098035548 ) ) ;
#102658 = CARTESIAN_POINT ( 'NONE',  ( 7.530627977747744062, 7.750430493652658015, -0.7998128361456341429 ) ) ;
#102660 = CARTESIAN_POINT ( 'NONE',  ( 5.851225812749518695, 8.984124660586543243, -1.199719254218452047 ) ) ;
#102661 = CARTESIAN_POINT ( 'NONE',  ( 3.285556943750000514, -0.6635416661887083567, 1.896917185911906500 ) ) ;
#102662 = CARTESIAN_POINT ( 'NONE',  ( -1.500000000000008216, 12.74999999999999822, 3.469446951953614189E-15 ) ) ;
#102663 = CARTESIAN_POINT ( 'NONE',  ( 0.2696249905001372182, 1.205521239366886821, 1.707859383111657747 ) ) ;
#102664 = CARTESIAN_POINT ( 'NONE',  ( 4.272111401563948085, 1.799923229630392640, -0.9091438646662284295 ) ) ;
#102665 = CARTESIAN_POINT ( 'NONE',  ( 4.388128076750056117, -0.4078595375654435751, -1.795341762384855544 ) ) ;
#102666 = COLOUR_RGB ( '', 0.09019608, 0.27058824, 0.51372549) ;
#102667 = EDGE_CURVE ( 'NONE', #18903, #129023, #172061, .T. ) ;
#102668 = CARTESIAN_POINT ( 'NONE',  ( 4.645640190976921602, 8.571663989448405019, 1.040834085586084257E-14 ) ) ;
#102669 = CARTESIAN_POINT ( 'NONE',  ( 0.8324923845523107824, 0.1201152365052655241, 1.720655618271366150 ) ) ;
#102670 = CARTESIAN_POINT ( 'NONE',  ( 3.176185322659801230E-15, -5.758458176070770485, 10.93186801223271587 ) ) ;
#102671 = CARTESIAN_POINT ( 'NONE',  ( -7.088215381846223906, 7.164006121775713609, 0.7998128361456341429 ) ) ;
#102672 = CARTESIAN_POINT ( 'NONE',  ( 0.7907308791721240349, -2.245476950237018432, -0.2759641350603259657 ) ) ;
#102673 = CARTESIAN_POINT ( 'NONE',  ( 2.860102072500060544, 2.095886770163409185, -0.2068341903323153708 ) ) ;
#102674 = CARTESIAN_POINT ( 'NONE',  ( -4.878955176071358757, 6.785476686873604280, -1.599625672291271394 ) ) ;
#102675 = CARTESIAN_POINT ( 'NONE',  ( 6.642605195691581699, 9.837124264027149678, 1.199719254218462483 ) ) ;
#102676 = CARTESIAN_POINT ( 'NONE',  ( 6.834718834620487016, 7.146462526578263308, 0.000000000000000000 ) ) ;
#102677 = CARTESIAN_POINT ( 'NONE',  ( 6.468749999177490828, 0.7852924545920478838, -1.895863743164218018 ) ) ;
#102678 = CARTESIAN_POINT ( 'NONE',  ( -6.196239896645333367, 7.187700286629718605, -1.199719254218446718 ) ) ;
#102679 = CARTESIAN_POINT ( 'NONE',  ( 7.253248993186735660, 7.564471368247083660, 0.7216878364870317197 ) ) ;
#102680 = CARTESIAN_POINT ( 'NONE',  ( 4.149381719138396818, 7.633502232665817289, 0.8094099469760536181 ) ) ;
#102681 = CARTESIAN_POINT ( 'NONE',  ( -2.923754682041362241, 6.562797562356882608, 0.7998128361456341429 ) ) ;
#102682 = CARTESIAN_POINT ( 'NONE',  ( 4.658541260611516854, 2.215511418189203496, 0.1622135575486300108 ) ) ;
#102683 = CARTESIAN_POINT ( 'NONE',  ( 2.027518650255655253, -1.432890729411402830, -1.658174735819064827 ) ) ;
#102684 = CARTESIAN_POINT ( 'NONE',  ( -4.550733115681270036, 8.460939068270139529, 0.7998128361456481317 ) ) ;
#102685 = CARTESIAN_POINT ( 'NONE',  ( -4.228163802615396705, 6.026220084508304708, -1.599625672291271394 ) ) ;
#102686 = CARTESIAN_POINT ( 'NONE',  ( 5.863715402168388380, -0.4781514528688200483, 1.902565108626976809 ) ) ;
#102687 = B_SPLINE_CURVE_WITH_KNOTS ( 'NONE', 3,
 ( #42672, #55685, #204036, #23163, #39438, #105532, #206195, #10130, #171566, #57823, #72988, #41602, #157479, #89279, #104452, #22082 ),
 .UNSPECIFIED., .F., .F.,
 ( 4, 2, 2, 2, 2, 2, 2, 4 ),
 ( 8.673617379884027768E-19, 0.001349084649940009107, 0.002698169299880017347, 0.004047253949820025370, 0.005396338599760033827, 0.006745423249700042284, 0.008094507899640049006, 0.01079267719952006592 ),
 .UNSPECIFIED. ) ;
#102688 = CARTESIAN_POINT ( 'NONE',  ( 0.6823417656249899377, 1.342708333674752508, 1.181850606188755259 ) ) ;
#102690 = ORIENTED_EDGE ( 'NONE', *, *, #187111, .T. ) ;
#102689 = CARTESIAN_POINT ( 'NONE',  ( -3.945059511896602089, 7.546393830613923548, 1.040834085586084257E-14 ) ) ;
#102691 = CARTESIAN_POINT ( 'NONE',  ( 4.113620189327307664, 1.705085180707970771, 1.260635662952174663 ) ) ;
#102692 = CARTESIAN_POINT ( 'NONE',  ( -6.780486220610184134, 9.003929572168926754, -1.443375672974066548 ) ) ;
#102693 = ORIENTED_EDGE ( 'NONE', *, *, #139910, .F. ) ;
#102695 = CARTESIAN_POINT ( 'NONE',  ( -1.445103857048105844, 8.688264192037886247, -2.625611233228243968 ) ) ;
#102694 = CARTESIAN_POINT ( 'NONE',  ( -5.478903473698247595, 8.445785581739666981, -1.082531754730549967 ) ) ;
#102696 = CARTESIAN_POINT ( 'NONE',  ( 5.524057522564145728, 8.532151978711786100, 1.199719254218462483 ) ) ;
#102697 = CARTESIAN_POINT ( 'NONE',  ( 5.372543328820884589, -0.05112055865702340440, -1.840719716649619198 ) ) ;
#102698 = UNCERTAINTY_MEASURE_WITH_UNIT (LENGTH_MEASURE( 1.000000000000000082E-05 ), #111481, 'distance_accuracy_value', 'NONE');
#102699 = CARTESIAN_POINT ( 'NONE',  ( 0.6124999999999828360, 0.9791666673494778816, -1.060881119635955327 ) ) ;
#102700 = CARTESIAN_POINT ( 'NONE',  ( -0.6823417656250003738, 3.030208333674754062, -1.181850606188749264 ) ) ;
#102701 = CARTESIAN_POINT ( 'NONE',  ( 0.5732861554464663278, -0.9687841611035786782, 1.445654263422226027 ) ) ;
#102702 = CARTESIAN_POINT ( 'NONE',  ( -1.364683531250014514, -1.157291666325248158, 0.7879004041258379498 ) ) ;
#102703 = CARTESIAN_POINT ( 'NONE',  ( -0.1604749557937330817, 7.629137130509052511, -2.703579865625728385 ) ) ;
#102704 = CARTESIAN_POINT ( 'NONE',  ( 5.190363053866647647, -2.144918610114197488, -0.2683968819863768451 ) ) ;
#102705 = CARTESIAN_POINT ( 'NONE',  ( -4.322352044658376968, 3.937165561723182883, 0.7998128361456341429 ) ) ;
#102706 = CARTESIAN_POINT ( 'NONE',  ( -7.497295758232731089, 8.809561808435409702, -1.082531754730543083 ) ) ;
#102707 = CARTESIAN_POINT ( 'NONE',  ( 4.364260218091946975, 1.016419123106377276, 1.907829002176253175 ) ) ;
#102708 = CARTESIAN_POINT ( 'NONE',  ( 0.6823417656249917140, 3.342708333674754506, 1.181850606188765695 ) ) ;
#102709 = CARTESIAN_POINT ( 'NONE',  ( 5.149669460738499183, 0.6209446730581876794, -1.871051946789156650 ) ) ;
#102710 = CARTESIAN_POINT ( 'NONE',  ( 4.446485213073447795, 1.132808404574834782, 1.312715084458302872 ) ) ;
#102711 = EDGE_CURVE ( 'NONE', #96984, #73222, #92465, .T. ) ;
#102712 = CARTESIAN_POINT ( 'NONE',  ( 0.6443834720083198020, 0.6415979653194536780, 2.095529601600601755 ) ) ;
#102713 = CARTESIAN_POINT ( 'NONE',  ( 2.204549329899041510, -2.307029201398633322, 0.05716382847485364238 ) ) ;
#102714 = CARTESIAN_POINT ( 'NONE',  ( 4.464173201700037730, 0.9678196394932538915, 1.819351253882226516 ) ) ;
#102715 = CARTESIAN_POINT ( 'NONE',  ( -0.02357939311542662716, -0.1349932991356362910, -1.911059701570053226 ) ) ;
#102716 = CARTESIAN_POINT ( 'NONE',  ( -7.524412065460066579, 7.880828285899290186, 0.7216878364870317197 ) ) ;
#102718 = EDGE_CURVE ( 'NONE', #187973, #104308, #85609, .T. ) ;
#102717 = CARTESIAN_POINT ( 'NONE',  ( -4.308458954092677651, 8.248562223075252220, -0.7998128361456362523 ) ) ;
#102719 = CARTESIAN_POINT ( 'NONE',  ( 1.084637062511528693, 3.023878807974804683, 1.105835307554807301 ) ) ;
#102720 = SURFACE_SIDE_STYLE ('',( #132058 ) ) ;
#102721 = CARTESIAN_POINT ( 'NONE',  ( -6.358410854684789726, 8.441231968597481483, -1.443375672974058777 ) ) ;
#102722 = CARTESIAN_POINT ( 'NONE',  ( 3.048105859194950362, 0.7956334958073747465, -2.058523145315640956 ) ) ;
#102723 = CARTESIAN_POINT ( 'NONE',  ( 3.285556943750000514, -2.151041666188709733, 1.896917185911906500 ) ) ;
#102724 = CARTESIAN_POINT ( 'NONE',  ( 1.217372920688150506, 0.3700031967454868176, -1.823611282344459239 ) ) ;
#102725 = CARTESIAN_POINT ( 'NONE',  ( 1.499912825862921295, 3.250189846351735135, 0.08469158891783865051 ) ) ;
#102726 = SURFACE_SIDE_STYLE ('',( #72333 ) ) ;
#102727 = CARTESIAN_POINT ( 'NONE',  ( 1.793740946118090429, 2.512284051036407728, -2.500000000000000444 ) ) ;
#102730 = AXIS2_PLACEMENT_3D ( 'NONE', #119251, #36858, #102942 ) ;
#102729 = CARTESIAN_POINT ( 'NONE',  ( 6.825078400183588023, 2.959908325773926041, 2.496992193004472504 ) ) ;
#102728 = CARTESIAN_POINT ( 'NONE',  ( -5.018240346111991990, 8.014652766117364990, -1.155606277404798821 ) ) ;
#102731 = CARTESIAN_POINT ( 'NONE',  ( 5.999929499617846496, -0.6670042279848520383, -1.716255146773135287 ) ) ;
#102732 = ORIENTED_EDGE ( 'NONE', *, *, #38945, .T. ) ;
#102733 = CARTESIAN_POINT ( 'NONE',  ( 3.625900526125751089, -1.226333045360414653, -1.656161981788171200 ) ) ;
#102734 = CARTESIAN_POINT ( 'NONE',  ( 1.360316468749943608, 1.494791667008105174, 0.7853790794158439503 ) ) ;
#102735 = UNCERTAINTY_MEASURE_WITH_UNIT (LENGTH_MEASURE( 1.000000000000000082E-05 ), #68448, 'distance_accuracy_value', 'NONE');
#102736 = CARTESIAN_POINT ( 'NONE',  ( -6.205881626753225966, 8.263281202677319470, 1.599625672291283607 ) ) ;
#102737 = CARTESIAN_POINT ( 'NONE',  ( 2.789718171214683462, 1.917044005781431748, -0.6357942740662542169 ) ) ;
#102738 = CARTESIAN_POINT ( 'NONE',  ( -1.500000000000015099, -0.1208333333333093396, -0.8660254037844383745 ) ) ;
#102739 = CARTESIAN_POINT ( 'NONE',  ( 4.684505768721569652, 5.424010470718658716, -1.199719254218452047 ) ) ;
#102740 = CARTESIAN_POINT ( 'NONE',  ( 2.448182087220668102, 2.060414928722671402, 0.05179878229087316738 ) ) ;
#102742 = CARTESIAN_POINT ( 'NONE',  ( 1.364683531250000303, 13.75520833367473195, -0.7879004041258355073 ) ) ;
#102741 = CARTESIAN_POINT ( 'NONE',  ( -1.500000000000055511, 7.268077025657054158, -4.207854987878878461 ) ) ;
#102743 = CARTESIAN_POINT ( 'NONE',  ( 6.602984505055297326, 7.662235663108029726, 1.199719254218462483 ) ) ;
#102744 = CARTESIAN_POINT ( 'NONE',  ( 3.614985261928882032, 3.508924507032078477, 2.500000000000000444 ) ) ;
#102745 = CARTESIAN_POINT ( 'NONE',  ( 5.531908139154323223, -1.397534428995873546, -1.707979418440738195 ) ) ;
#102746 = CARTESIAN_POINT ( 'NONE',  ( 1.282749207608822495, -2.108609127331688260, -0.4749100009155197699 ) ) ;
#102747 = CARTESIAN_POINT ( 'NONE',  ( -4.094199201646926412, 7.720390135322642067, 0.7216878364870317197 ) ) ;
#102748 = B_SPLINE_CURVE_WITH_KNOTS ( 'NONE', 3,
 ( #77585, #110161, #192388, #177231, #92800, #44042, #176173, #30991, #63473, #162053, #62403, #158845, #209700, #28844 ),
 .UNSPECIFIED., .F., .F.,
 ( 4, 2, 2, 2, 2, 2, 4 ),
 ( 0.001872291076886156399, 0.002107054070185122602, 0.002341817063484089023, 0.002811343050082021865, 0.003280869036679954706, 0.003515632029978921561, 0.003750395023277889282 ),
 .UNSPECIFIED. ) ;
#102749 = CARTESIAN_POINT ( 'NONE',  ( 0.3566581422463632189, -1.900417414521380133, -0.6748426577906708745 ) ) ;
#102750 = CARTESIAN_POINT ( 'NONE',  ( 1.986132587416184370, 2.144477605524505393, 0.8272852225373708013 ) ) ;
#102751 = DIRECTION ( 'NONE',  ( -3.706092522800016599E-15, 0.000000000000000000, -1.000000000000000000 ) ) ;
#102752 = CARTESIAN_POINT ( 'NONE',  ( 6.551426578739074635, -1.705833205818767295, 0.8644478841580637285 ) ) ;
#102754 = VERTEX_POINT ( 'NONE', #148288 ) ;
#102753 = CARTESIAN_POINT ( 'NONE',  ( 6.875078400183575411, 7.629137130509070275, 2.455651831298297338 ) ) ;
#102755 = CARTESIAN_POINT ( 'NONE',  ( 2.395189659270926086, 1.444574673180216706, 1.188490415850687265 ) ) ;
#102756 = CIRCLE ( 'NONE', #137399, 0.1000000000000000472 ) ;
#102757 = CARTESIAN_POINT ( 'NONE',  ( 3.854704076794239764, -1.883312302057647880, -0.7212934815618715634 ) ) ;
#102759 = CARTESIAN_POINT ( 'NONE',  ( 11.52888687719611305, 13.79423125104975689, 3.331331986263551315 ) ) ;
#102758 = CARTESIAN_POINT ( 'NONE',  ( -0.6823417656250212460, 1.551041667008083769, 1.181850606188755259 ) ) ;
#102761 = CARTESIAN_POINT ( 'NONE',  ( 5.654936504234950867, -1.661008888676926309, 1.294703585725354156 ) ) ;
#102760 = CARTESIAN_POINT ( 'NONE',  ( -6.679363233026820446, 10.94434087183997129, 0.000000000000000000 ) ) ;
#102762 = CARTESIAN_POINT ( 'NONE',  ( 7.121056995675668411, 9.330985799753529264, -1.599625672291262513 ) ) ;
#102764 = CARTESIAN_POINT ( 'NONE',  ( -7.711890448074853133, 7.891627032375787998, -0.7998128361456291469 ) ) ;
#102763 = CARTESIAN_POINT ( 'NONE',  ( 3.888156192069020634, 7.758209000714329839, 1.040834085586084257E-14 ) ) ;
#102765 = DIRECTION ( 'NONE',  ( 0.000000000000000000, -1.000000000000000000, 0.000000000000000000 ) ) ;
#102766 = CARTESIAN_POINT ( 'NONE',  ( 5.308855472784884455, -0.4948685743355190070, -1.958072916474236314 ) ) ;
#102767 = CARTESIAN_POINT ( 'NONE',  ( -1.364683531250010295, 5.530208333674751842, 0.7879004041258379498 ) ) ;
#102768 = CARTESIAN_POINT ( 'NONE',  ( 0.9013244701963195604, -1.770926582075180944, 1.057100273733258433 ) ) ;
#102769 = CARTESIAN_POINT ( 'NONE',  ( 8.771762198361678031, 9.336070107617867819, 1.040834085586084257E-14 ) ) ;
#102770 = CARTESIAN_POINT ( 'NONE',  ( 5.037736595929563244, 8.035053907629919223, -1.199719254218452047 ) ) ;
#102771 = CARTESIAN_POINT ( 'NONE',  ( -0.6823417656250003738, -0.2197916663252488800, -1.181850606188749264 ) ) ;
#102772 = CARTESIAN_POINT ( 'NONE',  ( 6.201928923608456046, 6.200281597156833691, 0.7998128361456352531 ) ) ;
#102773 = CARTESIAN_POINT ( 'NONE',  ( 8.256552360598020002, 8.734991963560254646, -0.7216878364870267237 ) ) ;
#102775 =( LENGTH_UNIT ( ) NAMED_UNIT ( * ) SI_UNIT ( .MILLI., .METRE. ) );
#102774 = CARTESIAN_POINT ( 'NONE',  ( 3.596278845262687263, 0.9791764565295042466, -1.937929667198809769 ) ) ;
#102777 = CARTESIAN_POINT ( 'NONE',  ( 1.979791773625012352, -1.805961398883266344, -0.3578489297004632808 ) ) ;
#102776 = CARTESIAN_POINT ( 'NONE',  ( -4.772106882330234612, 6.590544000850479200, -1.443375672974053447 ) ) ;
#102778 = CARTESIAN_POINT ( 'NONE',  ( -1.364683531250012516, 3.738541667008087099, -0.7879004041258300672 ) ) ;
#102779 = CARTESIAN_POINT ( 'NONE',  ( 3.966501855323391723, -2.045284974426237579, -0.7877190255709336508 ) ) ;
#102780 = CARTESIAN_POINT ( 'NONE',  ( 4.370663978927085580, 5.060324124126027279, 7.500000000000000000 ) ) ;
#102781 = CARTESIAN_POINT ( 'NONE',  ( 5.208033936170274103, -2.252144374781993363, 0.2163938657309023850 ) ) ;
#102782 = CARTESIAN_POINT ( 'NONE',  ( -6.715366157470410435, 6.729015360003925750, -0.7998128361456291469 ) ) ;
#102783 = CARTESIAN_POINT ( 'NONE',  ( -1.872871967411080307, 3.299999999999962519, 0.3999999999999628852 ) ) ;
#102784 = CARTESIAN_POINT ( 'NONE',  ( 4.913571454530422322, 8.125067815752732514, -1.031885869761673069 ) ) ;
#102785 = CARTESIAN_POINT ( 'NONE',  ( -1.500000000000001110, 13.52083333333332682, 0.8660254037844419273 ) ) ;
#102786 = CARTESIAN_POINT ( 'NONE',  ( -5.926322542504877333, 7.047036066744706950, -1.082531754730549967 ) ) ;
#102787 = CARTESIAN_POINT ( 'NONE',  ( 5.573810548993915148, 5.675402860013913475, 0.000000000000000000 ) ) ;
#102788 = CARTESIAN_POINT ( 'NONE',  ( 5.167173303313960631, 0.1731176489731758861, -1.761265287352784314 ) ) ;
#102789 = CONICAL_SURFACE ( 'NONE', #120175, 10.75000000000000000, 0.5235987755983064762 ) ;
#102790 = CARTESIAN_POINT ( 'NONE',  ( 3.527992865196138972, -1.982922396879973626, 0.3464002264041438073 ) ) ;
#102791 = CARTESIAN_POINT ( 'NONE',  ( 5.798083248138522272, 9.916180889470295412, 0.7998128361456462443 ) ) ;
#102792 = CARTESIAN_POINT ( 'NONE',  ( 1.887856735188620627, 1.451798466554796718, 1.525807353268118227 ) ) ;
#102793 = CARTESIAN_POINT ( 'NONE',  ( -0.6823417656250003738, 11.40104166700806765, 1.181850606188754593 ) ) ;
#102794 = CARTESIAN_POINT ( 'NONE',  ( 2.435944266227826116, 1.209484882827957630, 1.554366883019624668 ) ) ;
#102795 = CARTESIAN_POINT ( 'NONE',  ( 0.2154177506630133854, -1.835460468737951878, 0.3602540799089171131 ) ) ;
#102796 = CARTESIAN_POINT ( 'NONE',  ( 0.1507198084474276056, -0.4258245693303016610, -1.922078969575198526 ) ) ;
#102798 = ORIENTED_EDGE ( 'NONE', *, *, #61052, .F. ) ;
#102797 = CARTESIAN_POINT ( 'NONE',  ( 5.625234629914776185, 1.601787910378251967, 0.8462062870350762767 ) ) ;
#102799 = CARTESIAN_POINT ( 'NONE',  ( 5.992340707560151358, 8.014150130285418783, 1.443375672974062551 ) ) ;
#102800 = AXIS2_PLACEMENT_3D ( 'NONE', #170403, #21991, #201815 ) ;
#102801 = CARTESIAN_POINT ( 'NONE',  ( -1.402160292154681736E-14, 0.009375000341421267647, -1.575800808251665908 ) ) ;
#102802 = CARTESIAN_POINT ( 'NONE',  ( 5.506679003988666388, 1.415762158562785533, -1.222804595763474333 ) ) ;
#102803 = CARTESIAN_POINT ( 'NONE',  ( 4.227444969362701421, 3.826440640544909400, 1.214306433183764966E-14 ) ) ;
#102804 = CARTESIAN_POINT ( 'NONE',  ( 0.000000000000000000, 0.000000000000000000, 0.000000000000000000 ) ) ;
#102805 = CARTESIAN_POINT ( 'NONE',  ( 5.700075226665620498, 0.8442301939139056355, -1.890501578402821847 ) ) ;
#102806 = CARTESIAN_POINT ( 'NONE',  ( -4.597623488365601752, 8.377994813152914944, 0.7216878364870267237 ) ) ;
#102807 =( LENGTH_UNIT ( ) NAMED_UNIT ( * ) SI_UNIT ( .MILLI., .METRE. ) );
#102808 = CARTESIAN_POINT ( 'NONE',  ( -1.201851678989727383E-14, 0.7125000000000225597, 1.732050807568877637 ) ) ;
#102809 = CARTESIAN_POINT ( 'NONE',  ( 7.914208982075123799, 10.25632978388623684, -1.599625672291262513 ) ) ;
#102810 = CARTESIAN_POINT ( 'NONE',  ( -7.479294296233107708, 11.87759377891399204, 0.7998128361456481317 ) ) ;
#102811 = CARTESIAN_POINT ( 'NONE',  ( 5.397027666691686321, 8.454226823519094935, 1.199719254218451159 ) ) ;
#102812 = CARTESIAN_POINT ( 'NONE',  ( -1.364683531250014514, -0.5114583329919092369, -0.7879004041258359514 ) ) ;
#102813 = AXIS2_PLACEMENT_3D ( 'NONE', #25911, #22694, #41133 ) ;
#102814 = CARTESIAN_POINT ( 'NONE',  ( 0.7499999999999902300, 1.233333333333357151, 1.299038105676657340 ) ) ;
#102816 = CARTESIAN_POINT ( 'NONE',  ( 5.931855901178834323, 6.879252291918818152, 1.199719254218462483 ) ) ;
#102815 = CARTESIAN_POINT ( 'NONE',  ( 5.476992472119650124, 1.812042599547862176, 0.7524171098330989516 ) ) ;
#102817 = CARTESIAN_POINT ( 'NONE',  ( 3.462267382487670631, 1.587593928739635896, 1.242537129137813556 ) ) ;
#102818 = CARTESIAN_POINT ( 'NONE',  ( 2.272541799296357468, -0.3318032026102230581, -1.886604652318550901 ) ) ;
#102819 = CARTESIAN_POINT ( 'NONE',  ( -1.772826578343124959, 3.950000000000009059, -0.4500000000000423661 ) ) ;
#102820 = CARTESIAN_POINT ( 'NONE',  ( 0.6795420635867071013, 1.475991390215245058, 1.620154534501851096 ) ) ;
#102821 = CARTESIAN_POINT ( 'NONE',  ( 0.2331713839410939626, 4.091360563681152307, -2.508188233588979799 ) ) ;
#102822 = CARTESIAN_POINT ( 'NONE',  ( 1.862360739135361376, -1.326353699019737098, 1.319252464149045734 ) ) ;
#102823 = CARTESIAN_POINT ( 'NONE',  ( -1.500000000000013101, -0.2979166659838501929, 0.8660254037844403729 ) ) ;
#102824 = CARTESIAN_POINT ( 'NONE',  ( 3.638934968716364793, 1.913053428401530809, 0.6273635501436899409 ) ) ;
#102825 = CARTESIAN_POINT ( 'NONE',  ( -8.830438121202295321, 9.196599317691152464, -0.7998128361456291469 ) ) ;
#102827 = CARTESIAN_POINT ( 'NONE',  ( 4.956716356600668227, -1.994036693836033658, -0.7120731657841266049 ) ) ;
#102826 = CARTESIAN_POINT ( 'NONE',  ( -5.938108093105513241, 6.030140318152288792, 0.7216878364870317197 ) ) ;
#102828 = CARTESIAN_POINT ( 'NONE',  ( -0.5773502691896261751, -2.500000000000002220, -0.9999999999999991118 ) ) ;
#102829 = CARTESIAN_POINT ( 'NONE',  ( 5.564915762860970894, 1.570151797963925455, -1.349580972669261580 ) ) ;
#102831 = CARTESIAN_POINT ( 'NONE',  ( -5.884327782891165093, 6.523468454024004437, -0.8610041489593980302 ) ) ;
#102830 = CARTESIAN_POINT ( 'NONE',  ( 1.628582148955775910, 0.2080868244966528613, 2.080379227509927542 ) ) ;
#102833 = ORIENTED_EDGE ( 'NONE', *, *, #49246, .F. ) ;
#102832 = CARTESIAN_POINT ( 'NONE',  ( 6.282242891264209206, -0.9739734823789309992, 1.543877162560060912 ) ) ;
#102834 = CARTESIAN_POINT ( 'NONE',  ( 8.209625708274705502, 9.536650400197368427, 1.199719254218462483 ) ) ;
#102835 = CARTESIAN_POINT ( 'NONE',  ( -3.456965981804629884, 6.976951378839947537, 1.040834085586084257E-14 ) ) ;
#102836 = CARTESIAN_POINT ( 'NONE',  ( -10.50000000000000000, 12.69999999999999929, -3.600000000000000977 ) ) ;
#102837 = CARTESIAN_POINT ( 'NONE',  ( -10.37901820579008039, 4.889546506944066451, 5.358714317323078014 ) ) ;
#102838 = CARTESIAN_POINT ( 'NONE',  ( 5.626270559546804328, 9.507806719539201978, 0.7216878364870438212 ) ) ;
#102839 = CARTESIAN_POINT ( 'NONE',  ( -1.899436509991863531, 3.291494839451026166, 0.4074537448169551768 ) ) ;
#102841 = CARTESIAN_POINT ( 'NONE',  ( 0.9788403037365877024, -1.637337388150851725, -0.7752084675131820646 ) ) ;
#102840 = CARTESIAN_POINT ( 'NONE',  ( 6.668631453075247073, 8.873432343378178544, -1.599625672291281386 ) ) ;
#102842 = CARTESIAN_POINT ( 'NONE',  ( -6.886651960737580680, 10.12184548991413457, -1.199719254218440723 ) ) ;
#102843 = CARTESIAN_POINT ( 'NONE',  ( 6.003563092752934871, 5.898578451166879510, 0.7998128361456341429 ) ) ;
#102844 = FACE_OUTER_BOUND ( 'NONE', #146129, .T. ) ;
#102845 = CARTESIAN_POINT ( 'NONE',  ( -11.41381676900475917, 11.03041960022397561, 3.704697931490214646 ) ) ;
#102846 = CARTESIAN_POINT ( 'NONE',  ( 4.369805582306193870, 3.992528022312320957, 1.214306433183764966E-14 ) ) ;
#102847 = ORIENTED_EDGE ( 'NONE', *, *, #30754, .F. ) ;
#102848 = EDGE_CURVE ( 'NONE', #150774, #21539, #1089, .T. ) ;
#102849 = ADVANCED_FACE ( 'NONE', ( #12918 ), #111905, .F. ) ;
#102850 = CARTESIAN_POINT ( 'NONE',  ( 6.380482474105581225, -0.5405081658083621399, -1.942537888137134461 ) ) ;
#102851 = CARTESIAN_POINT ( 'NONE',  ( 0.5223349339509277822, -2.109880975928311031, 0.2119513895993754005 ) ) ;
#102852 = CYLINDRICAL_SURFACE ( 'NONE', #174884, 1.224999999999996980 ) ;
#102853 = CARTESIAN_POINT ( 'NONE',  ( 0.1405533004714279166, 6.947787103499396544, -2.874819994463383654 ) ) ;
#102854 = CARTESIAN_POINT ( 'NONE',  ( 1.822139829856954441, 2.508700120398218214, 2.498486944294420642 ) ) ;
#102855 = CARTESIAN_POINT ( 'NONE',  ( -3.619663825168619731, 7.166765529431275539, 1.040834085586084257E-14 ) ) ;
#102856 = CARTESIAN_POINT ( 'NONE',  ( 8.975134502566660899, 10.53370701015836275, -1.082531754730543083 ) ) ;
#102857 = CARTESIAN_POINT ( 'NONE',  ( 3.116014175596728109, 1.960399024780419275, -0.1881816519722582237 ) ) ;
#102858 = CARTESIAN_POINT ( 'NONE',  ( 4.183220377109976518, 1.621195451842275315, 1.198844725951081047 ) ) ;
#102859 = CARTESIAN_POINT ( 'NONE',  ( -5.371001409308059138, 9.417918744168066070, -0.7998128361456231517 ) ) ;
#102860 = CARTESIAN_POINT ( 'NONE',  ( -1.500000000000008216, 10.25000000000000178, 3.469446951953614189E-15 ) ) ;
#102861 = CARTESIAN_POINT ( 'NONE',  ( 4.259861650310483583, 1.032037387010206198, 1.933225914978464299 ) ) ;
#102862 = CARTESIAN_POINT ( 'NONE',  ( -1.420000000000001039, 6.264000000000040203, -2.851999999999994984 ) ) ;
#102863 = CARTESIAN_POINT ( 'NONE',  ( 3.065363963417499615, 0.2843319914107733104, -1.905185398925368423 ) ) ;
#102864 = CARTESIAN_POINT ( 'NONE',  ( -7.182068686937172153, 9.402166106225269715, 1.599625672291283607 ) ) ;
#102865 = CARTESIAN_POINT ( 'NONE',  ( -0.02968770228137587730, 2.889947918782026726, -2.315223470976325526 ) ) ;
#102866 = CARTESIAN_POINT ( 'NONE',  ( 0.1333542156527321720, 1.344858830485482937, -2.298444861300387387 ) ) ;
#102867 = CARTESIAN_POINT ( 'NONE',  ( -0.1460981902779853459, 7.101100029736113761, 2.114500818361210399 ) ) ;
#102868 = ORIENTED_EDGE ( 'NONE', *, *, #87783, .T. ) ;
#102869 = CARTESIAN_POINT ( 'NONE',  ( 4.258669648468281110, 6.061810238003387141, 1.443375672974058777 ) ) ;
#102870 = CARTESIAN_POINT ( 'NONE',  ( 5.348484190341658007, -1.954120660473107396, -0.2448405522006945334 ) ) ;
#102872 = CARTESIAN_POINT ( 'NONE',  ( 4.529943747908701468, -1.973814829549960237, 0.3949202218342766080 ) ) ;
#102871 = CARTESIAN_POINT ( 'NONE',  ( 0.8724827243445825165, -0.04916951280507049493, -1.941606035699546151 ) ) ;
#102873 = CIRCLE ( 'NONE', #43984, 0.07999999999999977962 ) ;
#102874 = CARTESIAN_POINT ( 'NONE',  ( 5.852921341749488526, -1.041456137194999521, 2.048983711149698461 ) ) ;
#102876 = CARTESIAN_POINT ( 'NONE',  ( 4.135495018730405370, 1.753490048523008049, -0.6236645969141580981 ) ) ;
#102875 = CARTESIAN_POINT ( 'NONE',  ( -6.583366107887490770, 9.838288338247510367, 1.199719254218452935 ) ) ;
#102877 = CARTESIAN_POINT ( 'NONE',  ( 6.363572996767764778, 8.517530811019446091, -1.599625672291283607 ) ) ;
#102878 = CARTESIAN_POINT ( 'NONE',  ( -10.99970480893081870, -6.134628647623513231, -0.08058608058607828750 ) ) ;
#102879 = CARTESIAN_POINT ( 'NONE',  ( -15.75000000000000000, 10.89999999999998259, 1.399999999999998579 ) ) ;
#102880 = CARTESIAN_POINT ( 'NONE',  ( -6.235860587281615075, 9.362588887548838557, -1.199719254218440723 ) ) ;
#102881 = CARTESIAN_POINT ( 'NONE',  ( -2.862179826260718762, 6.353310540697199471, 0.000000000000000000 ) ) ;
#102882 = CARTESIAN_POINT ( 'NONE',  ( 0.3631484714031462668, 0.2087870660046411420, -2.181583536649676525 ) ) ;
#102883 = CARTESIAN_POINT ( 'NONE',  ( 4.365362273920230685, 8.036747052974847705, 0.7216878364870298324 ) ) ;
#102884 = ORIENTED_EDGE ( 'NONE', *, *, #100966, .T. ) ;
#102885 = CARTESIAN_POINT ( 'NONE',  ( 10.98598255107576271, -7.721050908199750040, -0.1917610387292519314 ) ) ;
#102886 = CARTESIAN_POINT ( 'NONE',  ( 0.3108172448005979138, 1.586703044182024458, 0.9029097728878652251 ) ) ;
#102887 = CARTESIAN_POINT ( 'NONE',  ( -5.108724954250998707, 4.854600622914589714, -0.7998128361456221525 ) ) ;
#102888 = CARTESIAN_POINT ( 'NONE',  ( 2.373305363469370377, -0.2979590584733567971, -1.708161578628903055 ) ) ;
#102889 = CARTESIAN_POINT ( 'NONE',  ( 6.509000000000039421, 2.968845098214093703, 2.453284407971462411 ) ) ;
#102890 = CARTESIAN_POINT ( 'NONE',  ( -0.6124999999999880540, 0.2916666666666900554, 1.060881119635892933 ) ) ;
#102891 = CARTESIAN_POINT ( 'NONE',  ( 5.830640656690653678, 1.760721658632548037, 0.4824517239352192344 ) ) ;
#102892 = CARTESIAN_POINT ( 'NONE',  ( 3.450005804356533368, -0.7992637590314204399, 1.791754569076028147 ) ) ;
#102893 = CARTESIAN_POINT ( 'NONE',  ( 1.224999999999962341, -0.3124999993172061785, -1.387778780781445676E-14 ) ) ;
#102894 = CARTESIAN_POINT ( 'NONE',  ( -8.143643823302737061, 12.65266822716189843, 0.000000000000000000 ) ) ;
#102895 = CARTESIAN_POINT ( 'NONE',  ( 6.103141704446003679, 10.27208242182903142, 0.7998128361456462443 ) ) ;
#102896 = CARTESIAN_POINT ( 'NONE',  ( 4.354221869268804390, 0.9056986662851629344, -1.917456963280274040 ) ) ;
#102897 = CARTESIAN_POINT ( 'NONE',  ( 7.180978637093494044, 8.406838493811077839, -1.199719254218452047 ) ) ;
#102898 = CARTESIAN_POINT ( 'NONE',  ( -9.809487834687324437, 11.40315621434539395, 1.199719254218462483 ) ) ;
#102899 = CARTESIAN_POINT ( 'NONE',  ( 2.096617048772158487, 2.047133997803842753, 0.3078910663548983795 ) ) ;
#102901 = CARTESIAN_POINT ( 'NONE',  ( -1.402160292154681736E-14, 0.6343750003414162508, 1.575800808251672791 ) ) ;
#102900 = CARTESIAN_POINT ( 'NONE',  ( 6.827182134110196365, 2.083530588508203607, 2.119847806254702594 ) ) ;
#102903 = ORIENTED_EDGE ( 'NONE', *, *, #71839, .F. ) ;
#102902 = CARTESIAN_POINT ( 'NONE',  ( 4.459788417035775332, -1.717034742021033455, -1.409269467666877995 ) ) ;
#102904 = CARTESIAN_POINT ( 'NONE',  ( 3.112262249421397620, 0.05891664663748399922, 2.298092032709637689 ) ) ;
#102905 = CARTESIAN_POINT ( 'NONE',  ( 7.104109303880752790, 11.23195192126214970, -0.7216878364870267237 ) ) ;
#102907 = CARTESIAN_POINT ( 'NONE',  ( 0.000000000000000000, -2.646874999522040639, -3.793834371823813001 ) ) ;
#102906 = CARTESIAN_POINT ( 'NONE',  ( 6.536439455564150514, 9.679577560583279450, 1.082531754730549078 ) ) ;
#102908 = CYLINDRICAL_SURFACE ( 'NONE', #140889, 0.08000000000000020983 ) ;
#102909 = DIRECTION ( 'NONE',  ( 3.330669073875478989E-16, -4.632576442341012461E-16, -1.000000000000000000 ) ) ;
#102910 = ORIENTED_EDGE ( 'NONE', *, *, #24698, .T. ) ;
#102911 = CARTESIAN_POINT ( 'NONE',  ( -0.4294425147611471982, -9.006862915010142245, 9.490288674561782045 ) ) ;
#102912 = EDGE_CURVE ( 'NONE', #204799, #169582, #23443, .T. ) ;
#102913 = CARTESIAN_POINT ( 'NONE',  ( 3.322422747544371280, -0.7792853099402965444, -1.746611395919236642 ) ) ;
#102914 = CARTESIAN_POINT ( 'NONE',  ( -11.81900460097218186, 13.75757134874138465, -1.592493057836596337 ) ) ;
#102915 = CARTESIAN_POINT ( 'NONE',  ( 4.506709144069167117, 1.332172526941363344, -1.095522069602150372 ) ) ;
#102916 = CARTESIAN_POINT ( 'NONE',  ( 3.327361509216096191, -1.530157842762596143, -1.313544516083162028 ) ) ;
#102917 = CARTESIAN_POINT ( 'NONE',  ( 3.727375017909192234, 2.287664543646179105, 0.2247039424928508056 ) ) ;
#102918 = CARTESIAN_POINT ( 'NONE',  ( 0.000000000000000000, 8.499999999999996447, 0.000000000000000000 ) ) ;
#102919 = CARTESIAN_POINT ( 'NONE',  ( 6.721333371289576419, -0.1616129481825591130, 2.070667135302119544 ) ) ;
#102920 = CARTESIAN_POINT ( 'NONE',  ( -6.319508997745553636, 6.545384383557486530, 0.7216878364870257245 ) ) ;
#102921 = CARTESIAN_POINT ( 'NONE',  ( 4.428786516960594000, 0.08554295028175006033, 1.767770697671824820 ) ) ;
#102923 = CARTESIAN_POINT ( 'NONE',  ( 0.5160991691709617690, -1.231265438625952724, -1.933346247471772861 ) ) ;
#102922 = CARTESIAN_POINT ( 'NONE',  ( 6.339319342841494453, 9.553567112360518365, -1.199719254218452047 ) ) ;
#102924 = CARTESIAN_POINT ( 'NONE',  ( -0.01232043299871990460, -0.3711077647031227333, -1.706071622908360119 ) ) ;
#102925 = CARTESIAN_POINT ( 'NONE',  ( -7.930593509350902792, 8.217056947189661287, -0.7998128361456362523 ) ) ;
#102926 = CARTESIAN_POINT ( 'NONE',  ( 5.279302027902110339, 1.469929824498400039, 1.625505876179579534 ) ) ;
#102927 = CARTESIAN_POINT ( 'NONE',  ( -3.546339698426324460, 6.295090860542775779, -1.199719254218450271 ) ) ;
#102928 = FACE_OUTER_BOUND ( 'NONE', #9733, .T. ) ;
#102929 = CARTESIAN_POINT ( 'NONE',  ( 3.913815762669449416, 7.330443837381343641, -0.8582294057540799104 ) ) ;
#102930 = EDGE_CURVE ( 'NONE', #94234, #115982, #162405, .T. ) ;
#102931 = CARTESIAN_POINT ( 'NONE',  ( 0.6784789811392475389, -1.161776791282279397, -1.834017514133066129 ) ) ;
#102932 = CARTESIAN_POINT ( 'NONE',  ( 0.7961116948485976730, -0.9110139862544311962, -1.799120828532501326 ) ) ;
#102933 = AXIS2_PLACEMENT_3D ( 'NONE', #191423, #74499, #75562 ) ;
#102934 = CARTESIAN_POINT ( 'NONE',  ( 1.364683531249988535, 5.405208333674750953, -0.7879004041258300672 ) ) ;
#102935 = CARTESIAN_POINT ( 'NONE',  ( 4.652910101842601343, -1.546415465631932884, 1.148725279867918170 ) ) ;
#102936 = CARTESIAN_POINT ( 'NONE',  ( 0.6823417656249934904, 11.94270833367473017, 1.181850606188764807 ) ) ;
#102937 = CARTESIAN_POINT ( 'NONE',  ( 0.6686063958157261178, 2.218491797483721051, -0.1167170572400257761 ) ) ;
#102939 = ORIENTED_EDGE ( 'NONE', *, *, #66694, .F. ) ;
#102938 = CARTESIAN_POINT ( 'NONE',  ( 10.21336978979620191, 10.81001959771741205, 0.7998128361456462443 ) ) ;
#102941 = CARTESIAN_POINT ( 'NONE',  ( -1.177073619093346180, 3.256928502340592946, 0.7750000000000100142 ) ) ;
#102940 = FACE_OUTER_BOUND ( 'NONE', #75564, .T. ) ;
#102942 = DIRECTION ( 'NONE',  ( 0.7592566023653005702, -0.6507913734559639396, 0.000000000000000000 ) ) ;
#102943 = CARTESIAN_POINT ( 'NONE',  ( 3.891353782322113375, 4.498666486585943147, -1.199719254218446718 ) ) ;
#102944 = DIRECTION ( 'NONE',  ( -0.000000000000000000, 1.000000000000000000, 0.000000000000000000 ) ) ;
#102945 = DIRECTION ( 'NONE',  ( 0.000000000000000000, 0.000000000000000000, -1.000000000000000000 ) ) ;
#102946 = CARTESIAN_POINT ( 'NONE',  ( 4.862738897425579410, 0.1637244223539826016, -1.732714468228998994 ) ) ;
#102947 = CARTESIAN_POINT ( 'NONE',  ( 2.224987305166142626, -1.792472147789250236, -0.7979012372742313453 ) ) ;
#102949 = CARTESIAN_POINT ( 'NONE',  ( -1.201851678989727383E-14, 3.009375000341419248, -1.575800808251660134 ) ) ;
#102948 = CARTESIAN_POINT ( 'NONE',  ( 4.449046963578762615, 8.342305224150557308, -0.7998128361456231517 ) ) ;
#102950 = CARTESIAN_POINT ( 'NONE',  ( -5.862510748852908016, 6.029743210627831473, 0.3741650707956689081 ) ) ;
#102951 = CARTESIAN_POINT ( 'NONE',  ( 9.837588353260175111, -6.372041098633662415, -9.403289436706798103E-13 ) ) ;
#102952 = CARTESIAN_POINT ( 'NONE',  ( 6.795372052238223048, -1.752927774724974297, 0.8811163259476795240 ) ) ;
#102953 = CARTESIAN_POINT ( 'NONE',  ( -6.672584156219988571, 10.93643194889866521, -0.7998128361456291469 ) ) ;
#102954 = CARTESIAN_POINT ( 'NONE',  ( -4.948362878863562742, 5.835806782504650236, 1.082531754730558626 ) ) ;
#102955 = CARTESIAN_POINT ( 'NONE',  ( 4.926970384345759513, -1.727065721694167832, 1.040790168839386798 ) ) ;
#102956 = CARTESIAN_POINT ( 'NONE',  ( 1.059873865361460332, 0.4390357074517194369, -2.219354932451859330 ) ) ;
#102958 = VERTEX_POINT ( 'NONE', #80067 ) ;
#102957 = CARTESIAN_POINT ( 'NONE',  ( -5.473741331615264549, 7.409117525016355010, -1.599625672291256295 ) ) ;
#102959 = CARTESIAN_POINT ( 'NONE',  ( -0.7500000000000249800, 0.2229166673494847872, 1.299038105676659116 ) ) ;
#102960 = CARTESIAN_POINT ( 'NONE',  ( 1.581098268704693055, 1.730367963306264301, -0.7109649657882493035 ) ) ;
#102961 = CARTESIAN_POINT ( 'NONE',  ( 0.07043219980315276740, -0.8200377064033654850, 1.527959277978730768 ) ) ;
#102962 = ADVANCED_FACE ( 'NONE', ( #78998 ), #178264, .F. ) ;
#102963 = CARTESIAN_POINT ( 'NONE',  ( 4.089532599075940134, -0.8378280566024614018, 2.025282237563410526 ) ) ;
#102964 = CARTESIAN_POINT ( 'NONE',  ( 5.860475213782774695, 0.9281710514958280145, 2.112872520220021144 ) ) ;
#102965 = CARTESIAN_POINT ( 'NONE',  ( 0.7958619820324459582, -0.7424864502722209325, 1.922671381412993652 ) ) ;
#102966 = CARTESIAN_POINT ( 'NONE',  ( 3.661996979482002867, -1.303408580024501218, 1.439711300692345652 ) ) ;
#102967 = CARTESIAN_POINT ( 'NONE',  ( -5.083944415000202888, 5.033616027029415463, 0.7216878364870317197 ) ) ;
#102968 = CARTESIAN_POINT ( 'NONE',  ( 5.905500869136258046, -0.4549164269060863020, 1.814235589242949587 ) ) ;
#102969 = ADVANCED_FACE ( 'NONE', ( #21440 ), #166662, .T. ) ;
#102970 = CARTESIAN_POINT ( 'NONE',  ( 0.4644214298860996903, 7.369507887687365866, -4.459343850249745778 ) ) ;
#102971 = CARTESIAN_POINT ( 'NONE',  ( -0.6801582343750282034, 1.432291667008027458, 1.178068619123810334 ) ) ;
#102972 = CARTESIAN_POINT ( 'NONE',  ( 4.570935502227962743, -0.9480417383296577682, 1.779625852769652905 ) ) ;
#102973 = CARTESIAN_POINT ( 'NONE',  ( -3.267151830768946663, 6.755501535964989479, -0.7216878364870257245 ) ) ;
#102974 = CARTESIAN_POINT ( 'NONE',  ( -5.281783360975562225, 8.319775133516907673, 1.199719254218452935 ) ) ;
#102975 = CARTESIAN_POINT ( 'NONE',  ( 8.398386088661320414, 11.88553530582519357, -1.199719254218446718 ) ) ;
#102977 = CARTESIAN_POINT ( 'NONE',  ( -1.270916165646621243, 3.165225491120026380, 0.7750000000000152323 ) ) ;
#102976 = CARTESIAN_POINT ( 'NONE',  ( 2.297230901563730665, 1.410920830412419003, 1.158640757216542028 ) ) ;
#102978 = CARTESIAN_POINT ( 'NONE',  ( -4.274563570058511175, 8.209017608368725405, 0.000000000000000000 ) ) ;
#102979 = CARTESIAN_POINT ( 'NONE',  ( -4.685224601974262271, 7.623789914682047808, -1.199719254218453823 ) ) ;
#102980 = CARTESIAN_POINT ( 'NONE',  ( -10.48284956170200921, 5.077895721165493370, 7.121295720048954614 ) ) ;
#102981 = ORIENTED_EDGE ( 'NONE', *, *, #7522, .F. ) ;
#102982 = CARTESIAN_POINT ( 'NONE',  ( -5.356880090730904875, 7.343055753976412525, 1.443375672974058777 ) ) ;
#102983 = CARTESIAN_POINT ( 'NONE',  ( -4.613852347352193739, 4.277249248199312071, 1.214306433183764966E-14 ) ) ;
#102984 = CARTESIAN_POINT ( 'NONE',  ( -8.784793466650835825, 12.33634391347959713, 1.199719254218462483 ) ) ;
#102985 = CARTESIAN_POINT ( 'NONE',  ( 5.672522982350666432, 0.8204337683548768023, 1.845723718880077469 ) ) ;
#102987 = VERTEX_POINT ( 'NONE', #55046 ) ;
#102986 = CARTESIAN_POINT ( 'NONE',  ( -0.07530339154229391541, -0.9103892951793614019, -1.913193754492636067 ) ) ;
#102988 = CARTESIAN_POINT ( 'NONE',  ( -5.966470118465691641, 9.118576350588734059, -1.199719254218452047 ) ) ;
#102989 = CARTESIAN_POINT ( 'NONE',  ( 4.385172619016207918, 7.203452924572514959, 1.199719254218462483 ) ) ;
#102990 = CARTESIAN_POINT ( 'NONE',  ( 5.700091634879108859, -2.061077814751426818, -0.002399610236311285148 ) ) ;
#102991 = CARTESIAN_POINT ( 'NONE',  ( 4.852185490356213826, 0.1948433276699329531, -2.006959737079899497 ) ) ;
#102992 = ORIENTED_EDGE ( 'NONE', *, *, #142604, .F. ) ;
#102993 = ORIENTED_EDGE ( 'NONE', *, *, #129717, .F. ) ;
#102994 =( BOUNDED_CURVE ( )  B_SPLINE_CURVE ( 2, ( #141455, #107912, #186941, #155528, #104649, #207462, #7108, #123128, #189087 ),
 .UNSPECIFIED., .F., .T. ) 
 B_SPLINE_CURVE_WITH_KNOTS ( ( 3, 2, 2, 2, 3 ),
 ( 0.9375000000000000000, 0.9404761904761904656, 0.9464285714285713969, 0.9523809523809523281, 0.9553571428571427937 ),
 .UNSPECIFIED. ) 
 CURVE ( )  GEOMETRIC_REPRESENTATION_ITEM ( )  RATIONAL_B_SPLINE_CURVE ( ( 0.9330127018922194093, 0.9330127018922194093, 1.000000000000000000, 0.8660254037844387076, 1.000000000000000000, 0.8660254037844387076, 1.000000000000000000, 0.9330127018922206306, 0.9330127018922194093 ) ) 
 REPRESENTATION_ITEM ( '' )  );
#102995 = CARTESIAN_POINT ( 'NONE',  ( 3.577053382146960558, 7.342256794902024986, 0.3077596360769136452 ) ) ;
#102996 = FACE_OUTER_BOUND ( 'NONE', #209387, .T. ) ;
#102997 = B_SPLINE_CURVE_WITH_KNOTS ( 'NONE', 3,
 ( #71125, #137241, #205404, #203263 ),
 .UNSPECIFIED., .F., .F.,
 ( 4, 4 ),
 ( 0.000000000000000000, 6.033646489354907845E-05 ),
 .UNSPECIFIED. ) ;
#102999 = ORIENTED_EDGE ( 'NONE', *, *, #41033, .T. ) ;
#102998 = CARTESIAN_POINT ( 'NONE',  ( -5.284646014276622950, 9.387447126623207794, -0.7998128361456362523 ) ) ;
#103000 = CARTESIAN_POINT ( 'NONE',  ( 4.624709440338444111, 8.453137518702421360, 0.3515692964491355932 ) ) ;
#103001 = CARTESIAN_POINT ( 'NONE',  ( 5.659529772124847646, -0.4871306767523299608, -1.956261131662299535 ) ) ;
#103002 = CARTESIAN_POINT ( 'NONE',  ( 3.872867692073681756, 1.733033312621637068, -0.6219614626309655225 ) ) ;
#103003 = CARTESIAN_POINT ( 'NONE',  ( 1.843739406749204335, 9.999999999999998224, 0.7750000000000004663 ) ) ;
#103004 = CARTESIAN_POINT ( 'NONE',  ( 2.561488099217507308, -2.008522245525693695, -1.136227173556729975 ) ) ;
#103005 = CARTESIAN_POINT ( 'NONE',  ( 7.343676480457483002, 8.596652644402405841, -1.199719254218452047 ) ) ;
#103006 = CARTESIAN_POINT ( 'NONE',  ( 5.360679719606757487, -1.569739296358707570, 1.486333574453831297 ) ) ;
#103007 = CARTESIAN_POINT ( 'NONE',  ( 8.609591239877852686, 10.00327685373437347, -1.199719254218445830 ) ) ;
#103008 = CARTESIAN_POINT ( 'NONE',  ( -0.1235792489666731608, -0.1369701924231395973, -1.910945132828122395 ) ) ;
#103009 = CARTESIAN_POINT ( 'NONE',  ( -5.708146366553361162, 6.618257834855742594, -1.199719254218446718 ) ) ;
#103010 = CARTESIAN_POINT ( 'NONE',  ( 3.796502476701520301, -2.125173906124724343, 0.8757568767029444423 ) ) ;
#103011 = CARTESIAN_POINT ( 'NONE',  ( 2.609770642201841184, 0.3830433331901660354, -0.1872689674646474400 ) ) ;
#103012 = DIRECTION ( 'NONE',  ( -0.6507913734559658270, -0.7592566023652989049, 0.000000000000000000 ) ) ;
#103013 = CARTESIAN_POINT ( 'NONE',  ( 2.430351462470367707, 1.813921419787648315, 0.4566771774890953095 ) ) ;
#103014 = ORIENTED_EDGE ( 'NONE', *, *, #64072, .T. ) ;
#103015 = CARTESIAN_POINT ( 'NONE',  ( 0.2453084554022276487, -1.520975263078115258, -1.253778558530042053 ) ) ;
#103017 = CARTESIAN_POINT ( 'NONE',  ( -5.725286006720766707, 9.901527117808042178, 0.7998128361456291469 ) ) ;
#103016 = CARTESIAN_POINT ( 'NONE',  ( -1.364683531249997417, 5.759375000341418804, 1.214306433183764966E-14 ) ) ;
#103018 = CARTESIAN_POINT ( 'NONE',  ( 1.313402753022639091, 1.947697196196996217, 1.037691534346518729 ) ) ;
#103019 = ORIENTED_EDGE ( 'NONE', *, *, #74775, .F. ) ;
#103020 = CARTESIAN_POINT ( 'NONE',  ( 1.284279953904121641, 3.284610286488902187, 0.7750000000000135669 ) ) ;
#103021 = CARTESIAN_POINT ( 'NONE',  ( 2.842405760359353106, 6.467890487061221272, -0.7998128361456291469 ) ) ;
#103022 = CARTESIAN_POINT ( 'NONE',  ( -4.249591082879585535, 7.045274465746411252, 1.199719254218464037 ) ) ;
#103023 = CARTESIAN_POINT ( 'NONE',  ( -1.048552960303294919E-14, -9.091017468556975345, -10.23550087314634993 ) ) ;
#103024 = CARTESIAN_POINT ( 'NONE',  ( 6.508667090220362716, 1.461156067397894054, -1.323708773930740268 ) ) ;
#103025 = CARTESIAN_POINT ( 'NONE',  ( 0.2359759974720798681, -2.107749471535870445, 0.9397143452993106383 ) ) ;
#103026 = CARTESIAN_POINT ( 'NONE',  ( 0.8011316787140990714, -1.684513426579350659, 1.005393624328714264 ) ) ;
#103027 = CARTESIAN_POINT ( 'NONE',  ( 4.153227615898272163, 1.745077553047107433, -1.099210343703932669 ) ) ;
#103028 = CARTESIAN_POINT ( 'NONE',  ( 5.504247177468179153, 7.444707678511436555, 1.443375672974062551 ) ) ;
#103029 = CARTESIAN_POINT ( 'NONE',  ( 5.885121196783658526, 9.023669275293071834, 1.199719254218452047 ) ) ;
#103030 = ORIENTED_EDGE ( 'NONE', *, *, #117446, .T. ) ;
#103031 = CARTESIAN_POINT ( 'NONE',  ( 7.904040366642695048, 9.284097184913720824, 1.082531754730558626 ) ) ;
#103032 = CARTESIAN_POINT ( 'NONE',  ( -1.201851678989727383E-14, 4.509375000341417916, -1.575800808251660134 ) ) ;
#103033 = CARTESIAN_POINT ( 'NONE',  ( -10.36154070669560134, 3.772592418234324896, -6.054033915187476467 ) ) ;
#103034 = CARTESIAN_POINT ( 'NONE',  ( 5.192409643909512873, 6.120528008391641350, -1.082531754730549078 ) ) ;
#103035 = CARTESIAN_POINT ( 'NONE',  ( 6.654729725391004713, -0.5723678854598751586, -2.094333189781839355 ) ) ;
#103037 = CARTESIAN_POINT ( 'NONE',  ( 5.091278345985558396, -0.6575378499774006125, 1.720029930423284448 ) ) ;
#103036 = CARTESIAN_POINT ( 'NONE',  ( 9.481348452320370157, -9.006862915010128035, -0.5950054837411730135 ) ) ;
#103038 = EDGE_CURVE ( 'NONE', #41277, #176125, #44203, .T. ) ;
#103039 = FACE_OUTER_BOUND ( 'NONE', #122850, .T. ) ;
#103040 = CARTESIAN_POINT ( 'NONE',  ( 1.963753466588878283, 3.754052640047455647, 0.4000000000000453748 ) ) ;
#103041 = CARTESIAN_POINT ( 'NONE',  ( -9.579665964948882007, -7.473374494045003757, 5.204170427930421283E-15 ) ) ;
#103042 = CARTESIAN_POINT ( 'NONE',  ( -4.351171265391168497, 7.394090626460979365, 1.174491979025530597 ) ) ;
#103043 = DIRECTION ( 'NONE',  ( 0.000000000000000000, 1.000000000000000000, 0.000000000000000000 ) ) ;
#103044 = CARTESIAN_POINT ( 'NONE',  ( 5.544801429207002030, 7.539493339695484408, -1.337888636821100041 ) ) ;
#103045 = CARTESIAN_POINT ( 'NONE',  ( 1.364683531249992088, 5.446875000341417916, 1.214306433183764966E-14 ) ) ;
#103046 = CARTESIAN_POINT ( 'NONE',  ( 0.9614044138335111622, -1.507904615609249488, -1.175938229252027956 ) ) ;
#103048 = EDGE_CURVE ( 'NONE', #80885, #44585, #92902, .T. ) ;
#103047 = CARTESIAN_POINT ( 'NONE',  ( 1.568863545881917343, 0.1344791104000986337, -1.764800092583326929 ) ) ;
#103050 = CARTESIAN_POINT ( 'NONE',  ( 6.445953599032193004, -1.316566896158730238, -1.522954124987923930 ) ) ;
#103049 = AXIS2_PLACEMENT_3D ( 'NONE', #70606, #35993, #136720 ) ;
#103052 = CARTESIAN_POINT ( 'NONE',  ( 4.007376490896687571, -1.831982314510060883, 0.5597367571646000295 ) ) ;
#103051 = CARTESIAN_POINT ( 'NONE',  ( -10.16591625214838679, 10.75465713712827487, 1.040834085586084257E-14 ) ) ;
#103053 = CARTESIAN_POINT ( 'NONE',  ( -3.104453987849326690, 4.644948957289396496, 1.040834085586084257E-14 ) ) ;
#103054 = CARTESIAN_POINT ( 'NONE',  ( 5.336368261742150843, -1.095693791129894956, 1.636418990172120003 ) ) ;
#103055 = CARTESIAN_POINT ( 'NONE',  ( 6.152604576718359475, 1.998398145963925954, 0.2921455800133450631 ) ) ;
#103056 = FACE_OUTER_BOUND ( 'NONE', #111065, .T. ) ;
#103057 = CARTESIAN_POINT ( 'NONE',  ( 4.030043484472041193, 1.001115284758803625, -1.580040089582811280 ) ) ;
#103059 = ORIENTED_EDGE ( 'NONE', *, *, #204467, .T. ) ;
#103058 = CARTESIAN_POINT ( 'NONE',  ( 6.094358798449852621, -1.717309950877196956, -0.1615796057152525667 ) ) ;
#103061 = CARTESIAN_POINT ( 'NONE',  ( 2.250290310188348464, 5.569163095287620990, 0.7216878364870438212 ) ) ;
#103060 = CARTESIAN_POINT ( 'NONE',  ( 3.897267319706390065, 1.864829029706360330, -1.179861312946443697 ) ) ;
#103062 = CARTESIAN_POINT ( 'NONE',  ( -0.6823417656250003738, 2.780208333674753618, -1.181850606188749264 ) ) ;
#103063 = CARTESIAN_POINT ( 'NONE',  ( 1.012259994385706019, 2.060384570222949741, -0.09942193159017187476 ) ) ;
#103064 = CARTESIAN_POINT ( 'NONE',  ( 6.103141704446003679, 10.27208242182903142, 0.7998128361456462443 ) ) ;
#103065 = CARTESIAN_POINT ( 'NONE',  ( -9.124801077197171040, 10.60435499727357289, -1.199719254218441611 ) ) ;
#103066 = CARTESIAN_POINT ( 'NONE',  ( -7.790615780789408085, 15.44814080676280277, -9.079613476728765065 ) ) ;
#103067 = CARTESIAN_POINT ( 'NONE',  ( -4.525370967935856470, 8.233940877497639477, -0.3192380598915856571 ) ) ;
#103069 = CIRCLE ( 'NONE', #26964, 0.07999999999999998779 ) ;
#103068 =( GEOMETRIC_REPRESENTATION_CONTEXT ( 3 ) GLOBAL_UNCERTAINTY_ASSIGNED_CONTEXT ( ( #174125 ) ) GLOBAL_UNIT_ASSIGNED_CONTEXT ( ( #67169, #162586, #199309 ) ) REPRESENTATION_CONTEXT ( 'NONE', 'WORKASPACE' ) );
#103070 = ORIENTED_EDGE ( 'NONE', *, *, #141149, .T. ) ;
#103071 = CARTESIAN_POINT ( 'NONE',  ( 3.262232429473245432, -2.068111870375147987, 0.09887451149894616043 ) ) ;
#103072 = CARTESIAN_POINT ( 'NONE',  ( -1.500000000000011324, 5.129166666666691299, -0.8660254037844313801 ) ) ;
#103073 = CARTESIAN_POINT ( 'NONE',  ( 5.148345644887269756, 7.029489223833707001, -1.599625672291256295 ) ) ;
#103074 = CARTESIAN_POINT ( 'NONE',  ( -6.486107617800834113, 6.842887492708185526, 0.6303255377333163434 ) ) ;
#103075 = CARTESIAN_POINT ( 'NONE',  ( 0.6451828087791033894, 0.1507176824743546029, 2.014122433718650296 ) ) ;
#103076 = CARTESIAN_POINT ( 'NONE',  ( -5.000000000000024869, 3.300000000000025135, 0.7750000000000238920 ) ) ;
#103078 = CARTESIAN_POINT ( 'NONE',  ( 6.954969614130424027, 11.05795561655343384, 1.040834085586084257E-14 ) ) ;
#103077 = CARTESIAN_POINT ( 'NONE',  ( 0.1747926744264677867, 0.7439089246787933263, -1.939883394317852616 ) ) ;
#103079 = CARTESIAN_POINT ( 'NONE',  ( 6.432970213454214381, 1.034009579150240610, 1.730599625746793935 ) ) ;
#103080 = CARTESIAN_POINT ( 'NONE',  ( 6.333208386676280277, -1.543085173044305591, -1.135110930932172746 ) ) ;
#103081 = CARTESIAN_POINT ( 'NONE',  ( 3.263397454411249399, 2.137687552337414587, -0.4822058812353549606 ) ) ;
#103082 = CARTESIAN_POINT ( 'NONE',  ( 0.7499999999999885647, 3.347916667349487341, -1.299038105676658228 ) ) ;
#103083 = CARTESIAN_POINT ( 'NONE',  ( 2.127084423382288314, 1.709874882824816478, 0.8565708355050825062 ) ) ;
#103084 = CARTESIAN_POINT ( 'NONE',  ( -3.581325132304157943, 7.329963087663487364, -0.7998128361456281477 ) ) ;
#103085 = CARTESIAN_POINT ( 'NONE',  ( 2.684151225381301575, 6.075334163012737321, 0.000000000000000000 ) ) ;
#103087 = CARTESIAN_POINT ( 'NONE',  ( 1.019157904985489305, -1.821734318179563106, 0.8647433871810317196 ) ) ;
#103086 = CARTESIAN_POINT ( 'NONE',  ( 10.30245174296169175, 3.603753425775775288, -5.948123287112220936 ) ) ;
#103088 = CARTESIAN_POINT ( 'NONE',  ( -0.6823417656250039265, 11.63020833367473017, -1.181850606188755259 ) ) ;
#103090 = CARTESIAN_POINT ( 'NONE',  ( -4.305596300791617814, 7.180890229968955651, 1.199719254218452935 ) ) ;
#103089 = CARTESIAN_POINT ( 'NONE',  ( 6.585463931165095985, -0.9389328202267492873, 1.978239266594773671 ) ) ;
#103092 = ORIENTED_EDGE ( 'NONE', *, *, #136534, .T. ) ;
#103091 = CARTESIAN_POINT ( 'NONE',  ( 3.381609400508314600, 1.093566088711795281, 1.333772831174476758 ) ) ;
#103093 = CARTESIAN_POINT ( 'NONE',  ( 6.337546739384100292, 9.481222731668410120, 1.199719254218460707 ) ) ;
#103094 = CARTESIAN_POINT ( 'NONE',  ( 4.635998460869027227, 7.496083073400806818, -1.199719254218452047 ) ) ;
#103095 = CARTESIAN_POINT ( 'NONE',  ( 6.385527162356455122, 10.39360608948380538, 1.056142170575426150E-14 ) ) ;
#103096 = CARTESIAN_POINT ( 'NONE',  ( 1.750371521623844462, -1.952110535733902585, -0.1955497077021361163 ) ) ;
#103097 = FILL_AREA_STYLE ('',( #135608 ) ) ;
#103098 = CARTESIAN_POINT ( 'NONE',  ( 4.355193658487811703, 6.104145239700998538, -1.599625672291255185 ) ) ;
#103099 = CARTESIAN_POINT ( 'NONE',  ( 0.1755611466353655115, 0.2306421705509461850, -2.278008211689793061 ) ) ;
#103100 = EDGE_LOOP ( 'NONE', ( #40524, #148476, #212992, #51251 ) ) ;
#103101 = PRESENTATION_LAYER_ASSIGNMENT (  '', '', ( #203406 ) ) ;
#103102 = CARTESIAN_POINT ( 'NONE',  ( 1.697517146273963306E-12, -6.372041098632814204, 9.837588353259947738 ) ) ;
#103103 = ORIENTED_EDGE ( 'NONE', *, *, #112585, .F. ) ;
#103104 = CARTESIAN_POINT ( 'NONE',  ( 3.932113804724958417, -0.9344168170181254007, -1.551720482391373057 ) ) ;
#103105 = ORIENTED_EDGE ( 'NONE', *, *, #184735, .F. ) ;
#103106 = CARTESIAN_POINT ( 'NONE',  ( 8.890396042259068210, 11.39521468743417998, -1.599625672291257406 ) ) ;
#103107 = CARTESIAN_POINT ( 'NONE',  ( -5.385662150563701900, 6.164098921825184263, 1.139024650766025548 ) ) ;
#103108 = CARTESIAN_POINT ( 'NONE',  ( 4.723216582411014386, 1.578617123877921857, 0.8883131493910937371 ) ) ;
#103109 = CARTESIAN_POINT ( 'NONE',  ( 0.1963700886235890397, -6.681311647492909067, 9.612263720970508629 ) ) ;
#103110 = CARTESIAN_POINT ( 'NONE',  ( 0.4644097342742965484, -8.233137084989849086, 9.488641820551103834 ) ) ;
#103111 = CARTESIAN_POINT ( 'NONE',  ( 5.458613854904844409, 6.252117202148153474, -1.007154897844428687 ) ) ;
#103113 = EDGE_CURVE ( 'NONE', #87871, #202176, #32760, .T. ) ;
#103112 = AXIS2_PLACEMENT_3D ( 'NONE', #149454, #112764, #178777 ) ;
#103115 = CARTESIAN_POINT ( 'NONE',  ( 0.6823417656249934904, 15.19270833367473372, 1.181850606188764807 ) ) ;
#103114 = CARTESIAN_POINT ( 'NONE',  ( 4.844130899818556379, -0.8777628995196519179, 1.641066814073613767 ) ) ;
#103116 = CARTESIAN_POINT ( 'NONE',  ( 2.337376834759529398, 0.5087095155123841916, -1.846764813590465515 ) ) ;
#103117 = CARTESIAN_POINT ( 'NONE',  ( -6.649736275991368295, -8.039737506397923283, -6.784764760059130317 ) ) ;
#103118 = DIRECTION ( 'NONE',  ( 0.000000000000000000, 0.000000000000000000, 1.000000000000000000 ) ) ;
#103119 = FILL_AREA_STYLE_COLOUR ( '', #188035 ) ;
#103120 = CARTESIAN_POINT ( 'NONE',  ( 5.666945020832167224, 8.594891043404107478, 1.082531754730558626 ) ) ;
#103121 = CARTESIAN_POINT ( 'NONE',  ( -4.277761160311629673, 4.949475094240346706, 1.199719254218462483 ) ) ;
#103122 = DIRECTION ( 'NONE',  ( -5.662137425588289679E-15, 4.419671232041788924E-16, 1.000000000000000000 ) ) ;
#103123 = CARTESIAN_POINT ( 'NONE',  ( -5.315678745009726924, 8.359319748223434487, -1.199719254218453823 ) ) ;
#103124 = CARTESIAN_POINT ( 'NONE',  ( 0.7969595931820300239, 1.710167217185576183, 1.202247156440580556 ) ) ;
#103125 = CARTESIAN_POINT ( 'NONE',  ( 5.611095471209277541, 7.639640364534566075, 1.599625672291268286 ) ) ;
#103126 = CARTESIAN_POINT ( 'NONE',  ( 1.324926479183065497, -0.04897172810776688479, 1.825096452545173609 ) ) ;
#103127 = CARTESIAN_POINT ( 'NONE',  ( -3.418627288940168096, 7.140148937072163804, -0.7998128361456281477 ) ) ;
#103128 = CARTESIAN_POINT ( 'NONE',  ( 2.449991753796490368, 1.825138167369045661, 0.04731899098397300552 ) ) ;
#103129 = EDGE_CURVE ( 'NONE', #107579, #85668, #168089, .T. ) ;
#103130 = CARTESIAN_POINT ( 'NONE',  ( 9.703911172298809618, 13.32558040432908619, 8.137536601084995880 ) ) ;
#103131 = CARTESIAN_POINT ( 'NONE',  ( 2.320441991784210067, -0.7354482596747033973, -1.765520077574176394 ) ) ;
#103132 = CARTESIAN_POINT ( 'NONE',  ( 1.715229078707868782, -1.687648322675440626, -1.015142298990583614 ) ) ;
#103133 = CARTESIAN_POINT ( 'NONE',  ( 3.983879235506204264, -1.921370479222897165, -0.2818874784011967671 ) ) ;
#103134 = ORIENTED_EDGE ( 'NONE', *, *, #151508, .T. ) ;
#103135 = CARTESIAN_POINT ( 'NONE',  ( -5.738844160334429567, 9.917344963690652548, 0.000000000000000000 ) ) ;
#103137 = CARTESIAN_POINT ( 'NONE',  ( 4.500305224345508393, -0.9970752094022590217, 1.871535012320741265 ) ) ;
#103136 = CARTESIAN_POINT ( 'NONE',  ( 7.506374323821472849, 8.786466794993730289, -1.199719254218452047 ) ) ;
#103138 = CARTESIAN_POINT ( 'NONE',  ( 8.880754312151170282, 10.31963377138658089, 1.199719254218453823 ) ) ;
#103139 = CARTESIAN_POINT ( 'NONE',  ( 5.931217288863120274, 6.131947776268360961, 0.7575795127007216578 ) ) ;
#103140 = CARTESIAN_POINT ( 'NONE',  ( -10.91132967064557491, -5.166862915010145052, 0.4350687514514811616 ) ) ;
#103141 = ORIENTED_EDGE ( 'NONE', *, *, #15073, .F. ) ;
#103142 = CARTESIAN_POINT ( 'NONE',  ( 5.515134625708930649, 9.656350506627580543, 0.000000000000000000 ) ) ;
#103143 = DIRECTION ( 'NONE',  ( 0.000000000000000000, 1.000000000000000000, 0.000000000000000000 ) ) ;
#103144 = CARTESIAN_POINT ( 'NONE',  ( 3.439906511156048285, 0.8199118703316324863, -1.631291955839441865 ) ) ;
#103145 = CARTESIAN_POINT ( 'NONE',  ( 10.99943592164171235, -9.901472394401615418, -0.1113975120799817059 ) ) ;
#103146 = CARTESIAN_POINT ( 'NONE',  ( -7.348156068926747331, 11.51667314714914347, 0.7216878364870458196 ) ) ;
#103147 = CARTESIAN_POINT ( 'NONE',  ( -5.025714415505916577, 8.007183762769660262, 1.161964715574652196 ) ) ;
#103148 = DIRECTION ( 'NONE',  ( 1.000000000000000000, -0.000000000000000000, -0.000000000000000000 ) ) ;
#103149 = CARTESIAN_POINT ( 'NONE',  ( 4.891396039733495016, 1.386484060982313249, 1.255958711209571810 ) ) ;
#103150 = CARTESIAN_POINT ( 'NONE',  ( 7.670162217029129259, 9.971608557999250166, 1.599625672291281386 ) ) ;
#103151 = CARTESIAN_POINT ( 'NONE',  ( 2.701685709380332145, -0.6039436678997743835, 1.829457556829715115 ) ) ;
#103152 = CARTESIAN_POINT ( 'NONE',  ( 6.174655700867183405, 1.320063289540554408, -1.451312704123429498 ) ) ;
#103153 = AXIS2_PLACEMENT_3D ( 'NONE', #60193, #105791, #124229 ) ;
#103154 = CARTESIAN_POINT ( 'NONE',  ( -1.402160292154681736E-14, 9.484375000341398021, 1.575800808251682339 ) ) ;
#103155 = CARTESIAN_POINT ( 'NONE',  ( -6.144869935491728441, 8.192100896205577243, -1.599625672291263179 ) ) ;
#103156 = CARTESIAN_POINT ( 'NONE',  ( 3.649115900372475796, 7.409052317076538330, 1.040834085586084257E-14 ) ) ;
#103157 = CARTESIAN_POINT ( 'NONE',  ( -4.285785955251283141, 8.014184357852876417, 0.000000000000000000 ) ) ;
#103158 = CARTESIAN_POINT ( 'NONE',  ( 1.335737955381975928, 0.6106153762303926369, -2.027287256620951439 ) ) ;
#103159 = CARTESIAN_POINT ( 'NONE',  ( -0.6125000000000019318, 0.5208333340161186431, -1.060881119635944891 ) ) ;
#103160 = CARTESIAN_POINT ( 'NONE',  ( -3.578681416171278329, 3.551814636441860351, 2.500000000000000444 ) ) ;
#103161 = CARTESIAN_POINT ( 'NONE',  ( 6.631696427350994405, 1.982895789845315671, -0.5951614246157420629 ) ) ;
#103163 = CARTESIAN_POINT ( 'NONE',  ( 3.999300167945916584, 7.828775037665852921, -0.06519116529766534607 ) ) ;
#103162 = CARTESIAN_POINT ( 'NONE',  ( 0.6086344939593493208, -0.2706599535906920040, 1.821105742621460744 ) ) ;
#103164 = CARTESIAN_POINT ( 'NONE',  ( 0.2811772945982879968, -2.253408246774822210, 0.4517706223704387458 ) ) ;
#103165 = CARTESIAN_POINT ( 'NONE',  ( 4.351804120306567825, 8.020929207092235558, 1.040834085586084257E-14 ) ) ;
#103167 = DIRECTION ( 'NONE',  ( 0.6260462619842731558, 0.7797859179643593652, 0.000000000000000000 ) ) ;
#103166 = CARTESIAN_POINT ( 'NONE',  ( 5.573810548993915148, 5.675402860013913475, 0.000000000000000000 ) ) ;
#103168 = CARTESIAN_POINT ( 'NONE',  ( 1.166458296791187621, -1.450650017800562575, 1.774850106915156100 ) ) ;
#103169 = CARTESIAN_POINT ( 'NONE',  ( -0.009341296487041779104, -9.943660733012633202, -9.579650209538295158 ) ) ;
#103170 = CARTESIAN_POINT ( 'NONE',  ( -4.450819567036169211, 8.414649604842665553, -0.7998128361456362523 ) ) ;
#103171 = CARTESIAN_POINT ( 'NONE',  ( 6.298774621056003831, 1.615917059943820622, 1.076740554856120413 ) ) ;
#103172 = ORIENTED_EDGE ( 'NONE', *, *, #142087, .F. ) ;
#103173 = CARTESIAN_POINT ( 'NONE',  ( 7.253248993186713456, 11.40594822545244824, 0.7216878364870438212 ) ) ;
#103174 = EDGE_CURVE ( 'NONE', #8487, #25034, #181133, .T. ) ;
#103176 = ORIENTED_EDGE ( 'NONE', *, *, #189245, .F. ) ;
#103175 =( BOUNDED_SURFACE ( )  B_SPLINE_SURFACE ( 3, 2, ( 
 ( #199632, #119536, #104297 ),
 ( #68561, #17675, #38224 ),
 ( #154111, #168223, #19822 ),
 ( #70688, #83761, #203894 ) ),
 .UNSPECIFIED., .F., .F., .T. ) 
 B_SPLINE_SURFACE_WITH_KNOTS ( ( 4, 4 ),
 ( 3, 3 ),
 ( 0.000000000000000000, 3.124373657233979538E-05 ),
 ( 0.000000000000000000, 1.000000000000000000 ),
 .UNSPECIFIED. ) 
 GEOMETRIC_REPRESENTATION_ITEM ( )  RATIONAL_B_SPLINE_SURFACE ( (
 ( 1.000000000000000000, 0.7045118851641305469, 1.000000000000000000),
 ( 1.000000000000000000, 0.7044892147945193139, 1.000000000000000000),
 ( 1.000000000000000000, 0.7053501046726611268, 1.000000000000000000),
 ( 1.000000000000000000, 0.7071067811869123920, 1.000000000000000000) ) ) 
 REPRESENTATION_ITEM ( '' )  SURFACE ( )  );
#103177 = CARTESIAN_POINT ( 'NONE',  ( 6.205323455156911194, 1.660478276859885582, -0.9486371710855368011 ) ) ;
#103178 = CARTESIAN_POINT ( 'NONE',  ( 6.280482454654814362, -0.5424645211669875122, -1.942098458069536848 ) ) ;
#103179 =( REPRESENTATION_RELATIONSHIP ('NONE','NONE', #84563, #135824 ) REPRESENTATION_RELATIONSHIP_WITH_TRANSFORMATION ( #108889 )SHAPE_REPRESENTATION_RELATIONSHIP( ) );
#103181 = CARTESIAN_POINT ( 'NONE',  ( -9.828980619278564011E-14, 7.054063922337708625, 3.955400951015630273 ) ) ;
#103180 = CARTESIAN_POINT ( 'NONE',  ( -7.015454420067433361, 10.27211502579893754, 1.199719254218453823 ) ) ;
#103182 = CARTESIAN_POINT ( 'NONE',  ( -10.33392256004288079, 4.765625372279607141, 5.445010993851796322 ) ) ;
#103184 = CARTESIAN_POINT ( 'NONE',  ( 1.498528727375374459, 1.449451107477307987, -1.015301706168385998 ) ) ;
#103183 = CARTESIAN_POINT ( 'NONE',  ( 2.695356974763486679, -0.6552250210129506591, 1.985377264055338209 ) ) ;
#103185 = CARTESIAN_POINT ( 'NONE',  ( 0.000000000000000000, 4.000000000000003553, 6.450000000000003730 ) ) ;
#103186 = CARTESIAN_POINT ( 'NONE',  ( 4.259948577007838466, 1.078808246893525391, 2.022540810160260882 ) ) ;
#103187 = CARTESIAN_POINT ( 'NONE',  ( 3.187183321348503018, -0.7043554338151243321, 1.591608241653941214 ) ) ;
#103188 = CARTESIAN_POINT ( 'NONE',  ( 9.459838494033030898, 12.05956421450382088, 1.599625672291281386 ) ) ;
#103189 = CARTESIAN_POINT ( 'NONE',  ( 4.712340909201580885, 7.655425606447271214, -1.199719254218452047 ) ) ;
#103190 = CARTESIAN_POINT ( 'NONE',  ( 3.198323437492247123, -1.162659817912135019, -1.286436312214979338 ) ) ;
#103191 = CARTESIAN_POINT ( 'NONE',  ( 3.649033395009869452, -0.4203537998966280220, -2.129940419224036763 ) ) ;
#103192 = CARTESIAN_POINT ( 'NONE',  ( 4.985647801523278133, 6.839675073242382553, -1.599625672291256295 ) ) ;
#103193 = CARTESIAN_POINT ( 'NONE',  ( 4.962125165302472496, -1.116212726388360998, 1.679221540125563905 ) ) ;
#103194 = CARTESIAN_POINT ( 'NONE',  ( 1.625000000000001554, -2.052068128417951165, 9.007296548519099900E-14 ) ) ;
#103195 = AXIS2_PLACEMENT_3D ( 'NONE', #70349, #118133, #37882 ) ;
#103196 = CARTESIAN_POINT ( 'NONE',  ( -0.7500000000000006661, 2.889583334016148974, -1.299038105676652011 ) ) ;
#103197 = CARTESIAN_POINT ( 'NONE',  ( 1.571183270939533694, 0.1444824169965253369, -1.921038573443895059 ) ) ;
#103198 = CARTESIAN_POINT ( 'NONE',  ( -6.009258394948636914E-15, 8.718750000682796042, -1.732050807568875195 ) ) ;
#103199 = CARTESIAN_POINT ( 'NONE',  ( 4.166425639909420831, 2.220860392705526820, -0.05667459126444325535 ) ) ;
#103200 = ORIENTED_EDGE ( 'NONE', *, *, #144483, .F. ) ;
#103201 = CARTESIAN_POINT ( 'NONE',  ( -0.1106856583841424602, 0.7110496148716296538, -2.078439740052108853 ) ) ;
#103202 = CARTESIAN_POINT ( 'NONE',  ( -0.7500000000000215383, 1.441666666666688190, 1.299038105676659116 ) ) ;
#103203 = CARTESIAN_POINT ( 'NONE',  ( 7.637320603199683866, 7.804628880021436288, -0.7998128361456281477 ) ) ;
#103204 = CARTESIAN_POINT ( 'NONE',  ( 3.334942598837264960, 6.834590765378040444, 1.214306433183764966E-14 ) ) ;
#103205 = CARTESIAN_POINT ( 'NONE',  ( -1.642778471875000035, -2.267708332855375541, -2.845375778867859751 ) ) ;
#103206 = CARTESIAN_POINT ( 'NONE',  ( 0.3467151180503316166, 1.136585144892443777, -1.908366640695156047 ) ) ;
#103207 = CARTESIAN_POINT ( 'NONE',  ( 5.512146440779991607, 1.959692598237902761, -0.09458084330612320789 ) ) ;
#103208 = CARTESIAN_POINT ( 'NONE',  ( 9.110716038703335684, 9.731516254683127087, -0.7216878364870197293 ) ) ;
#103209 = CARTESIAN_POINT ( 'NONE',  ( 0.001013208909606179041, 3.413442832661036430, 2.083547725167233633 ) ) ;
#103210 = CARTESIAN_POINT ( 'NONE',  ( 0.4917760118960182170, 1.601382895956671826, 1.452064325093614716 ) ) ;
#103211 = CARTESIAN_POINT ( 'NONE',  ( 5.204350862799327793, 7.165104988056252289, -1.599625672291281386 ) ) ;
#103213 = VECTOR ( 'NONE', #109867, 1000.000000000000114 ) ;
#103212 = VECTOR ( 'NONE', #105756, 1000.000000000000000 ) ;
#103214 = CARTESIAN_POINT ( 'NONE',  ( -5.072158865288277418, 7.010880990960010273, 1.443375672974058777 ) ) ;
#103215 = CARTESIAN_POINT ( 'NONE',  ( 2.910651161647914265, 0.6924047515337331538, 1.943132885215630878 ) ) ;
#103216 = CARTESIAN_POINT ( 'NONE',  ( -6.389970470742427189, 6.349387058821269747, -0.7998128361456291469 ) ) ;
#103217 = CARTESIAN_POINT ( 'NONE',  ( -1.201851678989727383E-14, 3.993750000682817713, 1.732050807568877637 ) ) ;
#103218 = CARTESIAN_POINT ( 'NONE',  ( -1.364683531250000748, -1.240624999658580752, 0.000000000000000000 ) ) ;
#103219 = CARTESIAN_POINT ( 'NONE',  ( 5.061713478001653499, 1.850364105758989020, -0.2730526881008291662 ) ) ;
#103220 = CARTESIAN_POINT ( 'NONE',  ( 4.078545790824074757, -0.6587176911285116399, 1.604389539659875297 ) ) ;
#103221 = CARTESIAN_POINT ( 'NONE',  ( 3.262975863287612466, 1.697222826579761534, -0.3846178214849705901 ) ) ;
#103222 = EDGE_CURVE ( 'NONE', #210726, #58569, #54546, .T. ) ;
#103223 = CARTESIAN_POINT ( 'NONE',  ( 0.2227793574855509162, 2.196107815404338748, 0.6574155683778097892 ) ) ;
#103224 = CARTESIAN_POINT ( 'NONE',  ( 0.6823417656249917140, 3.405208333674754506, 1.181850606188765695 ) ) ;
#103225 = CARTESIAN_POINT ( 'NONE',  ( 6.093324021728765416, -0.7037842761165017391, 1.968882989559454622 ) ) ;
#103226 = CARTESIAN_POINT ( 'NONE',  ( -0.02968770228140016343, 0.003472272166151618711, -1.826291111852257343 ) ) ;
#103227 = CARTESIAN_POINT ( 'NONE',  ( -0.1945363205450327815, 1.000000000000000888, 11.93115981699678585 ) ) ;
#103228 = CARTESIAN_POINT ( 'NONE',  ( 1.846327496167538884, 0.3419342931599393398, -1.987046799686801757 ) ) ;
#103229 = CARTESIAN_POINT ( 'NONE',  ( 0.1995291103054769866, -0.5802879427523646161, 2.113158525371459096 ) ) ;
#103230 = CARTESIAN_POINT ( 'NONE',  ( 9.681426354872444406, 13.43812210156014686, -8.165041025796163865 ) ) ;
#103231 = CARTESIAN_POINT ( 'NONE',  ( -7.666245793523398078, 11.03137162816423356, 1.199719254218453823 ) ) ;
#103232 = CARTESIAN_POINT ( 'NONE',  ( 6.681470773436232413, 6.689470745297396270, -0.7998128361456281477 ) ) ;
#103233 = CARTESIAN_POINT ( 'NONE',  ( 2.614065066921432479, -0.6628553294307990562, 2.014303955012682223 ) ) ;
#103234 = CARTESIAN_POINT ( 'NONE',  ( -1.364683531250014514, -0.7614583329919104582, -0.7879004041258359514 ) ) ;
#103236 = EDGE_CURVE ( 'NONE', #108282, #135381, #108689, .T. ) ;
#103235 = CARTESIAN_POINT ( 'NONE',  ( 5.039593146249602640, -1.293522693445446015, -1.288650932716684849 ) ) ;
#103237 = ORIENTED_EDGE ( 'NONE', *, *, #93674, .F. ) ;
#103238 = CARTESIAN_POINT ( 'NONE',  ( -7.456058132872594335, 7.663432341298296535, 0.000000000000000000 ) ) ;
#103239 = CARTESIAN_POINT ( 'NONE',  ( 2.275391796764376640, 5.643962577969389827, -0.5307291018262025872 ) ) ;
#103240 = CARTESIAN_POINT ( 'NONE',  ( 7.648208051440442468, 8.095533279534887328, 0.000000000000000000 ) ) ;
#103241 = CARTESIAN_POINT ( 'NONE',  ( 1.642778471875000035, -0.6635416661887084677, -2.845375778867859751 ) ) ;
#103242 = CARTESIAN_POINT ( 'NONE',  ( -6.669721502918952716, 9.868759955792373972, 1.199719254218452047 ) ) ;
#103243 = CARTESIAN_POINT ( 'NONE',  ( 2.390883991616198578, -1.934022345091526818, -0.5824046739145176677 ) ) ;
#103244 = CARTESIAN_POINT ( 'NONE',  ( 0.2004011508093841987, -2.105512755765154509, -0.05116925900590372361 ) ) ;
#103245 = CARTESIAN_POINT ( 'NONE',  ( -4.442231607132987925, 5.211633625523774960, -1.199719254218453823 ) ) ;
#103246 = CARTESIAN_POINT ( 'NONE',  ( 4.592532296707762640, 1.824399381888962779, 0.3660411688805977337 ) ) ;
#103247 = CARTESIAN_POINT ( 'NONE',  ( 8.218213668177886788, 12.73966637951625813, 0.7998128361456462443 ) ) ;
#103248 = LINE ( 'NONE', #4635, #64264 ) ;
#103249 = CARTESIAN_POINT ( 'NONE',  ( -4.416205349749324327, 6.175325546172740765, 1.599625672291267398 ) ) ;
#103250 = CARTESIAN_POINT ( 'NONE',  ( -7.965578943228732278, 9.251929174310385307, -1.199719254218446718 ) ) ;
#103251 = CARTESIAN_POINT ( 'NONE',  ( 4.934128534657983067, 0.9357288403324083292, -1.567518238613223813 ) ) ;
#103253 = CARTESIAN_POINT ( 'NONE',  ( -4.377891688998395203, 7.365737962781053305, -1.202262209786943759 ) ) ;
#103252 = CARTESIAN_POINT ( 'NONE',  ( -5.413448473606448985, 9.537716662508005427, 0.000000000000000000 ) ) ;
#103254 = CARTESIAN_POINT ( 'NONE',  ( -1.364683531250000748, -0.4906249996585801409, 0.000000000000000000 ) ) ;
#103255 = CARTESIAN_POINT ( 'NONE',  ( 2.143477642578191844, -0.07974179160761747653, -1.732128062886995057 ) ) ;
#103256 = CARTESIAN_POINT ( 'NONE',  ( 6.404252597826388893, 1.360807738692754176, -1.240355271200761278 ) ) ;
#103258 = CARTESIAN_POINT ( 'NONE',  ( 6.778713617152772208, 10.85232362007950258, -0.7216878364870267237 ) ) ;
#103257 = CARTESIAN_POINT ( 'NONE',  ( 5.057380973065424001, -1.947307563149714316, -1.238062830034118988 ) ) ;
#103259 = CARTESIAN_POINT ( 'NONE',  ( 3.902768115887398803, 5.646591783325653147, -1.599625672291269396 ) ) ;
#103260 = CARTESIAN_POINT ( 'NONE',  ( 1.089218918643636069, 1.818803954151678726, -0.9688405272365168130 ) ) ;
#103261 = CARTESIAN_POINT ( 'NONE',  ( 4.981731378017507872, 7.899438143407371271, -1.199719254218452047 ) ) ;
#103262 = CARTESIAN_POINT ( 'NONE',  ( 0.3860920070548681804, -0.1017387759476989784, 2.013677428805898728 ) ) ;
#103263 = CARTESIAN_POINT ( 'NONE',  ( 8.561438655473816439, 14.95580071018964041, -8.346266854202061936 ) ) ;
#103264 = CARTESIAN_POINT ( 'NONE',  ( -6.424584688029276514, 8.588711117491191871, 1.599625672291269396 ) ) ;
#103265 = EDGE_CURVE ( 'NONE', #204799, #206986, #30282, .T. ) ;
#103266 = CARTESIAN_POINT ( 'NONE',  ( 0.4441303031895106890, 1.966005183986684335, 0.1476035654904006011 ) ) ;
#103268 = CARTESIAN_POINT ( 'NONE',  ( -5.171509248969888617, 4.998125310078441075, 0.7998128361456281477 ) ) ;
#103267 = CARTESIAN_POINT ( 'NONE',  ( 3.779479514802902340, 0.2291398179169491789, -1.898525689255560422 ) ) ;
#103269 = CARTESIAN_POINT ( 'NONE',  ( 4.635508124736155366, -2.018492079602551392, 0.8926152185086615454 ) ) ;
#103270 = CARTESIAN_POINT ( 'NONE',  ( -0.6125000000000175859, 2.104166667349471886, 1.060881119635908476 ) ) ;
#103271 = CARTESIAN_POINT ( 'NONE',  ( 3.390947816749319443, 6.970206529600588397, -1.734723475976807094E-15 ) ) ;
#103272 = CARTESIAN_POINT ( 'NONE',  ( -3.485854892044994102, 7.080931450778859215, -0.7216878364870458196 ) ) ;
#103273 = CARTESIAN_POINT ( 'NONE',  ( 6.252600707356171128, 2.097339953035493476, 0.3115551810550786227 ) ) ;
#103274 = ORIENTED_EDGE ( 'NONE', *, *, #210003, .T. ) ;
#103275 = CARTESIAN_POINT ( 'NONE',  ( 3.804037270277782490, -0.6727452520632947186, 2.207335857111696331 ) ) ;
#103276 = CARTESIAN_POINT ( 'NONE',  ( 3.578520225191741844, 1.246510459297203610, -1.514941731618473009 ) ) ;
#103277 = CARTESIAN_POINT ( 'NONE',  ( -6.296835998904160014, 6.311006518335105397, 0.000000000000000000 ) ) ;
#103278 = CARTESIAN_POINT ( 'NONE',  ( 1.024179675629211861, 0.9620134025654383247, 1.709582039726687652 ) ) ;
#103279 = CARTESIAN_POINT ( 'NONE',  ( 8.559698219247815487, 14.95637777618389208, 8.348061575730120865 ) ) ;
#103280 = CARTESIAN_POINT ( 'NONE',  ( 6.447267651612376582, -6.532648833121157850, 6.949925879317534694 ) ) ;
#103281 = ORIENTED_EDGE ( 'NONE', *, *, #203182, .F. ) ;
#103282 = CARTESIAN_POINT ( 'NONE',  ( 5.893767612163585135, -2.000732204962274441, 0.2516274335107801519 ) ) ;
#103283 = CARTESIAN_POINT ( 'NONE',  ( -8.833300774503376473, 10.26427131079744193, 1.199719254218462483 ) ) ;
#103284 = LINE ( 'NONE', #68619, #30292 ) ;
#103285 = CARTESIAN_POINT ( 'NONE',  ( 3.168971741543443077, 1.575705016696099081, -1.493804678357780524 ) ) ;
#103286 = CARTESIAN_POINT ( 'NONE',  ( 4.878955176071344546, 6.785476686873604280, -1.599625672291269396 ) ) ;
#103287 = CARTESIAN_POINT ( 'NONE',  ( 0.4398875993102538962, -2.011672884243600024, 0.6710486789910232730 ) ) ;
#103288 = CARTESIAN_POINT ( 'NONE',  ( -1.201851678989727383E-14, 2.243750000682818158, 1.732050807568877637 ) ) ;
#103289 = CARTESIAN_POINT ( 'NONE',  ( 10.21336978979620191, 10.81001959771741205, 0.7998128361456462443 ) ) ;
#103290 = CARTESIAN_POINT ( 'NONE',  ( 0.1895306985669804323, 2.637130183346470869, -2.069997288510221800 ) ) ;
#103291 = CARTESIAN_POINT ( 'NONE',  ( 5.043764445095213489, 7.992138250556588552, 1.161813593947092382 ) ) ;
#103292 = ORIENTED_EDGE ( 'NONE', *, *, #63733, .T. ) ;
#103293 = CARTESIAN_POINT ( 'NONE',  ( 1.229839986812499175, -1.305282058118014010, -1.594721697489847045 ) ) ;
#103295 = CARTESIAN_POINT ( 'NONE',  ( 0.2053016774634074115, 2.557622706723280182, 1.991036163670555359 ) ) ;
#103294 = CARTESIAN_POINT ( 'NONE',  ( -9.829825065107822724, 11.42688298316931572, 1.199719254218462483 ) ) ;
#103296 = CARTESIAN_POINT ( 'NONE',  ( 0.6823417656249899377, 2.342708333674753618, 1.181850606188767472 ) ) ;
#103297 = DIRECTION ( 'NONE',  ( 2.949029909160572061E-17, 1.000000000000000000, -8.673600428462353400E-15 ) ) ;
#103298 = VERTEX_POINT ( 'NONE', #192490 ) ;
#103299 = CARTESIAN_POINT ( 'NONE',  ( 4.248624793116656306, 1.876006594227698221, 0.3698101955103145766 ) ) ;
#103300 = CARTESIAN_POINT ( 'NONE',  ( 6.821687566331318564, 7.987665577921906568, 1.199719254218452935 ) ) ;
#103301 = CARTESIAN_POINT ( 'NONE',  ( -3.358669367883384105, 4.941533567329135401, -1.599625672291262513 ) ) ;
#103302 = CARTESIAN_POINT ( 'NONE',  ( 0.2283786121510515688, 1.249231189971045319, -1.312217732533569103 ) ) ;
#103304 = CARTESIAN_POINT ( 'NONE',  ( 0.2861690844194793026, -0.6482510287857257136, -1.802810126718904504 ) ) ;
#103303 = CARTESIAN_POINT ( 'NONE',  ( 1.436838838544733044, 7.449283400311756509, -4.203727439823553347 ) ) ;
#103305 = CIRCLE ( 'NONE', #207039, 11.18000000000000149 ) ;
#103306 = CARTESIAN_POINT ( 'NONE',  ( 2.102089431743926706, 0.7944251937819692966, -1.912079865474418439 ) ) ;
#103307 = CARTESIAN_POINT ( 'NONE',  ( -1.364683531250014514, -0.4489583329919089039, -0.7879004041258359514 ) ) ;
#103308 = CARTESIAN_POINT ( 'NONE',  ( 1.024223545076022424, 1.176019522272594875, -1.582147633265261977 ) ) ;
#103309 = CARTESIAN_POINT ( 'NONE',  ( 2.947667120405720986, 0.6567698719579934119, -1.703645827024417914 ) ) ;
#103311 = CARTESIAN_POINT ( 'NONE',  ( 6.276967689384127524, 6.888745287521969907, 0.7578909454171089966 ) ) ;
#103310 = CARTESIAN_POINT ( 'NONE',  ( 6.393228082638676923, 1.922373441260841087, -1.083778638264052852 ) ) ;
#103312 = CARTESIAN_POINT ( 'NONE',  ( 0.6823417656249882723, 1.676041667008083769, -1.181850606188749264 ) ) ;
#103313 = CARTESIAN_POINT ( 'NONE',  ( 4.158677964895734824, -0.6440432224011168882, -1.959637643944433849 ) ) ;
#103314 = CARTESIAN_POINT ( 'NONE',  ( -6.413170354464012846, 7.440785820751486312, 1.199719254218450271 ) ) ;
#103315 = CARTESIAN_POINT ( 'NONE',  ( 6.753933077901968396, 11.03133902419432566, 0.7998128361456462443 ) ) ;
#103316 = FACE_OUTER_BOUND ( 'NONE', #70640, .T. ) ;
#103317 = CARTESIAN_POINT ( 'NONE',  ( 4.320244504248938355, 8.192035688265757898, 1.040834085586084257E-14 ) ) ;
#103319 = CARTESIAN_POINT ( 'NONE',  ( 1.499999999999989120, 3.504166666666683749, 0.8660254037844524744 ) ) ;
#103318 = CARTESIAN_POINT ( 'NONE',  ( 4.893641883129576264, 1.558557130586870398, 1.416501212539149845 ) ) ;
#103320 = CARTESIAN_POINT ( 'NONE',  ( 6.162566008723842081, -0.7415158119226210598, -1.933206815039355320 ) ) ;
#103321 = CARTESIAN_POINT ( 'NONE',  ( 1.364683531249986537, 1.967708333674750731, -0.7879004041258239610 ) ) ;
#103322 = CARTESIAN_POINT ( 'NONE',  ( 3.286554482555790191, -2.129011082553730727, -0.3730605165198074280 ) ) ;
#103323 = CARTESIAN_POINT ( 'NONE',  ( 3.844402842710480162, 1.078523329768014349, -1.707388236230653611 ) ) ;
#103324 = CARTESIAN_POINT ( 'NONE',  ( 6.620655732516679493, 7.051632961313193171, 2.871890384929445261 ) ) ;
#103327 = CARTESIAN_POINT ( 'NONE',  ( 5.124618876285529367, 7.962177208099690873, -1.082531754730549078 ) ) ;
#103326 = CARTESIAN_POINT ( 'NONE',  ( 1.737499999999999378, -0.4666666666666673402, -3.009438278150925683 ) ) ;
#103325 = CARTESIAN_POINT ( 'NONE',  ( 4.072979602660211640, 7.274571027119063338, -0.9456576254009234628 ) ) ;
#103328 = CARTESIAN_POINT ( 'NONE',  ( -5.094831863685302942, 9.165997284266655498, 0.7998128361456291469 ) ) ;
#103329 = CARTESIAN_POINT ( 'NONE',  ( 2.835173002801576914, -1.651343842416473917, -1.157098616274463865 ) ) ;
#103330 = CARTESIAN_POINT ( 'NONE',  ( -9.341731535015849630, 10.85744053139533349, 1.199719254218462483 ) ) ;
#103332 = CARTESIAN_POINT ( 'NONE',  ( 1.777638883463141806, 0.9165151389911742053, 1.199999999999999734 ) ) ;
#103331 = CARTESIAN_POINT ( 'NONE',  ( -3.066115294984855133, 6.728884944124295053, 0.7998128361456341429 ) ) ;
#103333 = CARTESIAN_POINT ( 'NONE',  ( 0.4019237886466847653, 12.57366454968463110, 1.499999999999997113 ) ) ;
#103334 = CARTESIAN_POINT ( 'NONE',  ( 4.207107738942202246, 3.802713871720993399, 1.214306433183764966E-14 ) ) ;
#103335 = CARTESIAN_POINT ( 'NONE',  ( -10.94883623364795966, 5.391122956802682609, -4.806613302849912728 ) ) ;
#103337 = CARTESIAN_POINT ( 'NONE',  ( 4.464470365011488973, -1.956567236562205325, -0.4871837624095613495 ) ) ;
#103336 = CARTESIAN_POINT ( 'NONE',  ( -6.819388077549415783, 10.89977715720891815, 0.7216878364870458196 ) ) ;
#103338 = CARTESIAN_POINT ( 'NONE',  ( 0.7499999999999902300, 4.566666666666691299, -1.299038105676658228 ) ) ;
#103339 = CARTESIAN_POINT ( 'NONE',  ( 6.475633750228043439, 1.648727237068832396, -0.5065655092456061714 ) ) ;
#103340 = CARTESIAN_POINT ( 'NONE',  ( 4.715203562502613188, 8.723097599553565118, 0.7998128361456341429 ) ) ;
#103342 = CARTESIAN_POINT ( 'NONE',  ( -6.056815632531343141, 6.015240258500212711, 0.3115616189311651296 ) ) ;
#103341 = CARTESIAN_POINT ( 'NONE',  ( 7.754900677336718395, 11.99120852362745460, -0.7216878364870267237 ) ) ;
#103343 = LINE ( 'NONE', #165143, #46999 ) ;
#103344 = CARTESIAN_POINT ( 'NONE',  ( 5.676977070516882051, -0.04517083460114229565, -1.870152005306220611 ) ) ;
#103345 = CARTESIAN_POINT ( 'NONE',  ( 0.1354021741525688050, -0.09674683032310191222, 2.010873914455484801 ) ) ;
#103346 = DIRECTION ( 'NONE',  ( 0.000000000000000000, -0.000000000000000000, 1.000000000000000000 ) ) ;
#103347 = LINE ( 'NONE', #169412, #92007 ) ;
#103348 = VERTEX_POINT ( 'NONE', #160011 ) ;
#103349 = CARTESIAN_POINT ( 'NONE',  ( 9.856414487010587422, 11.56186699200962487, 1.082531754730548412 ) ) ;
#103350 = B_SPLINE_CURVE_WITH_KNOTS ( 'NONE', 3,
 ( #77925, #127849, #177572, #30254, #95275, #161323, #96338, #13971, #32386, #100576, #167711, #82184, #98451, #163458, #151477, #19315 ),
 .UNSPECIFIED., .F., .F.,
 ( 4, 2, 2, 2, 2, 2, 2, 4 ),
 ( 2.453269466693426431E-18, 8.859500147854104581E-05, 0.0001771900029570796522, 0.0003543800059141551844, 0.0007087600118283104772, 0.001063140017742465445, 0.001240330020699543633, 0.001417520023656621822 ),
 .UNSPECIFIED. ) ;
#103351 = CARTESIAN_POINT ( 'NONE',  ( 0.8609541034889022226, -0.05231784723681161264, -2.015913592316537439 ) ) ;
#103352 = CARTESIAN_POINT ( 'NONE',  ( 0.9491188979427627181, -1.637284982186116400, 0.7756696494297130595 ) ) ;
#103353 = CARTESIAN_POINT ( 'NONE',  ( 4.163762572728282763, 6.911454530608037494, -1.082531754730548412 ) ) ;
#103354 = DIRECTION ( 'NONE',  ( -0.6507913734559640506, -0.7592566023653003482, 0.000000000000000000 ) ) ;
#103355 = EDGE_CURVE ( 'NONE', #62036, #43349, #44142, .T. ) ;
#103356 = PRODUCT_DEFINITION ( 'UNKNOWN', '', #142178, #113337 ) ;
#103357 = CARTESIAN_POINT ( 'NONE',  ( 7.253248993186713456, 11.40594822545244824, 0.7216878364870438212 ) ) ;
#103358 = CARTESIAN_POINT ( 'NONE',  ( 5.940443861082012944, 10.08226827123770697, 0.7998128361456462443 ) ) ;
#103360 = CARTESIAN_POINT ( 'NONE',  ( 5.870691181925934643, -0.2860506952705432204, -1.894010149965511758 ) ) ;
#103359 = CARTESIAN_POINT ( 'NONE',  ( -5.915435094264120508, 5.795762452929912101, 0.000000000000000000 ) ) ;
#103361 = CARTESIAN_POINT ( 'NONE',  ( 1.499999999999968914, 5.045833333333356485, -0.8660254037844440367 ) ) ;
#103362 = DIRECTION ( 'NONE',  ( 0.000000000000000000, 0.000000000000000000, 1.000000000000000000 ) ) ;
#103363 = CARTESIAN_POINT ( 'NONE',  ( -10.99370838174331055, -6.893137084989843011, 0.3821126922044791874 ) ) ;
#103365 = ORIENTED_EDGE ( 'NONE', *, *, #55251, .T. ) ;
#103364 = CARTESIAN_POINT ( 'NONE',  ( 4.202664430556261266, 4.005456045178151570, 0.7216878364870317197 ) ) ;
#103366 = CARTESIAN_POINT ( 'NONE',  ( -10.13488352141530768, 11.78278451552804817, 1.199719254218462483 ) ) ;
#103367 = CARTESIAN_POINT ( 'NONE',  ( 3.625982885822197410, -1.285997354380935098, -1.737435825693342872 ) ) ;
#103368 = CARTESIAN_POINT ( 'NONE',  ( -6.997416678428844072, 8.296645891989347987, 1.082531754730549078 ) ) ;
#103369 = CARTESIAN_POINT ( 'NONE',  ( 6.590672070018850803, 7.822110515511036866, -1.082531754730548412 ) ) ;
#103370 = CARTESIAN_POINT ( 'NONE',  ( 0.7914572142167939361, -0.05789999323873443182, -2.119991495365561640 ) ) ;
#103371 = CARTESIAN_POINT ( 'NONE',  ( 5.807590115592688562, -0.4411735188285180187, 1.771332044933016547 ) ) ;
#103372 = EDGE_CURVE ( 'NONE', #82008, #24990, #37226, .T. ) ;
#103373 = CARTESIAN_POINT ( 'NONE',  ( 2.319545460040703500, -1.913138470506670075, 0.4751570986292509846 ) ) ;
#103374 = CARTESIAN_POINT ( 'NONE',  ( 4.658414424252744546, 1.907665749568526747, 0.1350064596054162680 ) ) ;
#103375 = ORIENTED_EDGE ( 'NONE', *, *, #133002, .T. ) ;
#103376 = FACE_OUTER_BOUND ( 'NONE', #210209, .T. ) ;
#103377 = CARTESIAN_POINT ( 'NONE',  ( 5.740667673349629574, -1.921128208576441843, -0.4332487841941043971 ) ) ;
#103378 = CARTESIAN_POINT ( 'NONE',  ( 0.2517628464389579102, 0.7423079377118102506, 1.794666626680625932 ) ) ;
#103379 = ORIENTED_EDGE ( 'NONE', *, *, #191821, .T. ) ;
#103380 = CARTESIAN_POINT ( 'NONE',  ( -5.971440312176176768, 5.931378217152456500, 0.000000000000000000 ) ) ;
#103381 = CARTESIAN_POINT ( 'NONE',  ( -4.995253251992230581, 4.792493313604505367, 0.000000000000000000 ) ) ;
#103383 = CARTESIAN_POINT ( 'NONE',  ( 4.692530563661249765, 8.488719734331187539, 0.000000000000000000 ) ) ;
#103382 = CARTESIAN_POINT ( 'NONE',  ( 7.422199028477372451, 10.74665040227725044, -1.199719254218441611 ) ) ;
#103385 = ORIENTED_EDGE ( 'NONE', *, *, #117140, .F. ) ;
#103384 = CARTESIAN_POINT ( 'NONE',  ( 4.529883686416775745, -1.874680353417649492, 0.3764776581506729114 ) ) ;
#103386 = CARTESIAN_POINT ( 'NONE',  ( 0.3236265600991515834, -0.1057403636935544400, 2.204373366691187108 ) ) ;
#103387 = STYLED_ITEM ( 'NONE', ( #168756 ), #21012 ) ;
#103388 = CARTESIAN_POINT ( 'NONE',  ( 1.519204386771063398, 8.761797318405452728, 2.483775294098995889 ) ) ;
#103389 = CARTESIAN_POINT ( 'NONE',  ( 5.936195100277483760, -1.120233448768311435, -1.672418650214458014 ) ) ;
#103390 = CARTESIAN_POINT ( 'NONE',  ( 0.07680821025391781909, 4.096870002413341538, -2.365840309731046975 ) ) ;
#103391 = CARTESIAN_POINT ( 'NONE',  ( -0.03829719982252339366, 15.47641828198856295, 11.98867496343628680 ) ) ;
#103392 = CARTESIAN_POINT ( 'NONE',  ( -6.710127771514629025, -7.162053774861991684, -6.725445687907746439 ) ) ;
#103393 = CARTESIAN_POINT ( 'NONE',  ( 2.945825538390863141, 1.462269270728074222, 1.465923284304726959 ) ) ;
#103394 = CARTESIAN_POINT ( 'NONE',  ( -5.925076824372040640, 6.871343368977510302, 1.199719254218450271 ) ) ;
#103395 = CARTESIAN_POINT ( 'NONE',  ( -4.740694425254917910, 8.216228820413899570, 0.6995903363472668612 ) ) ;
#103396 = B_SPLINE_CURVE_WITH_KNOTS ( 'NONE', 3,
 ( #148636, #108996, #192286, #59103, #10342, #110062, #175013, #191223, #49009, #65219, #82549 ),
 .UNSPECIFIED., .F., .F.,
 ( 4, 1, 1, 1, 1, 1, 1, 1, 4 ),
 ( 0.000000000000000000, 0.2255509035172358623, 0.3975895543896152406, 0.5252637114030099807, 0.6177357421269481508, 0.6841390318922365710, 0.7334310489036851566, 0.7741974304450970346, 1.000000000000000000 ),
 .UNSPECIFIED. ) ;
#103398 = CARTESIAN_POINT ( 'NONE',  ( 1.006953172832128152, 1.636353683469338183, -1.412668763314451903 ) ) ;
#103397 = CARTESIAN_POINT ( 'NONE',  ( -4.776550190716183586, 4.467063398790632966, 1.214306433183764966E-14 ) ) ;
#103399 = CARTESIAN_POINT ( 'NONE',  ( -11.15698333951949195, 7.317141096829810287, 4.424938813521728243 ) ) ;
#103400 = DIRECTION ( 'NONE',  ( 0.3162277660168376636, 0.9486832980505138790, 0.000000000000000000 ) ) ;
#103401 = DIRECTION ( 'NONE',  ( 0.000000000000000000, 1.000000000000000000, 0.000000000000000000 ) ) ;
#103402 = CARTESIAN_POINT ( 'NONE',  ( 1.364683531250000303, 12.81770833367473372, -0.7879004041258355073 ) ) ;
#103404 = CARTESIAN_POINT ( 'NONE',  ( -5.550083779947821760, 7.568460058062819407, -1.599625672291271394 ) ) ;
#103403 = CARTESIAN_POINT ( 'NONE',  ( 6.825078400183510752, 3.697836898538444217, 2.470016017273040543 ) ) ;
#103405 = CARTESIAN_POINT ( 'NONE',  ( 2.624232735793774030, 2.001858099149746550, 0.2420302859193757539 ) ) ;
#103406 = CARTESIAN_POINT ( 'NONE',  ( 6.117740286212093537, 0.1793736470585994280, 1.724862758254825712 ) ) ;
#103407 = CARTESIAN_POINT ( 'NONE',  ( -2.819205876637805641, 5.376491725131008259, -1.199719254218446718 ) ) ;
#103408 = CARTESIAN_POINT ( 'NONE',  ( 3.204029340230400091, 0.7494766052340908757, -1.929994576353490032 ) ) ;
#103409 = CARTESIAN_POINT ( 'NONE',  ( 4.640305734921336800, 0.8116497034467985427, 1.955664341570842790 ) ) ;
#103410 = CARTESIAN_POINT ( 'NONE',  ( 7.721532178182734185, 8.967207948423393304, 1.199719254218462483 ) ) ;
#103411 = CARTESIAN_POINT ( 'NONE',  ( -1.001543065824772872E-14, 4.821875000341421469, 1.575800808251672791 ) ) ;
#103412 = CARTESIAN_POINT ( 'NONE',  ( 3.326963294591319009, -1.817917149290064982, -0.7580491890798303212 ) ) ;
#103413 = B_SPLINE_CURVE_WITH_KNOTS ( 'NONE', 3,
 ( #132727, #98088, #183564, #68729, #147894, #48274 ),
 .UNSPECIFIED., .F., .F.,
 ( 4, 2, 4 ),
 ( 0.001916662113439827377, 0.002237152494173779219, 0.002557642874907731494 ),
 .UNSPECIFIED. ) ;
#103414 = CARTESIAN_POINT ( 'NONE',  ( 0.8789968191965717992, -1.730013457311157188, -0.8152767527440167861 ) ) ;
#103415 = CARTESIAN_POINT ( 'NONE',  ( 4.506013928309719141, -0.9778350203078637337, -2.073373472838499598 ) ) ;
#103416 = CARTESIAN_POINT ( 'NONE',  ( 3.264084022359412973, 0.8216391472936384055, 1.630427331384459055 ) ) ;
#103417 = CARTESIAN_POINT ( 'NONE',  ( 5.716698046817569434, 6.698511138489155137, -1.199719254218452047 ) ) ;
#103418 = CARTESIAN_POINT ( 'NONE',  ( 5.544921637864819175, 7.492161215640853023, -1.443375672974057666 ) ) ;
#103419 = CARTESIAN_POINT ( 'NONE',  ( -7.019370843573183194, 9.212351955633947043, 1.599625672291283607 ) ) ;
#103420 = CARTESIAN_POINT ( 'NONE',  ( 4.218997895827368616, 1.553599190986540091, -1.280318274872578543 ) ) ;
#103421 = CARTESIAN_POINT ( 'NONE',  ( 2.729291793292155432, 0.1011638768560127188, -1.959297240552673181 ) ) ;
#103422 = CARTESIAN_POINT ( 'NONE',  ( -6.496328159242330536, 10.73079995242472862, 0.000000000000000000 ) ) ;
#103423 = CARTESIAN_POINT ( 'NONE',  ( -5.656776405399756236, 7.622658444431597680, -1.599625672291256295 ) ) ;
#103424 = CARTESIAN_POINT ( 'NONE',  ( -1.743066579297358008E-15, 1.875000000682791379, 1.224999999999958566 ) ) ;
#103426 = CARTESIAN_POINT ( 'NONE',  ( 5.049538948550310380, 0.5532318831848512808, -1.681206329525422483 ) ) ;
#103425 = CARTESIAN_POINT ( 'NONE',  ( 6.333939708931282553, 2.067699390258682879, 0.3079354192142729763 ) ) ;
#103427 = CARTESIAN_POINT ( 'NONE',  ( -2.364368148460603614, 5.338642027447423999, -0.7873643464157237259 ) ) ;
#103428 = CARTESIAN_POINT ( 'NONE',  ( 1.218978173989828884, -0.05078841826402366588, 2.191026318449231791 ) ) ;
#103429 = CARTESIAN_POINT ( 'NONE',  ( 6.703062861115646420, -0.3699031437116198084, 1.706546720392573491 ) ) ;
#103430 = AXIS2_PLACEMENT_3D ( 'NONE', #144346, #210346, #178949 ) ;
#103431 = CARTESIAN_POINT ( 'NONE',  ( 6.401421083946654100, 10.62007503124645957, -0.7998128361456291469 ) ) ;
#103432 = CARTESIAN_POINT ( 'NONE',  ( 0.1331715793776652446, 7.629137130509056952, -2.553547540661147419 ) ) ;
#103433 = CARTESIAN_POINT ( 'NONE',  ( 0.6678281019706671096, -0.7765434158916887375, -2.163364592831273470 ) ) ;
#103434 = CARTESIAN_POINT ( 'NONE',  ( 0.1170720436180875679, -0.1011795954627830590, 2.189343785608413917 ) ) ;
#103435 = CARTESIAN_POINT ( 'NONE',  ( 6.696678128945787734, -1.136521523357211017, -1.309519827187540564 ) ) ;
#103436 = CARTESIAN_POINT ( 'NONE',  ( 3.282038605231399231, 1.400092287458438722, 1.705885466304429166 ) ) ;
#103437 = CARTESIAN_POINT ( 'NONE',  ( 6.443812750726708671, 1.492410320797844747, 1.577172898185905670 ) ) ;
#103438 = CARTESIAN_POINT ( 'NONE',  ( -11.04536101718726293, 0.000000000000000000, -1.100000000000002087 ) ) ;
#103439 = CARTESIAN_POINT ( 'NONE',  ( 1.393934723748765814, -2.100642827862955198, 0.2651745403093440090 ) ) ;
#103440 = CARTESIAN_POINT ( 'NONE',  ( 4.343750000000002665, 1.895863743164175608, 0.7852924748297558377 ) ) ;
#103441 = CARTESIAN_POINT ( 'NONE',  ( 6.620655732516651071, 2.021119449029490589, 2.477762541108457839 ) ) ;
#103442 = CARTESIAN_POINT ( 'NONE',  ( 4.946275538936047766, 1.921213873770099445, 0.1421515328255736899 ) ) ;
#103443 = ORIENTED_EDGE ( 'NONE', *, *, #15247, .T. ) ;
#103444 = CONICAL_SURFACE ( 'NONE', #124266, 1249.999999999991587, 0.8960553845713407073 ) ;
#103446 = CARTESIAN_POINT ( 'NONE',  ( -0.6823417656250003738, -0.7197916663252492686, -1.181850606188749264 ) ) ;
#103445 = CARTESIAN_POINT ( 'NONE',  ( 1.646416196899816997, 0.7239943723881783200, 2.175097950400638691 ) ) ;
#103447 = CARTESIAN_POINT ( 'NONE',  ( 5.196852952739813070, 4.957416621151553571, -0.7998128361456221525 ) ) ;
#103448 = CARTESIAN_POINT ( 'NONE',  ( 4.496500501226593727, 8.397667684739696270, 0.7998128361456462443 ) ) ;
#103449 = CARTESIAN_POINT ( 'NONE',  ( 3.633611385093922674, -0.1624337102359394436, 2.215399726503309630 ) ) ;
#103450 = CARTESIAN_POINT ( 'NONE',  ( -7.375272376154081932, 10.58793962461302485, -1.082531754730543971 ) ) ;
#103451 = CARTESIAN_POINT ( 'NONE',  ( 0.000000000000000000, 18.91999999999999815, 0.000000000000000000 ) ) ;
#103452 = CARTESIAN_POINT ( 'NONE',  ( 6.344852701515477200, 6.504675694630598137, -0.7216878364870257245 ) ) ;
#103453 = CARTESIAN_POINT ( 'NONE',  ( -8.812436658758329600, 9.383523644747281622, 1.040834085586084257E-14 ) ) ;
#103454 = CARTESIAN_POINT ( 'NONE',  ( 6.075462232699553766, 6.260663157670496304, -0.7216878364870458196 ) ) ;
#103455 = CARTESIAN_POINT ( 'NONE',  ( 2.092422861153935276, -0.4390285686692517175, 1.967888031366466395 ) ) ;
#103457 = CARTESIAN_POINT ( 'NONE',  ( 6.707491137888100141, -1.654371308887558234, -1.231747576844913539 ) ) ;
#103456 = CARTESIAN_POINT ( 'NONE',  ( 9.237182729612253951, 9.671134694169463586, 0.7998128361456462443 ) ) ;
#103458 = FACE_OUTER_BOUND ( 'NONE', #193774, .T. ) ;
#103459 = CARTESIAN_POINT ( 'NONE',  ( 7.160114521348466710, 7.526090827760914870, 0.000000000000000000 ) ) ;
#103460 = CARTESIAN_POINT ( 'NONE',  ( 6.427322163675834865, -1.144589508088897478, -1.311236935029986173 ) ) ;
#103461 = PLANE ( 'NONE',  #195827 ) ;
#103462 = CARTESIAN_POINT ( 'NONE',  ( -1.402160292154681736E-14, 2.446875000341416584, -1.575800808251660134 ) ) ;
#103463 = CARTESIAN_POINT ( 'NONE',  ( 2.881836681058600913, -0.9132262334808398663, 1.515770159524139515 ) ) ;
#103464 = CARTESIAN_POINT ( 'NONE',  ( 1.108046318188542489, -0.04667474159409169127, 2.016033875899234662 ) ) ;
#103465 = CARTESIAN_POINT ( 'NONE',  ( 6.614805129994690169, -0.1227637983064084892, 1.711830280531308812 ) ) ;
#103466 = CARTESIAN_POINT ( 'NONE',  ( 5.548434679399758984, -1.809038938731177160, 1.407827746306972827 ) ) ;
#103467 = CARTESIAN_POINT ( 'NONE',  ( 2.906014618889842360, 1.333239036598636407, -1.269987479889053139 ) ) ;
#103468 = CARTESIAN_POINT ( 'NONE',  ( 6.936968151686458306, 11.24487994360957188, 0.7998128361456462443 ) ) ;
#103469 = CARTESIAN_POINT ( 'NONE',  ( 3.610199614654508338, -0.7391254383575728282, -1.669438027971142047 ) ) ;
#103470 = CARTESIAN_POINT ( 'NONE',  ( 5.063125043234593115, -1.117834493326537393, 1.678003986596336761 ) ) ;
#103471 = CARTESIAN_POINT ( 'NONE',  ( -8.208571938070008400, 11.66408546346865016, -1.199719254218446718 ) ) ;
#103473 = CARTESIAN_POINT ( 'NONE',  ( -6.770317605177755382, 8.992066187497757213, 1.599625672291269396 ) ) ;
#103472 = CARTESIAN_POINT ( 'NONE',  ( 3.028476438156304962, 1.258033425225786983, -1.880328901638250505 ) ) ;
#103474 = CARTESIAN_POINT ( 'NONE',  ( -0.01685825368398767912, -0.1589125243241385210, -2.071875930555002743 ) ) ;
#103475 = DIRECTION ( 'NONE',  ( 0.9885327375000381167, 0.000000000000000000, 0.1510067114093955609 ) ) ;
#103476 = CARTESIAN_POINT ( 'NONE',  ( 4.035645461687249913, 1.950487776689105557, -0.6946759356915442885 ) ) ;
#103477 = CARTESIAN_POINT ( 'NONE',  ( 4.539282502477016479, 4.190251095844947926, 0.7998128361456341429 ) ) ;
#103478 = CARTESIAN_POINT ( 'NONE',  ( 1.360316468750005559, 1.567708333674729282, -0.7853790794158981292 ) ) ;
#103479 = CARTESIAN_POINT ( 'NONE',  ( 6.270199134133584096, 2.114857618286110075, -0.1555134818699495936 ) ) ;
#103480 = APPLICATION_PROTOCOL_DEFINITION ( 'draft international standard', 'automotive_design', 1998, #119687 ) ;
#103483 = EDGE_CURVE ( 'NONE', #124391, #65269, #187731, .T. ) ;
#103482 = CARTESIAN_POINT ( 'NONE',  ( 2.086434564137104264, -1.889293373815591481, -0.3759864732829041878 ) ) ;
#103481 = CARTESIAN_POINT ( 'NONE',  ( -10.01677656239806247, 10.58066083241955901, 0.7998128361456462443 ) ) ;
#103484 = UNCERTAINTY_MEASURE_WITH_UNIT (LENGTH_MEASURE( 1.000000000000000082E-05 ), #172642, 'distance_accuracy_value', 'NONE');
#103485 = CARTESIAN_POINT ( 'NONE',  ( -4.004454267989906668, 5.765225627445230927, 1.599625672291270506 ) ) ;
#103486 = CARTESIAN_POINT ( 'NONE',  ( 0.4847283499135228713, 1.883623918205453718, 0.5753430019505183513 ) ) ;
#103487 = CARTESIAN_POINT ( 'NONE',  ( 4.380693030546916944, 6.204170850428461392, 1.443375672974058777 ) ) ;
#103488 = CARTESIAN_POINT ( 'NONE',  ( 5.616475580598488726, 6.148514233939430973, 0.8375902553012237739 ) ) ;
#103489 = CARTESIAN_POINT ( 'NONE',  ( -1.115562610750309283E-14, 11.09375000068279427, 1.500000000000001554 ) ) ;
#103490 = CARTESIAN_POINT ( 'NONE',  ( -3.415764635639130020, 6.072476943965863683, 1.199719254218462483 ) ) ;
#103491 = CARTESIAN_POINT ( 'NONE',  ( 0.1236698368150884464, 1.936885272324913698, 1.087587522935773876 ) ) ;
#103492 = CARTESIAN_POINT ( 'NONE',  ( 3.575310672209235374, 0.05349853608750848588, -2.105455972502618955 ) ) ;
#103493 = CARTESIAN_POINT ( 'NONE',  ( -5.327428015527048366, 5.180030537728460338, -0.7998128361456362523 ) ) ;
#103494 = CARTESIAN_POINT ( 'NONE',  ( 6.612626235163189925, 8.737816579155630592, -1.599625672291262513 ) ) ;
#103495 = CARTESIAN_POINT ( 'NONE',  ( 0.7657746542184565852, -1.852627923093919771, 0.1767624929009704582 ) ) ;
#103496 = CARTESIAN_POINT ( 'NONE',  ( 5.113396490648394632, 9.117379672398465473, 1.040834085586084257E-14 ) ) ;
#103497 = CARTESIAN_POINT ( 'NONE',  ( 3.825371897350130723, 7.614684313550482031, 0.7998128361456321445 ) ) ;
#103498 = CARTESIAN_POINT ( 'NONE',  ( -7.444835747679825033, 7.858265591814152629, 0.000000000000000000 ) ) ;
#103499 = CARTESIAN_POINT ( 'NONE',  ( -8.080296364064746939, 9.489729181906076505, 1.082531754730558626 ) ) ;
#103501 = CARTESIAN_POINT ( 'NONE',  ( 1.512141599020993432, -0.7094941370262074498, 1.998545949238240027 ) ) ;
#103500 = AXIS2_PLACEMENT_3D ( 'NONE', #117090, #100771, #69315 ) ;
#103502 = CARTESIAN_POINT ( 'NONE',  ( -5.413448473606448985, 9.537716662508005427, 0.000000000000000000 ) ) ;
#103504 = CARTESIAN_POINT ( 'NONE',  ( 4.580490334204036174, 1.208584658811951762, -1.545285769342201965 ) ) ;
#103503 = CARTESIAN_POINT ( 'NONE',  ( 0.6124999999999880540, 0.1666666666666899443, -1.060881119635979530 ) ) ;
#103505 = CARTESIAN_POINT ( 'NONE',  ( 1.815512348505427642, -0.2646426633909418347, 2.145385951886819242 ) ) ;
#103506 = CARTESIAN_POINT ( 'NONE',  ( 1.821575194732877545, 1.059174331173462935, -1.505913648122420900 ) ) ;
#103507 = B_SPLINE_CURVE_WITH_KNOTS ( 'NONE', 3,
 ( #24631, #143783, #142704, #11589, #77662, #90738 ),
 .UNSPECIFIED., .F., .F.,
 ( 4, 2, 4 ),
 ( 0.000000000000000000, 0.3573083853819281064, 0.7146167707638562128 ),
 .UNSPECIFIED. ) ;
#103509 = CARTESIAN_POINT ( 'NONE',  ( -5.725072791067139732, 6.113630025739863250, -0.7036897515925732982 ) ) ;
#103508 = CARTESIAN_POINT ( 'NONE',  ( -2.959422669532919326, 6.674686557755516780, 0.7998128361456352531 ) ) ;
#103510 = CARTESIAN_POINT ( 'NONE',  ( 3.275097224137039742, 1.105054647683247460, 1.344453793780414186 ) ) ;
#103511 = CARTESIAN_POINT ( 'NONE',  ( 4.040494898817784453, 7.752230779688214390, 0.4466632393476636098 ) ) ;
#103512 = CARTESIAN_POINT ( 'NONE',  ( 4.351804120306567825, 8.020929207092235558, 1.040834085586084257E-14 ) ) ;
#103513 = CARTESIAN_POINT ( 'NONE',  ( -11.69243366784185945, 8.407932920124673970, 1.097391832464843286 ) ) ;
#103514 = CARTESIAN_POINT ( 'NONE',  ( 0.4093245661422850734, 1.881582470445356314, 1.064130679222355491 ) ) ;
#103515 = CARTESIAN_POINT ( 'NONE',  ( 2.864611068004913275, -0.6351033500862738324, 1.913510180259501592 ) ) ;
#103516 = CARTESIAN_POINT ( 'NONE',  ( -9.829298179783291900, 11.53023130024440768, 1.082531754730558626 ) ) ;
#103517 = CARTESIAN_POINT ( 'NONE',  ( 0.3214396764580421118, -0.1044536432763705502, 2.159311484102262479 ) ) ;
#103518 = EDGE_CURVE ( 'NONE', #51765, #191668, #96164, .T. ) ;
#103519 = CARTESIAN_POINT ( 'NONE',  ( 3.274254179156810274, -1.175395456433829144, 1.582609504276990320 ) ) ;
#103520 = CARTESIAN_POINT ( 'NONE',  ( -1.499999999999963141, 7.750000000000000000, -10.99818166789402518 ) ) ;
#103521 = CARTESIAN_POINT ( 'NONE',  ( 2.155715342533376155, 0.8324662149039625536, 1.754741561904197056 ) ) ;
#103523 = ORIENTED_EDGE ( 'NONE', *, *, #60102, .F. ) ;
#103522 = CARTESIAN_POINT ( 'NONE',  ( -2.862179826260718762, 6.353310540697199471, 0.000000000000000000 ) ) ;
#103524 = CARTESIAN_POINT ( 'NONE',  ( -5.790741006368224753, 5.928488393617260321, 0.7216878364870257245 ) ) ;
#103525 = CARTESIAN_POINT ( 'NONE',  ( -0.2106854629475270468, 2.024676876401194203, -2.413177685601196831 ) ) ;
#103526 = CARTESIAN_POINT ( 'NONE',  ( 4.736594563127852098, 6.619389305106191834, -1.599625672291273171 ) ) ;
#103527 = CARTESIAN_POINT ( 'NONE',  ( -5.492988512192097161, 6.437516681426083132, 1.199719254218452935 ) ) ;
#103529 = ORIENTED_EDGE ( 'NONE', *, *, #205827, .F. ) ;
#103528 = CARTESIAN_POINT ( 'NONE',  ( -6.444921918449773024, 8.612437886315108315, 1.599625672291269396 ) ) ;
#103530 = CARTESIAN_POINT ( 'NONE',  ( -1.382971907303421233, 4.316406942282006831, -0.2136448034514826788 ) ) ;
#103531 = CARTESIAN_POINT ( 'NONE',  ( 0.2533207856364183552, -1.770817270756098960, 1.316655756711228253 ) ) ;
#103532 = CARTESIAN_POINT ( 'NONE',  ( -9.963041989461812520, 4.512757371444226173, 6.615979002877482529 ) ) ;
#103533 = CARTESIAN_POINT ( 'NONE',  ( 4.487127722112081329, 0.09209952633786910869, 1.959694304038139379 ) ) ;
#103534 = CARTESIAN_POINT ( 'NONE',  ( 8.097244055859613709, 10.46987070330147063, -1.599625672291262513 ) ) ;
#103535 = CARTESIAN_POINT ( 'NONE',  ( 1.951796282902381163, -1.844710420878793444, -0.8146254186931353169 ) ) ;
#103536 = VERTEX_POINT ( 'NONE', #43089 ) ;
#103537 = CARTESIAN_POINT ( 'NONE',  ( 2.483745868283081748, -0.6592627125163934565, 2.012192174959149149 ) ) ;
#103538 = CARTESIAN_POINT ( 'NONE',  ( -1.402160292154681736E-14, 2.118750000682816825, -1.732050807568863648 ) ) ;
#103539 = CARTESIAN_POINT ( 'NONE',  ( -5.311043488251275591, 7.219303374425030562, -1.599625672291256295 ) ) ;
#103540 = CARTESIAN_POINT ( 'NONE',  ( 3.573999110145977820, -1.774750109099573869, -0.4897004633943187191 ) ) ;
#103541 = VERTEX_POINT ( 'NONE', #40945 ) ;
#103542 = CARTESIAN_POINT ( 'NONE',  ( -8.239604668803112375, 10.63595808506888396, -1.599625672291263179 ) ) ;
#103543 =( LENGTH_UNIT ( ) NAMED_UNIT ( * ) SI_UNIT ( .MILLI., .METRE. ) );
#103544 = CARTESIAN_POINT ( 'NONE',  ( 4.078469121099765005, 1.002472831208834680, 1.868716877859360137 ) ) ;
#103545 = DIRECTION ( 'NONE',  ( 0.9782075119096202975, 0.1245777785630026030, 0.1661037047506698505 ) ) ;
#103546 = CARTESIAN_POINT ( 'NONE',  ( 6.425674737872927089, 9.584038729905381970, -1.199719254218440723 ) ) ;
#103547 = CARTESIAN_POINT ( 'NONE',  ( 6.011025214932095295, 1.815421535059216662, 0.9752673143463059802 ) ) ;
#103548 = CIRCLE ( 'NONE', #51606, 0.7499999999999997780 ) ;
#103550 = CARTESIAN_POINT ( 'NONE',  ( 2.050122339901743196, -1.422379512129726908, 1.169167124061460949 ) ) ;
#103549 = CARTESIAN_POINT ( 'NONE',  ( -7.562750758324527922, 7.717630727667075696, 1.040834085586084257E-14 ) ) ;
#103551 = CARTESIAN_POINT ( 'NONE',  ( 8.452618703115982512, 11.94880668935564216, 1.199719254218450271 ) ) ;
#103552 = CARTESIAN_POINT ( 'NONE',  ( -0.6823417656249969321, 5.467708333674756283, -1.181850606188749264 ) ) ;
#103553 = SURFACE_STYLE_FILL_AREA ( #37475 ) ;
#103554 = CARTESIAN_POINT ( 'NONE',  ( -7.608060475923978494, 8.905100639113307182, 1.199719254218452047 ) ) ;
#103555 = CARTESIAN_POINT ( 'NONE',  ( 0.000000000000000000, 13.49999999999999822, 0.000000000000000000 ) ) ;
#103556 = CARTESIAN_POINT ( 'NONE',  ( 2.262606014870732096, 0.9450075053254001212, 1.994452002680577429 ) ) ;
#103557 = CARTESIAN_POINT ( 'NONE',  ( 3.761208288054026738, -1.993080904335465142, -1.070619287061522318 ) ) ;
#103558 = CARTESIAN_POINT ( 'NONE',  ( -8.527715433315703919, 9.051348881730875817, 1.040834085586084257E-14 ) ) ;
#103559 = CARTESIAN_POINT ( 'NONE',  ( 3.673895663291579350, 1.797233291820631962, -0.2271657407440821064 ) ) ;
#103560 = CARTESIAN_POINT ( 'NONE',  ( 4.610495038435900916, 1.835019742331613690, 0.5502660077172877306 ) ) ;
#103561 = CARTESIAN_POINT ( 'NONE',  ( 1.364683531249990311, 4.446875000341417028, 1.214306433183764966E-14 ) ) ;
#103562 = CARTESIAN_POINT ( 'NONE',  ( 4.100430126988792168, -0.6171887515804741486, -1.872443122656509029 ) ) ;
#103563 = CARTESIAN_POINT ( 'NONE',  ( 1.325083149161108365, -0.05013198271685941065, 1.925904219417676089 ) ) ;
#103564 = CARTESIAN_POINT ( 'NONE',  ( 5.436355746168001879, 1.843147576875401983, 0.3187000444574567548 ) ) ;
#103565 = AXIS2_PLACEMENT_3D ( 'NONE', #192355, #12541, #44012 ) ;
#103566 = CARTESIAN_POINT ( 'NONE',  ( 3.246982502279437188, 0.5605648102574630753, 2.238460633888791573 ) ) ;
#103567 = CARTESIAN_POINT ( 'NONE',  ( 4.457361271359429722, 1.493968932455931542, 1.109517434556703597 ) ) ;
#103568 = CARTESIAN_POINT ( 'NONE',  ( 4.517335436343476118, 8.499999999999996447, -0.7749999999999996891 ) ) ;
#103569 = CARTESIAN_POINT ( 'NONE',  ( 0.3390778084843976137, -1.706115258973059490, -1.074657883261991076 ) ) ;
#103570 =( BOUNDED_CURVE ( )  B_SPLINE_CURVE ( 2, ( #201704, #53348, #147667, #39233, #139964, #189740, #4560, #138887, #123780 ),
 .UNSPECIFIED., .F., .T. ) 
 B_SPLINE_CURVE_WITH_KNOTS ( ( 3, 2, 2, 2, 3 ),
 ( 0.6406250000000002220, 0.6458333333333333703, 0.6562500000000000000, 0.6666666666666666297, 0.6718749999999998890 ),
 .UNSPECIFIED. ) 
 CURVE ( )  GEOMETRIC_REPRESENTATION_ITEM ( )  RATIONAL_B_SPLINE_CURVE ( ( 0.9330127018922194093, 0.9330127018922221849, 1.000000000000000000, 0.8660254037844387076, 1.000000000000000000, 0.8660254037844387076, 1.000000000000000000, 0.9330127018922207416, 0.9330127018922192983 ) ) 
 REPRESENTATION_ITEM ( '' )  );
#103572 = CARTESIAN_POINT ( 'NONE',  ( 1.770285920821415449, 1.083698108115097591, 1.805711900068427411 ) ) ;
#103571 = CARTESIAN_POINT ( 'NONE',  ( -3.592547517496935683, 6.174760622846296343, -1.082531754730548412 ) ) ;
#103573 = CARTESIAN_POINT ( 'NONE',  ( 4.324687812634892659, 5.108185871904570519, 1.082531754730560403 ) ) ;
#103575 = DIRECTION ( 'NONE',  ( -5.578564026256490882E-16, -1.000000000000000000, -9.066213480720158442E-32 ) ) ;
#103574 = CARTESIAN_POINT ( 'NONE',  ( 0.6823417656249899377, 4.738541667008086655, -1.181850606188754593 ) ) ;
#103576 = CARTESIAN_POINT ( 'NONE',  ( 2.760144723603759065, 0.7592700852765141839, -1.980205354017528840 ) ) ;
#103577 = CARTESIAN_POINT ( 'NONE',  ( -6.966220764712148572, 6.002124920821316323, 2.420000000000000373 ) ) ;
#103578 = CARTESIAN_POINT ( 'NONE',  ( 0.6682303662221461549, 2.017294962401328107, -0.1032846847020176678 ) ) ;
#103579 = CARTESIAN_POINT ( 'NONE',  ( -1.402160292154681736E-14, 0.6968750003414164729, -1.575800808251659024 ) ) ;
#103580 = CARTESIAN_POINT ( 'NONE',  ( -2.318081078256692518, 5.648252324700675508, 1.040834085586084257E-14 ) ) ;
#103581 = CARTESIAN_POINT ( 'NONE',  ( 4.462605117192430804, 8.358123070033169455, 1.040834085586084257E-14 ) ) ;
#103582 = ORIENTED_EDGE ( 'NONE', *, *, #17999, .F. ) ;
#103583 = CARTESIAN_POINT ( 'NONE',  ( 2.354944161360218224, -1.672559397656541824, 1.369352967626968898 ) ) ;
#103584 = CARTESIAN_POINT ( 'NONE',  ( 3.863710590214593399, 7.451486755318259547, 1.040834085586084257E-14 ) ) ;
#103587 = CARTESIAN_POINT ( 'NONE',  ( 2.223174002961016082, 5.537527403522402025, -0.7216878364870267237 ) ) ;
#103586 = CARTESIAN_POINT ( 'NONE',  ( 6.400857919427532572, 6.640291458853147866, -0.7216878364870458196 ) ) ;
#103585 = CARTESIAN_POINT ( 'NONE',  ( 3.711900195091365262, 7.552577004240394132, -0.7998128361456362523 ) ) ;
#103588 = CARTESIAN_POINT ( 'NONE',  ( 10.52076401408022299, 11.37657222595619189, 0.000000000000000000 ) ) ;
#103589 = CARTESIAN_POINT ( 'NONE',  ( 5.770720322323381168, -0.3006437417610394736, -1.993894057904864514 ) ) ;
#103590 = CARTESIAN_POINT ( 'NONE',  ( -7.510853912290736289, 11.70648729774046792, 0.7216878364870458196 ) ) ;
#103591 = CARTESIAN_POINT ( 'NONE',  ( 0.1346727191937693857, 0.3808678606769915209, 2.158067550307264604 ) ) ;
#103592 = CARTESIAN_POINT ( 'NONE',  ( 2.725000000000005862, 0.000000000000000000, 0.000000000000000000 ) ) ;
#103594 = CARTESIAN_POINT ( 'NONE',  ( -1.364683531250000748, 11.60937500034139802, 0.000000000000000000 ) ) ;
#103593 = CARTESIAN_POINT ( 'NONE',  ( 0.3919815047150644327, 1.678997099660347603, 1.516718289441946199 ) ) ;
#103595 = CARTESIAN_POINT ( 'NONE',  ( -9.806625181386236179, 10.33548422123910449, -0.7998128361456291469 ) ) ;
#103596 = CARTESIAN_POINT ( 'NONE',  ( -4.243338890952904841, 5.973648010910253880, -1.443375672974051449 ) ) ;
#103597 = CARTESIAN_POINT ( 'NONE',  ( -0.6823417656250212460, 2.113541667008083991, 1.181850606188767472 ) ) ;
#103598 = CARTESIAN_POINT ( 'NONE',  ( -1.402160292154681736E-14, 10.31250000000000178, 1.732050807568881190 ) ) ;
#103599 = CARTESIAN_POINT ( 'NONE',  ( 4.037519343584392573, -1.191552764850771995, -1.247402213628981293 ) ) ;
#103600 = CARTESIAN_POINT ( 'NONE',  ( 4.960304097753311936, 6.880383762169266504, 1.599625672291268286 ) ) ;
#103601 =( BOUNDED_SURFACE ( )  B_SPLINE_SURFACE ( 3, 3, ( 
 ( #96084, #32126, #115560, #14786, #146967, #145911, #178388, #181556, #99266, #179452, #128650 ),
 ( #165314, #162138, #182619, #149064, #80877, #132851, #31075, #116625, #150148, #64622, #97149 ),
 ( #1718, #39579, #4905, #68853, #21161, #87265, #101377, #38517, #120912, #168511, #67775 ),
 ( #153331, #5982, #121985, #151212, #2782, #36368, #152269, #154404, #186885, #187951, #51577 ),
 ( #20111, #55829, #105681, #134973, #104595, #185810, #72053, #117702, #102445, #170641, #23307 ),
 ( #138165, #70982, #52628, #183693, #118756, #204172, #200981, #171710, #86197, #136025, #167452 ),
 ( #137095, #3841, #69914, #202038, #169578, #89418, #22226, #203121, #37442, #155467, #35300 ) ),
 .UNSPECIFIED., .T., .F., .T. ) 
 B_SPLINE_SURFACE_WITH_KNOTS ( ( 4, 3, 4 ),
 ( 4, 1, 1, 1, 1, 1, 1, 1, 4 ),
 ( 0.000000000000000000, 0.5000000000000000000, 1.000000000000000000 ),
 ( 0.000000000000000000, 0.2256085737580844630, 0.3975982043691296264, 0.5251069566405043298, 0.6172860083021659561, 0.6832860984239963464, 0.7321959383537668398, 0.7728624839797392232, 1.000000000000000000 ),
 .UNSPECIFIED. ) 
 GEOMETRIC_REPRESENTATION_ITEM ( )  RATIONAL_B_SPLINE_SURFACE ( (
 ( 1.000000000000000222, 1.000000000000000222, 1.000000000000000444, 0.9999999999999996669, 1.000000000000000444, 0.9999999999999997780, 1.000000000000000222, 1.000000000000000222, 0.9999999999999996669, 1.000000000000000000, 1.000000000000000000),
 ( 0.3333333333333334259, 0.3333333333333334259, 0.3333333333333334259, 0.3333333333333333703, 0.3333333333333334259, 0.3333333333333333148, 0.3333333333333334814, 0.3333333333333334259, 0.3333333333333331483, 0.3333333333333334259, 0.3333333333333333703),
 ( 0.3333333333333334259, 0.3333333333333334259, 0.3333333333333334259, 0.3333333333333333703, 0.3333333333333334259, 0.3333333333333333148, 0.3333333333333334814, 0.3333333333333334259, 0.3333333333333331483, 0.3333333333333334259, 0.3333333333333333703),
 ( 1.000000000000000222, 1.000000000000000222, 1.000000000000000444, 0.9999999999999996669, 1.000000000000000444, 0.9999999999999997780, 1.000000000000000222, 1.000000000000000222, 0.9999999999999996669, 1.000000000000000000, 1.000000000000000000),
 ( 0.3333333333333334259, 0.3333333333333334259, 0.3333333333333334259, 0.3333333333333333703, 0.3333333333333334259, 0.3333333333333333148, 0.3333333333333334814, 0.3333333333333334259, 0.3333333333333331483, 0.3333333333333334259, 0.3333333333333333703),
 ( 0.3333333333333334259, 0.3333333333333334259, 0.3333333333333334259, 0.3333333333333333703, 0.3333333333333334259, 0.3333333333333333148, 0.3333333333333334814, 0.3333333333333334259, 0.3333333333333331483, 0.3333333333333334259, 0.3333333333333333703),
 ( 1.000000000000000222, 1.000000000000000222, 1.000000000000000444, 0.9999999999999996669, 1.000000000000000444, 0.9999999999999997780, 1.000000000000000222, 1.000000000000000222, 0.9999999999999996669, 1.000000000000000000, 1.000000000000000000) ) ) 
 REPRESENTATION_ITEM ( '' )  SURFACE ( )  );
#103602 = CARTESIAN_POINT ( 'NONE',  ( 2.073191327021279839, 1.695144128639828551, -0.5084401619379045334 ) ) ;
#103603 = CARTESIAN_POINT ( 'NONE',  ( 2.684242053459008570, 1.078846248543659403, 1.699430804756915547 ) ) ;
#103604 = CARTESIAN_POINT ( 'NONE',  ( 10.42352117080803708, 11.05519620889787724, -0.7998128361456281477 ) ) ;
#103605 = CARTESIAN_POINT ( 'NONE',  ( 4.770673279661371780, -1.444480529215144804, 1.668407551275403300 ) ) ;
#103606 = EDGE_LOOP ( 'NONE', ( #178251, #152903, #9508, #8555 ) ) ;
#103607 = CARTESIAN_POINT ( 'NONE',  ( 4.623309962349557267, 1.759429041943610716, 0.9917458525283324722 ) ) ;
#103608 = CARTESIAN_POINT ( 'NONE',  ( -7.273023059088104425, 7.449891421883056530, 0.000000000000000000 ) ) ;
#103610 = CARTESIAN_POINT ( 'NONE',  ( 4.253529916566947122, 1.955168710539030075, -0.4926619687581067497 ) ) ;
#103609 = CARTESIAN_POINT ( 'NONE',  ( 4.442108405842562391, -1.305342523080333272, -1.670987904322115636 ) ) ;
#103612 = ORIENTED_EDGE ( 'NONE', *, *, #205827, .T. ) ;
#103611 = CARTESIAN_POINT ( 'NONE',  ( 4.324329094900294379, -0.7804802743817635946, -1.635003121989448971 ) ) ;
#103613 = CARTESIAN_POINT ( 'NONE',  ( 3.250922972226694352, 7.014770244231638863, 0.7998128361456281477 ) ) ;
#103614 = ORIENTED_EDGE ( 'NONE', *, *, #124593, .T. ) ;
#103616 = ADVANCED_FACE ( 'NONE', ( #39869 ), #141025, .T. ) ;
#103615 = CIRCLE ( 'NONE', #107078, 1.224999999999996980 ) ;
#103617 = CARTESIAN_POINT ( 'NONE',  ( 0.9888773766892228201, 1.651582696977690112, -0.8784067438419728147 ) ) ;
#103618 = CARTESIAN_POINT ( 'NONE',  ( 3.701970883082863040, 7.364863713882357388, -2.499999999999995115 ) ) ;
#103619 = CARTESIAN_POINT ( 'NONE',  ( 5.865820270629499511, 0.5193939906856791522, -1.735422816724658146 ) ) ;
#103620 = DIRECTION ( 'NONE',  ( -1.000000000000000000, 5.578564026256503701E-16, 1.479114197289397135E-31 ) ) ;
#103621 = CARTESIAN_POINT ( 'NONE',  ( -9.979907920417568690, 3.147823346236176878, -6.101210848797135711 ) ) ;
#103622 = SURFACE_STYLE_USAGE ( .BOTH. , #202141 ) ;
#103623 = EDGE_CURVE ( 'NONE', #21223, #51705, #139720, .T. ) ;
#103624 = CARTESIAN_POINT ( 'NONE',  ( -1.201851678989727383E-14, 3.634375000341422357, 1.575800808251672791 ) ) ;
#103625 = PLANE ( 'NONE',  #148256 ) ;
#103626 = CARTESIAN_POINT ( 'NONE',  ( 6.536439455564168277, 6.798469917679251573, 0.7216878364870328300 ) ) ;
#103627 = CARTESIAN_POINT ( 'NONE',  ( 1.803102349535959714, -1.659081995624330563, 1.046767247423967095 ) ) ;
#103628 = CARTESIAN_POINT ( 'NONE',  ( -3.526529353330350336, 7.128384988945109413, -0.7216878364870458196 ) ) ;
#103629 = CARTESIAN_POINT ( 'NONE',  ( -6.771371375382467583, 6.864631124226471037, -0.7998128361456362523 ) ) ;
#103630 = CARTESIAN_POINT ( 'NONE',  ( 3.709332143218791789, 1.789599998243587731, -1.137392358348317201 ) ) ;
#103632 = CARTESIAN_POINT ( 'NONE',  ( 11.07790593930098311, 9.799999999999998934, -0.7000000000000009548 ) ) ;
#103631 = CARTESIAN_POINT ( 'NONE',  ( 9.772729797352075920, 10.29593960653257234, -0.7998128361456281477 ) ) ;
#103633 = CARTESIAN_POINT ( 'NONE',  ( 5.009034487593355678, 1.713717141372484765, 0.9743026824079579207 ) ) ;
#103634 = CARTESIAN_POINT ( 'NONE',  ( -0.6823417656250003738, 1.467708333674752730, -1.181850606188749264 ) ) ;
#103635 = CARTESIAN_POINT ( 'NONE',  ( 1.213140692357208117, 1.643459361250454442, -1.162501220127802437 ) ) ;
#103636 = ORIENTED_EDGE ( 'NONE', *, *, #207633, .T. ) ;
#103637 = CARTESIAN_POINT ( 'NONE',  ( 0.8611331728165865229, -0.05642918589183294059, -2.116647836221299261 ) ) ;
#103638 = CARTESIAN_POINT ( 'NONE',  ( 11.95123587697795564, 6.644955863035443500, -0.4920656033008508623 ) ) ;
#103639 = CARTESIAN_POINT ( 'NONE',  ( 2.647004975520852454, -0.3514972095969396970, -2.040143077068845123 ) ) ;
#103640 = ORIENTED_EDGE ( 'NONE', *, *, #203982, .F. ) ;
#103641 = CARTESIAN_POINT ( 'NONE',  ( 5.713835393516482952, 5.630839145382857680, 0.7998128361456352531 ) ) ;
#103642 = CARTESIAN_POINT ( 'NONE',  ( 6.873057527484919937, 6.983264968346048818, 0.7998128361456352531 ) ) ;
#103643 = ORIENTED_EDGE ( 'NONE', *, *, #99125, .T. ) ;
#103645 = CARTESIAN_POINT ( 'NONE',  ( 3.818592820543298405, 7.606775390609172405, -0.7998128361456221525 ) ) ;
#103644 = CARTESIAN_POINT ( 'NONE',  ( 5.138659532522440010, -1.793477146331866612, 1.074093663348500760 ) ) ;
#103648 = EDGE_LOOP ( 'NONE', ( #191698, #86737, #29677, #104129 ) ) ;
#103647 = CARTESIAN_POINT ( 'NONE',  ( 2.086290463123147365, -1.113812826415590651, 1.428500571052490953 ) ) ;
#103646 = CARTESIAN_POINT ( 'NONE',  ( 3.258640109524315154, -1.383274205585843797, 1.191454006006509303 ) ) ;
#103649 = B_SPLINE_CURVE_WITH_KNOTS ( 'NONE', 3,
 ( #143040, #157131, #139824, #207981, #9788, #140906, #159240 ),
 .UNSPECIFIED., .F., .F.,
 ( 4, 3, 4 ),
 ( 0.000000000000000000, 0.0008000000000004422844, 0.002977368225425622381 ),
 .UNSPECIFIED. ) ;
#103650 = CARTESIAN_POINT ( 'NONE',  ( 6.393228082638676923, 1.922373441260841087, -1.083778638264052852 ) ) ;
#103651 = DIRECTION ( 'NONE',  ( 0.7366372490352351976, 0.000000000000000000, -0.6762880771785058087 ) ) ;
#103652 = CARTESIAN_POINT ( 'NONE',  ( 4.401547605996741552, 1.770323140634282311, 1.317293360403009927 ) ) ;
#103653 = CARTESIAN_POINT ( 'NONE',  ( 1.364683531249996529, 9.276041667008062319, 0.7879004041258403923 ) ) ;
#103654 = ORIENTED_EDGE ( 'NONE', *, *, #43529, .F. ) ;
#103655 = CARTESIAN_POINT ( 'NONE',  ( 3.668532269402470458, 0.6909111621477401766, 1.783275653667259597 ) ) ;
#103656 = CARTESIAN_POINT ( 'NONE',  ( -3.785751206713858785, 5.439795712631356750, 1.599625672291267398 ) ) ;
#103657 =( BOUNDED_SURFACE ( )  B_SPLINE_SURFACE ( 1, 2, ( 
 ( #38485, #20076, #202005, #150112, #138131, #170607, #37409, #1685, #199895, #103485, #117666, #87231, #3807, #204140, #121950, #51542, #183659, #35263, #134940, #23273, #124096, #190060, #172767, #159705, #208432, #43847, #155433, #141368, #89384, #24340, #76318, #9183, #74195, #139195, #75254, #140289, #173847, #60066, #90450, #123042, #109961, #156516, #41712, #7018, #73094, #206308, #77382, #40636, #59001, #209494, #205225, #107822, #106738, #188993, #56866, #158644, #25423, #207380, #193267, #175971, #92601, #191116, #44913, #171676, #125157, #8107, #42782, #91530, #108891, #174914, #57932, #157588, #27565, #26494, #10242, #142423, #126222, #192183, #11304, #93663, #143499, #61135, #127297, #177026, #178100, #15560, #162918, #148786, #97927, #29717, #82707, #112098, #14498, #65372, #197522, #163985, #28643, #12369, #131519, #78449, #49166, #179165, #95799, #47044, #115284, #129431, #45977, #81647, #113161, #80590, #48118, #111021, #62211, #30789, #147734, #146686, #128368, #144567, #114230, #212702, #96868, #64343, #130488, #181275, #31851, #161855, #32901, #98979, #63270, #165032, #180228, #194335, #210580, #13444, #79521, #145639, #196476, #356, #211634, #16625, #195415, #213749, #66429, #132572, #94730, #160776, #198574, #117414, #183410, #100036, #71770, #134698, #67499, #69638, #51289, #35014, #200703, #116341, #37160, #20882, #166098, #199643, #185532, #101085, #149865, #167174, #36084, #2497, #102167, #86981, #53409, #153051, #70697, #184466, #202838, #52354, #5693, #136811, #1433, #3565, #18761, #84846, #54486, #118481, #120631, #168235, #103238, #137886, #19834, #50221, #4626, #150936, #21942, #38235, #186608, #133642, #201769, #182332, #119547, #85918, #88052, #17686, #154123, #83772, #68571, #151991, #169298, #135746, #33960, #104309, #170357, #208183, #175713, #41460, #89138, #172514, #140030, #190867, #159447, #204975, #76067, #157334, #173603, #171433, #188745, #56621, #25175, #125970, #58751, #138955, #121707, #122785, #72849, #207126, #40384, #203906, #27304, #57690, #124904, #75006, #174662 ),
 ( #108635, #107568, #93410, #42531, #106487, #11045, #24100, #91277, #158392, #142166, #26237, #187670, #105393, #9989, #23021, #59815, #123847, #90203, #206055, #191926, #7849, #156267, #92354, #189808, #8925, #141115, #55553, #155192, #43591, #109709, #77124, #6773, #73936, #39300, #30532, #145385, #96612, #211383, #97671, #210318, #94476, #81397, #128113, #95549, #127040, #193000, #177847, #48909, #12120, #162666, #181027, #209236, #13190, #78194, #160517, #28382, #130230, #79268, #46792, #164781, #147481, #64087, #14235, #16372, #143247, #112906, #144320, #178917, #161601, #80330, #146431, #110767, #111843, #213501, #60881, #44653, #63010, #129180, #61954, #131281, #179974, #15309, #176766, #212445, #194071, #45724, #47866, #195158, #32645, #196224, #29460, #115029, #113977, #31595, #163728, #65124, #197269, #98722, #198325, #36900, #49965, #169040, #150682, #83517, #18516, #102982, #100837, #17434, #135492, #84594, #134451, #19585, #82450, #33706, #2243, #119291, #118227, #99783, #116083, #85657, #184213, #68320, #35836, #200454, #20637, #3314, #67248, #86726, #152795, #34763, #4375, #151744, #165848, #182074, #133383, #149598, #1184, #52100, #120373, #199388, #70446, #166922, #117157, #69384, #51034, #148540, #66173, #101914, #183160, #167979, #132319, #104056, #201514, #53162, #185277, #136562, #202583, #54235, #107, #186348, #37983, #170102, #203649, #73674, #138697, #23844, #124652, #157079, #75810, #74749, #206864, #109454, #153872, #172257, #71520, #189555, #8668, #57430, #56364, #92088, #191671, #87798, #123591, #122527, #106231, #171175, #91017, #204715, #188490, #140852, #41202, #43335, #72596, #40120, #139773, #58496, #24911, #107309, #39050, #108380, #22765, #89952, #173333, #156002, #190609, #21688, #174403, #42267, #25981, #158144, #9735, #7589, #141918, #137632, #88882, #207930, #154935, #121450, #6520, #205799, #59552, #125711, #5441, #55300, #187419, #105135, #95290, #113719, #45462, #131031, #47605, #126782, #128908, #11862, #28127, #195971, #29201, #179723, #161339, #13987, #197021 ) ),
 .UNSPECIFIED., .F., .F., .T. ) 
 B_SPLINE_SURFACE_WITH_KNOTS ( ( 2, 2 ),
 ( 3, 2, 2, 2, 2, 2, 2, 2, 2, 2, 2, 2, 2, 2, 2, 2, 2, 2, 2, 2, 2, 2, 2, 2, 2, 2, 2, 2, 2, 2, 2, 2, 2, 2, 2, 2, 2, 2, 2, 2, 2, 2, 2, 2, 2, 2, 2, 2, 2, 2, 2, 2, 2, 2, 2, 2, 2, 2, 2, 2, 2, 2, 2, 2, 2, 2, 2, 2, 2, 2, 2, 2, 2, 2, 2, 2, 2, 2, 2, 2, 2, 2, 2, 2, 2, 2, 2, 2, 2, 2, 2, 2, 2, 2, 2, 2, 2, 2, 2, 2, 2, 2, 2, 2, 2, 2, 2, 2, 2, 2, 2, 2, 2, 2, 2, 2, 2, 2, 2, 2, 3 ),
 ( 0.000000000000000000, 1.000000000000000000 ),
 ( 0.000000000000000000, 0.008333333333333333218, 0.01666666666666666644, 0.02500000000000000139, 0.03333333333333333287, 0.04166666666666666435, 0.05000000000000000278, 0.05833333333333333426, 0.06666666666666666574, 0.07499999999999999722, 0.08333333333333332871, 0.09166666666666666019, 0.1000000000000000056, 0.1083333333333333370, 0.1166666666666666685, 0.1250000000000000000, 0.1333333333333333315, 0.1416666666666666630, 0.1499999999999999944, 0.1583333333333333259, 0.1666666666666666574, 0.1749999999999999889, 0.1833333333333333204, 0.1916666666666666796, 0.2000000000000000111, 0.2083333333333333426, 0.2166666666666666741, 0.2250000000000000056, 0.2333333333333333370, 0.2416666666666666685, 0.2500000000000000000, 0.2583333333333333592, 0.2666666666666666630, 0.2750000000000000222, 0.2833333333333333259, 0.2916666666666666852, 0.2999999999999999889, 0.3083333333333333481, 0.3166666666666666519, 0.3250000000000000111, 0.3333333333333333148, 0.3416666666666666741, 0.3499999999999999778, 0.3583333333333333370, 0.3666666666666666408, 0.3750000000000000000, 0.3833333333333333592, 0.3916666666666666630, 0.4000000000000000222, 0.4083333333333333259, 0.4166666666666666852, 0.4249999999999999889, 0.4333333333333333481, 0.4416666666666666519, 0.4500000000000000111, 0.4583333333333333148, 0.4666666666666666741, 0.4749999999999999778, 0.4833333333333333370, 0.4916666666666666408, 0.5000000000000000000, 0.5083333333333333037, 0.5166666666666667185, 0.5250000000000000222, 0.5333333333333333259, 0.5416666666666666297, 0.5500000000000000444, 0.5583333333333333481, 0.5666666666666666519, 0.5749999999999999556, 0.5833333333333333703, 0.5916666666666666741, 0.5999999999999999778, 0.6083333333333332815, 0.6166666666666666963, 0.6250000000000000000, 0.6333333333333333037, 0.6416666666666667185, 0.6500000000000000222, 0.6583333333333333259, 0.6666666666666666297, 0.6750000000000000444, 0.6833333333333333481, 0.6916666666666666519, 0.6999999999999999556, 0.7083333333333333703, 0.7166666666666666741, 0.7249999999999999778, 0.7333333333333332815, 0.7416666666666666963, 0.7500000000000000000, 0.7583333333333333037, 0.7666666666666667185, 0.7750000000000000222, 0.7833333333333333259, 0.7916666666666666297, 0.8000000000000000444, 0.8083333333333333481, 0.8166666666666666519, 0.8249999999999999556, 0.8333333333333333703, 0.8416666666666666741, 0.8499999999999999778, 0.8583333333333332815, 0.8666666666666666963, 0.8750000000000000000, 0.8833333333333333037, 0.8916666666666667185, 0.9000000000000000222, 0.9083333333333333259, 0.9166666666666666297, 0.9250000000000000444, 0.9333333333333333481, 0.9416666666666666519, 0.9499999999999999556, 0.9583333333333333703, 0.9666666666666666741, 0.9749999999999999778, 0.9833333333333332815, 0.9916666666666666963, 1.000000000000000000 ),
 .UNSPECIFIED. ) 
 GEOMETRIC_REPRESENTATION_ITEM ( )  RATIONAL_B_SPLINE_SURFACE ( (
 ( 1.000000000000000000, 0.8660254037844387076, 1.000000000000000000, 0.8660254037844387076, 1.000000000000000000, 0.8660254037844387076, 1.000000000000000000, 0.8660254037844387076, 1.000000000000000000, 0.8660254037844387076, 1.000000000000000000, 0.8660254037844387076, 1.000000000000000000, 0.8660254037844387076, 1.000000000000000000, 0.8660254037844387076, 1.000000000000000000, 0.8660254037844387076, 1.000000000000000000, 0.8660254037844387076, 1.000000000000000000, 0.8660254037844387076, 1.000000000000000000, 0.8660254037844387076, 1.000000000000000000, 0.8660254037844387076, 1.000000000000000000, 0.8660254037844387076, 1.000000000000000000, 0.8660254037844387076, 1.000000000000000000, 0.8660254037844387076, 1.000000000000000000, 0.8660254037844387076, 1.000000000000000000, 0.8660254037844387076, 1.000000000000000000, 0.8660254037844387076, 1.000000000000000000, 0.8660254037844387076, 1.000000000000000000, 0.8660254037844387076, 1.000000000000000000, 0.8660254037844387076, 1.000000000000000000, 0.8660254037844387076, 1.000000000000000000, 0.8660254037844387076, 1.000000000000000000, 0.8660254037844387076, 1.000000000000000000, 0.8660254037844387076, 1.000000000000000000, 0.8660254037844387076, 1.000000000000000000, 0.8660254037844387076, 1.000000000000000000, 0.8660254037844387076, 1.000000000000000000, 0.8660254037844387076, 1.000000000000000000, 0.8660254037844387076, 1.000000000000000000, 0.8660254037844387076, 1.000000000000000000, 0.8660254037844387076, 1.000000000000000000, 0.8660254037844387076, 1.000000000000000000, 0.8660254037844387076, 1.000000000000000000, 0.8660254037844387076, 1.000000000000000000, 0.8660254037844387076, 1.000000000000000000, 0.8660254037844387076, 1.000000000000000000, 0.8660254037844387076, 1.000000000000000000, 0.8660254037844387076, 1.000000000000000000, 0.8660254037844387076, 1.000000000000000000, 0.8660254037844387076, 1.000000000000000000, 0.8660254037844387076, 1.000000000000000000, 0.8660254037844387076, 1.000000000000000000, 0.8660254037844387076, 1.000000000000000000, 0.8660254037844387076, 1.000000000000000000, 0.8660254037844387076, 1.000000000000000000, 0.8660254037844387076, 1.000000000000000000, 0.8660254037844387076, 1.000000000000000000, 0.8660254037844387076, 1.000000000000000000, 0.8660254037844387076, 1.000000000000000000, 0.8660254037844387076, 1.000000000000000000, 0.8660254037844387076, 1.000000000000000000, 0.8660254037844387076, 1.000000000000000000, 0.8660254037844387076, 1.000000000000000000, 0.8660254037844387076, 1.000000000000000000, 0.8660254037844387076, 1.000000000000000000, 0.8660254037844387076, 1.000000000000000000, 0.8660254037844387076, 1.000000000000000000, 0.8660254037844387076, 1.000000000000000000, 0.8660254037844387076, 1.000000000000000000, 0.8660254037844387076, 1.000000000000000000, 0.8660254037844387076, 1.000000000000000000, 0.8660254037844387076, 1.000000000000000000, 0.8660254037844387076, 1.000000000000000000, 0.8660254037844387076, 1.000000000000000000, 0.8660254037844387076, 1.000000000000000000, 0.8660254037844387076, 1.000000000000000000, 0.8660254037844387076, 1.000000000000000000, 0.8660254037844387076, 1.000000000000000000, 0.8660254037844387076, 1.000000000000000000, 0.8660254037844387076, 1.000000000000000000, 0.8660254037844387076, 1.000000000000000000, 0.8660254037844387076, 1.000000000000000000, 0.8660254037844387076, 1.000000000000000000, 0.8660254037844387076, 1.000000000000000000, 0.8660254037844387076, 1.000000000000000000, 0.8660254037844387076, 1.000000000000000000, 0.8660254037844387076, 1.000000000000000000, 0.8660254037844387076, 1.000000000000000000, 0.8660254037844387076, 1.000000000000000000, 0.8660254037844387076, 1.000000000000000000, 0.8660254037844387076, 1.000000000000000000, 0.8660254037844387076, 1.000000000000000000, 0.8660254037844387076, 1.000000000000000000, 0.8660254037844387076, 1.000000000000000000, 0.8660254037844387076, 1.000000000000000000, 0.8660254037844387076, 1.000000000000000000, 0.8660254037844387076, 1.000000000000000000, 0.8660254037844387076, 1.000000000000000000, 0.8660254037844387076, 1.000000000000000000, 0.8660254037844387076, 1.000000000000000000, 0.8660254037844387076, 1.000000000000000000, 0.8660254037844387076, 1.000000000000000000, 0.8660254037844387076, 1.000000000000000000, 0.8660254037844387076, 1.000000000000000000, 0.8660254037844387076, 1.000000000000000000, 0.8660254037844387076, 1.000000000000000000, 0.8660254037844387076, 1.000000000000000000, 0.8660254037844387076, 1.000000000000000000, 0.8660254037844387076, 1.000000000000000000, 0.8660254037844387076, 1.000000000000000000, 0.8660254037844387076, 1.000000000000000000, 0.8660254037844387076, 1.000000000000000000, 0.8660254037844387076, 1.000000000000000000, 0.8660254037844387076, 1.000000000000000000, 0.8660254037844387076, 1.000000000000000000, 0.8660254037844387076, 1.000000000000000000, 0.8660254037844387076, 1.000000000000000000, 0.8660254037844387076, 1.000000000000000000, 0.8660254037844387076, 1.000000000000000000, 0.8660254037844387076, 1.000000000000000000, 0.8660254037844387076, 1.000000000000000000, 0.8660254037844387076, 1.000000000000000000, 0.8660254037844387076, 1.000000000000000000, 0.8660254037844387076, 1.000000000000000000, 0.8660254037844387076, 1.000000000000000000, 0.8660254037844387076, 1.000000000000000000, 0.8660254037844387076, 1.000000000000000000, 0.8660254037844387076, 1.000000000000000000),
 ( 1.000000000000000000, 0.8660254037844387076, 1.000000000000000000, 0.8660254037844387076, 1.000000000000000000, 0.8660254037844387076, 1.000000000000000000, 0.8660254037844387076, 1.000000000000000000, 0.8660254037844387076, 1.000000000000000000, 0.8660254037844387076, 1.000000000000000000, 0.8660254037844387076, 1.000000000000000000, 0.8660254037844387076, 1.000000000000000000, 0.8660254037844387076, 1.000000000000000000, 0.8660254037844387076, 1.000000000000000000, 0.8660254037844387076, 1.000000000000000000, 0.8660254037844387076, 1.000000000000000000, 0.8660254037844387076, 1.000000000000000000, 0.8660254037844387076, 1.000000000000000000, 0.8660254037844387076, 1.000000000000000000, 0.8660254037844387076, 1.000000000000000000, 0.8660254037844387076, 1.000000000000000000, 0.8660254037844387076, 1.000000000000000000, 0.8660254037844387076, 1.000000000000000000, 0.8660254037844387076, 1.000000000000000000, 0.8660254037844387076, 1.000000000000000000, 0.8660254037844387076, 1.000000000000000000, 0.8660254037844387076, 1.000000000000000000, 0.8660254037844387076, 1.000000000000000000, 0.8660254037844387076, 1.000000000000000000, 0.8660254037844387076, 1.000000000000000000, 0.8660254037844387076, 1.000000000000000000, 0.8660254037844387076, 1.000000000000000000, 0.8660254037844387076, 1.000000000000000000, 0.8660254037844387076, 1.000000000000000000, 0.8660254037844387076, 1.000000000000000000, 0.8660254037844387076, 1.000000000000000000, 0.8660254037844387076, 1.000000000000000000, 0.8660254037844387076, 1.000000000000000000, 0.8660254037844387076, 1.000000000000000000, 0.8660254037844387076, 1.000000000000000000, 0.8660254037844387076, 1.000000000000000000, 0.8660254037844387076, 1.000000000000000000, 0.8660254037844387076, 1.000000000000000000, 0.8660254037844387076, 1.000000000000000000, 0.8660254037844387076, 1.000000000000000000, 0.8660254037844387076, 1.000000000000000000, 0.8660254037844387076, 1.000000000000000000, 0.8660254037844387076, 1.000000000000000000, 0.8660254037844387076, 1.000000000000000000, 0.8660254037844387076, 1.000000000000000000, 0.8660254037844387076, 1.000000000000000000, 0.8660254037844387076, 1.000000000000000000, 0.8660254037844387076, 1.000000000000000000, 0.8660254037844387076, 1.000000000000000000, 0.8660254037844387076, 1.000000000000000000, 0.8660254037844387076, 1.000000000000000000, 0.8660254037844387076, 1.000000000000000000, 0.8660254037844387076, 1.000000000000000000, 0.8660254037844387076, 1.000000000000000000, 0.8660254037844387076, 1.000000000000000000, 0.8660254037844387076, 1.000000000000000000, 0.8660254037844387076, 1.000000000000000000, 0.8660254037844387076, 1.000000000000000000, 0.8660254037844387076, 1.000000000000000000, 0.8660254037844387076, 1.000000000000000000, 0.8660254037844387076, 1.000000000000000000, 0.8660254037844387076, 1.000000000000000000, 0.8660254037844387076, 1.000000000000000000, 0.8660254037844387076, 1.000000000000000000, 0.8660254037844387076, 1.000000000000000000, 0.8660254037844387076, 1.000000000000000000, 0.8660254037844387076, 1.000000000000000000, 0.8660254037844387076, 1.000000000000000000, 0.8660254037844387076, 1.000000000000000000, 0.8660254037844387076, 1.000000000000000000, 0.8660254037844387076, 1.000000000000000000, 0.8660254037844387076, 1.000000000000000000, 0.8660254037844387076, 1.000000000000000000, 0.8660254037844387076, 1.000000000000000000, 0.8660254037844387076, 1.000000000000000000, 0.8660254037844387076, 1.000000000000000000, 0.8660254037844387076, 1.000000000000000000, 0.8660254037844387076, 1.000000000000000000, 0.8660254037844387076, 1.000000000000000000, 0.8660254037844387076, 1.000000000000000000, 0.8660254037844387076, 1.000000000000000000, 0.8660254037844387076, 1.000000000000000000, 0.8660254037844387076, 1.000000000000000000, 0.8660254037844387076, 1.000000000000000000, 0.8660254037844387076, 1.000000000000000000, 0.8660254037844387076, 1.000000000000000000, 0.8660254037844387076, 1.000000000000000000, 0.8660254037844387076, 1.000000000000000000, 0.8660254037844387076, 1.000000000000000000, 0.8660254037844387076, 1.000000000000000000, 0.8660254037844387076, 1.000000000000000000, 0.8660254037844387076, 1.000000000000000000, 0.8660254037844387076, 1.000000000000000000, 0.8660254037844387076, 1.000000000000000000, 0.8660254037844387076, 1.000000000000000000, 0.8660254037844387076, 1.000000000000000000, 0.8660254037844387076, 1.000000000000000000, 0.8660254037844387076, 1.000000000000000000, 0.8660254037844387076, 1.000000000000000000, 0.8660254037844387076, 1.000000000000000000, 0.8660254037844387076, 1.000000000000000000, 0.8660254037844387076, 1.000000000000000000, 0.8660254037844387076, 1.000000000000000000, 0.8660254037844387076, 1.000000000000000000, 0.8660254037844387076, 1.000000000000000000, 0.8660254037844387076, 1.000000000000000000, 0.8660254037844387076, 1.000000000000000000, 0.8660254037844387076, 1.000000000000000000, 0.8660254037844387076, 1.000000000000000000, 0.8660254037844387076, 1.000000000000000000, 0.8660254037844387076, 1.000000000000000000, 0.8660254037844387076, 1.000000000000000000, 0.8660254037844387076, 1.000000000000000000, 0.8660254037844387076, 1.000000000000000000, 0.8660254037844387076, 1.000000000000000000, 0.8660254037844387076, 1.000000000000000000, 0.8660254037844387076, 1.000000000000000000, 0.8660254037844387076, 1.000000000000000000, 0.8660254037844387076, 1.000000000000000000) ) ) 
 REPRESENTATION_ITEM ( '' )  SURFACE ( )  );
#103658 = MECHANICAL_DESIGN_GEOMETRIC_PRESENTATION_REPRESENTATION (  '', ( #69140 ), #110683 ) ;
#103659 = CARTESIAN_POINT ( 'NONE',  ( 8.446893396513862839, 9.813462703143045474, -1.199719254218445830 ) ) ;
#103660 = CARTESIAN_POINT ( 'NONE',  ( 6.461392557816405535, 1.719054114842766268, 1.153505076091146275 ) ) ;
#103661 = CARTESIAN_POINT ( 'NONE',  ( 0.6801582343749744686, 0.3385416670080923507, -1.178068619123886718 ) ) ;
#103662 = ADVANCED_FACE ( 'NONE', ( #108129 ), #8052, .T. ) ;
#103663 = CARTESIAN_POINT ( 'NONE',  ( 6.444889499930222421, -1.758869480593090673, -1.307235502039267860 ) ) ;
#103664 = CARTESIAN_POINT ( 'NONE',  ( 6.083581728852979431, 7.123651168416324175, -1.137916992902558100 ) ) ;
#103665 = CARTESIAN_POINT ( 'NONE',  ( -5.600700517108988308, 15.46906632287834071, -10.62221823295361567 ) ) ;
#103666 = EDGE_LOOP ( 'NONE', ( #173809, #205775, #75152, #130166 ) ) ;
#103667 = VERTEX_POINT ( 'NONE', #30854 ) ;
#103668 = DIRECTION ( 'NONE',  ( 0.7592566023652995710, -0.6507913734559650498, -0.000000000000000000 ) ) ;
#103669 = CARTESIAN_POINT ( 'NONE',  ( 4.147608549738549755, 0.6325110726591240962, -1.760471310998643402 ) ) ;
#103670 = CARTESIAN_POINT ( 'NONE',  ( -3.285556943749998737, -1.217708332855376607, 1.896917185911908721 ) ) ;
#103671 = LINE ( 'NONE', #121063, #140420 ) ;
#103672 = CARTESIAN_POINT ( 'NONE',  ( -7.293923454472094114, 9.532663335016016148, 1.443375672974090751 ) ) ;
#103673 = CARTESIAN_POINT ( 'NONE',  ( 5.194709132691408549, 6.089524072008651423, 1.199719254218452935 ) ) ;
#103674 = CARTESIAN_POINT ( 'NONE',  ( 0.3737962156708526384, -1.932529848913757897, 0.3785758322861746406 ) ) ;
#103675 = EDGE_CURVE ( 'NONE', #24541, #153164, #44975, .T. ) ;
#103676 = CARTESIAN_POINT ( 'NONE',  ( 1.458611474731505986, -1.915607644094442064, -0.6298556652749932594 ) ) ;
#103677 = CARTESIAN_POINT ( 'NONE',  ( -9.917953063596627317, 11.52969898140628047, -1.199719254218441611 ) ) ;
#103678 = CARTESIAN_POINT ( 'NONE',  ( 5.182959862174088883, 9.268813282503625572, 0.7998128361456331437 ) ) ;
#103679 = CARTESIAN_POINT ( 'NONE',  ( 0.000000000000000000, -7.666862915010147717, 0.000000000000000000 ) ) ;
#103680 = CARTESIAN_POINT ( 'NONE',  ( 1.482659311839970684, -0.3241159351022730450, -2.167229700873399612 ) ) ;
#103681 = CARTESIAN_POINT ( 'NONE',  ( -2.123823618835070537, 5.629544655282869847, 1.040834085586084257E-14 ) ) ;
#103682 = CARTESIAN_POINT ( 'NONE',  ( 5.058600711674583472, 8.915801573680086634, 0.000000000000000000 ) ) ;
#103683 = CARTESIAN_POINT ( 'NONE',  ( 7.899597058256738968, 12.36794700127490820, 1.040834085586084257E-14 ) ) ;
#103684 = CARTESIAN_POINT ( 'NONE',  ( 3.948449050077836642, 5.629609863222681199, 1.599625672291267398 ) ) ;
#103685 = CARTESIAN_POINT ( 'NONE',  ( 7.688882512725796481, 8.142986817701137525, 0.000000000000000000 ) ) ;
#103686 = VERTEX_POINT ( 'NONE', #96931 ) ;
#103688 = CARTESIAN_POINT ( 'NONE',  ( 0.5045416345675997061, -1.998124945550180609, -0.2444111669489754113 ) ) ;
#103687 = CARTESIAN_POINT ( 'NONE',  ( 4.317794123949899365, 1.129187743159822288, -1.454283868005897151 ) ) ;
#103689 = CARTESIAN_POINT ( 'NONE',  ( 2.478211020838327894, 2.052291828077044133, 1.034905392717075046 ) ) ;
#103691 = CARTESIAN_POINT ( 'NONE',  ( 6.104347744599991188, 1.959368324604572775, 0.09974838594294095639 ) ) ;
#103690 = CARTESIAN_POINT ( 'NONE',  ( 5.205967797967541166, 5.175976640491323444, -0.7216878364870197293 ) ) ;
#103692 = CARTESIAN_POINT ( 'NONE',  ( -1.642778471875000035, -4.017708332855376874, -2.845375778867859751 ) ) ;
#103693 = CARTESIAN_POINT ( 'NONE',  ( -4.283486466913726254, 7.084819080452935403, -1.199719254218452047 ) ) ;
#103694 = CARTESIAN_POINT ( 'NONE',  ( 4.693567934957057375, 1.782326746607498791, -0.6936623114904352239 ) ) ;
#103695 = CARTESIAN_POINT ( 'NONE',  ( -9.459838494033043332, 12.05956421450382088, 1.599625672291281386 ) ) ;
#103696 = CARTESIAN_POINT ( 'NONE',  ( 6.335378924966214242, 6.849830188997488634, 0.6565068261209184852 ) ) ;
#103697 = CARTESIAN_POINT ( 'NONE',  ( -6.292392690518202159, 9.394856334696294553, -1.082531754730549967 ) ) ;
#103699 = CARTESIAN_POINT ( 'NONE',  ( 1.955717210371358483, 1.865846021326333926, -0.1348392221205765851 ) ) ;
#103698 = CARTESIAN_POINT ( 'NONE',  ( 2.296528860280427686, 1.677371239548936854, -1.247825592998616617 ) ) ;
#103700 = CARTESIAN_POINT ( 'NONE',  ( 8.270110514656034084, 9.711179024262627024, 1.082531754730558626 ) ) ;
#103701 = CARTESIAN_POINT ( 'NONE',  ( -1.364683531250010740, 5.092708333674757171, 0.7879004041258379498 ) ) ;
#103702 = CARTESIAN_POINT ( 'NONE',  ( 2.946521060880839205, -1.424341091986385921, -0.9998927444686573907 ) ) ;
#103703 = CARTESIAN_POINT ( 'NONE',  ( 3.635557746758808495, 7.393234471193928847, -0.7998128361456291469 ) ) ;
#103705 = CARTESIAN_POINT ( 'NONE',  ( 0.2798451837294911870, 3.302884587574776099, -1.982903847885383763 ) ) ;
#103704 = CARTESIAN_POINT ( 'NONE',  ( 1.734723475976807094E-15, -3.469446951953614189E-15, -0.2879360613984097150 ) ) ;
#103706 = CARTESIAN_POINT ( 'NONE',  ( 3.492533829797561218, -0.3379890457658150105, -1.691244694301207829 ) ) ;
#103707 = CARTESIAN_POINT ( 'NONE',  ( 3.966501855323391723, -2.045284974426237579, -0.7877190255709336508 ) ) ;
#103708 = CARTESIAN_POINT ( 'NONE',  ( 5.901041445831936016, 1.806360628843254768, -1.267562117129708232 ) ) ;
#103709 = CARTESIAN_POINT ( 'NONE',  ( 4.081882008079450230, 3.980588341361369853, -0.7346435760097062007 ) ) ;
#103710 = CARTESIAN_POINT ( 'NONE',  ( 3.502934933135398055, 0.5226102428602089622, 2.107139934106997181 ) ) ;
#103711 = CARTESIAN_POINT ( 'NONE',  ( 2.367563199519676420, 1.790531440309536926, -0.3556685536310541518 ) ) ;
#103712 = CARTESIAN_POINT ( 'NONE',  ( 0.000000000000000000, -6.893137084989842123, 0.000000000000000000 ) ) ;
#103713 = CARTESIAN_POINT ( 'NONE',  ( 4.997310516409209313, -0.3076690597460414733, 2.094731796426703152 ) ) ;
#103714 = EDGE_LOOP ( 'NONE', ( #176698, #109045, #72848, #175746 ) ) ;
#103716 = CARTESIAN_POINT ( 'NONE',  ( 1.364683531249988535, 3.217708333674748289, -0.7879004041258239610 ) ) ;
#103715 = CARTESIAN_POINT ( 'NONE',  ( 5.144168085839278426, 0.6632553684719083575, 2.194301386939989218 ) ) ;
#103717 = CARTESIAN_POINT ( 'NONE',  ( 6.720655732516671144, 1.288224904612661925, 1.942155157606942240 ) ) ;
#103718 = CARTESIAN_POINT ( 'NONE',  ( 8.353795204314554468, 12.89784483834236184, -0.7998128361456352531 ) ) ;
#103719 = CARTESIAN_POINT ( 'NONE',  ( 0.3992906662320141464, -0.2637550127744873185, -2.103967267096308991 ) ) ;
#103720 = CARTESIAN_POINT ( 'NONE',  ( -5.748293942514189681, 5.808690475795744490, -0.7216878364870207285 ) ) ;
#103721 = AXIS2_PLACEMENT_3D ( 'NONE', #173170, #46353, #45289 ) ;
#103722 = DIRECTION ( 'NONE',  ( 0.000000000000000000, 0.000000000000000000, -1.000000000000000000 ) ) ;
#103723 = CARTESIAN_POINT ( 'NONE',  ( -5.761852095683518193, 6.784877535461274256, 1.082531754730546636 ) ) ;
#103725 = CARTESIAN_POINT ( 'NONE',  ( -6.009258394948636914E-15, 10.71875000068279959, -1.732050807568875195 ) ) ;
#103724 = CARTESIAN_POINT ( 'NONE',  ( 6.883263157960376688, 2.059069814638575302, 2.260828084523508252 ) ) ;
#103726 = EDGE_LOOP ( 'NONE', ( #10534, #81022, #208078, #108940 ) ) ;
#103727 = CARTESIAN_POINT ( 'NONE',  ( 4.940077362011475515, -1.704937458037486531, -1.076318853994034930 ) ) ;
#103729 = CARTESIAN_POINT ( 'NONE',  ( 4.522371018022923295, 0.9678747400500853360, 1.821345444039919270 ) ) ;
#103728 = CARTESIAN_POINT ( 'NONE',  ( 5.473741331615251227, 7.409117525016355010, -1.599625672291262513 ) ) ;
#103731 = CARTESIAN_POINT ( 'NONE',  ( -0.2409995289980246258, 7.629137130509076492, -2.600476469121239198 ) ) ;
#103730 = CARTESIAN_POINT ( 'NONE',  ( 4.857564175446106525, 8.889184981320973122, 0.7998128361456331437 ) ) ;
#103732 = CARTESIAN_POINT ( 'NONE',  ( 7.876360894896227371, 8.153785563659219804, -0.7998128361456341429 ) ) ;
#103733 = CARTESIAN_POINT ( 'NONE',  ( -3.285556943749998737, -1.130208332855377140, 1.896917185911908499 ) ) ;
#103734 = CARTESIAN_POINT ( 'NONE',  ( -15.75000000000000000, 10.19999999999999929, 0.6999999999999992895 ) ) ;
#103735 = CARTESIAN_POINT ( 'NONE',  ( 1.007895156502825573, -0.9414231642565270564, -1.866751856443664037 ) ) ;
#103736 = CARTESIAN_POINT ( 'NONE',  ( 4.535779832184696936, -1.617819081767550182, 1.203352566194588746 ) ) ;
#103737 = CARTESIAN_POINT ( 'NONE',  ( 2.911469271472226339, -0.9098125248445630975, -1.600700954789348263 ) ) ;
#103738 = CARTESIAN_POINT ( 'NONE',  ( 6.356075086708249167, 6.309842444114747373, -0.7998128361456281477 ) ) ;
#103739 = FILL_AREA_STYLE_COLOUR ( '', #37786 ) ;
#103740 = CARTESIAN_POINT ( 'NONE',  ( 0.3754632410046651048, 0.9867877818048297334, 1.414398233496700907 ) ) ;
#103741 = CARTESIAN_POINT ( 'NONE',  ( 0.1747926744264660659, 7.629137130509076492, -2.455305974604492292 ) ) ;
#103742 = CARTESIAN_POINT ( 'NONE',  ( 0.8097366424872083357, 1.363176973609769416, -1.850781266144943205 ) ) ;
#103743 = CARTESIAN_POINT ( 'NONE',  ( -6.196239896645333367, 7.187700286629718605, -1.199719254218446718 ) ) ;
#103744 = CARTESIAN_POINT ( 'NONE',  ( 0.3513179634891601677, -1.816012830335328232, 1.349138783986586931 ) ) ;
#103745 = CARTESIAN_POINT ( 'NONE',  ( 3.071027892464781583, -1.946086441943569723, -0.8056474276203289264 ) ) ;
#103746 = CARTESIAN_POINT ( 'NONE',  ( -4.122561227007127016, 6.967349310553715647, 1.199719254218452935 ) ) ;
#103747 = CARTESIAN_POINT ( 'NONE',  ( 7.721532178182734185, 8.967207948423393304, 1.199719254218462483 ) ) ;
#103748 = CARTESIAN_POINT ( 'NONE',  ( 4.692530563661249765, 8.488719734331187539, 0.000000000000000000 ) ) ;
#103749 = CARTESIAN_POINT ( 'NONE',  ( 0.000000000000000000, 1.328312333417671853, -2.244820250217825830 ) ) ;
#103751 = EDGE_CURVE ( 'NONE', #171829, #18446, #170771, .T. ) ;
#103750 = CARTESIAN_POINT ( 'NONE',  ( -7.061099074618889304, 7.132370430010492868, -0.7998128361456291469 ) ) ;
#103752 = CARTESIAN_POINT ( 'NONE',  ( 5.463572716182812705, 9.317992568947877530, 0.7216878364870438212 ) ) ;
#103753 = CARTESIAN_POINT ( 'NONE',  ( 4.815752433886056671, 6.955745678547994970, 1.411323681429425880 ) ) ;
#103754 = CARTESIAN_POINT ( 'NONE',  ( -3.598799709423620374, 6.286017863381107240, 1.199719254218464037 ) ) ;
#103756 = CARTESIAN_POINT ( 'NONE',  ( 3.516091144284401171, -0.6417545297995127518, 2.126723297420398673 ) ) ;
#103755 = CARTESIAN_POINT ( 'NONE',  ( 2.426173717206762781, -2.096881089210366422, 0.3156149858808757203 ) ) ;
#103757 = CARTESIAN_POINT ( 'NONE',  ( 2.291216553123593958, 1.694975396412688351, 1.389067552005143646 ) ) ;
#103758 = CARTESIAN_POINT ( 'NONE',  ( -5.819474248763749635, 7.812472595022922128, -1.599625672291256295 ) ) ;
#103759 = CARTESIAN_POINT ( 'NONE',  ( -3.797165540279144214, 6.587721009371067638, 1.199719254218452935 ) ) ;
#103760 = CARTESIAN_POINT ( 'NONE',  ( 5.775826483351648832, -1.914393393812302113, 0.4282712878391075062 ) ) ;
#103761 = CARTESIAN_POINT ( 'NONE',  ( 0.6823417656249882723, 2.176041667008084435, -1.181850606188749264 ) ) ;
#103762 = CARTESIAN_POINT ( 'NONE',  ( 6.610000000000009202, 6.036727194997777879, 2.594899704271665275 ) ) ;
#103764 = EDGE_LOOP ( 'NONE', ( #128412, #2939, #156393, #28401 ) ) ;
#103763 = CARTESIAN_POINT ( 'NONE',  ( -5.748293942514186128, 6.769059690097084747, -1.082531754730544860 ) ) ;
#103765 = CARTESIAN_POINT ( 'NONE',  ( 4.588201236890728119, 1.223260742344203900, 1.732012071221388450 ) ) ;
#103766 = CARTESIAN_POINT ( 'NONE',  ( -3.471769853551161411, 6.208092708188416076, 1.199719254218452935 ) ) ;
#103767 = EDGE_LOOP ( 'NONE', ( #203184, #6673, #73057, #121641, #3503, #150935, #178992 ) ) ;
#103769 = CARTESIAN_POINT ( 'NONE',  ( 5.787991602622606813, -0.9759734195362681497, 1.928925553883020338 ) ) ;
#103768 = CARTESIAN_POINT ( 'NONE',  ( -4.502716413514296079, 8.267269892493059658, -0.7216878364870338292 ) ) ;
#103770 = CARTESIAN_POINT ( 'NONE',  ( 6.819914962873951936, 7.915321197229798322, -1.199719254218446718 ) ) ;
#103771 = CARTESIAN_POINT ( 'NONE',  ( 5.513187957602974976, -1.795010045117376496, 0.4093405989887277663 ) ) ;
#103772 = LINE ( 'NONE', #169824, #72140 ) ;
#103773 = CARTESIAN_POINT ( 'NONE',  ( 0.6823417656249882723, 2.488541667008084435, -1.181850606188749264 ) ) ;
#103774 = CARTESIAN_POINT ( 'NONE',  ( 1.575334329707895664, -0.9311816076861539893, 1.470162731330543426 ) ) ;
#103775 = CARTESIAN_POINT ( 'NONE',  ( 1.264911064067349322, 3.816124033181332642, 0.5000000000000056621 ) ) ;
#103776 = DIRECTION ( 'NONE',  ( 0.000000000000000000, 0.000000000000000000, 1.000000000000000000 ) ) ;
#103777 = CARTESIAN_POINT ( 'NONE',  ( 9.809231760985728243, 10.20995912723616428, -6.918706496639274839 ) ) ;
#103778 = AXIS2_PLACEMENT_3D ( 'NONE', #19966, #184601, #117549 ) ;
#103779 = CARTESIAN_POINT ( 'NONE',  ( 4.786082296487640164, -1.021991182799499409, 1.904868704497929333 ) ) ;
#103780 = CARTESIAN_POINT ( 'NONE',  ( -4.355193658487827690, 6.104145239700998538, -1.599625672291256295 ) ) ;
#103781 = CARTESIAN_POINT ( 'NONE',  ( -7.822691444960716112, 8.228820895316715678, -0.7216878364870267237 ) ) ;
#103782 = CARTESIAN_POINT ( 'NONE',  ( 4.786082296487640164, -1.021991182799499409, 1.904868704497929333 ) ) ;
#103783 = CARTESIAN_POINT ( 'NONE',  ( 5.290288327143207958, -1.956129722686357431, -0.2442305991610035365 ) ) ;
#103784 = CARTESIAN_POINT ( 'NONE',  ( 4.428821037005469030, 0.8169072895964669678, 1.529287752448208471 ) ) ;
#103785 = CARTESIAN_POINT ( 'NONE',  ( 0.9959476074029065540, -2.191739723303194332, 0.005169097091584088505 ) ) ;
#103786 = CARTESIAN_POINT ( 'NONE',  ( 2.239721530183640841, -2.061013379209011287, 1.037980457044695992 ) ) ;
#103787 = CARTESIAN_POINT ( 'NONE',  ( 3.954412886046823949, 0.7382688757093980314, 1.924196998259326996 ) ) ;
#103788 = CARTESIAN_POINT ( 'NONE',  ( 0.2869206542332564114, 1.438414604794725049, 1.304842588618974952 ) ) ;
#103789 = CARTESIAN_POINT ( 'NONE',  ( -7.158341917891067219, 11.29522330427417565, 0.000000000000000000 ) ) ;
#103791 = EDGE_CURVE ( 'NONE', #195702, #115034, #185942, .T. ) ;
#103790 = CARTESIAN_POINT ( 'NONE',  ( -4.606738333593328072, 8.596554832492683929, 0.7998128361456281477 ) ) ;
#103792 = PLANE ( 'NONE',  #120030 ) ;
#103793 = CARTESIAN_POINT ( 'NONE',  ( -3.492107083971660586, 6.231819477012331632, 1.199719254218452935 ) ) ;
#103794 = CARTESIAN_POINT ( 'NONE',  ( -6.738039155867462604, 7.923762439009225389, 1.082531754730549967 ) ) ;
#103795 = CARTESIAN_POINT ( 'NONE',  ( 3.716033540554028125, -2.174548934981130444, 0.3748234698989146851 ) ) ;
#103796 = CARTESIAN_POINT ( 'NONE',  ( 1.642778471875000035, -2.063541666188710266, -2.845375778867859751 ) ) ;
#103797 = VERTEX_POINT ( 'NONE', #180291 ) ;
#103798 = CARTESIAN_POINT ( 'NONE',  ( 0.8833916088089890373, -1.769421289247067097, 0.5767519331581376640 ) ) ;
#103799 = CARTESIAN_POINT ( 'NONE',  ( -0.1288028175206725467, 2.854926803129751001, -2.761885894952537779 ) ) ;
#103800 = SURFACE_STYLE_USAGE ( .BOTH. , #102726 ) ;
#103801 = CARTESIAN_POINT ( 'NONE',  ( -9.499050059654539524, -8.104757123234332283, 0.1520312049661968479 ) ) ;
#103803 = CARTESIAN_POINT ( 'NONE',  ( 6.925078400183548588, 3.689301810296021777, 2.558360072861276979 ) ) ;
#103802 = CARTESIAN_POINT ( 'NONE',  ( -6.335246490290919574, 6.944623119882351148, -0.8941629942194727620 ) ) ;
#103804 = CARTESIAN_POINT ( 'NONE',  ( 11.96215121607992771, 13.82833553780823976, 0.9565349792967584586 ) ) ;
#103805 = VERTEX_POINT ( 'NONE', #61201 ) ;
#103806 = CARTESIAN_POINT ( 'NONE',  ( 2.782161975763951300, -1.060548055690222702, 1.766919142140084720 ) ) ;
#103807 = CARTESIAN_POINT ( 'NONE',  ( 1.360316468749983576, 0.9947916670081107249, 0.7853790794158601596 ) ) ;
#103808 = CARTESIAN_POINT ( 'NONE',  ( -6.013204822860843457, 6.974159367214481264, -1.199719254218446718 ) ) ;
#103809 = DIRECTION ( 'NONE',  ( 0.000000000000000000, 1.000000000000000000, -3.330669073875479482E-16 ) ) ;
#103810 = CARTESIAN_POINT ( 'NONE',  ( 4.792970997630896512, 5.550553237779539018, 1.199719254218464037 ) ) ;
#103811 = CARTESIAN_POINT ( 'NONE',  ( 2.413025777909239000, 1.840395853916647173, 0.9276406582674895374 ) ) ;
#103813 = CARTESIAN_POINT ( 'NONE',  ( -0.6823417656250003738, 12.65104166700806232, 1.181850606188754593 ) ) ;
#103812 = DIRECTION ( 'NONE',  ( -5.551115123125765446E-17, 0.000000000000000000, 1.000000000000000000 ) ) ;
#103814 = CARTESIAN_POINT ( 'NONE',  ( 5.282873410819217241, 9.315102745931094219, -0.7998128361456281477 ) ) ;
#103815 =( GEOMETRIC_REPRESENTATION_CONTEXT ( 3 ) GLOBAL_UNCERTAINTY_ASSIGNED_CONTEXT ( ( #137887 ) ) GLOBAL_UNIT_ASSIGNED_CONTEXT ( ( #198809, #138117, #22177 ) ) REPRESENTATION_CONTEXT ( 'NONE', 'WORKASPACE' ) );
#103816 = FILL_AREA_STYLE_COLOUR ( '', #74065 ) ;
#103817 = CARTESIAN_POINT ( 'NONE',  ( 5.918643953348324160, 1.484978324971843566, -1.632713241052483832 ) ) ;
#103818 = CARTESIAN_POINT ( 'NONE',  ( 6.854744688279930998, -1.755419801747569286, 1.426855864884185809 ) ) ;
#103819 = CARTESIAN_POINT ( 'NONE',  ( -4.826339496784927796, 5.693446170079573321, 1.082531754730560403 ) ) ;
#103820 = CARTESIAN_POINT ( 'NONE',  ( 0.3039231887648624619, -1.082844287645868375, -1.700959134490941160 ) ) ;
#103821 = SURFACE_SIDE_STYLE ('',( #101675 ) ) ;
#103822 = DIRECTION ( 'NONE',  ( -0.000000000000000000, -1.000000000000000000, -0.000000000000000000 ) ) ;
#103823 = SURFACE_STYLE_FILL_AREA ( #137397 ) ;
#103824 = CARTESIAN_POINT ( 'NONE',  ( 1.902992089709685031, 1.553661375375714471, 1.041555772207984676 ) ) ;
#103825 = CARTESIAN_POINT ( 'NONE',  ( 3.977750132953357998, -0.7672935630990398437, 1.865046046545227654 ) ) ;
#103827 = CARTESIAN_POINT ( 'NONE',  ( 6.639320575229264776, 1.250520135805782029, 2.217830841512329787 ) ) ;
#103826 = CARTESIAN_POINT ( 'NONE',  ( -1.402160292154681736E-14, 0.9468750003414176941, -1.575800808251659024 ) ) ;
#103829 = CARTESIAN_POINT ( 'NONE',  ( 4.969407589744497145, 0.2071734034183834172, -2.095845648730967792 ) ) ;
#103828 = CARTESIAN_POINT ( 'NONE',  ( -6.177711549321182716, 10.35908057418338402, 0.7998128361456481317 ) ) ;
#103830 = CARTESIAN_POINT ( 'NONE',  ( 6.470265622219697477, 8.571729197388226140, -1.599625672291262513 ) ) ;
#103832 = CARTESIAN_POINT ( 'NONE',  ( -6.201965203247477909, 9.323044272842313518, 1.199719254218452047 ) ) ;
#103831 = CARTESIAN_POINT ( 'NONE',  ( 6.086684617892325733, 6.065829907154645539, -0.7998128361456481317 ) ) ;
#103833 = CARTESIAN_POINT ( 'NONE',  ( -0.2039282260588116402, -6.674536912880628670, -9.612297698795913448 ) ) ;
#103834 = CARTESIAN_POINT ( 'NONE',  ( 4.640881595473839383, 1.934004784890541062, 0.5824627899903914718 ) ) ;
#103835 = CARTESIAN_POINT ( 'NONE',  ( -1.201851678989727383E-14, 5.196875000341422357, -1.575800808251660134 ) ) ;
#103836 = CARTESIAN_POINT ( 'NONE',  ( 0.2685208109398624088, -0.8776176662104094861, -1.864379643416124166 ) ) ;
#103837 = CARTESIAN_POINT ( 'NONE',  ( 7.890482213473377193, 11.18901776815221716, -1.082531754730543083 ) ) ;
#103838 = CARTESIAN_POINT ( 'NONE',  ( 5.466167184710096549, 1.060119519021487378, 1.883692621652333532 ) ) ;
#103839 = CARTESIAN_POINT ( 'NONE',  ( 6.658989722967328717, 7.797851427330578566, 1.199719254218452935 ) ) ;
#103840 = CARTESIAN_POINT ( 'NONE',  ( 1.364683531249986537, -0.5322916663252452718, -0.7879004041258309554 ) ) ;
#103842 = CARTESIAN_POINT ( 'NONE',  ( 0.000000000000000000, 3.500000000000003109, 0.000000000000000000 ) ) ;
#103841 = CARTESIAN_POINT ( 'NONE',  ( 5.611095471209277541, 7.639640364534566075, 1.599625672291268286 ) ) ;
#103843 =( BOUNDED_SURFACE ( )  B_SPLINE_SURFACE ( 1, 2, ( 
 ( #54528, #120673, #186651, #10036, #90242, #7892, #76110, #156308, #190911, #142214, #106530, #206098, #91321, #203945, #171476, #207170, #57732, #123889, #41500, #107613, #121747, #55592, #157379, #188792, #189855, #73980, #172556, #138999, #173644, #208228, #140074, #25217, #59860, #8973, #42576, #126012, #24140, #75047, #141162, #187715, #23066, #58794, #124949, #108679, #174707, #26283, #39344, #92397, #205021, #122831, #158435, #191972, #175764, #43639, #109754, #88096, #56667, #154169, #5735, #71814, #137924, #72893, #105440, #89182, #155234, #6815, #40427, #27357, #193051, #127088, #31643, #44705, #29507, #95600, #178965, #161648, #12171, #80381, #210366, #195203, #15357, #209284, #212496, #110812, #93459, #60931, #128162, #78243, #194123, #144365, #143293, #112954, #159496, #30580, #146477, #13243, #115078, #11095, #130281, #196269, #213548, #45773, #145432, #176817, #111890, #79316, #211432, #177894, #64137, #114027, #62006, #47916, #28432, #63063, #129230, #77171, #46840, #96661, #94525, #162714, #147527, #160563, #14286, #180022, #97720, #163778, #81450, #65171, #131326, #197320, #48960, #4420, #198371, #1229, #119339, #82499, #50011, #155, #18561, #165896, #135537, #2288, #185326, #67291, #117205, #66222, #86774, #32692, #152845, #134498, #52144, #133430, #53207, #19629, #150728, #83565, #182124, #149648, #132369, #54281, #70490, #116135, #33753, #151788, #85700, #199437, #181074, #98773, #200501, #51080, #118272, #99830, #148586, #100883, #17481, #164829, #184257, #35883, #101959, #36949, #202631, #169084, #136606, #183202, #3362, #16419, #34808, #166970, #103029, #69432, #84637, #168025, #20683, #201562, #68364, #170150, #105181, #91062, #204759, #158189, #139816, #188534, #5486, #123637, #189600, #124693, #23888, #74796, #7633, #39096, #89994, #141961, #171217, #207973, #21736, #122572, #156045, #120418, #186392, #41246, #40164, #157122, #205845, #8711, #87845, #106278, #73719, #104100, #174448, #140897, #154980, #206907, #153916, #58538, #42312, #138741, #203696, #56411, #172299, #92134, #57478 ),
 ( #107354, #190651, #108428, #9781, #24960, #173376, #26024, #75853, #38029, #71567, #137675, #55342, #121494, #187466, #22811, #88926, #6565, #72645, #45508, #161386, #125758, #130022, #61740, #162449, #176560, #97456, #11910, #14025, #77983, #175504, #145162, #191719, #211167, #178700, #127907, #147264, #43376, #80111, #146216, #31380, #144106, #177637, #27094, #210100, #111624, #193859, #29245, #96399, #212234, #44441, #63867, #60663, #95337, #12970, #59600, #79046, #62792, #126826, #128954, #179764, #192783, #110559, #194933, #46570, #93201, #28170, #30314, #94266, #112689, #196013, #163511, #76907, #160306, #47649, #159232, #143033, #10833, #113760, #15097, #81186, #109497, #209028, #99569, #149383, #98505, #119077, #64922, #185058, #180811, #2027, #165633, #116939, #67030, #83298, #49748, #84379, #135286, #965, #133167, #201300, #199167, #101695, #52940, #17221, #182939, #68096, #114812, #82237, #118013, #34555, #100626, #166702, #18293, #32437, #150466, #115875, #33496, #167765, #36683, #86512, #50813, #85442, #134231, #181860, #102770, #51890, #151527, #200240, #198117, #184002, #168825, #35617, #214328, #19362, #213296, #164567, #16152, #3096, #148328, #69166, #20429, #131072, #197060, #48698, #65960, #132109, #106021, #140641, #120156, #123381, #37767, #4164, #186132, #38835, #137414, #104918, #55087, #72381, #124442, #90803, #189346, #54017, #138480, #74541, #5227, #22559, #103839, #204502, #39912, #70234, #8453, #154724, #40986, #121236, #190400, #170959, #107097, #88664, #172042, #23635, #6307, #24701, #205584, #122314, #187206, #153658, #56152, #169888, #25770, #42058, #21477, #87586, #173120, #57221, #188271, #152577, #136346, #89743, #155792, #7376, #71301, #203433, #73455, #139557, #202368, #156867, #206654, #58286, #108171, #174197, #79857, #211976, #175254, #210915, #157937, #125502, #113504, #30054, #62542, #47391, #28988, #96144, #111370, #76658, #141714, #142773, #128704, #176312, #129771, #177374, #160051, #191465, #95074, #161123, #162195, #209842, #46317, #193610, #10584, #61481, #179512 ) ),
 .UNSPECIFIED., .F., .F., .F. ) 
 B_SPLINE_SURFACE_WITH_KNOTS ( ( 2, 2 ),
 ( 3, 2, 2, 2, 2, 2, 2, 2, 2, 2, 2, 2, 2, 2, 2, 2, 2, 2, 2, 2, 2, 2, 2, 2, 2, 2, 2, 2, 2, 2, 2, 2, 2, 2, 2, 2, 2, 2, 2, 2, 2, 2, 2, 2, 2, 2, 2, 2, 2, 2, 2, 2, 2, 2, 2, 2, 2, 2, 2, 2, 2, 2, 2, 2, 2, 2, 2, 2, 2, 2, 2, 2, 2, 2, 2, 2, 2, 2, 2, 2, 2, 2, 2, 2, 2, 2, 2, 2, 2, 2, 2, 2, 2, 2, 2, 2, 2, 2, 2, 2, 2, 2, 2, 2, 2, 2, 2, 2, 2, 2, 2, 2, 2, 2, 2, 2, 2, 2, 2, 2, 3 ),
 ( 0.000000000000000000, 1.000000000000000000 ),
 ( 0.000000000000000000, 0.008333333333333333218, 0.01666666666666666644, 0.02500000000000000139, 0.03333333333333333287, 0.04166666666666666435, 0.05000000000000000278, 0.05833333333333333426, 0.06666666666666666574, 0.07499999999999999722, 0.08333333333333332871, 0.09166666666666666019, 0.1000000000000000056, 0.1083333333333333370, 0.1166666666666666685, 0.1250000000000000000, 0.1333333333333333315, 0.1416666666666666630, 0.1499999999999999944, 0.1583333333333333259, 0.1666666666666666574, 0.1749999999999999889, 0.1833333333333333204, 0.1916666666666666796, 0.2000000000000000111, 0.2083333333333333426, 0.2166666666666666741, 0.2250000000000000056, 0.2333333333333333370, 0.2416666666666666685, 0.2500000000000000000, 0.2583333333333333592, 0.2666666666666666630, 0.2750000000000000222, 0.2833333333333333259, 0.2916666666666666852, 0.2999999999999999889, 0.3083333333333333481, 0.3166666666666666519, 0.3250000000000000111, 0.3333333333333333148, 0.3416666666666666741, 0.3499999999999999778, 0.3583333333333333370, 0.3666666666666666408, 0.3750000000000000000, 0.3833333333333333592, 0.3916666666666666630, 0.4000000000000000222, 0.4083333333333333259, 0.4166666666666666852, 0.4249999999999999889, 0.4333333333333333481, 0.4416666666666666519, 0.4500000000000000111, 0.4583333333333333148, 0.4666666666666666741, 0.4749999999999999778, 0.4833333333333333370, 0.4916666666666666408, 0.5000000000000000000, 0.5083333333333333037, 0.5166666666666667185, 0.5250000000000000222, 0.5333333333333333259, 0.5416666666666666297, 0.5500000000000000444, 0.5583333333333333481, 0.5666666666666666519, 0.5749999999999999556, 0.5833333333333333703, 0.5916666666666666741, 0.5999999999999999778, 0.6083333333333332815, 0.6166666666666666963, 0.6250000000000000000, 0.6333333333333333037, 0.6416666666666667185, 0.6500000000000000222, 0.6583333333333333259, 0.6666666666666666297, 0.6750000000000000444, 0.6833333333333333481, 0.6916666666666666519, 0.6999999999999999556, 0.7083333333333333703, 0.7166666666666666741, 0.7249999999999999778, 0.7333333333333332815, 0.7416666666666666963, 0.7500000000000000000, 0.7583333333333333037, 0.7666666666666667185, 0.7750000000000000222, 0.7833333333333333259, 0.7916666666666666297, 0.8000000000000000444, 0.8083333333333333481, 0.8166666666666666519, 0.8249999999999999556, 0.8333333333333333703, 0.8416666666666666741, 0.8499999999999999778, 0.8583333333333332815, 0.8666666666666666963, 0.8750000000000000000, 0.8833333333333333037, 0.8916666666666667185, 0.9000000000000000222, 0.9083333333333333259, 0.9166666666666666297, 0.9250000000000000444, 0.9333333333333333481, 0.9416666666666666519, 0.9499999999999999556, 0.9583333333333333703, 0.9666666666666666741, 0.9749999999999999778, 0.9833333333333332815, 0.9916666666666666963, 1.000000000000000000 ),
 .UNSPECIFIED. ) 
 GEOMETRIC_REPRESENTATION_ITEM ( )  RATIONAL_B_SPLINE_SURFACE ( (
 ( 1.000000000000000000, 0.8660254037844387076, 1.000000000000000000, 0.8660254037844387076, 1.000000000000000000, 0.8660254037844387076, 1.000000000000000000, 0.8660254037844387076, 1.000000000000000000, 0.8660254037844387076, 1.000000000000000000, 0.8660254037844387076, 1.000000000000000000, 0.8660254037844387076, 1.000000000000000000, 0.8660254037844387076, 1.000000000000000000, 0.8660254037844387076, 1.000000000000000000, 0.8660254037844387076, 1.000000000000000000, 0.8660254037844387076, 1.000000000000000000, 0.8660254037844387076, 1.000000000000000000, 0.8660254037844387076, 1.000000000000000000, 0.8660254037844387076, 1.000000000000000000, 0.8660254037844387076, 1.000000000000000000, 0.8660254037844387076, 1.000000000000000000, 0.8660254037844387076, 1.000000000000000000, 0.8660254037844387076, 1.000000000000000000, 0.8660254037844387076, 1.000000000000000000, 0.8660254037844387076, 1.000000000000000000, 0.8660254037844387076, 1.000000000000000000, 0.8660254037844387076, 1.000000000000000000, 0.8660254037844387076, 1.000000000000000000, 0.8660254037844387076, 1.000000000000000000, 0.8660254037844387076, 1.000000000000000000, 0.8660254037844387076, 1.000000000000000000, 0.8660254037844387076, 1.000000000000000000, 0.8660254037844387076, 1.000000000000000000, 0.8660254037844387076, 1.000000000000000000, 0.8660254037844387076, 1.000000000000000000, 0.8660254037844387076, 1.000000000000000000, 0.8660254037844387076, 1.000000000000000000, 0.8660254037844387076, 1.000000000000000000, 0.8660254037844387076, 1.000000000000000000, 0.8660254037844387076, 1.000000000000000000, 0.8660254037844387076, 1.000000000000000000, 0.8660254037844387076, 1.000000000000000000, 0.8660254037844387076, 1.000000000000000000, 0.8660254037844387076, 1.000000000000000000, 0.8660254037844387076, 1.000000000000000000, 0.8660254037844387076, 1.000000000000000000, 0.8660254037844387076, 1.000000000000000000, 0.8660254037844387076, 1.000000000000000000, 0.8660254037844387076, 1.000000000000000000, 0.8660254037844387076, 1.000000000000000000, 0.8660254037844387076, 1.000000000000000000, 0.8660254037844387076, 1.000000000000000000, 0.8660254037844387076, 1.000000000000000000, 0.8660254037844387076, 1.000000000000000000, 0.8660254037844387076, 1.000000000000000000, 0.8660254037844387076, 1.000000000000000000, 0.8660254037844387076, 1.000000000000000000, 0.8660254037844387076, 1.000000000000000000, 0.8660254037844387076, 1.000000000000000000, 0.8660254037844387076, 1.000000000000000000, 0.8660254037844387076, 1.000000000000000000, 0.8660254037844387076, 1.000000000000000000, 0.8660254037844387076, 1.000000000000000000, 0.8660254037844387076, 1.000000000000000000, 0.8660254037844387076, 1.000000000000000000, 0.8660254037844387076, 1.000000000000000000, 0.8660254037844387076, 1.000000000000000000, 0.8660254037844387076, 1.000000000000000000, 0.8660254037844387076, 1.000000000000000000, 0.8660254037844387076, 1.000000000000000000, 0.8660254037844387076, 1.000000000000000000, 0.8660254037844387076, 1.000000000000000000, 0.8660254037844387076, 1.000000000000000000, 0.8660254037844387076, 1.000000000000000000, 0.8660254037844387076, 1.000000000000000000, 0.8660254037844387076, 1.000000000000000000, 0.8660254037844387076, 1.000000000000000000, 0.8660254037844387076, 1.000000000000000000, 0.8660254037844387076, 1.000000000000000000, 0.8660254037844387076, 1.000000000000000000, 0.8660254037844387076, 1.000000000000000000, 0.8660254037844387076, 1.000000000000000000, 0.8660254037844387076, 1.000000000000000000, 0.8660254037844387076, 1.000000000000000000, 0.8660254037844387076, 1.000000000000000000, 0.8660254037844387076, 1.000000000000000000, 0.8660254037844387076, 1.000000000000000000, 0.8660254037844387076, 1.000000000000000000, 0.8660254037844387076, 1.000000000000000000, 0.8660254037844387076, 1.000000000000000000, 0.8660254037844387076, 1.000000000000000000, 0.8660254037844387076, 1.000000000000000000, 0.8660254037844387076, 1.000000000000000000, 0.8660254037844387076, 1.000000000000000000, 0.8660254037844387076, 1.000000000000000000, 0.8660254037844387076, 1.000000000000000000, 0.8660254037844387076, 1.000000000000000000, 0.8660254037844387076, 1.000000000000000000, 0.8660254037844387076, 1.000000000000000000, 0.8660254037844387076, 1.000000000000000000, 0.8660254037844387076, 1.000000000000000000, 0.8660254037844387076, 1.000000000000000000, 0.8660254037844387076, 1.000000000000000000, 0.8660254037844387076, 1.000000000000000000, 0.8660254037844387076, 1.000000000000000000, 0.8660254037844387076, 1.000000000000000000, 0.8660254037844387076, 1.000000000000000000, 0.8660254037844387076, 1.000000000000000000, 0.8660254037844387076, 1.000000000000000000, 0.8660254037844387076, 1.000000000000000000, 0.8660254037844387076, 1.000000000000000000, 0.8660254037844387076, 1.000000000000000000, 0.8660254037844387076, 1.000000000000000000, 0.8660254037844387076, 1.000000000000000000, 0.8660254037844387076, 1.000000000000000000, 0.8660254037844387076, 1.000000000000000000, 0.8660254037844387076, 1.000000000000000000, 0.8660254037844387076, 1.000000000000000000, 0.8660254037844387076, 1.000000000000000000, 0.8660254037844387076, 1.000000000000000000, 0.8660254037844387076, 1.000000000000000000, 0.8660254037844387076, 1.000000000000000000, 0.8660254037844387076, 1.000000000000000000, 0.8660254037844387076, 1.000000000000000000, 0.8660254037844387076, 1.000000000000000000),
 ( 1.000000000000000000, 0.8660254037844387076, 1.000000000000000000, 0.8660254037844387076, 1.000000000000000000, 0.8660254037844387076, 1.000000000000000000, 0.8660254037844387076, 1.000000000000000000, 0.8660254037844387076, 1.000000000000000000, 0.8660254037844387076, 1.000000000000000000, 0.8660254037844387076, 1.000000000000000000, 0.8660254037844387076, 1.000000000000000000, 0.8660254037844387076, 1.000000000000000000, 0.8660254037844387076, 1.000000000000000000, 0.8660254037844387076, 1.000000000000000000, 0.8660254037844387076, 1.000000000000000000, 0.8660254037844387076, 1.000000000000000000, 0.8660254037844387076, 1.000000000000000000, 0.8660254037844387076, 1.000000000000000000, 0.8660254037844387076, 1.000000000000000000, 0.8660254037844387076, 1.000000000000000000, 0.8660254037844387076, 1.000000000000000000, 0.8660254037844387076, 1.000000000000000000, 0.8660254037844387076, 1.000000000000000000, 0.8660254037844387076, 1.000000000000000000, 0.8660254037844387076, 1.000000000000000000, 0.8660254037844387076, 1.000000000000000000, 0.8660254037844387076, 1.000000000000000000, 0.8660254037844387076, 1.000000000000000000, 0.8660254037844387076, 1.000000000000000000, 0.8660254037844387076, 1.000000000000000000, 0.8660254037844387076, 1.000000000000000000, 0.8660254037844387076, 1.000000000000000000, 0.8660254037844387076, 1.000000000000000000, 0.8660254037844387076, 1.000000000000000000, 0.8660254037844387076, 1.000000000000000000, 0.8660254037844387076, 1.000000000000000000, 0.8660254037844387076, 1.000000000000000000, 0.8660254037844387076, 1.000000000000000000, 0.8660254037844387076, 1.000000000000000000, 0.8660254037844387076, 1.000000000000000000, 0.8660254037844387076, 1.000000000000000000, 0.8660254037844387076, 1.000000000000000000, 0.8660254037844387076, 1.000000000000000000, 0.8660254037844387076, 1.000000000000000000, 0.8660254037844387076, 1.000000000000000000, 0.8660254037844387076, 1.000000000000000000, 0.8660254037844387076, 1.000000000000000000, 0.8660254037844387076, 1.000000000000000000, 0.8660254037844387076, 1.000000000000000000, 0.8660254037844387076, 1.000000000000000000, 0.8660254037844387076, 1.000000000000000000, 0.8660254037844387076, 1.000000000000000000, 0.8660254037844387076, 1.000000000000000000, 0.8660254037844387076, 1.000000000000000000, 0.8660254037844387076, 1.000000000000000000, 0.8660254037844387076, 1.000000000000000000, 0.8660254037844387076, 1.000000000000000000, 0.8660254037844387076, 1.000000000000000000, 0.8660254037844387076, 1.000000000000000000, 0.8660254037844387076, 1.000000000000000000, 0.8660254037844387076, 1.000000000000000000, 0.8660254037844387076, 1.000000000000000000, 0.8660254037844387076, 1.000000000000000000, 0.8660254037844387076, 1.000000000000000000, 0.8660254037844387076, 1.000000000000000000, 0.8660254037844387076, 1.000000000000000000, 0.8660254037844387076, 1.000000000000000000, 0.8660254037844387076, 1.000000000000000000, 0.8660254037844387076, 1.000000000000000000, 0.8660254037844387076, 1.000000000000000000, 0.8660254037844387076, 1.000000000000000000, 0.8660254037844387076, 1.000000000000000000, 0.8660254037844387076, 1.000000000000000000, 0.8660254037844387076, 1.000000000000000000, 0.8660254037844387076, 1.000000000000000000, 0.8660254037844387076, 1.000000000000000000, 0.8660254037844387076, 1.000000000000000000, 0.8660254037844387076, 1.000000000000000000, 0.8660254037844387076, 1.000000000000000000, 0.8660254037844387076, 1.000000000000000000, 0.8660254037844387076, 1.000000000000000000, 0.8660254037844387076, 1.000000000000000000, 0.8660254037844387076, 1.000000000000000000, 0.8660254037844387076, 1.000000000000000000, 0.8660254037844387076, 1.000000000000000000, 0.8660254037844387076, 1.000000000000000000, 0.8660254037844387076, 1.000000000000000000, 0.8660254037844387076, 1.000000000000000000, 0.8660254037844387076, 1.000000000000000000, 0.8660254037844387076, 1.000000000000000000, 0.8660254037844387076, 1.000000000000000000, 0.8660254037844387076, 1.000000000000000000, 0.8660254037844387076, 1.000000000000000000, 0.8660254037844387076, 1.000000000000000000, 0.8660254037844387076, 1.000000000000000000, 0.8660254037844387076, 1.000000000000000000, 0.8660254037844387076, 1.000000000000000000, 0.8660254037844387076, 1.000000000000000000, 0.8660254037844387076, 1.000000000000000000, 0.8660254037844387076, 1.000000000000000000, 0.8660254037844387076, 1.000000000000000000, 0.8660254037844387076, 1.000000000000000000, 0.8660254037844387076, 1.000000000000000000, 0.8660254037844387076, 1.000000000000000000, 0.8660254037844387076, 1.000000000000000000, 0.8660254037844387076, 1.000000000000000000, 0.8660254037844387076, 1.000000000000000000, 0.8660254037844387076, 1.000000000000000000, 0.8660254037844387076, 1.000000000000000000, 0.8660254037844387076, 1.000000000000000000, 0.8660254037844387076, 1.000000000000000000, 0.8660254037844387076, 1.000000000000000000, 0.8660254037844387076, 1.000000000000000000, 0.8660254037844387076, 1.000000000000000000, 0.8660254037844387076, 1.000000000000000000, 0.8660254037844387076, 1.000000000000000000, 0.8660254037844387076, 1.000000000000000000, 0.8660254037844387076, 1.000000000000000000, 0.8660254037844387076, 1.000000000000000000, 0.8660254037844387076, 1.000000000000000000, 0.8660254037844387076, 1.000000000000000000, 0.8660254037844387076, 1.000000000000000000, 0.8660254037844387076, 1.000000000000000000) ) ) 
 REPRESENTATION_ITEM ( '' )  SURFACE ( )  );
#103844 = CARTESIAN_POINT ( 'NONE',  ( 7.036318535368067728, 10.19249347702934294, -1.082531754730537976 ) ) ;
#103846 = CARTESIAN_POINT ( 'NONE',  ( -0.4373225248172925017, -7.723431457505085085, 10.96785329849814339 ) ) ;
#103845 = CARTESIAN_POINT ( 'NONE',  ( 3.455704523497793001, 1.709784277118444162, 1.338028058695311273 ) ) ;
#103848 = CARTESIAN_POINT ( 'NONE',  ( 2.138008341990283778, 0.4048980806483238326, 1.796005048712509655 ) ) ;
#103847 = CARTESIAN_POINT ( 'NONE',  ( -5.965224400332865606, 7.022145224218852455, 1.082531754730549967 ) ) ;
#103849 = CARTESIAN_POINT ( 'NONE',  ( 0.6823417656249899377, 3.426041667008085323, -1.181850606188754593 ) ) ;
#103850 = CARTESIAN_POINT ( 'NONE',  ( 2.947022816757136621, -1.793111998972513277, -1.259777465452505796 ) ) ;
#103851 = CARTESIAN_POINT ( 'NONE',  ( 6.883263157960364254, 3.685033293952295175, 2.667793810733168236 ) ) ;
#103852 = CARTESIAN_POINT ( 'NONE',  ( 4.346707190358800155, 0.5996197433882300976, 2.181559591530066289 ) ) ;
#103853 = CARTESIAN_POINT ( 'NONE',  ( -7.366157530926372488, 7.488271962369228874, -0.7998128361456291469 ) ) ;
#103854 = CARTESIAN_POINT ( 'NONE',  ( 0.6823417656249899377, 5.488541667008087543, -1.181850606188754593 ) ) ;
#103855 = CARTESIAN_POINT ( 'NONE',  ( 6.039396378094620488, 7.052381734106362821, -1.030794243266313082 ) ) ;
#103856 = CARTESIAN_POINT ( 'NONE',  ( 0.7500000000000006661, 13.08333333333333570, 1.299038105676657340 ) ) ;
#103857 = CARTESIAN_POINT ( 'NONE',  ( -6.766928066552171828, 7.067373297165212342, 0.7216878364870317197 ) ) ;
#103858 = CARTESIAN_POINT ( 'NONE',  ( 6.238160076063542725, 6.450477308261824305, -0.7216878364870458196 ) ) ;
#103859 = CARTESIAN_POINT ( 'NONE',  ( 5.835142003873758476, -1.599326089537930873, 0.7579421051841316315 ) ) ;
#103860 = CARTESIAN_POINT ( 'NONE',  ( 3.440093027223433797, -1.200828029685986786, -1.615568007891918789 ) ) ;
#103861 = CARTESIAN_POINT ( 'NONE',  ( 7.151035956204054855, 10.43029348462504124, 1.199719254218460707 ) ) ;
#103862 = CARTESIAN_POINT ( 'NONE',  ( 1.448413646618036399, 2.103543699351087870, 0.1036336169341102176 ) ) ;
#103864 = CARTESIAN_POINT ( 'NONE',  ( 0.7499999999999902300, 2.233333333333351156, 1.299038105676669330 ) ) ;
#103863 = CARTESIAN_POINT ( 'NONE',  ( -8.012344526598182026E-15, 12.04687500034140335, -1.575800808251669460 ) ) ;
#103866 = EDGE_CURVE ( 'NONE', #119366, #90575, #62269, .T. ) ;
#103865 = CARTESIAN_POINT ( 'NONE',  ( 1.943746065852373972, 1.356001085411572049, 1.428673526509681047 ) ) ;
#103867 = FACE_OUTER_BOUND ( 'NONE', #150655, .T. ) ;
#103868 = CARTESIAN_POINT ( 'NONE',  ( -9.367496997601184816, 15.42330868760440410, -7.413898975931886959 ) ) ;
#103870 = ORIENTED_EDGE ( 'NONE', *, *, #32262, .T. ) ;
#103869 = CARTESIAN_POINT ( 'NONE',  ( 5.906502150075481516, -1.803732336900876421, -0.1683732622318224459 ) ) ;
#103871 = CARTESIAN_POINT ( 'NONE',  ( 4.853455804012203778, 8.606189504748821051, 0.7216878364870438212 ) ) ;
#103872 = CARTESIAN_POINT ( 'NONE',  ( 0.6823417656249882723, -0.3447916663252489911, 1.181850606188755259 ) ) ;
#103873 = EDGE_CURVE ( 'NONE', #206877, #22516, #77028, .T. ) ;
#103874 = CARTESIAN_POINT ( 'NONE',  ( 4.944154083221364182, 1.865701114312174225, 0.1370711555178441010 ) ) ;
#103875 = CARTESIAN_POINT ( 'NONE',  ( 5.787960296632533641, -1.308950758395693414, -1.603975846202657429 ) ) ;
#103876 = CARTESIAN_POINT ( 'NONE',  ( -0.6125000000000262457, 2.791666666666692276, 1.060881119635882497 ) ) ;
#103877 = CARTESIAN_POINT ( 'NONE',  ( -4.434925645001610128, 8.188180662561590495, 0.7216878364870338292 ) ) ;
#103878 = CARTESIAN_POINT ( 'NONE',  ( -0.02338929933905827679, 0.006294950389555676457, -1.710968156697997289 ) ) ;
#103879 = CARTESIAN_POINT ( 'NONE',  ( -1.500000000000015099, 0.8791666666666874130, -0.8660254037844313801 ) ) ;
#103880 = CARTESIAN_POINT ( 'NONE',  ( 8.423693512792301163, 8.722063941212843119, 0.7998128361456481317 ) ) ;
#103881 = CARTESIAN_POINT ( 'NONE',  ( -7.655550293210764856, 12.08322577538792331, 0.000000000000000000 ) ) ;
#103882 = CARTESIAN_POINT ( 'NONE',  ( 7.015418140428412386, 7.149352350113456822, 0.7998128361456331437 ) ) ;
#103883 = CARTESIAN_POINT ( 'NONE',  ( -0.6823417656250003738, -0.2822916663252489355, -1.181850606188749264 ) ) ;
#103885 = EDGE_CURVE ( 'NONE', #97759, #71636, #13088, .T. ) ;
#103884 = CARTESIAN_POINT ( 'NONE',  ( -0.7500000000000006661, 1.108333333333356929, -1.299038105676652011 ) ) ;
#103887 = CARTESIAN_POINT ( 'NONE',  ( 6.159481859310094620, 6.080483678816896109, 1.040834085586084257E-14 ) ) ;
#103886 = CARTESIAN_POINT ( 'NONE',  ( 5.090269282739749102, 1.010147525469132557, -1.681691772506640481 ) ) ;
#103888 = CARTESIAN_POINT ( 'NONE',  ( 2.970077202574809228, 1.701686883299750264, 1.080900613174784475 ) ) ;
#103889 = CARTESIAN_POINT ( 'NONE',  ( 2.044013137410850778, 0.8228895493161382246, 1.730149048491230301 ) ) ;
#103890 = CARTESIAN_POINT ( 'NONE',  ( 0.000000000000000000, 8.500000000000000000, 0.000000000000000000 ) ) ;
#103891 = CARTESIAN_POINT ( 'NONE',  ( 0.8904706703079521279, -0.5376514911656914419, -2.124458794526106864 ) ) ;
#103892 = CARTESIAN_POINT ( 'NONE',  ( -11.80235830595197655, 9.799999999999982947, 1.696088231482817399 ) ) ;
#103893 = CARTESIAN_POINT ( 'NONE',  ( 2.635844295777586943, 0.8854499327175249235, -1.647724587607077851 ) ) ;
#103894 = CARTESIAN_POINT ( 'NONE',  ( 0.6823417656249917140, 5.092708333674749177, 1.181850606188765695 ) ) ;
#103895 = CARTESIAN_POINT ( 'NONE',  ( 4.271743731491533858, 0.4368499997736470797, -1.965098791395853750 ) ) ;
#103896 = B_SPLINE_CURVE_WITH_KNOTS ( 'NONE', 3,
 ( #147689, #133597, #134657, #316, #98935, #66387, #116299, #64297, #196430, #81604, #213706, #65330, #99992, #16580, #180184, #150891, #18719, #131477, #130443, #97883, #197480, #1391, #149820, #132535, #182290, #164990, #184426, #48075, #33916, #181232, #68529, #32860, #166058, #17644, #51245, #117371, #183368, #34972, #114186, #101044, #84803, #2453, #200660, #52309, #118439, #36043, #102123, #19791, #146641, #71730, #70659, #90163, #136769, #103194, #169257, #6734, #151951, #20843, #138914, #107527, #156229, #106449, #56585, #7806, #137842, #120589, #86942, #153008, #73899, #4585, #21901, #204934, #54447, #39258, #40343, #139992, #121663, #206013, #202797, #88011, #3521, #186567, #69593, #37116, #38195, #154082, #171389, #5649, #24060, #122744, #188707, #170313, #155152, #57648, #172472, #203864, #123808, #189768, #22980, #135703, #119505, #104267, #201729, #41420, #55509, #187631, #105352, #173558, #89099, #72813, #85873, #53370, #185490, #142129, #94437, #91233, #43551, #61912, #78150, #158357, #145340, #160476, #111797, #211341, #58711, #207079, #79222, #9950, #109672, #141072, #112860, #210274, #190824, #174622, #124860, #159406, #175674, #144280, #93370, #42485, #46747, #194030, #62965, #11005, #74962, #128074, #45680, #27262, #77082, #26198, #177802, #29419, #25131, #76026, #95510, #161557, #143210, #209200, #208142, #60840, #127001, #59772, #125931, #157293, #176728, #8883, #192960, #108594, #191889, #44612, #110728, #92314, #28341, #12083, #13146, #129135, #195111, #202274, #30487, #84282, #100534, #137325, #169800, #133073, #83203, #52851, #53925, #101601, #21389, #4072, #183914, #200148, #99475, #67999, #165534, #118986, #1939, #120062, #116843, #36590, #134141, #203341, #37673, #54994, #166609, #17127, #150369, #182844, #102677, #87498, #35525, #51802, #167669, #19270, #149284, #865, #199071, #50718, #34462 ),
 .UNSPECIFIED., .F., .F.,
 ( 4, 1, 1, 1, 1, 1, 1, 1, 1, 1, 1, 1, 1, 1, 1, 1, 1, 1, 1, 1, 1, 1, 1, 1, 1, 1, 1, 1, 1, 1, 1, 1, 1, 1, 1, 1, 1, 1, 1, 1, 1, 1, 1, 1, 1, 1, 1, 1, 1, 1, 1, 1, 1, 1, 1, 1, 1, 1, 1, 1, 1, 1, 1, 1, 1, 1, 1, 1, 1, 1, 1, 1, 1, 1, 1, 1, 1, 1, 1, 1, 1, 1, 1, 1, 1, 1, 1, 1, 1, 1, 1, 1, 1, 1, 1, 1, 1, 1, 1, 1, 1, 1, 1, 1, 1, 1, 1, 1, 1, 1, 1, 1, 1, 1, 1, 1, 1, 1, 1, 1, 1, 1, 1, 1, 1, 1, 1, 1, 1, 1, 1, 1, 1, 1, 1, 1, 1, 1, 1, 1, 1, 1, 1, 1, 1, 1, 1, 1, 1, 1, 1, 1, 1, 1, 1, 1, 1, 1, 1, 1, 1, 1, 1, 1, 1, 1, 1, 1, 1, 1, 1, 1, 1, 1, 1, 1, 1, 1, 1, 1, 1, 1, 1, 1, 1, 1, 1, 1, 1, 1, 1, 1, 1, 1, 1, 1, 1, 1, 1, 1, 1, 1, 1, 1, 1, 1, 1, 1, 1, 1, 1, 1, 1, 1, 1, 1, 4 ),
 ( 0.000000000000000000, 0.004629629629629626771, 0.009259259259259253541, 0.01388888888888887771, 0.01851851851851850361, 0.02314814814814812952, 0.02777777777777775542, 0.03240740740740737785, 0.03703703703703700723, 0.04166666666666662966, 0.04629629629629625903, 0.05092592592592588147, 0.05555555555555549696, 0.06018518518518511939, 0.06481481481481474183, 0.06944444444444436426, 0.07407407407407398670, 0.07870370370370359525, 0.08333333333333321769, 0.08796296296296284012, 0.09259259259259246255, 0.09722222222222209886, 0.1018518518518517213, 0.1064814814814813299, 0.1111111111111109523, 0.1157407407407405747, 0.1203703703703701972, 0.1249999999999998196, 0.1296296296296294281, 0.1342592592592590506, 0.1388888888888886730, 0.1435185185185182954, 0.1481481481481479179, 0.1527777777777775403, 0.1574074074074071627, 0.1620370370370367852, 0.1666666666666664076, 0.1712962962962960300, 0.1759259259259256525, 0.1805555555555552749, 0.1851851851851848973, 0.1898148148148145198, 0.1944444444444441145, 0.1990740740740737091, 0.2037037037037033038, 0.2083333333333328985, 0.2129629629629625209, 0.2175925925925921156, 0.2222222222222217103, 0.2268518518518513050, 0.2314814814814808996, 0.2361111111111104943, 0.2407407407407401168, 0.2453703703703697114, 0.2499999999999993061, 0.2546296296296289285, 0.2592592592592585232, 0.2638888888888881179, 0.2685185185185177126, 0.2731481481481473073, 0.2777777777777769019, 0.2824074074074064966, 0.2870370370370360913, 0.2916666666666656860, 0.2962962962962952806, 0.3009259259259249308, 0.3055555555555545255, 0.3101851851851841202, 0.3148148148148137149, 0.3194444444444433095, 0.3240740740740729042, 0.3287037037037024989, 0.3333333333333320936, 0.3379629629629616883, 0.3425925925925912829, 0.3472222222222209331, 0.3518518518518505278, 0.3564814814814801225, 0.3611111111111097172, 0.3657407407407393118, 0.3703703703703689065, 0.3749999999999985567, 0.3796296296296282069, 0.3842592592592578571, 0.3888888888888874518, 0.3935185185185171020, 0.3981481481481467521, 0.4027777777777764023, 0.4074074074074060525, 0.4120370370370357027, 0.4166666666666652974, 0.4212962962962949476, 0.4259259259259245978, 0.4305555555555542480, 0.4351851851851838981, 0.4398148148148135483, 0.4444444444444431430, 0.4490740740740727932, 0.4537037037037024434, 0.4583333333333320936, 0.4629629629629617438, 0.4675925925925913940, 0.4722222222222209886, 0.4768518518518506388, 0.4814814814814802890, 0.4861111111111099392, 0.4907407407407395894, 0.4953703703703692396, 0.4999999999999988898, 0.5046296296296285400, 0.5092592592592581902, 0.5138888888888878403, 0.5185185185185173795, 0.5231481481481470297, 0.5277777777777766799, 0.5324074074074063301, 0.5370370370370359803, 0.5416666666666656305, 0.5462962962962952806, 0.5509259259259249308, 0.5555555555555545810, 0.5601851851851842312, 0.5648148148148138814, 0.5694444444444435316, 0.5740740740740730708, 0.5787037037037027210, 0.5833333333333323711, 0.5879629629629620213, 0.5925925925925916715, 0.5972222222222213217, 0.6018518518518509719, 0.6064814814814806221, 0.6111111111111102723, 0.6157407407407399225, 0.6203703703703695727, 0.6249999999999992228, 0.6296296296296287620, 0.6342592592592584122, 0.6388888888888880624, 0.6435185185185177126, 0.6481481481481473628, 0.6527777777777770130, 0.6574074074074066631, 0.6620370370370363133, 0.6666666666666659635, 0.6712962962962956137, 0.6759259259259252639, 0.6805555555555549141, 0.6851851851851845643, 0.6898148148148141034, 0.6944444444444437536, 0.6990740740740734038, 0.7037037037037030540, 0.7083333333333327042, 0.7129629629629623544, 0.7175925925925920046, 0.7222222222222216548, 0.7268518518518513050, 0.7314814814814809552, 0.7361111111111106053, 0.7407407407407402555, 0.7453703703703697947, 0.7499999999999994449, 0.7546296296296290951, 0.7592592592592586342, 0.7638888888888882844, 0.7685185185185179346, 0.7731481481481475848, 0.7777777777777772350, 0.7824074074074068852, 0.7870370370370365354, 0.7916666666666661856, 0.7962962962962958358, 0.8009259259259254859, 0.8055555555555551361, 0.8101851851851847863, 0.8148148148148143255, 0.8194444444444439757, 0.8240740740740736259, 0.8287037037037032761, 0.8333333333333329263, 0.8379629629629625764, 0.8425925925925922266, 0.8472222222222218768, 0.8518518518518515270, 0.8564814814814811772, 0.8611111111111108274, 0.8657407407407404776, 0.8703703703703701278, 0.8749999999999996669, 0.8796296296296293171, 0.8842592592592589673, 0.8888888888888886175, 0.8935185185185182677, 0.8981481481481479179, 0.9027777777777775681, 0.9074074074074072183, 0.9120370370370368684, 0.9166666666666665186, 0.9212962962962961688, 0.9259259259259258190, 0.9305555555555553582, 0.9351851851851850084, 0.9398148148148146586, 0.9444444444444443088, 0.9490740740740739589, 0.9537037037037036091, 0.9583333333333332593, 0.9629629629629629095, 0.9675925925925925597, 0.9722222222222222099, 0.9768518518518518601, 0.9814814814814815103, 0.9861111111111110494, 0.9907407407407406996, 0.9953703703703703498, 1.000000000000000000 ),
 .UNSPECIFIED. ) ;
#103897 = CARTESIAN_POINT ( 'NONE',  ( -8.134002093194872884, 11.57708731111429401, 1.199719254218453823 ) ) ;
#103899 = CARTESIAN_POINT ( 'NONE',  ( 4.306348207420813701, 1.301105652591315387, -1.670210365991892987 ) ) ;
#103898 = CARTESIAN_POINT ( 'NONE',  ( -4.717874267875590277, 7.487641831621378863, 1.082531754730560403 ) ) ;
#103900 = CARTESIAN_POINT ( 'NONE',  ( -15.75000000000000000, 13.79999999999998295, 1.799999999999999600 ) ) ;
#103901 = CARTESIAN_POINT ( 'NONE',  ( 6.021949436824264978, 2.040384406434097464, -0.3501103912618847014 ) ) ;
#103903 = CARTESIAN_POINT ( 'NONE',  ( 6.720655732516620517, 2.957990990047154600, 2.526349433132681011 ) ) ;
#103902 = CARTESIAN_POINT ( 'NONE',  ( 1.206708187092224716, 1.845608279032302512, 0.9822807542516975854 ) ) ;
#103905 = ORIENTED_EDGE ( 'NONE', *, *, #182674, .F. ) ;
#103904 = CARTESIAN_POINT ( 'NONE',  ( 6.686557121163758666, -1.791048715316777562, -0.3524728914669760793 ) ) ;
#103906 = CARTESIAN_POINT ( 'NONE',  ( 6.751070424600909448, 9.963667031088037973, -1.199719254218441611 ) ) ;
#103907 = CARTESIAN_POINT ( 'NONE',  ( 7.796438949605505542, -6.657020681837042986, -7.586009164902113078 ) ) ;
#103908 = CARTESIAN_POINT ( 'NONE',  ( 9.710969956560674632, 13.29837910982962690, -8.127984515541683663 ) ) ;
#103909 = CARTESIAN_POINT ( 'NONE',  ( -9.348561386651960348, 5.000000000000002665, 7.001914024036568485 ) ) ;
#103911 = CARTESIAN_POINT ( 'NONE',  ( 7.253248993186731219, 8.524840582548424806, 1.082531754730558626 ) ) ;
#103910 = CARTESIAN_POINT ( 'NONE',  ( 5.784525094524856748, 9.900363043587685041, 1.040834085586084257E-14 ) ) ;
#103912 = CARTESIAN_POINT ( 'NONE',  ( -1.902112725515587632, 3.289212146679059146, 0.4096023912811905809 ) ) ;
#103913 = CARTESIAN_POINT ( 'NONE',  ( 0.2756360753965527155, 1.792041154956749871, -0.2637626551888968551 ) ) ;
#103914 = CARTESIAN_POINT ( 'NONE',  ( -8.507905087775398556, 9.884643009614800135, 1.199719254218462483 ) ) ;
#103915 = CARTESIAN_POINT ( 'NONE',  ( 6.193377243344257543, 6.120028293523423812, -0.7998128361456281477 ) ) ;
#103916 = B_SPLINE_CURVE_WITH_KNOTS ( 'NONE', 3,
 ( #144123, #194951, #28187, #128972, #45525, #63883 ),
 .UNSPECIFIED., .F., .F.,
 ( 4, 2, 4 ),
 ( 0.000000000000000000, 0.001226111284895915884, 0.002452222569791831334 ),
 .UNSPECIFIED. ) ;
#103917 = CARTESIAN_POINT ( 'NONE',  ( 0.2680151545362241539, -6.654245765634851928, 10.99740610014212550 ) ) ;
#103918 = CARTESIAN_POINT ( 'NONE',  ( 2.372313692266983853, 5.711523707712699682, 0.7216878364870438212 ) ) ;
#103919 = CARTESIAN_POINT ( 'NONE',  ( -10.62873463776380056, 11.29999999999998117, 3.199999999999997957 ) ) ;
#103920 = CARTESIAN_POINT ( 'NONE',  ( 2.900554798319789906, 5.471398800426671372, 1.199719254218452047 ) ) ;
#103921 = ORIENTED_EDGE ( 'NONE', *, *, #57944, .T. ) ;
#103922 =( GEOMETRIC_REPRESENTATION_CONTEXT ( 3 ) GLOBAL_UNCERTAINTY_ASSIGNED_CONTEXT ( ( #31342 ) ) GLOBAL_UNIT_ASSIGNED_CONTEXT ( ( #63187, #33878, #150854 ) ) REPRESENTATION_CONTEXT ( 'NONE', 'WORKASPACE' ) );
#103923 = CARTESIAN_POINT ( 'NONE',  ( 6.591432905763006111, -0.4393008961055907546, 1.975236973087670656 ) ) ;
#103924 = CARTESIAN_POINT ( 'NONE',  ( 0.1180496341894651385, -0.5612577129426484790, 2.044807062438446454 ) ) ;
#103925 = DIRECTION ( 'NONE',  ( 0.000000000000000000, 0.000000000000000000, -1.000000000000000000 ) ) ;
#103926 = DIRECTION ( 'NONE',  ( 0.000000000000000000, -1.000000000000000000, 0.000000000000000000 ) ) ;
#103927 = CARTESIAN_POINT ( 'NONE',  ( -3.945059511896602089, 7.546393830613923548, 1.040834085586084257E-14 ) ) ;
#103928 = CARTESIAN_POINT ( 'NONE',  ( 4.207107738942202246, 3.802713871720993399, 1.214306433183764966E-14 ) ) ;
#103929 = CARTESIAN_POINT ( 'NONE',  ( 2.957809129533952142, -0.6224678976109696560, 1.868526426519439898 ) ) ;
#103930 = EDGE_CURVE ( 'NONE', #31992, #56290, #121398, .T. ) ;
#103931 = CARTESIAN_POINT ( 'NONE',  ( 4.640250013031629095, 0.7743308749140092040, 1.862011755488258480 ) ) ;
#103932 = CARTESIAN_POINT ( 'NONE',  ( -7.230575994789712801, 7.330093503543126054, 0.7998128361456341429 ) ) ;
#103933 = CARTESIAN_POINT ( 'NONE',  ( -2.324088772396477673E-16, -2.143749999044084031, -3.475000000000000089 ) ) ;
#103934 = CARTESIAN_POINT ( 'NONE',  ( -10.93020303578476415, -8.258458176070773149, 0.1907874036681941887 ) ) ;
#103935 = CARTESIAN_POINT ( 'NONE',  ( 4.558633756138521065, -1.956834287480881063, -0.9866608250781592204 ) ) ;
#103936 = CARTESIAN_POINT ( 'NONE',  ( 0.9486429539237064557, 2.980410930033766448, -1.028101543438967758 ) ) ;
#103937 = CARTESIAN_POINT ( 'NONE',  ( 2.854421793556624731, 0.6472853923233500284, 1.814523859438036624 ) ) ;
#103938 = CARTESIAN_POINT ( 'NONE',  ( -6.645467848992654858, 10.90479625713344625, 0.7998128361456481317 ) ) ;
#103939 = EDGE_CURVE ( 'NONE', #40528, #3320, #172210, .T. ) ;
#103940 = CARTESIAN_POINT ( 'NONE',  ( -0.02988540731097348233, 2.061246921799511966, -2.144091820287073791 ) ) ;
#103941 = CARTESIAN_POINT ( 'NONE',  ( 0.2412292383832773390, 0.3817025157030576321, 2.173470055567463088 ) ) ;
#103942 = CARTESIAN_POINT ( 'NONE',  ( 10.95308175811721085, 11.29999999999998117, 1.799999999999999600 ) ) ;
#103943 = EDGE_LOOP ( 'NONE', ( #79158, #119377, #159598, #192403 ) ) ;
#103944 = CARTESIAN_POINT ( 'NONE',  ( 3.770576118376306241, 6.452737000530752276, 1.082531754730549078 ) ) ;
#103945 = CARTESIAN_POINT ( 'NONE',  ( 5.612145322048014862, 1.967363499941950034, -0.09270071294615632451 ) ) ;
#103946 = VERTEX_POINT ( 'NONE', #118544 ) ;
#103948 = CARTESIAN_POINT ( 'NONE',  ( 3.985024600404694972, -1.879186454625543901, -0.7224040237710227519 ) ) ;
#103947 = CARTESIAN_POINT ( 'NONE',  ( 0.2396544122938427390, 1.936909983681795344, 0.1419545801408238772 ) ) ;
#103949 = CARTESIAN_POINT ( 'NONE',  ( 5.870575887392723402, -0.5666052741825926553, 2.227357739769205924 ) ) ;
#103950 = CARTESIAN_POINT ( 'NONE',  ( 4.821077630544555070, -1.661119493813640657, -0.8391380156763434961 ) ) ;
#103951 = CARTESIAN_POINT ( 'NONE',  ( 6.851666526859736983, 9.086973262793417661, -1.599625672291269396 ) ) ;
#103952 = DIRECTION ( 'NONE',  ( 0.000000000000000000, -1.000000000000000000, 0.000000000000000000 ) ) ;
#103953 = CARTESIAN_POINT ( 'NONE',  ( -5.856232286098998152, 8.919689202835742847, 1.199719254218452047 ) ) ;
#103954 = CARTESIAN_POINT ( 'NONE',  ( -3.187575512988701565, 6.732938841879847480, 0.000000000000000000 ) ) ;
#103955 = CARTESIAN_POINT ( 'NONE',  ( 0.5038066827526345159, -2.180447833630628107, 0.2205874978757973448 ) ) ;
#103956 = CARTESIAN_POINT ( 'NONE',  ( 4.799223189557548785, 7.582548906917042864, -1.082531754730549078 ) ) ;
#103957 = ORIENTED_EDGE ( 'NONE', *, *, #80728, .F. ) ;
#103958 = PLANE ( 'NONE',  #39693 ) ;
#103959 = DIRECTION ( 'NONE',  ( -3.491481338843133355E-15, 0.000000000000000000, -1.000000000000000000 ) ) ;
#103960 = CARTESIAN_POINT ( 'NONE',  ( 0.02954982209854748257, -1.120125052174587577, -1.442194003765177257 ) ) ;
#103961 = CARTESIAN_POINT ( 'NONE',  ( -3.785751206713858785, 5.439795712631356750, 1.599625672291267398 ) ) ;
#103962 = AXIS2_PLACEMENT_3D ( 'NONE', #194581, #163167, #114472 ) ;
#103963 = CARTESIAN_POINT ( 'NONE',  ( 2.724952806592676691, 1.721339412077933284, 0.2094855716100688936 ) ) ;
#103964 = CARTESIAN_POINT ( 'NONE',  ( -5.438229012412899799, 7.437962829272074750, -1.443375672974066770 ) ) ;
#103965 = CARTESIAN_POINT ( 'NONE',  ( 6.509000000000034980, 7.629137130509102249, 2.499999999999994227 ) ) ;
#103966 = CARTESIAN_POINT ( 'NONE',  ( -5.148345644887285744, 7.029489223833707001, -1.599625672291256295 ) ) ;
#103967 = DIRECTION ( 'NONE',  ( 0.6507913734559650498, 0.7592566023652995710, -0.000000000000000000 ) ) ;
#103968 = CARTESIAN_POINT ( 'NONE',  ( 0.6728209460903146200, 1.430239379376567976, -1.496996390900617646 ) ) ;
#103969 = CARTESIAN_POINT ( 'NONE',  ( 5.602125774977974260, -1.825872481414937853, 0.004271240736861136277 ) ) ;
#103970 = CARTESIAN_POINT ( 'NONE',  ( 3.643363735869999509, 1.775428317022755609, -0.8347113108059035502 ) ) ;
#103971 = CARTESIAN_POINT ( 'NONE',  ( 1.224999999999949241, -0.2916666659838533793, -0.7072540797573176885 ) ) ;
#103972 = CARTESIAN_POINT ( 'NONE',  ( -8.962103233833181193, 10.41454084668224489, -1.199719254218446718 ) ) ;
#103973 = CARTESIAN_POINT ( 'NONE',  ( 7.613066949273408213, 8.840665181362512115, -1.199719254218441611 ) ) ;
#103974 = CARTESIAN_POINT ( 'NONE',  ( 3.510498622083501719, -2.118129049236017192, -0.1023006277712720374 ) ) ;
#103975 = CARTESIAN_POINT ( 'NONE',  ( 6.505933609711257226, 8.683618192786854095, -1.599625672291281386 ) ) ;
#103976 = CARTESIAN_POINT ( 'NONE',  ( -8.890396042259075315, 11.39521468743417998, -1.599625672291263179 ) ) ;
#103977 = CARTESIAN_POINT ( 'NONE',  ( 1.551716534671506498, 1.565040117424065347, 1.355267069636761912 ) ) ;
#103979 = CARTESIAN_POINT ( 'NONE',  ( -0.7500000000000006661, 14.98958333401613530, -1.299038105676657340 ) ) ;
#103978 = CARTESIAN_POINT ( 'NONE',  ( 6.827182134110209688, 6.038954451951505042, 2.405852596708078384 ) ) ;
#103981 = VERTEX_POINT ( 'NONE', #100099 ) ;
#103980 = CARTESIAN_POINT ( 'NONE',  ( 4.951916289638909063, -1.570117426187572107, -1.571520405092931005 ) ) ;
#103982 = CARTESIAN_POINT ( 'NONE',  ( 1.547921954348607354, -1.621480451111120047, 1.629585861659810009 ) ) ;
#103983 = CARTESIAN_POINT ( 'NONE',  ( 9.598809568795314107, 10.30095870645710754, -0.7216878364870257245 ) ) ;
#103985 = CARTESIAN_POINT ( 'NONE',  ( 3.285556943750000070, -3.784374999522041705, 0.000000000000000000 ) ) ;
#103984 = CARTESIAN_POINT ( 'NONE',  ( 4.415115299905642665, 5.179997933758551554, -1.199719254218450271 ) ) ;
#103986 = CARTESIAN_POINT ( 'NONE',  ( 0.000000000000000000, 0.000000000000000000, 0.000000000000000000 ) ) ;
#103987 = EDGE_LOOP ( 'NONE', ( #137822, #88801, #38896, #45736, #168439, #81403, #46944, #188037 ) ) ;
#103988 = CARTESIAN_POINT ( 'NONE',  ( -5.547286221698657371, 6.226642220600762556, -0.9388435239387061815 ) ) ;
#103989 = CARTESIAN_POINT ( 'NONE',  ( 3.023589307540079041, -0.3687504995396119201, 1.876329818327879817 ) ) ;
#103990 = CARTESIAN_POINT ( 'NONE',  ( -0.3895070363647045175, 6.983478840415547673, -3.944638453887328922 ) ) ;
#103991 = CARTESIAN_POINT ( 'NONE',  ( 3.785938739704467260, -0.8500231715772713637, 1.500685565699668933 ) ) ;
#103992 = CARTESIAN_POINT ( 'NONE',  ( 2.430875351317234756, -1.673853735218135741, 1.124246214196801485 ) ) ;
#103993 = CARTESIAN_POINT ( 'NONE',  ( 3.446149177467156655, -2.027825264502993718, -1.082511230532481106 ) ) ;
#103994 = CARTESIAN_POINT ( 'NONE',  ( 3.796368952254399964, -2.259583311708447617, -0.1157369865004975740 ) ) ;
#103995 = CARTESIAN_POINT ( 'NONE',  ( 6.340466044077378349, 2.082889313809291654, 0.3107213310214774760 ) ) ;
#103996 = CARTESIAN_POINT ( 'NONE',  ( -4.489158259900630554, 8.251452046610447510, 0.000000000000000000 ) ) ;
#103997 = ORIENTED_EDGE ( 'NONE', *, *, #177848, .F. ) ;
#103998 = CARTESIAN_POINT ( 'NONE',  ( 4.586996685387556560, 1.581260375356493331, -0.7947977318805318214 ) ) ;
#104000 = CARTESIAN_POINT ( 'NONE',  ( 0.2876181914312899157, 1.702867465475272901, 1.534690983289775712 ) ) ;
#103999 = CARTESIAN_POINT ( 'NONE',  ( 5.501576472095266901, 9.640532660744973725, -0.7998128361456481317 ) ) ;
#104001 = CARTESIAN_POINT ( 'NONE',  ( 5.630750141678076304, -1.662707896839428434, 0.7909858098210584831 ) ) ;
#104002 = CARTESIAN_POINT ( 'NONE',  ( -4.485049888022365927, 4.126979712314507331, 0.7998128361456341429 ) ) ;
#104003 = CARTESIAN_POINT ( 'NONE',  ( 5.947271710577298975, 0.6394180277670692414, -2.096098967930816848 ) ) ;
#104004 = CARTESIAN_POINT ( 'NONE',  ( -5.764151584465413869, 6.753873599078290546, -1.199719254218453823 ) ) ;
#104005 = CARTESIAN_POINT ( 'NONE',  ( 1.360316468749957597, -0.2239583329919110355, 0.7853790794158921340 ) ) ;
#104006 = CARTESIAN_POINT ( 'NONE',  ( -9.367496997397941172, 15.46908218389366851, 7.500000000249372079 ) ) ;
#104007 = CARTESIAN_POINT ( 'NONE',  ( 6.004363041306050697, 2.067815565686380364, 0.1054426792976848049 ) ) ;
#104008 = CARTESIAN_POINT ( 'NONE',  ( 1.007046422456716384, -0.04465021774549028655, 2.016188868504041665 ) ) ;
#104009 = CARTESIAN_POINT ( 'NONE',  ( -1.201851678989727383E-14, 5.446875000341422357, -1.575800808251660134 ) ) ;
#104010 = CARTESIAN_POINT ( 'NONE',  ( 4.090394749938445429, -1.905694808957728137, -0.2815942358586983607 ) ) ;
#104011 = CARTESIAN_POINT ( 'NONE',  ( 1.364683531250000303, 11.25520833367473550, -0.7879004041258355073 ) ) ;
#104012 = CARTESIAN_POINT ( 'NONE',  ( 0.9673671849170182302, -1.746833394359051495, 1.372194155552537431 ) ) ;
#104013 = VERTEX_POINT ( 'NONE', #101149 ) ;
#104015 = CARTESIAN_POINT ( 'NONE',  ( -1.284279953904156280, 3.202889714876734573, 0.7750000000000117906 ) ) ;
#104014 = CARTESIAN_POINT ( 'NONE',  ( 1.203941962966152968, 3.008481847795084541, -0.7749999999999840350 ) ) ;
#104016 = CARTESIAN_POINT ( 'NONE',  ( 1.499999999999959588, 6.999999999999999112, -10.89724735885168805 ) ) ;
#104017 = CARTESIAN_POINT ( 'NONE',  ( 4.878236342818665250, 4.585697242910212523, 1.040834085586084257E-14 ) ) ;
#104018 = CARTESIAN_POINT ( 'NONE',  ( 0.000000000000000000, -9.999999999999994671, 10.99999999999999112 ) ) ;
#104019 = CARTESIAN_POINT ( 'NONE',  ( 3.825523041098664034, 0.9271419989833797892, -1.472723941875812237 ) ) ;
#104020 = CARTESIAN_POINT ( 'NONE',  ( 2.523818479427087702, 1.924573107942130656, -0.3798230296482503210 ) ) ;
#104022 = CARTESIAN_POINT ( 'NONE',  ( 1.364683531249988535, 3.176041667008084435, 0.7879004041258500513 ) ) ;
#104021 = CARTESIAN_POINT ( 'NONE',  ( 4.299907273828439180, 8.168308919441841454, 1.040834085586084257E-14 ) ) ;
#104023 = CARTESIAN_POINT ( 'NONE',  ( -4.595282798756362475, 6.958845989550745514, 1.192800718855389297 ) ) ;
#104024 = CARTESIAN_POINT ( 'NONE',  ( 8.920375002787457319, 12.49452237230570084, 1.199719254218450271 ) ) ;
#104025 = CARTESIAN_POINT ( 'NONE',  ( 6.303176765056641706, -1.658072099422291057, 1.048360225930293321 ) ) ;
#104026 = CARTESIAN_POINT ( 'NONE',  ( -7.862839020921525091, 11.26073039346208660, -1.199719254218446718 ) ) ;
#104027 = CIRCLE ( 'NONE', #83280, 12.00000000000000178 ) ;
#104028 = CARTESIAN_POINT ( 'NONE',  ( -5.721177634842498527, 5.777054783512106440, 0.000000000000000000 ) ) ;
#104029 = CARTESIAN_POINT ( 'NONE',  ( 5.067592334412735156, 1.357865985192594271, 1.490972259599515848 ) ) ;
#104030 = CARTESIAN_POINT ( 'NONE',  ( 0.9719599696450488269, 2.179858136331577434, -0.6057951801161051142 ) ) ;
#104032 = ORIENTED_EDGE ( 'NONE', *, *, #211265, .T. ) ;
#104031 = CARTESIAN_POINT ( 'NONE',  ( -6.124532705071231931, 8.168374127381657246, -1.599625672291263179 ) ) ;
#104033 = CARTESIAN_POINT ( 'NONE',  ( 1.364683531249992088, 5.634375000341417916, 1.214306433183764966E-14 ) ) ;
#104034 = CARTESIAN_POINT ( 'NONE',  ( 1.633845377418343237, 0.9265681688636999702, -1.624882239709434018 ) ) ;
#104035 = CARTESIAN_POINT ( 'NONE',  ( 0.5450593487147866734, -1.257523079656326148, 1.194353625382915673 ) ) ;
#104037 = CARTESIAN_POINT ( 'NONE',  ( 4.107102485094754840, -0.3736803571842538529, 2.159302612355806339 ) ) ;
#104036 = CARTESIAN_POINT ( 'NONE',  ( 1.360316468749957597, 1.265625000341379147, -5.030698080332740574E-14 ) ) ;
#104038 = CARTESIAN_POINT ( 'NONE',  ( 6.141700272255690152, -1.665644196019906875, -1.597301777034014991 ) ) ;
#104039 = CARTESIAN_POINT ( 'NONE',  ( 0.6200826401135750565, -1.101877700393244952, -1.741386573944928795 ) ) ;
#104040 = CARTESIAN_POINT ( 'NONE',  ( 2.976435162280165247, -0.1435924003432750840, -1.936700533151126891 ) ) ;
#104041 = CARTESIAN_POINT ( 'NONE',  ( -3.578989363883261277, 7.119311991265024453, 1.040834085586084257E-14 ) ) ;
#104042 = ADVANCED_FACE ( 'NONE', ( #152056 ), #143509, .T. ) ;
#104043 = CARTESIAN_POINT ( 'NONE',  ( 1.403499169903363875, 7.376709478542918141, -4.304123474984290709 ) ) ;
#104044 = CARTESIAN_POINT ( 'NONE',  ( 4.421367491832270957, 6.251624388594711590, 1.443375672974058777 ) ) ;
#104045 = CARTESIAN_POINT ( 'NONE',  ( 5.151017605526480025, 0.9962996879465220168, 1.753031629501592192 ) ) ;
#104046 = CARTESIAN_POINT ( 'NONE',  ( -4.324687812634898876, 6.068555086205916105, 1.443375672974064550 ) ) ;
#104047 = CARTESIAN_POINT ( 'NONE',  ( -6.038177310039794854, 8.137902509836795417, -1.599625672291271394 ) ) ;
#104048 = CARTESIAN_POINT ( 'NONE',  ( 8.609591239877852686, 10.00327685373437347, -1.199719254218445830 ) ) ;
#104050 = CARTESIAN_POINT ( 'NONE',  ( -6.949550370341250449, -6.532648880269213088, 6.447678837262236229 ) ) ;
#104049 = CARTESIAN_POINT ( 'NONE',  ( 0.8381832108898427114, 1.798179982845280467, 0.3147962740308178353 ) ) ;
#104051 = CARTESIAN_POINT ( 'NONE',  ( -5.041653019435350380, 6.975290837464928728, -1.599625672291271394 ) ) ;
#104052 = CARTESIAN_POINT ( 'NONE',  ( -4.305596300791617814, 7.180890229968955651, 1.199719254218452935 ) ) ;
#104053 = CARTESIAN_POINT ( 'NONE',  ( -11.55001508359621987, 4.031797291955615314, 5.408777164504234847 ) ) ;
#104054 = EDGE_LOOP ( 'NONE', ( #202429, #176779 ) ) ;
#104055 = CARTESIAN_POINT ( 'NONE',  ( 6.455941844152293996, 2.055567607077302128, -0.1488206295068068841 ) ) ;
#104056 = CARTESIAN_POINT ( 'NONE',  ( -6.929625909916163451, 7.257187447756535903, 0.7216878364870317197 ) ) ;
#104057 = CARTESIAN_POINT ( 'NONE',  ( -2.927671105547157371, 5.503034492191895666, 1.199719254218462483 ) ) ;
#104058 = CARTESIAN_POINT ( 'NONE',  ( -4.067937748088393590, 7.725456827083305278, 0.6547958487484796253 ) ) ;
#104059 = CARTESIAN_POINT ( 'NONE',  ( 5.408855464265644564, -0.4929012147626107843, -1.958461550952787844 ) ) ;
#104060 = CARTESIAN_POINT ( 'NONE',  ( 6.129551335524713096, -0.2748284885467215943, 2.204153950570774345 ) ) ;
#104061 = CARTESIAN_POINT ( 'NONE',  ( -3.546339698426324460, 6.295090860542775779, -1.199719254218450271 ) ) ;
#104062 = CARTESIAN_POINT ( 'NONE',  ( 5.005985031943777308, 6.863401842066294556, -1.599625672291256295 ) ) ;
#104063 = VECTOR ( 'NONE', #117796, 1000.000000000000000 ) ;
#104064 = CARTESIAN_POINT ( 'NONE',  ( 5.647358743468454456, -1.623080139260910437, -1.269863021155111849 ) ) ;
#104065 = CARTESIAN_POINT ( 'NONE',  ( 4.096327398540238640, -0.3419367296172080017, 1.987046374476949095 ) ) ;
#104066 = ORIENTED_EDGE ( 'NONE', *, *, #50294, .F. ) ;
#104067 = CARTESIAN_POINT ( 'NONE',  ( -15.75000000000000000, 12.69999999999999929, -3.200000000000001510 ) ) ;
#104068 = CARTESIAN_POINT ( 'NONE',  ( 3.785751206713845018, 5.439795712631356750, 1.599625672291267398 ) ) ;
#104070 = ORIENTED_EDGE ( 'NONE', *, *, #193642, .T. ) ;
#104069 = CARTESIAN_POINT ( 'NONE',  ( -7.282664789195997912, 8.525472337930658284, 1.199719254218452047 ) ) ;
#104071 = CARTESIAN_POINT ( 'NONE',  ( 5.126881573038487794, 7.911131357477594328, 1.221340741751137493 ) ) ;
#104072 = CARTESIAN_POINT ( 'NONE',  ( 3.690779688840303496, -1.198677090843719872, -1.620934038430859703 ) ) ;
#104073 = CARTESIAN_POINT ( 'NONE',  ( 3.415785861374909249, 1.167101634185686576, -1.423959568491977912 ) ) ;
#104074 = CARTESIAN_POINT ( 'NONE',  ( 1.734723475976807094E-15, 15.42691958146951414, 11.91973154060106665 ) ) ;
#104075 = CARTESIAN_POINT ( 'NONE',  ( 2.333053021162025953, 2.238922732217122125, 0.5587339331782120722 ) ) ;
#104076 = CARTESIAN_POINT ( 'NONE',  ( 3.898851692381625877, 6.706354853490643642, -1.199719254218452047 ) ) ;
#104077 = CARTESIAN_POINT ( 'NONE',  ( 4.393933622532245842, -0.8317529007547798114, 1.995363109761492337 ) ) ;
#104078 = CARTESIAN_POINT ( 'NONE',  ( 8.015895134177609904, 10.37496362800581018, 1.599625672291281386 ) ) ;
#104079 = CARTESIAN_POINT ( 'NONE',  ( 6.585540641348407220, -0.7802508550805786758, 1.666130356082275998 ) ) ;
#104080 = CARTESIAN_POINT ( 'NONE',  ( -4.076197739202962467, 7.907314462378773001, 1.040834085586084257E-14 ) ) ;
#104081 = AXIS2_PLACEMENT_3D ( 'NONE', #61085, #46989, #144515 ) ;
#104082 = EDGE_CURVE ( 'NONE', #169050, #28009, #209860, .T. ) ;
#104083 = CARTESIAN_POINT ( 'NONE',  ( -1.863116269212363063, 15.51999112189398033, 11.88797926174050268 ) ) ;
#104084 = DIRECTION ( 'NONE',  ( -0.7592566023652995710, -0.6507913734559651608, 0.000000000000000000 ) ) ;
#104085 = CARTESIAN_POINT ( 'NONE',  ( 2.623731232481395725, -1.075365945362505293, -1.530472918023266571 ) ) ;
#104086 = CARTESIAN_POINT ( 'NONE',  ( 0.4035112227387879225, -0.5299352985012796280, 1.898712856893035816 ) ) ;
#104088 = CARTESIAN_POINT ( 'NONE',  ( -7.598418745816086783, 7.829519723065708092, 0.000000000000000000 ) ) ;
#104087 = CARTESIAN_POINT ( 'NONE',  ( 0.7499999999999885647, -0.9854166659838472508, 1.299038105676657340 ) ) ;
#104089 = CARTESIAN_POINT ( 'NONE',  ( 2.209865124170300898, -0.4819264253047173541, 2.153463223375853719 ) ) ;
#104090 = VERTEX_POINT ( 'NONE', #1495 ) ;
#104091 = CARTESIAN_POINT ( 'NONE',  ( -4.719485776398897769, 6.960464655427080594, 1.371982998767233175 ) ) ;
#104092 = CARTESIAN_POINT ( 'NONE',  ( 3.734381245560244089, 6.444196322207211836, 1.199719254218462483 ) ) ;
#104093 = CARTESIAN_POINT ( 'NONE',  ( -4.192495815123836955, 5.914331089109674089, -1.599625672291256295 ) ) ;
#104094 = CARTESIAN_POINT ( 'NONE',  ( 2.920214025141053327, 6.445393704534057022, 0.4458799699700779495 ) ) ;
#104095 = CARTESIAN_POINT ( 'NONE',  ( 5.998895389381466714, 1.612053949438954303, -1.134635204971563782 ) ) ;
#104096 = CARTESIAN_POINT ( 'NONE',  ( 5.567085169132608868, -2.083932277878234096, -0.9915751667191848862 ) ) ;
#104097 = CARTESIAN_POINT ( 'NONE',  ( 0.5023040531197673353, 1.956348610274569744, 0.1481081594910879096 ) ) ;
#104098 = CARTESIAN_POINT ( 'NONE',  ( 3.696185820831139779, 0.9318344738791024540, -1.840181792940546179 ) ) ;
#104099 = CARTESIAN_POINT ( 'NONE',  ( 5.721177635286841756, 6.737423998331861341, -1.082531754730543083 ) ) ;
#104100 = CARTESIAN_POINT ( 'NONE',  ( 7.991605200612358573, 8.288237253661408843, 0.7998128361456281477 ) ) ;
#104101 = CARTESIAN_POINT ( 'NONE',  ( 6.914295152845067349, 11.01050207838719075, 1.040834085586084257E-14 ) ) ;
#104102 = CARTESIAN_POINT ( 'NONE',  ( -1.364683531250012516, 3.592708333674750509, 0.7879004041258379498 ) ) ;
#104103 = CARTESIAN_POINT ( 'NONE',  ( -10.47216923660538335, 4.011714437494937613, -5.771917547288382799 ) ) ;
#104104 = CARTESIAN_POINT ( 'NONE',  ( 5.300874872818840622, 6.247070775452521652, 1.082531754730560403 ) ) ;
#104105 = CARTESIAN_POINT ( 'NONE',  ( 0.2862954470153349362, -1.335216113735339105, -1.712835229902017531 ) ) ;
#104107 = CARTESIAN_POINT ( 'NONE',  ( 4.810013364240863787, 1.265987717737980134, -1.337210144835267345 ) ) ;
#104106 = CARTESIAN_POINT ( 'NONE',  ( 11.41267819554179042, 4.000000000000003553, -3.708203932499494648 ) ) ;
#104108 = CARTESIAN_POINT ( 'NONE',  ( 11.91826848330682331, 12.59270354043007067, 1.400000080589832052 ) ) ;
#104109 = CARTESIAN_POINT ( 'NONE',  ( 6.075747529084263299, -1.173811750163206158, 1.850510016281024850 ) ) ;
#104110 = CARTESIAN_POINT ( 'NONE',  ( 0.7548939078372005618, -1.576849831105286537, -1.005952255950369301 ) ) ;
#104111 = EDGE_CURVE ( 'NONE', #37563, #62806, #193761, .T. ) ;
#104112 = CARTESIAN_POINT ( 'NONE',  ( -4.637175514440688318, 7.109613026884349374, 1.382187809737724704 ) ) ;
#104113 = DIRECTION ( 'NONE',  ( -0.000000000000000000, 1.000000000000000000, 9.023263958591317418E-17 ) ) ;
#104114 = CARTESIAN_POINT ( 'NONE',  ( 6.170730229783032428, 7.061345527190763249, -1.063955632616358615 ) ) ;
#104115 = CARTESIAN_POINT ( 'NONE',  ( 0.3988866192712777758, -0.2342882197893907670, -1.897819253221716851 ) ) ;
#104116 = PRODUCT_DEFINITION_FORMATION_WITH_SPECIFIED_SOURCE ( 'ANY', '', #93852, .NOT_KNOWN. ) ;
#104117 = CARTESIAN_POINT ( 'NONE',  ( 2.096244624822783731, -0.4688358662975153357, -1.706545078221621603 ) ) ;
#104118 = CIRCLE ( 'NONE', #48772, 0.08000000000000041800 ) ;
#104119 = CARTESIAN_POINT ( 'NONE',  ( 6.041657904462632622, -1.894779907254999118, 0.6802824325803021877 ) ) ;
#104121 = CARTESIAN_POINT ( 'NONE',  ( 4.271028807069753519, 1.709443138559762376, -0.8646770750302870123 ) ) ;
#104120 = CARTESIAN_POINT ( 'NONE',  ( -8.910733272679575379, 11.41894145625809820, -1.599625672291263179 ) ) ;
#104122 = AXIS2_PLACEMENT_3D ( 'NONE', #11814, #32347, #28078 ) ;
#104123 = DIRECTION ( 'NONE',  ( 0.000000000000000000, 0.000000000000000000, 1.000000000000000000 ) ) ;
#104124 = CARTESIAN_POINT ( 'NONE',  ( 5.248484213797577347, -1.954463446003468885, -0.2428638724455249587 ) ) ;
#104125 = CARTESIAN_POINT ( 'NONE',  ( 6.293224362130668936, -0.1031327824093461465, -2.017302584901353946 ) ) ;
#104126 = CARTESIAN_POINT ( 'NONE',  ( -2.449219305563052895, 6.009172956465517856, 1.040834085586084257E-14 ) ) ;
#104127 = CARTESIAN_POINT ( 'NONE',  ( 2.465516990510143280, 1.834972510290140191, -0.3627323784974947340 ) ) ;
#104129 = ORIENTED_EDGE ( 'NONE', *, *, #49388, .F. ) ;
#104128 = CARTESIAN_POINT ( 'NONE',  ( 5.918504666124354330, 1.153338095414379261, -1.282764499605532738 ) ) ;
#104131 = DIRECTION ( 'NONE',  ( -0.9983585005135560131, 0.000000000000000000, 0.05727394217551282085 ) ) ;
#104130 = CARTESIAN_POINT ( 'NONE',  ( 3.317197348578094562, 1.995112415077514356, 0.9436014139095407760 ) ) ;
#104132 = CARTESIAN_POINT ( 'NONE',  ( -1.364683531249997417, 2.821875000341422801, 1.214306433183764966E-14 ) ) ;
#104133 = CARTESIAN_POINT ( 'NONE',  ( 0.4849267205471480269, 1.973383872003172224, 0.6002626889692606049 ) ) ;
#104134 = CARTESIAN_POINT ( 'NONE',  ( 6.938021921891177612, 9.117444880338284818, -1.599625672291262513 ) ) ;
#104135 = CARTESIAN_POINT ( 'NONE',  ( -9.854078719034067291, 10.39084668182823634, 0.7998128361456462443 ) ) ;
#104136 = CARTESIAN_POINT ( 'NONE',  ( -7.815970093360414158E-14, 8.210952333604092601, -2.038660652713623733 ) ) ;
#104137 = CARTESIAN_POINT ( 'NONE',  ( -3.391510981712834383, 7.108513245306943062, 0.7998128361456341429 ) ) ;
#104138 = DIRECTION ( 'NONE',  ( 0.000000000000000000, 1.000000000000000000, 0.000000000000000000 ) ) ;
#104139 = VERTEX_POINT ( 'NONE', #199710 ) ;
#104140 = CARTESIAN_POINT ( 'NONE',  ( 3.508316276398337319, 2.070544812355082254, 0.002818362966339192730 ) ) ;
#104141 = CARTESIAN_POINT ( 'NONE',  ( 0.7499999999999902300, 4.066666666666690411, -1.299038105676658228 ) ) ;
#104142 = CARTESIAN_POINT ( 'NONE',  ( 5.497994985541524215, 6.373081223675282736, -1.199719254218445830 ) ) ;
#104143 = CARTESIAN_POINT ( 'NONE',  ( -6.035068427865825313, 7.156668563632000435, 1.186355232826277417 ) ) ;
#104144 = CARTESIAN_POINT ( 'NONE',  ( 1.348313414878389294, 0.9933643222376374871, -1.758399455230485575 ) ) ;
#104145 = CARTESIAN_POINT ( 'NONE',  ( 1.499999999999999334, 7.388542872122531691, 4.154462424328197123 ) ) ;
#104146 = CARTESIAN_POINT ( 'NONE',  ( -1.201851678989727383E-14, 4.196875000341417028, -1.575800808251660134 ) ) ;
#104147 = ORIENTED_EDGE ( 'NONE', *, *, #127031, .F. ) ;
#104148 = ADVANCED_FACE ( 'NONE', ( #37228 ), #17545, .T. ) ;
#104150 = CARTESIAN_POINT ( 'NONE',  ( 8.107412671292022921, 12.40247251657532956, 0.7216878364870438212 ) ) ;
#104149 = CARTESIAN_POINT ( 'NONE',  ( 0.1745949693968146810, 5.726316517925682525, -2.349368801211670021 ) ) ;
#104151 = CARTESIAN_POINT ( 'NONE',  ( 6.608749954595573683, 0.7741944705832277673, -1.861732896133998727 ) ) ;
#104152 = CARTESIAN_POINT ( 'NONE',  ( 5.524599559428126305, 0.3805214045222211627, 1.877366190154891701 ) ) ;
#104153 = FILL_AREA_STYLE ('',( #186444 ) ) ;
#104154 = CARTESIAN_POINT ( 'NONE',  ( 4.159861740090546434, 1.033864333764370702, 1.932389678422803181 ) ) ;
#104155 = CARTESIAN_POINT ( 'NONE',  ( 0.7499999999999885647, 1.597916667349486008, -1.299038105676652899 ) ) ;
#104156 = CARTESIAN_POINT ( 'NONE',  ( 2.144650067465687648, 1.855875215511919363, 0.4610605321611755958 ) ) ;
#104157 = CARTESIAN_POINT ( 'NONE',  ( -3.744022975668147790, 7.519777238254810925, -0.7998128361456281477 ) ) ;
#104158 = CARTESIAN_POINT ( 'NONE',  ( 5.816084710138150093, 5.887779704690372817, -0.7216878364870257245 ) ) ;
#104160 = CARTESIAN_POINT ( 'NONE',  ( 0.9840001696646907270, -2.016598147255070472, 0.002831364411433334727 ) ) ;
#104159 = CARTESIAN_POINT ( 'NONE',  ( 3.565173639196337341, 7.339832546762534271, -0.2726055590975334786 ) ) ;
#104161 = CARTESIAN_POINT ( 'NONE',  ( 1.364683531250000303, 10.56770833367473195, -0.7879004041258355073 ) ) ;
#104163 = CARTESIAN_POINT ( 'NONE',  ( -5.815521545619021460, 5.749472989502435460, -0.7998128361456362523 ) ) ;
#104162 = CARTESIAN_POINT ( 'NONE',  ( 5.741772062182810998, 2.188963553168365994, 0.1087695542012837302 ) ) ;
#104165 = ORIENTED_EDGE ( 'NONE', *, *, #141101, .T. ) ;
#104164 = CARTESIAN_POINT ( 'NONE',  ( 3.047548298876975537, 0.6224300751757807504, -1.608722921838340092 ) ) ;
#104166 = DIRECTION ( 'NONE',  ( 0.000000000000000000, 1.000000000000000000, 0.000000000000000000 ) ) ;
#104167 = CARTESIAN_POINT ( 'NONE',  ( 6.448874621594486989, 10.67543749183559143, 0.7998128361456462443 ) ) ;
#104168 = CARTESIAN_POINT ( 'NONE',  ( 6.010342169559767633, 5.906487374108181143, -0.7998128361456281477 ) ) ;
#104169 = DIRECTION ( 'NONE',  ( 0.000000000000000000, 0.000000000000000000, 1.000000000000000000 ) ) ;
#104170 = CARTESIAN_POINT ( 'NONE',  ( 0.9944974185457016169, 1.932217576897478528, 0.3389098420027157332 ) ) ;
#104171 = EDGE_CURVE ( 'NONE', #126115, #146910, #158312, .T. ) ;
#104172 = SURFACE_STYLE_FILL_AREA ( #103097 ) ;
#104173 = CARTESIAN_POINT ( 'NONE',  ( 5.840865249388943248, 5.708764300575555062, 0.7998128361456341429 ) ) ;
#104174 = CARTESIAN_POINT ( 'NONE',  ( 2.057629584373536602, 2.441452740530747789, -11.54123292161950687 ) ) ;
#104175 = ORIENTED_EDGE ( 'NONE', *, *, #173881, .F. ) ;
#104176 = DIRECTION ( 'NONE',  ( -0.000000000000000000, -0.000000000000000000, -1.000000000000000000 ) ) ;
#104177 = ORIENTED_EDGE ( 'NONE', *, *, #40619, .T. ) ;
#104178 = CARTESIAN_POINT ( 'NONE',  ( 3.826654739275455519, 1.278450958818643901, -1.283618901898140985 ) ) ;
#104179 = ORIENTED_EDGE ( 'NONE', *, *, #165266, .T. ) ;
#104180 = CARTESIAN_POINT ( 'NONE',  ( 10.21336978979620191, 10.81001959771741205, 0.7998128361456462443 ) ) ;
#104181 = CARTESIAN_POINT ( 'NONE',  ( -5.366912616075431686, 6.182013390275966636, 1.156538041605560174 ) ) ;
#104182 = CARTESIAN_POINT ( 'NONE',  ( 5.092358660276916638, -1.001593112396873098, 1.509162939045370466 ) ) ;
#104183 = CARTESIAN_POINT ( 'NONE',  ( 6.333067150914805765, 9.442309871825708356, 1.082531754730549967 ) ) ;
#104184 = CARTESIAN_POINT ( 'NONE',  ( 4.739561450132447007, 6.795411536013346243, -1.240012687728889951 ) ) ;
#104186 = CARTESIAN_POINT ( 'NONE',  ( 10.22692794340986921, 10.82583744360002243, 0.000000000000000000 ) ) ;
#104185 = CARTESIAN_POINT ( 'NONE',  ( 5.512096448594467901, 1.858919848428818300, -0.09134777953435403719 ) ) ;
#104187 = CARTESIAN_POINT ( 'NONE',  ( 3.093272052591877763, -0.3707496286316728229, 1.879197483129394719 ) ) ;
#104188 =( NAMED_UNIT ( * ) PLANE_ANGLE_UNIT ( ) SI_UNIT ( $, .RADIAN. ) );
#104189 = CARTESIAN_POINT ( 'NONE',  ( -11.01578653029999266, 5.045029590669321884, -4.264301349201883085 ) ) ;
#104190 = PRESENTATION_LAYER_ASSIGNMENT (  '', '', ( #149100 ) ) ;
#104191 = CARTESIAN_POINT ( 'NONE',  ( -10.99962150373186809, -9.919999999999998153, 0.09125116240079125807 ) ) ;
#104192 = CARTESIAN_POINT ( 'NONE',  ( -0.6823417656250246877, -1.198958332991911790, 1.181850606188755259 ) ) ;
#104193 = CARTESIAN_POINT ( 'NONE',  ( 6.643132081016117851, 8.773406732650713025, 1.443375672974076540 ) ) ;
#104194 = ADVANCED_FACE ( 'NONE', ( #61747 ), #206674, .T. ) ;
#104195 = CARTESIAN_POINT ( 'NONE',  ( -3.307299406729781399, 5.945934176904983381, -1.199719254218452935 ) ) ;
#104196 = CARTESIAN_POINT ( 'NONE',  ( -9.500385102287573602, -7.162053774861992572, 0.01083140255525650089 ) ) ;
#104197 = CARTESIAN_POINT ( 'NONE',  ( 1.113355907768112774, -2.039295093617380594, 0.4597149659458180104 ) ) ;
#104198 = CARTESIAN_POINT ( 'NONE',  ( 5.234329823327693809, 8.264412672927770487, 1.199719254218451159 ) ) ;
#104199 = CARTESIAN_POINT ( 'NONE',  ( 0.1998643617870856648, -1.825052844667142349, -0.05062755788937112200 ) ) ;
#104200 = CARTESIAN_POINT ( 'NONE',  ( -5.037017762676898158, 5.835274463666530131, -1.199719254218446718 ) ) ;
#104201 = EDGE_CURVE ( 'NONE', #149524, #108531, #103649, .T. ) ;
#104202 = CARTESIAN_POINT ( 'NONE',  ( 2.467563089314188662, 1.790814366166630034, -0.3536809140580049471 ) ) ;
#104203 = CARTESIAN_POINT ( 'NONE',  ( -6.471393748265563239, 5.229711127717889596, 2.499999999999998668 ) ) ;
#104204 = CARTESIAN_POINT ( 'NONE',  ( 2.119528921591812498, 0.3396393280722594388, -1.939881811770089115 ) ) ;
#104205 = CARTESIAN_POINT ( 'NONE',  ( 3.632312094575868677, 0.2880498525525148623, 1.920478541846024179 ) ) ;
#104206 = ORIENTED_EDGE ( 'NONE', *, *, #178431, .T. ) ;
#104207 = CARTESIAN_POINT ( 'NONE',  ( -15.75000000000000000, 12.69999999999999929, 1.099999999999996758 ) ) ;
#104208 = CARTESIAN_POINT ( 'NONE',  ( -3.980200614063634568, 6.801261928786307642, 1.199719254218452935 ) ) ;
#104210 = CARTESIAN_POINT ( 'NONE',  ( 3.797228045176269440, -0.2112621354826669517, -2.110076569278092062 ) ) ;
#104209 = CARTESIAN_POINT ( 'NONE',  ( 5.806634928402749196, 9.996434193103704402, -0.7998128361456481317 ) ) ;
#104211 = CARTESIAN_POINT ( 'NONE',  ( -10.56513397747884397, 13.75900096514340198, 3.405015282931166620 ) ) ;
#104212 = CARTESIAN_POINT ( 'NONE',  ( 7.574201371528760163, 11.98831870009225931, 1.040834085586084257E-14 ) ) ;
#104213 = CARTESIAN_POINT ( 'NONE',  ( -5.424143973919053785, 8.485862515284315677, 1.199719254218454489 ) ) ;
#104214 = CARTESIAN_POINT ( 'NONE',  ( 11.97929049433705373, 13.88000000000000078, -0.7046979865771834106 ) ) ;
#104215 = COLOUR_RGB ( '', 0.40784314, 0.44705882, 0.49803922) ;
#104216 = CARTESIAN_POINT ( 'NONE',  ( 7.686546744304875389, 7.932335721302671949, 0.7998128361456291469 ) ) ;
#104217 = DIRECTION ( 'NONE',  ( 0.9998476951563912696, 0.000000000000000000, -0.01745240643728004568 ) ) ;
#104219 = CARTESIAN_POINT ( 'NONE',  ( 6.104703911763087909, 1.883310800321544409, 0.7212973825745233603 ) ) ;
#104218 = CARTESIAN_POINT ( 'NONE',  ( 3.598116246361187542, -1.823677485248562435, -0.08826725125678223927 ) ) ;
#104220 = CARTESIAN_POINT ( 'NONE',  ( 0.1685321339487330372, -0.8835925182541467526, -1.870455940253319183 ) ) ;
#104221 = CARTESIAN_POINT ( 'NONE',  ( -8.161645285746702783, 12.46574390010577105, 0.7216878364870478180 ) ) ;
#104222 = CARTESIAN_POINT ( 'NONE',  ( -4.587973201513257493, 8.494803767824503637, 0.1163994284540965235 ) ) ;
#104223 = CARTESIAN_POINT ( 'NONE',  ( 6.925078400183553917, 6.038071034253152725, 2.450556290382682523 ) ) ;
#104224 = CARTESIAN_POINT ( 'NONE',  ( 4.293723057671197552, -0.7160966649314598476, 1.728361679364013748 ) ) ;
#104225 = CARTESIAN_POINT ( 'NONE',  ( 7.293396569147545527, 10.59638086639245280, 1.199719254218460707 ) ) ;
#104226 = CARTESIAN_POINT ( 'NONE',  ( 2.367692237863534555, 1.889325326408105576, -0.3758258368516536052 ) ) ;
#104227 = CARTESIAN_POINT ( 'NONE',  ( 6.702011072381410806, 0.7537920952922130269, -1.811353739714548272 ) ) ;
#104228 = AXIS2_PLACEMENT_3D ( 'NONE', #121575, #185408, #3444 ) ;
#104229 = CARTESIAN_POINT ( 'NONE',  ( -0.6823417656250039265, 9.630208333674728394, -1.181850606188755259 ) ) ;
#104230 = CARTESIAN_POINT ( 'NONE',  ( -5.442708600882160574, 8.437244903416123876, -1.199719254218446718 ) ) ;
#104231 = CARTESIAN_POINT ( 'NONE',  ( 5.020596955762157698, 4.751784624677624080, 1.040834085586084257E-14 ) ) ;
#104232 = CARTESIAN_POINT ( 'NONE',  ( -3.634994581795317536, 7.254927755487573293, 0.000000000000000000 ) ) ;
#104233 = CARTESIAN_POINT ( 'NONE',  ( 1.581820014152079956, -0.7095999980938502150, 1.994918640774499430 ) ) ;
#104234 = PLANE ( 'NONE',  #73571 ) ;
#104235 = CARTESIAN_POINT ( 'NONE',  ( -1.407792700327074931, 4.233596129272890529, 0.5229849042009224735 ) ) ;
#104236 = CARTESIAN_POINT ( 'NONE',  ( 5.102424979711988051, 2.064335680360945169, 0.1577259720206558580 ) ) ;
#104238 = CARTESIAN_POINT ( 'NONE',  ( -1.201851678989727383E-14, 3.134375000341420137, 1.575800808251672791 ) ) ;
#104237 = CARTESIAN_POINT ( 'NONE',  ( 0.2394788589213901198, 1.836227513651207177, 0.1364553164684492448 ) ) ;
#104239 = CARTESIAN_POINT ( 'NONE',  ( 5.133504205653830255, 0.6649215086056580182, 2.200401518963719383 ) ) ;
#104240 = CARTESIAN_POINT ( 'NONE',  ( 5.612712406377503349, 8.531619659873665995, -1.082531754730543083 ) ) ;
#104242 = FILL_AREA_STYLE ('',( #53346 ) ) ;
#104241 = CARTESIAN_POINT ( 'NONE',  ( 3.716343503921665459, 6.389465617000312569, -1.082531754730549967 ) ) ;
#104243 = CARTESIAN_POINT ( 'NONE',  ( 1.816774867096879964, 2.139948438195220071, 0.8220829075690959664 ) ) ;
#104244 = CARTESIAN_POINT ( 'NONE',  ( -0.09263630470260257599, -10.00000000000047251, -9.579493439010613898 ) ) ;
#104245 = CARTESIAN_POINT ( 'NONE',  ( -4.749098946536820520, 8.762642214260091933, 0.7998128361456281477 ) ) ;
#104246 = CARTESIAN_POINT ( 'NONE',  ( 6.017518264666532168, -1.080727962582687773, -1.613252759315900731 ) ) ;
#104247 = ORIENTED_EDGE ( 'NONE', *, *, #50690, .T. ) ;
#104248 = CARTESIAN_POINT ( 'NONE',  ( 7.063434842595398777, 11.18449838309590483, -0.7216878364870267237 ) ) ;
#104249 = VERTEX_POINT ( 'NONE', #41254 ) ;
#104250 = CARTESIAN_POINT ( 'NONE',  ( 6.533470333208203584, -0.1312131129157616261, 1.882018712217728318 ) ) ;
#104251 = CARTESIAN_POINT ( 'NONE',  ( 5.700407750362016301, 1.350738941191354625, -1.497498989668680114 ) ) ;
#104253 = CARTESIAN_POINT ( 'NONE',  ( 4.318600669050584706, 4.999583595936801572, 2.499999999999999556 ) ) ;
#104252 = CARTESIAN_POINT ( 'NONE',  ( -8.365544474831901667, 9.718555627847388578, 1.199719254218462483 ) ) ;
#104254 = CARTESIAN_POINT ( 'NONE',  ( 1.642778471875000035, -1.713541666188707291, -2.845375778867859751 ) ) ;
#104256 = CARTESIAN_POINT ( 'NONE',  ( 1.516075769870619316, 1.192070010050453099, -1.308345436402546191 ) ) ;
#104255 = CARTESIAN_POINT ( 'NONE',  ( 3.222686667372671732, 0.05170946606813638102, 2.090169120961588245 ) ) ;
#104257 = CARTESIAN_POINT ( 'NONE',  ( 6.416638760586134360, -1.319225726833603840, -1.525046029381103452 ) ) ;
#104258 = CARTESIAN_POINT ( 'NONE',  ( 3.750172280943805170, 0.8240398376481252729, 2.139190334408520577 ) ) ;
#104259 = CARTESIAN_POINT ( 'NONE',  ( 3.872797606970843631, 1.637851192275063816, -0.5887498661538635991 ) ) ;
#104260 = CARTESIAN_POINT ( 'NONE',  ( 3.379006598303866848, 4.965260336153046516, -1.599625672291262513 ) ) ;
#104261 = CARTESIAN_POINT ( 'NONE',  ( -2.810282979782591006, 6.500690253046801814, 0.000000000000000000 ) ) ;
#104262 = CARTESIAN_POINT ( 'NONE',  ( 1.985274739808037481, 1.615814429867837410, 0.6292545280836835397 ) ) ;
#104263 =( BOUNDED_CURVE ( )  B_SPLINE_CURVE ( 2, ( #55327, #49204, #165073, #32943, #198614, #36929, #213787, #186375, #65410 ),
 .UNSPECIFIED., .F., .T. ) 
 B_SPLINE_CURVE_WITH_KNOTS ( ( 3, 2, 2, 2, 3 ),
 ( 0.3482142857142856429, 0.3511904761904761640, 0.3571428571428571508, 0.3630952380952380820, 0.3660714285714286031 ),
 .UNSPECIFIED. ) 
 CURVE ( )  GEOMETRIC_REPRESENTATION_ITEM ( )  RATIONAL_B_SPLINE_CURVE ( ( 0.9330127018922194093, 0.9330127018922180770, 1.000000000000000000, 0.8660254037844387076, 1.000000000000000000, 0.8660254037844387076, 1.000000000000000000, 0.9330127018922187432, 0.9330127018922194093 ) ) 
 REPRESENTATION_ITEM ( '' )  );
#104264 = CARTESIAN_POINT ( 'NONE',  ( 3.473242058572806990, 1.961495611989271248, 0.9311941066344242568 ) ) ;
#104265 = CARTESIAN_POINT ( 'NONE',  ( 4.792970997630896512, 5.550553237779539018, 1.199719254218464037 ) ) ;
#104266 = CARTESIAN_POINT ( 'NONE',  ( 4.557827498477605488, 1.164984774316142113, 1.645760986912048640 ) ) ;
#104267 = CARTESIAN_POINT ( 'NONE',  ( 3.125000000000001776, -2.052068128417947168, 1.787079010424618414E-13 ) ) ;
#104268 = AXIS2_PLACEMENT_3D ( 'NONE', #64499, #2655, #148945 ) ;
#104269 = CARTESIAN_POINT ( 'NONE',  ( -1.201851678989727383E-14, 2.743750000682820378, 1.732050807568877637 ) ) ;
#104270 = CARTESIAN_POINT ( 'NONE',  ( 0.8504600536136133204, 0.5560621936452102565, 1.844401357902447414 ) ) ;
#104271 = CARTESIAN_POINT ( 'NONE',  ( -0.7500000000000179856, 8.322916667349467446, 1.299038105676658228 ) ) ;
#104272 = CARTESIAN_POINT ( 'NONE',  ( 4.289451472217206351, -0.001904023060144560469, -2.221583672334653148 ) ) ;
#104273 = ORIENTED_EDGE ( 'NONE', *, *, #149088, .T. ) ;
#104275 = AXIS2_PLACEMENT_3D ( 'NONE', #54369, #202718, #83649 ) ;
#104274 = CARTESIAN_POINT ( 'NONE',  ( 6.883263157960366918, 3.696842586722656865, 2.460469087180997327 ) ) ;
#104276 = CARTESIAN_POINT ( 'NONE',  ( 0.7499999999999867883, 0.06666666666668707997, -1.299038105676652899 ) ) ;
#104277 = CARTESIAN_POINT ( 'NONE',  ( 6.938021921891177612, 9.117444880338284818, -1.599625672291262513 ) ) ;
#104278 = CARTESIAN_POINT ( 'NONE',  ( 5.029711800545521250, 5.930713857800314237, -1.082531754730549078 ) ) ;
#104279 = CARTESIAN_POINT ( 'NONE',  ( 3.285556943749998737, -1.655208332855374609, -1.896917185911906722 ) ) ;
#104280 = CARTESIAN_POINT ( 'NONE',  ( 1.190412498926897600, 1.327076764020938882, 1.781161496267854361 ) ) ;
#104281 = CARTESIAN_POINT ( 'NONE',  ( 5.318788500806308051, -1.422220495204097546, 1.351624447685224162 ) ) ;
#104282 = CARTESIAN_POINT ( 'NONE',  ( 10.24960094225127172, 11.06021530882240356, -0.7216878364870257245 ) ) ;
#104283 = CARTESIAN_POINT ( 'NONE',  ( -1.364564222265963300, 3.685551582065023091, -0.6239050962422643121 ) ) ;
#104284 = CARTESIAN_POINT ( 'NONE',  ( 6.626273523942327159, 1.310778252226969975, -1.843845376178480322 ) ) ;
#104285 = CARTESIAN_POINT ( 'NONE',  ( -4.163762573172648196, 7.871823745427799501, 0.000000000000000000 ) ) ;
#104286 = CARTESIAN_POINT ( 'NONE',  ( 3.684078386338876854, -1.226296459201616340, -1.658441301575198645 ) ) ;
#104287 = CARTESIAN_POINT ( 'NONE',  ( -5.576481253922474401, 5.400316305864651056, -0.7998128361456221525 ) ) ;
#104288 = CARTESIAN_POINT ( 'NONE',  ( -0.7499999999999972244, 3.639583334016149863, -1.299038105676652011 ) ) ;
#104289 = CARTESIAN_POINT ( 'NONE',  ( -1.201851678989727383E-14, 5.509375000341415252, -1.575800808251660134 ) ) ;
#104290 = CARTESIAN_POINT ( 'NONE',  ( 4.833189656263336964, -1.710893631887340227, 0.7565425265826587475 ) ) ;
#104291 = CARTESIAN_POINT ( 'NONE',  ( 3.551122959743778562, -1.161752147869070884, 1.287673551650715842 ) ) ;
#104292 = CARTESIAN_POINT ( 'NONE',  ( 3.034399582073334489, -1.533639759443014894, 0.8228653360542650397 ) ) ;
#104293 = CARTESIAN_POINT ( 'NONE',  ( 0.7500711518760843077, 2.289381476473162369, -0.1197363719210968458 ) ) ;
#104294 = CARTESIAN_POINT ( 'NONE',  ( 0.6823417656249917140, 4.655208333674755394, 1.181850606188765695 ) ) ;
#104295 = CARTESIAN_POINT ( 'NONE',  ( 5.038659576058011957, -1.792549807278142726, 1.075873411605046348 ) ) ;
#104296 = CARTESIAN_POINT ( 'NONE',  ( 0.2339851986729903077, 0.3116528534230639247, 1.814411239467295101 ) ) ;
#104297 = CARTESIAN_POINT ( 'NONE',  ( 0.08058608058607380498, -9.900000000000005684, 10.99970480893082225 ) ) ;
#104298 = FILL_AREA_STYLE_COLOUR ( '', #31150 ) ;
#104299 = CARTESIAN_POINT ( 'NONE',  ( 1.934220422044398813, -1.621183349045727473, -1.198859219795316955 ) ) ;
#104300 = DIRECTION ( 'NONE',  ( 0.000000000000000000, 0.000000000000000000, 1.000000000000000000 ) ) ;
#104301 = CARTESIAN_POINT ( 'NONE',  ( 7.577342237528466029, 14.99429123645997919, -10.16790800466224987 ) ) ;
#104302 = CARTESIAN_POINT ( 'NONE',  ( -8.850775351622791831, 9.220326086515070685, -0.7998128361456291469 ) ) ;
#104303 = CARTESIAN_POINT ( 'NONE',  ( 6.494519276145969577, 7.535692896047149425, -1.199719254218446718 ) ) ;
#104304 = CARTESIAN_POINT ( 'NONE',  ( 2.578903501431661915, -1.460476376761214556, 1.537597662120089081 ) ) ;
#104305 = B_SPLINE_CURVE_WITH_KNOTS ( 'NONE', 3,
 ( #9166, #7002, #141353, #124082, #155418, #105633 ),
 .UNSPECIFIED., .F., .F.,
 ( 4, 2, 4 ),
 ( 0.000000000000000000, 0.5000000000000000000, 1.000000000000000000 ),
 .UNSPECIFIED. ) ;
#104306 = DIRECTION ( 'NONE',  ( 0.000000000000000000, -1.000000000000000000, 0.000000000000000000 ) ) ;
#104307 = CARTESIAN_POINT ( 'NONE',  ( 4.793472150574508817, 1.354911484294840429, 1.223852735664505698 ) ) ;
#104308 = VERTEX_POINT ( 'NONE', #8722 ) ;
#104309 = CARTESIAN_POINT ( 'NONE',  ( -7.767895665986912057, 8.027242796598338614, -0.7998128361456362523 ) ) ;
#104310 = CARTESIAN_POINT ( 'NONE',  ( 1.001543065824772753E-15, -4.068749999044083410, 4.012584370867899430 ) ) ;
#104311 = CARTESIAN_POINT ( 'NONE',  ( -7.881367368245678406, 8.089350105908421185, 0.7998128361456602331 ) ) ;
#104312 = CARTESIAN_POINT ( 'NONE',  ( 1.845969175824228925, -1.322618866652914393, -1.526557775719493915 ) ) ;
#104313 = CARTESIAN_POINT ( 'NONE',  ( 5.631908123138919642, -1.395923778694251105, -1.709176034821748624 ) ) ;
#104314 = EDGE_CURVE ( 'NONE', #45033, #98073, #60671, .T. ) ;
#104315 = CARTESIAN_POINT ( 'NONE',  ( -5.093022980588950865, 5.970890227889075419, -1.199719254218453823 ) ) ;
#104316 = CARTESIAN_POINT ( 'NONE',  ( 4.258551055683129860, -0.5805891344777401875, -1.768159363456432764 ) ) ;
#104317 = CARTESIAN_POINT ( 'NONE',  ( 9.297140650669039275, 11.86975006391249643, 1.599625672291281386 ) ) ;
#104318 = DIRECTION ( 'NONE',  ( -1.000000000000000000, 0.000000000000000000, 0.000000000000000000 ) ) ;
#104319 = EDGE_LOOP ( 'NONE', ( #140715, #95601, #130875, #200412 ) ) ;
#104320 = ORIENTED_EDGE ( 'NONE', *, *, #53608, .T. ) ;
#104321 = CARTESIAN_POINT ( 'NONE',  ( -5.603597561149804562, 5.431951997629870910, 0.7998128361456341429 ) ) ;
#104322 = CARTESIAN_POINT ( 'NONE',  ( -6.821723845970312894, 11.11042825360738284, 0.000000000000000000 ) ) ;
#104323 = CARTESIAN_POINT ( 'NONE',  ( 4.740742070742828496, 0.3150700179065483719, 1.798135100120237251 ) ) ;
#104325 = CARTESIAN_POINT ( 'NONE',  ( -4.391370929004954959, 7.351591927832363815, -1.215465595245905250 ) ) ;
#104324 = CARTESIAN_POINT ( 'NONE',  ( -7.075376061485238566, 9.347967719856493218, 1.599625672291269396 ) ) ;
#104326 = CARTESIAN_POINT ( 'NONE',  ( 0.6823417656249882723, -0.6572916663252492686, 1.181850606188755259 ) ) ;
#104327 = CARTESIAN_POINT ( 'NONE',  ( 0.9304778391672563487, 0.8475688526466665929, 1.512457944649912012 ) ) ;
#104328 = CARTESIAN_POINT ( 'NONE',  ( 0.1986093482617317107, -0.4694325260376422948, 1.675759954737522150 ) ) ;
#104329 = CARTESIAN_POINT ( 'NONE',  ( 6.006511608602003172, -0.8246739634825739351, -2.155485180906725251 ) ) ;
#104330 = CARTESIAN_POINT ( 'NONE',  ( 4.095444919779759552, 6.935713618788495793, 1.199719254218451159 ) ) ;
#104331 = CARTESIAN_POINT ( 'NONE',  ( 1.018906392562862528, 1.903027849223213330, 0.7912521351585340978 ) ) ;
#104332 = CARTESIAN_POINT ( 'NONE',  ( 6.169123589417988995, 7.156064594864501416, -1.199719254218445830 ) ) ;
#104333 = EDGE_CURVE ( 'NONE', #208480, #124513, #26858, .T. ) ;
#104334 = EDGE_CURVE ( 'NONE', #6267, #31530, #106549, .T. ) ;
#104335 = CARTESIAN_POINT ( 'NONE',  ( 6.766976407292540685, -2.298085592349991213, 0.04593636341931536110 ) ) ;
#104336 = CARTESIAN_POINT ( 'NONE',  ( 1.500000000000001332, 11.40625000068279427, 0.000000000000000000 ) ) ;
#104337 = CARTESIAN_POINT ( 'NONE',  ( -7.096767062110449942, 7.244259425409119046, -0.7998128361456362523 ) ) ;
#104338 = VECTOR ( 'NONE', #89426, 1000.000000000000000 ) ;
#104339 = CARTESIAN_POINT ( 'NONE',  ( 6.262560305340551636, -1.321439916381482060, 1.324322166508178356 ) ) ;
#104341 = CARTESIAN_POINT ( 'NONE',  ( -3.284818356260900796, 7.054314858938165678, 0.7998128361456352531 ) ) ;
#104340 = CARTESIAN_POINT ( 'NONE',  ( 3.867365959033176814, -1.592763314076732106, -1.058159689705892692 ) ) ;
#104342 = CARTESIAN_POINT ( 'NONE',  ( 4.828867971087246858, 2.111205472107956282, 0.6427781511747706622 ) ) ;
#104343 = CARTESIAN_POINT ( 'NONE',  ( -1.225000000000033396, 2.062500000682796042, -2.949029909160572061E-14 ) ) ;
#104344 = CARTESIAN_POINT ( 'NONE',  ( -0.3878679656440350842, 4.000000000000003553, -1.007084189318380618 ) ) ;
#104345 = CARTESIAN_POINT ( 'NONE',  ( 4.055297343818931033, 6.784911763547157193, 1.082531754730549078 ) ) ;
#104346 = CARTESIAN_POINT ( 'NONE',  ( -5.614485009390564940, 5.722856397143323726, 0.000000000000000000 ) ) ;
#104347 = CARTESIAN_POINT ( 'NONE',  ( 5.953796468794862129, -1.535729488331440074, -1.462440914314271811 ) ) ;
#104348 = EDGE_LOOP ( 'NONE', ( #169039, #182001, #132859, #54000, #4490, #78594 ) ) ;
#104349 = CARTESIAN_POINT ( 'NONE',  ( 3.276728144386112263, -1.376063543960687641, 1.852258789692583507 ) ) ;
#104350 = CARTESIAN_POINT ( 'NONE',  ( 3.947668504265917644, 1.419370528949075005, 1.354593381527373186 ) ) ;
#104351 = CARTESIAN_POINT ( 'NONE',  ( -4.447956913735107598, 7.346977611736363656, 1.199719254218452935 ) ) ;
#104352 = CARTESIAN_POINT ( 'NONE',  ( 1.094497266827038962, 1.931770780797737341, 0.3408682529649207926 ) ) ;
#104353 = CARTESIAN_POINT ( 'NONE',  ( 1.734723475976807094E-15, 14.57308041853048231, 11.91973154060107376 ) ) ;
#104354 = CARTESIAN_POINT ( 'NONE',  ( -11.92046840572485777, 13.65252124794268873, 1.382231356234940867 ) ) ;
#104355 = ORIENTED_EDGE ( 'NONE', *, *, #171151, .F. ) ;
#104356 = CARTESIAN_POINT ( 'NONE',  ( 5.841029835422532734, -1.731992920607817288, -1.032484497598872064 ) ) ;
#104357 = CARTESIAN_POINT ( 'NONE',  ( -9.321394304595349567, 10.83371376257142416, 1.199719254218462483 ) ) ;
#104358 = CARTESIAN_POINT ( 'NONE',  ( 0.07576575995338691305, -1.785066692240460329, -0.4505573523648153667 ) ) ;
#104359 = CARTESIAN_POINT ( 'NONE',  ( 3.415042003188377251, -1.647272610417279015, 1.414370313860166872 ) ) ;
#104360 = CARTESIAN_POINT ( 'NONE',  ( 4.016958651398847557, 7.908478536599130138, -0.7998128361456361413 ) ) ;
#104361 = CARTESIAN_POINT ( 'NONE',  ( 0.9672155168029163974, -1.668165459610539081, 1.309123814877902969 ) ) ;
#104362 = CARTESIAN_POINT ( 'NONE',  ( -0.7500000000000215383, 1.972916667349486453, 1.299038105676659116 ) ) ;
#104363 = CARTESIAN_POINT ( 'NONE',  ( 9.028840231696797503, 12.62106513936658203, -1.199719254218446718 ) ) ;
#104364 = CARTESIAN_POINT ( 'NONE',  ( 0.4000000000062943761, 2.913060511812307407, -2.023857702505970302 ) ) ;
#104365 = CARTESIAN_POINT ( 'NONE',  ( 5.997720278586790243, 7.186234674792547850, 1.197368251494409286 ) ) ;
#104366 = CARTESIAN_POINT ( 'NONE',  ( 0.8782832160191712534, -1.147062573054495216, 1.711818785435960111 ) ) ;
#104367 = VECTOR ( 'NONE', #162634, 1000.000000000000000 ) ;
#104369 = CARTESIAN_POINT ( 'NONE',  ( 6.827182134110188372, 3.700652156503980716, 2.425390344263624431 ) ) ;
#104368 = FACE_OUTER_BOUND ( 'NONE', #97565, .T. ) ;
#104370 = CARTESIAN_POINT ( 'NONE',  ( 1.364683531249988535, 1.363541667008083769, 0.7879004041258500513 ) ) ;
#104371 = CARTESIAN_POINT ( 'NONE',  ( 1.249999999999961142, 8.500000000000000000, -10.85702537530424472 ) ) ;
#104372 = EDGE_LOOP ( 'NONE', ( #85701, #155889 ) ) ;
#104373 = CARTESIAN_POINT ( 'NONE',  ( 4.547458224165379370, -1.746952781796941911, 0.7782266863690867620 ) ) ;
#104374 = CARTESIAN_POINT ( 'NONE',  ( 4.856192259477753126, 0.6790438925599675546, 1.634599669825251178 ) ) ;
#104375 = CARTESIAN_POINT ( 'NONE',  ( 5.580062740476173566, 8.667767742934335828, 1.199719254218451159 ) ) ;
#104376 = CARTESIAN_POINT ( 'NONE',  ( -4.120788623549732854, 6.895004929861607401, -1.199719254218452047 ) ) ;
#104377 = CARTESIAN_POINT ( 'NONE',  ( 0.5624193892179689680, 0.5266301872345402479, 1.733300928327138113 ) ) ;
#104379 = CARTESIAN_POINT ( 'NONE',  ( 1.165091096179095675, 1.768693976065521589, -0.7364918582971339278 ) ) ;
#104378 = CARTESIAN_POINT ( 'NONE',  ( 1.499999999999990896, 8.266799604814712765, -3.162088779279259132 ) ) ;
#104380 = CARTESIAN_POINT ( 'NONE',  ( 2.119664376568120012, 0.3561266789769075292, -2.039353370234835872 ) ) ;
#104381 = CARTESIAN_POINT ( 'NONE',  ( -1.364683531250000748, 0.8218750003414210248, 0.000000000000000000 ) ) ;
#104382 = CARTESIAN_POINT ( 'NONE',  ( 0.7078139640715176428, -1.962176506181498636, 0.1910761354673266577 ) ) ;
#104383 = CARTESIAN_POINT ( 'NONE',  ( 3.211362085483655981, -0.3553965070040401852, 1.790585553824732390 ) ) ;
#104385 = CARTESIAN_POINT ( 'NONE',  ( 6.210774601750883583, 6.933448576277219111, 0.8519936491524527922 ) ) ;
#104384 = CARTESIAN_POINT ( 'NONE',  ( 6.721333373144884327, -0.1645177889858795151, 2.170883633896856679 ) ) ;
#104386 = CARTESIAN_POINT ( 'NONE',  ( -1.402160292154681736E-14, 0.1968750003414221628, -1.575800808251665908 ) ) ;
#104387 = CARTESIAN_POINT ( 'NONE',  ( 3.895030958483152173, 0.2998364479755392664, 2.040644712996171339 ) ) ;
#104388 = CARTESIAN_POINT ( 'NONE',  ( -5.215082642750900277, 9.236013516518044142, 0.000000000000000000 ) ) ;
#104389 = CARTESIAN_POINT ( 'NONE',  ( 7.344766530301147789, 9.591980256816594164, 1.599625672291281386 ) ) ;
#104390 = CARTESIAN_POINT ( 'NONE',  ( 3.506755287428983792, 7.242964935309132990, 1.040834085586084257E-14 ) ) ;
#104391 = CARTESIAN_POINT ( 'NONE',  ( 4.710568305744190276, 7.583081225755162968, 1.199719254218462483 ) ) ;
#104392 = CARTESIAN_POINT ( 'NONE',  ( 0.7499999999999902300, 3.983333333333352488, 1.299038105676669330 ) ) ;
#104393 = CARTESIAN_POINT ( 'NONE',  ( 6.373496627357888578, -0.2573980274669443458, 2.054251119134167691 ) ) ;
#104394 = CARTESIAN_POINT ( 'NONE',  ( -0.6823417656250003738, 1.780208333674752952, -1.181850606188749264 ) ) ;
#104395 = CARTESIAN_POINT ( 'NONE',  ( 4.024825912876791811, 2.051136489140188424, 0.6822911077620784637 ) ) ;
#104396 = CARTESIAN_POINT ( 'NONE',  ( 4.758466132964124462, 2.014421802844321707, 0.1462751549737814905 ) ) ;
#104397 = CARTESIAN_POINT ( 'NONE',  ( 6.620655732516651071, 1.241313378043694238, 2.288056600130850882 ) ) ;
#104398 = EDGE_CURVE ( 'NONE', #202042, #176704, #193867, .T. ) ;
#104401 = CARTESIAN_POINT ( 'NONE',  ( 7.782016984564065432, 8.181367358187307204, 0.7216878364870458196 ) ) ;
#104400 = CARTESIAN_POINT ( 'NONE',  ( 1.642778471875000035, -3.376041666188708046, -2.845375778867859751 ) ) ;
#104399 = CARTESIAN_POINT ( 'NONE',  ( 0.4499999999999975131, 3.999999999999961808, -0.9353126743251579667 ) ) ;
#104402 = CARTESIAN_POINT ( 'NONE',  ( -5.173318132066234476, 8.193232366456022930, -1.199719254218453823 ) ) ;
#104403 = CARTESIAN_POINT ( 'NONE',  ( 2.782435679340321766, -0.5899881929209308540, -1.928257399728677601 ) ) ;
#104404 = CARTESIAN_POINT ( 'NONE',  ( -5.852315862593199469, 9.979452273000736895, 0.7998128361456481317 ) ) ;
#104406 =( NAMED_UNIT ( * ) PLANE_ANGLE_UNIT ( ) SI_UNIT ( $, .RADIAN. ) );
#104405 = CARTESIAN_POINT ( 'NONE',  ( -4.253507506385335368, 5.985511395581417204, 1.599625672291267398 ) ) ;
#104407 = CARTESIAN_POINT ( 'NONE',  ( -3.735410078681058010, 7.355792676762846760, 0.6188595546183575102 ) ) ;
#104408 = CARTESIAN_POINT ( 'NONE',  ( 6.135011676971933170, 1.786887936952135769, 0.6819008164158718577 ) ) ;
#104409 = CARTESIAN_POINT ( 'NONE',  ( 6.720655732516624070, 2.949086357957014570, 2.625980845328681923 ) ) ;
#104411 = CARTESIAN_POINT ( 'NONE',  ( 4.903922820734956112, -1.081083478763317007, -1.701937824264573518 ) ) ;
#104410 = CARTESIAN_POINT ( 'NONE',  ( -6.670248387799091461, 10.72578085250020585, 0.000000000000000000 ) ) ;
#104412 = CARTESIAN_POINT ( 'NONE',  ( -1.201851678989727383E-14, 5.337500000000020783, -1.732050807568863648 ) ) ;
#104413 = CARTESIAN_POINT ( 'NONE',  ( 1.364683531249997417, 15.29687500034139447, 2.602085213965210642E-15 ) ) ;
#104414 = CARTESIAN_POINT ( 'NONE',  ( 6.334932600541999470, 0.1746011871221597178, 1.715888227437605718 ) ) ;
#104415 = CARTESIAN_POINT ( 'NONE',  ( 4.864343252252968597, 8.897093904262280972, 0.000000000000000000 ) ) ;
#104417 = DIRECTION ( 'NONE',  ( -0.1700204568168937336, 0.9655305911742121383, 0.1970881066187179509 ) ) ;
#104416 = CARTESIAN_POINT ( 'NONE',  ( 9.463228032658635769, 11.10314946193233965, -1.082531754730543083 ) ) ;
#104418 = CARTESIAN_POINT ( 'NONE',  ( -11.33772463945036968, 10.90000000000000036, -3.600000000000000977 ) ) ;
#104419 = CARTESIAN_POINT ( 'NONE',  ( 5.149604166610965095, 0.5880212298954893280, -1.775756280894603689 ) ) ;
#104420 = CARTESIAN_POINT ( 'NONE',  ( 6.099863781956886832, 1.391357071557168146, 1.455236689230124947 ) ) ;
#104421 = LINE ( 'NONE', #125018, #161498 ) ;
#104422 = CARTESIAN_POINT ( 'NONE',  ( 2.536061329345109971, 1.270221119870031057, 1.634730569901183150 ) ) ;
#104423 = CARTESIAN_POINT ( 'NONE',  ( -2.331034670843834533E-15, -9.756397064627583049, -9.569424307476229075 ) ) ;
#104424 = EDGE_LOOP ( 'NONE', ( #102732, #157732, #126100, #18798, #146364, #56376 ) ) ;
#104425 = CARTESIAN_POINT ( 'NONE',  ( 10.66990370383054731, 11.55056853066490952, 0.7216878364870317197 ) ) ;
#104426 = CARTESIAN_POINT ( 'NONE',  ( 1.054314798682391530, -1.277026470193865171, 1.560515422851154854 ) ) ;
#104427 = CARTESIAN_POINT ( 'NONE',  ( 1.089788312850032526, 1.080336570596603929, 1.454002670061284919 ) ) ;
#104428 = CARTESIAN_POINT ( 'NONE',  ( 4.136646265500957043, 5.919449624541475607, -1.443375672974068769 ) ) ;
#104429 = LINE ( 'NONE', #25295, #131925 ) ;
#104430 = CARTESIAN_POINT ( 'NONE',  ( 8.446366511189332016, 9.916811020218137429, -1.082531754730543083 ) ) ;
#104431 = CARTESIAN_POINT ( 'NONE',  ( 8.260995669428309540, 8.532249790621511565, 0.7998128361456481317 ) ) ;
#104433 = CARTESIAN_POINT ( 'NONE',  ( 5.677321882007140275, 1.453744714618950606, 1.247594701790984306 ) ) ;
#104432 = CARTESIAN_POINT ( 'NONE',  ( -5.018489415352746619, 9.006654751220198207, 0.7998128361456481317 ) ) ;
#104434 = CYLINDRICAL_SURFACE ( 'NONE', #90521, 1.250000000000000000 ) ;
#104435 = CARTESIAN_POINT ( 'NONE',  ( -4.487385655998893164, 6.258369236797239665, 1.443375672974064550 ) ) ;
#104436 = CARTESIAN_POINT ( 'NONE',  ( -1.402160292154681736E-14, -0.7406249996585823059, -1.575800808251665908 ) ) ;
#104438 = ORIENTED_EDGE ( 'NONE', *, *, #205622, .F. ) ;
#104437 = CARTESIAN_POINT ( 'NONE',  ( 4.867013957625893283, 4.780530493426062399, 1.040834085586084257E-14 ) ) ;
#104439 = CARTESIAN_POINT ( 'NONE',  ( -4.243865776277440993, 4.909930479533815451, -1.199719254218446718 ) ) ;
#104440 = EDGE_CURVE ( 'NONE', #19069, #44666, #64895, .T. ) ;
#104441 = CARTESIAN_POINT ( 'NONE',  ( 2.448304249002517974, 2.161202317112873139, 0.05382173394478938222 ) ) ;
#104442 = CARTESIAN_POINT ( 'NONE',  ( -3.471769853551161411, 6.208092708188416076, 1.199719254218452935 ) ) ;
#104443 = CARTESIAN_POINT ( 'NONE',  ( 7.051649292883499953, 7.399548061218447437, -0.7216878364870317197 ) ) ;
#104444 = CARTESIAN_POINT ( 'NONE',  ( 0.6859744409541921328, 2.042103856186634925, -0.5713114342573709648 ) ) ;
#104445 = ADVANCED_FACE ( 'NONE', ( #111632 ), #128379, .F. ) ;
#104446 = CARTESIAN_POINT ( 'NONE',  ( 5.895480738319402114, 1.384055093596334274, 1.190509915477963698 ) ) ;
#104447 =( BOUNDED_CURVE ( )  B_SPLINE_CURVE ( 2, ( #119932, #67869, #166475, #200023, #185908, #71082, #20208 ),
 .UNSPECIFIED., .F., .T. ) 
 B_SPLINE_CURVE_WITH_KNOTS ( ( 3, 2, 2, 3 ),
 ( 0.2999999999999993783, 0.3083333333333330151, 0.3166666666666665408, 0.3250000000000001776 ),
 .UNSPECIFIED. ) 
 CURVE ( )  GEOMETRIC_REPRESENTATION_ITEM ( )  RATIONAL_B_SPLINE_CURVE ( ( 1.000000000000009770, 0.8660254037844289376, 1.000000000000000000, 0.8660254037844387076, 1.000000000000000000, 0.8660254037844360431, 1.000000000000002665 ) ) 
 REPRESENTATION_ITEM ( '' )  );
#104448 = CARTESIAN_POINT ( 'NONE',  ( 1.774623370849885085, -1.870687226035630646, -0.6220538675408300300 ) ) ;
#104449 = CARTESIAN_POINT ( 'NONE',  ( 4.904515063324526025, -1.898637117948184017, -0.2282459111111398431 ) ) ;
#104450 = VERTEX_POINT ( 'NONE', #8588 ) ;
#104451 = APPLICATION_CONTEXT ( 'automotive_design' ) ;
#104452 = CARTESIAN_POINT ( 'NONE',  ( -0.8999481596081082557, 14.48154075026957877, -12.00000000000000178 ) ) ;
#104453 = CARTESIAN_POINT ( 'NONE',  ( 5.371531009330141160, -0.2907324665500017891, 1.947856185699713638 ) ) ;
#104454 = CARTESIAN_POINT ( 'NONE',  ( -0.02357939311542662716, -0.1349932991356362910, -1.911059701570053226 ) ) ;
#104455 = VERTEX_POINT ( 'NONE', #204637 ) ;
#104456 = CARTESIAN_POINT ( 'NONE',  ( -4.261005416444848315, 8.193199762486115034, 0.7998128361456352531 ) ) ;
#104458 = CYLINDRICAL_SURFACE ( 'NONE', #65078, 1.500000000000000222 ) ;
#104457 = CARTESIAN_POINT ( 'NONE',  ( -4.930325137224961907, 5.781076077297750970, -1.199719254218453823 ) ) ;
#104460 = CARTESIAN_POINT ( 'NONE',  ( 5.926322542504858681, 8.007405281046052536, -1.443375672974078761 ) ) ;
#104459 = CARTESIAN_POINT ( 'NONE',  ( 8.606728586576791074, 8.935604860628076906, 0.7998128361456462443 ) ) ;
#104462 = EDGE_LOOP ( 'NONE', ( #16810, #104165 ) ) ;
#104461 = CARTESIAN_POINT ( 'NONE',  ( 5.549440478958017842, -1.726947976793650197, 0.8215754744917986852 ) ) ;
#104463 = CARTESIAN_POINT ( 'NONE',  ( 1.237671066534186792, -1.994493743981802680, 0.9446329514863486265 ) ) ;
#104464 = MECHANICAL_DESIGN_GEOMETRIC_PRESENTATION_REPRESENTATION (  '', ( #31953 ), #118433 ) ;
#104465 = CARTESIAN_POINT ( 'NONE',  ( 1.445367865410934982, 8.714818166637854802, 2.590103969856952126 ) ) ;
#104466 = CARTESIAN_POINT ( 'NONE',  ( -0.005422908085399994089, -1.854866876809873943, -0.4647201794698225252 ) ) ;
#104467 = CARTESIAN_POINT ( 'NONE',  ( 0.07680821025393863577, 2.892152076732486421, -2.299782885777381658 ) ) ;
#104468 = CARTESIAN_POINT ( 'NONE',  ( 10.98676690055266114, -7.666862915010303148, -0.5459353850038921596 ) ) ;
#104469 = CARTESIAN_POINT ( 'NONE',  ( 0.000000000000000000, 1.000000000000000888, 0.000000000000000000 ) ) ;
#104470 = CARTESIAN_POINT ( 'NONE',  ( 2.682155120989743402, -1.190029146579720587, -1.693995171316540427 ) ) ;
#104471 = CARTESIAN_POINT ( 'NONE',  ( -6.144869935491728441, 8.192100896205577243, -1.599625672291263179 ) ) ;
#104472 = CARTESIAN_POINT ( 'NONE',  ( -4.756313517479579644, 8.198030745052275137, 0.7332552394410801755 ) ) ;
#104474 = CARTESIAN_POINT ( 'NONE',  ( 0.9542513359644848592, 2.159166806557303531, -0.1069676271590186134 ) ) ;
#104473 = CARTESIAN_POINT ( 'NONE',  ( -3.391510981712833939, 7.108513245306943062, 0.7998128361456341429 ) ) ;
#104475 = CARTESIAN_POINT ( 'NONE',  ( -11.56045418304177197, 8.213790699071104484, -3.228785083172883486 ) ) ;
#104476 = CARTESIAN_POINT ( 'NONE',  ( 4.068855497876973537, 7.761098824249525130, -0.7216878364870338292 ) ) ;
#104477 = ADVANCED_FACE ( 'NONE', ( #23769 ), #172574, .T. ) ;
#104478 = CARTESIAN_POINT ( 'NONE',  ( 0.000000000000000000, 7.849261790823902629, 0.000000000000000000 ) ) ;
#104479 = CARTESIAN_POINT ( 'NONE',  ( -1.402160292154681736E-14, 12.73437500034139980, 1.575800808251682339 ) ) ;
#104481 = CARTESIAN_POINT ( 'NONE',  ( -6.154475385960665790, 6.144919136567696505, 0.000000000000000000 ) ) ;
#104480 = CARTESIAN_POINT ( 'NONE',  ( 6.925078400183548588, 0.0006614011395407459748, 1.855452278108092656 ) ) ;
#104482 = CARTESIAN_POINT ( 'NONE',  ( 4.518016650454199201, -1.583040169018738785, 0.7084668738900431473 ) ) ;
#104484 = EDGE_CURVE ( 'NONE', #182295, #101986, #159148, .T. ) ;
#104483 = CIRCLE ( 'NONE', #159831, 12.00000000000000178 ) ;
#104485 = B_SPLINE_CURVE_WITH_KNOTS ( 'NONE', 3,
 ( #85493, #15150, #81236, #214381, #150517, #165684, #31432, #2078, #132160, #134285, #200290, #181913, #114862, #149434, #51941, #35669, #101748, #167815, #19415, #97509, #180862, #32484 ),
 .UNSPECIFIED., .F., .F.,
 ( 4, 3, 3, 3, 3, 3, 3, 4 ),
 ( 0.000000000000000000, 1.209865308640392985E-05, 2.418763075657826564E-05, 3.626888754243231552E-05, 5.481069466191479497E-05, 8.058589917395160660E-05, 0.0001081451638904113897, 0.0001095998438940794050 ),
 .UNSPECIFIED. ) ;
#104486 = CARTESIAN_POINT ( 'NONE',  ( -4.952806187693842510, 4.672695395264567786, 0.7998128361456341429 ) ) ;
#104487 = CARTESIAN_POINT ( 'NONE',  ( 3.819242646454374057, -1.823515126939363462, -0.9802443236400715243 ) ) ;
#104488 = CARTESIAN_POINT ( 'NONE',  ( 4.886377882447483501, -0.7144107685513987338, -1.993165935382594789 ) ) ;
#104489 = CARTESIAN_POINT ( 'NONE',  ( 8.125414133291656071, 8.374071331795406081, -0.7998128361456291469 ) ) ;
#104490 = CARTESIAN_POINT ( 'NONE',  ( -0.6823417656250212460, 4.551041667008086655, 1.181850606188767472 ) ) ;
#104491 = CARTESIAN_POINT ( 'NONE',  ( 1.340603599695965764, -1.920222134930357427, -0.4367614745469716730 ) ) ;
#104492 = CARTESIAN_POINT ( 'NONE',  ( 0.4395310841842986482, -1.815173276516975243, 0.6020934215927520317 ) ) ;
#104493 = CARTESIAN_POINT ( 'NONE',  ( 4.664210274407590617, -1.499448637150493813, 1.733910808658318814 ) ) ;
#104494 = CARTESIAN_POINT ( 'NONE',  ( 1.910518402784128433, 1.353611321597010253, -1.225282022559864625 ) ) ;
#104495 = CARTESIAN_POINT ( 'NONE',  ( 3.718679271898170491, 7.560485927181699317, 0.7998128361456271485 ) ) ;
#104496 = CARTESIAN_POINT ( 'NONE',  ( 5.138177029454841893, 7.017625839162543677, 1.443375672974062551 ) ) ;
#104497 = CARTESIAN_POINT ( 'NONE',  ( -7.640183256500752584, 8.872300873127729304, -1.199719254218446718 ) ) ;
#104498 = CARTESIAN_POINT ( 'NONE',  ( 2.338141740155843085, -1.162522942608142928, -1.643444077351646326 ) ) ;
#104499 = CARTESIAN_POINT ( 'NONE',  ( 3.537899350542179189, 1.241011212050652901, 1.519374649786103149 ) ) ;
#104500 = CARTESIAN_POINT ( 'NONE',  ( -7.531718027591449705, 8.745758106066849891, 1.199719254218462483 ) ) ;
#104501 = CARTESIAN_POINT ( 'NONE',  ( -3.899941742225307539, 7.701682465904834629, 0.7998128361456341429 ) ) ;
#104502 = CARTESIAN_POINT ( 'NONE',  ( 0.07556134207192893859, 0.6772206542668850471, -2.324809334106460845 ) ) ;
#104504 = CARTESIAN_POINT ( 'NONE',  ( 4.434285456697817374, 1.735847377751572385, 0.3442416992474469084 ) ) ;
#104503 = CARTESIAN_POINT ( 'NONE',  ( 5.912080347638632993, 1.404955882617323848, -1.548356120136730851 ) ) ;
#104505 = CARTESIAN_POINT ( 'NONE',  ( -0.6125000000000019318, 2.291666666666664298, 1.060881119635910252 ) ) ;
#104506 = CARTESIAN_POINT ( 'NONE',  ( 0.4456111923471539615, 0.6836232613432814409, -2.082162021007263331 ) ) ;
#104507 = CARTESIAN_POINT ( 'NONE',  ( 6.369106938980155341, 1.663098657370492672, -0.5127371055620026929 ) ) ;
#104508 = AXIS2_PLACEMENT_3D ( 'NONE', #22994, #9964, #88024 ) ;
#104509 = CARTESIAN_POINT ( 'NONE',  ( 7.287671262545424966, 8.461036880179857889, -1.199719254218451159 ) ) ;
#104510 = CARTESIAN_POINT ( 'NONE',  ( 0.1331715793776600265, 0.003733371859311259821, -1.953671397793784070 ) ) ;
#104511 = CARTESIAN_POINT ( 'NONE',  ( 6.469376040731918742, -2.253416215261240918, -0.4533134382209720314 ) ) ;
#104512 = CARTESIAN_POINT ( 'NONE',  ( 0.1333692844072801587, 4.087911462428309051, -2.608372271572469092 ) ) ;
#104513 = CARTESIAN_POINT ( 'NONE',  ( 6.749374558768074017, -1.701276501228730309, -0.3333242692393871831 ) ) ;
#104514 = CARTESIAN_POINT ( 'NONE',  ( 2.051678093609669240, -1.773579625386853875, -1.313098587465796774 ) ) ;
#104515 = CARTESIAN_POINT ( 'NONE',  ( 6.391115334191724173, 0.2064332055253786102, 2.161336459811058042 ) ) ;
#104516 = CARTESIAN_POINT ( 'NONE',  ( -0.1000000000000028644, -9.900000000000005684, 0.000000000000000000 ) ) ;
#104517 = CARTESIAN_POINT ( 'NONE',  ( 1.675176079212177260, 1.839371217556123650, -1.048680071690030413 ) ) ;
#104518 = CARTESIAN_POINT ( 'NONE',  ( 4.375000000000001776, 2.052068128417944504, -2.491713675105573160E-13 ) ) ;
#104519 = CARTESIAN_POINT ( 'NONE',  ( -0.007473969438217894709, 8.279395425053857949, -1.999986034896452880 ) ) ;
#104520 = CARTESIAN_POINT ( 'NONE',  ( 4.559546607354286074, 0.4225000031176616710, -1.879333123156016860 ) ) ;
#104521 = EDGE_LOOP ( 'NONE', ( #117168, #148098, #15467, #65123 ) ) ;
#104523 = CARTESIAN_POINT ( 'NONE',  ( -1.201851678989727383E-14, 5.087500000000019007, -1.732050807568863648 ) ) ;
#104522 = CARTESIAN_POINT ( 'NONE',  ( 1.488225144363482189, -2.281859108288700089, -0.2192131398826550337 ) ) ;
#104524 = CARTESIAN_POINT ( 'NONE',  ( 5.606460214450851964, 6.499623990736163037, 1.199719254218462483 ) ) ;
#104525 = CARTESIAN_POINT ( 'NONE',  ( 6.494519276145969577, 7.535692896047149425, -1.199719254218446718 ) ) ;
#104526 = CARTESIAN_POINT ( 'NONE',  ( 3.985193088136604889, -2.072824570928345711, -0.7989420372410382942 ) ) ;
#104527 = CARTESIAN_POINT ( 'NONE',  ( -9.002250809794006159, 10.56534270192358704, -1.082531754730543971 ) ) ;
#104528 = SURFACE_STYLE_USAGE ( .BOTH. , #4836 ) ;
#104529 = CARTESIAN_POINT ( 'NONE',  ( 7.131225611108096274, 8.382479970123348778, 1.082531754730558626 ) ) ;
#104530 = CARTESIAN_POINT ( 'NONE',  ( -7.171900071504738072, 10.35067193585544665, -1.082531754730543083 ) ) ;
#104531 = CARTESIAN_POINT ( 'NONE',  ( 6.888951449519509218, 7.209733910627123876, -0.7216878364870317197 ) ) ;
#104532 = CARTESIAN_POINT ( 'NONE',  ( 1.828750219146151323, 0.7691198443132395424, -1.864169014999479623 ) ) ;
#104534 = CARTESIAN_POINT ( 'NONE',  ( 0.3915631436273382948, -1.887207296038289961, 0.8326094146433449250 ) ) ;
#104533 = CARTESIAN_POINT ( 'NONE',  ( 8.599949509769960088, 8.927695937686774386, 1.040834085586084257E-14 ) ) ;
#104535 = CARTESIAN_POINT ( 'NONE',  ( -10.89423718502888860, -6.453216945989406206, 0.03415196713902314551 ) ) ;
#104536 = CARTESIAN_POINT ( 'NONE',  ( 5.465345319640213972, 8.429967735338637524, -1.082531754730548412 ) ) ;
#104537 = CARTESIAN_POINT ( 'NONE',  ( 0.3097736896383457839, 1.270387085892955792, -1.333027339516623888 ) ) ;
#104538 = CARTESIAN_POINT ( 'NONE',  ( -10.98549472050129694, 13.75729797278727773, -1.592011381755360722 ) ) ;
#104539 = CARTESIAN_POINT ( 'NONE',  ( -1.364683531250012516, 2.030208333674750953, 0.7879004041258379498 ) ) ;
#104540 = CARTESIAN_POINT ( 'NONE',  ( 1.651228947852514173, 0.5200303365089484764, -1.691588852159523704 ) ) ;
#104541 = CARTESIAN_POINT ( 'NONE',  ( 0.1412502902482688505, 0.7743183493036235321, 1.862015731718666078 ) ) ;
#104542 = CARTESIAN_POINT ( 'NONE',  ( 6.374529642495492254, -0.09526421964337064563, -1.737987611564382862 ) ) ;
#104543 = CARTESIAN_POINT ( 'NONE',  ( 4.265347265089792117, 2.223640956194427254, -0.5566138344911036873 ) ) ;
#104544 = CARTESIAN_POINT ( 'NONE',  ( 3.872867692073681756, 1.733033312621637068, -0.6219614626309655225 ) ) ;
#104545 = CARTESIAN_POINT ( 'NONE',  ( 7.574201371528760163, 11.98831870009225931, 1.040834085586084257E-14 ) ) ;
#104546 = CARTESIAN_POINT ( 'NONE',  ( 7.879630799735125812, 14.91438228929072274, -9.066625182108625225 ) ) ;
#104547 = CARTESIAN_POINT ( 'NONE',  ( 4.647361241834577328, -1.411646026218037253, -1.157555111390089264 ) ) ;
#104548 = EDGE_CURVE ( 'NONE', #205532, #73290, #194693, .T. ) ;
#104549 = CARTESIAN_POINT ( 'NONE',  ( 5.133435478496918947, 0.5880181904946503169, 1.928752423557971829 ) ) ;
#104550 = CARTESIAN_POINT ( 'NONE',  ( -8.157201976916404362, 12.66848607304450702, -0.7998128361456281477 ) ) ;
#104552 = CARTESIAN_POINT ( 'NONE',  ( -7.553827861469316396, 8.841829255582865699, -1.199719254218452047 ) ) ;
#104551 = CARTESIAN_POINT ( 'NONE',  ( 3.046068780686244981, 0.8155736813739141722, -2.110571434806473690 ) ) ;
#104553 = CARTESIAN_POINT ( 'NONE',  ( 6.141652715049399802, -1.522797514780509065, -1.454946885519771582 ) ) ;
#104554 = CARTESIAN_POINT ( 'NONE',  ( 10.11573063517565707, 13.81601979175187545, 7.347423794093835170 ) ) ;
#104555 = CARTESIAN_POINT ( 'NONE',  ( 3.912603064140641074, 0.7423916865902054907, 1.932869565047180549 ) ) ;
#104556 = CARTESIAN_POINT ( 'NONE',  ( 2.530568227245037605, 6.104080031761181857, 0.000000000000000000 ) ) ;
#104557 = CARTESIAN_POINT ( 'NONE',  ( 1.360316468749957597, 1.276041667008120051, 0.7853790794158580502 ) ) ;
#104558 = CARTESIAN_POINT ( 'NONE',  ( 5.602226918196428151, -0.9533447246646039597, 1.894147766696724799 ) ) ;
#104559 = ITEM_DEFINED_TRANSFORMATION ( 'NONE', 'NONE', #128323,  #200407 ) ;
#104561 = CARTESIAN_POINT ( 'NONE',  ( 2.543477943364984117, -1.427709268621931260, -1.293647605089723429 ) ) ;
#104560 = CARTESIAN_POINT ( 'NONE',  ( -9.826962411806732689, 10.35921099006301382, -0.7998128361456291469 ) ) ;
#104562 = DIRECTION ( 'NONE',  ( 0.000000000000000000, 1.000000000000000000, 0.000000000000000000 ) ) ;
#104563 = CARTESIAN_POINT ( 'NONE',  ( 0.4671662993806492414, 1.711898730999446228, 0.9738141270322558940 ) ) ;
#104564 = CARTESIAN_POINT ( 'NONE',  ( 5.872089928050205465, 6.023395468912922546, -0.7216878364870458196 ) ) ;
#104565 = CARTESIAN_POINT ( 'NONE',  ( 5.833718835943604297, 6.012594516355426855, -0.4067158398524447493 ) ) ;
#104566 = CARTESIAN_POINT ( 'NONE',  ( -0.8368079278675620847, 2.800000000000018918, -1.135296483310510585 ) ) ;
#104567 = CARTESIAN_POINT ( 'NONE',  ( -5.037017762676898158, 5.835274463666530131, -1.199719254218446718 ) ) ;
#104568 = CARTESIAN_POINT ( 'NONE',  ( 0.1939906290522614152, 2.069702213058471241, -0.8072921158600793179 ) ) ;
#104569 = CARTESIAN_POINT ( 'NONE',  ( 3.381953601626528361, 1.334784698733671560, 1.628938261321200232 ) ) ;
#104570 = CARTESIAN_POINT ( 'NONE',  ( -4.679499295372141709, 5.488445928469455559, 1.199719254218452935 ) ) ;
#104571 = CARTESIAN_POINT ( 'NONE',  ( 6.751070424600909448, 9.963667031088037973, -1.199719254218441611 ) ) ;
#104572 = CARTESIAN_POINT ( 'NONE',  ( 0.4142149233586078227, 0.7067589711089922178, 1.721844540100337717 ) ) ;
#104573 = CARTESIAN_POINT ( 'NONE',  ( 7.124973419181436007, 8.271222729588529887, -1.199719254218446718 ) ) ;
#104574 = CARTESIAN_POINT ( 'NONE',  ( 3.714044015139744914, 6.420469553383295391, 1.199719254218462483 ) ) ;
#104575 = CARTESIAN_POINT ( 'NONE',  ( -5.289089323106922258, 9.184704953684462936, 0.7216878364870267237 ) ) ;
#104576 = CARTESIAN_POINT ( 'NONE',  ( -8.351459436338037889, 10.76645531385962862, -1.443375672974059665 ) ) ;
#104577 = CIRCLE ( 'NONE', #45838, 1.500000000000005107 ) ;
#104578 = CARTESIAN_POINT ( 'NONE',  ( 1.037531286769650452, -0.04638328994046451298, 2.120250110247793085 ) ) ;
#104579 = CARTESIAN_POINT ( 'NONE',  ( -5.562588163356775972, 9.711712967216715953, 0.7998128361456291469 ) ) ;
#104581 = CARTESIAN_POINT ( 'NONE',  ( 3.068751266904270025, 1.422870340827029345, -1.350941015047700366 ) ) ;
#104580 = CARTESIAN_POINT ( 'NONE',  ( -0.6125000000000262457, 1.208333333333311277, -1.060881119635962211 ) ) ;
#104582 = CARTESIAN_POINT ( 'NONE',  ( 2.641676655999642076, -1.601130012699041982, -1.452526871000489495 ) ) ;
#104583 = CARTESIAN_POINT ( 'NONE',  ( 1.171164436615620863, 1.096940724416964885, 1.478650282607060440 ) ) ;
#104585 = CARTESIAN_POINT ( 'NONE',  ( -5.266540691475234404, 6.417032612176464923, -1.150853802781536039 ) ) ;
#104584 = CARTESIAN_POINT ( 'NONE',  ( -4.309512724297390740, 6.121127159803966933, 1.599625672291270506 ) ) ;
#104586 = CARTESIAN_POINT ( 'NONE',  ( 4.013389373331836651, -0.8969206028703354816, -1.491242602974415243 ) ) ;
#104587 = CARTESIAN_POINT ( 'NONE',  ( 4.026408433578586354, 7.641300905909586660, 1.040834085586084257E-14 ) ) ;
#104588 = CARTESIAN_POINT ( 'NONE',  ( -10.60630082101195804, 5.715768461961713953, -4.896526734066639186 ) ) ;
#104589 = ADVANCED_FACE ( 'NONE', ( #152500 ), #24510, .F. ) ;
#104590 = CARTESIAN_POINT ( 'NONE',  ( 1.305796196612364124, -0.5247483525172502716, 2.096912610238470975 ) ) ;
#104591 = CARTESIAN_POINT ( 'NONE',  ( 3.110703712691643918, 0.7282687159771012997, -1.880146464672841411 ) ) ;
#104592 = CARTESIAN_POINT ( 'NONE',  ( -10.27671724903424888, 11.09185100006920877, 1.040834085586084257E-14 ) ) ;
#104593 = CARTESIAN_POINT ( 'NONE',  ( 0.6905621207787122628, -2.145541755201633372, -0.2633910710312590275 ) ) ;
#104594 = CARTESIAN_POINT ( 'NONE',  ( 1.920718329235811872, 1.838843090712917405, 0.7113003943867537426 ) ) ;
#104595 = CARTESIAN_POINT ( 'NONE',  ( 6.609000000000047947, 3.700659725723095761, 2.414405743007182359 ) ) ;
#104596 = CARTESIAN_POINT ( 'NONE',  ( 2.349080241353004528, 0.5156090978439072936, -1.872316843566106614 ) ) ;
#104599 = EDGE_LOOP ( 'NONE', ( #185932, #61332, #44253, #176417, #23994, #214248, #209544 ) ) ;
#104598 = CARTESIAN_POINT ( 'NONE',  ( -5.207740401424942434, 6.208690235484773723, 1.082531754730549078 ) ) ;
#104597 = CARTESIAN_POINT ( 'NONE',  ( 6.416268857797894576, -1.911816439625917852, 0.05404522429636184067 ) ) ;
#104600 = CARTESIAN_POINT ( 'NONE',  ( -3.811250578772981346, 6.500190537660166079, -1.082531754730546636 ) ) ;
#104601 = CARTESIAN_POINT ( 'NONE',  ( 4.899292406491845497, 6.809203455697518947, -1.599625672291273171 ) ) ;
#104602 = CARTESIAN_POINT ( 'NONE',  ( -6.089547271193396227, 7.133501900260939443, -1.199719254218453823 ) ) ;
#104603 = CARTESIAN_POINT ( 'NONE',  ( -5.596483547390937119, 9.751257581923240991, 0.000000000000000000 ) ) ;
#104604 = CARTESIAN_POINT ( 'NONE',  ( -6.638014823939186293, 6.741195553212168790, -0.1154932285401210346 ) ) ;
#104605 = CARTESIAN_POINT ( 'NONE',  ( 0.4291286860223576527, 2.112415399404877547, 0.6383354507134838540 ) ) ;
#104606 = LINE ( 'NONE', #204185, #25312 ) ;
#104607 = ADVANCED_FACE ( 'NONE', ( #174118 ), #185178, .T. ) ;
#104608 = CARTESIAN_POINT ( 'NONE',  ( 4.082823661314609609, 1.861412734803047142, 0.6194944872321901386 ) ) ;
#104609 = CARTESIAN_POINT ( 'NONE',  ( 7.283754839039659146, 9.520799950344851936, -1.599625672291262513 ) ) ;
#104610 = CARTESIAN_POINT ( 'NONE',  ( 1.582657950916711131, -0.6767122143778031562, 1.899619169727875700 ) ) ;
#104611 = ORIENTED_EDGE ( 'NONE', *, *, #198277, .T. ) ;
#104612 = CARTESIAN_POINT ( 'NONE',  ( 2.430995767774553062, -1.757534028733166442, 1.180493747047051567 ) ) ;
#104613 = CARTESIAN_POINT ( 'NONE',  ( -0.7500000000000006661, 1.639583334016154970, -1.299038105676652011 ) ) ;
#104614 = CARTESIAN_POINT ( 'NONE',  ( -5.530836599371015794, 8.540060901653093950, 1.199719254218452047 ) ) ;
#104615 = CARTESIAN_POINT ( 'NONE',  ( 2.906014618889841916, 1.333239036598636185, -1.269987479889052917 ) ) ;
#104616 = ORIENTED_EDGE ( 'NONE', *, *, #3410, .T. ) ;
#104617 = CARTESIAN_POINT ( 'NONE',  ( -10.32183501870554387, 10.93656236477829502, 0.7998128361456462443 ) ) ;
#104618 = FACE_OUTER_BOUND ( 'NONE', #204787, .T. ) ;
#104619 = CARTESIAN_POINT ( 'NONE',  ( 3.709332143218791789, 1.789599998243587731, -1.137392358348317201 ) ) ;
#104620 = CARTESIAN_POINT ( 'NONE',  ( 0.3043191165176573620, 1.600368420507289668, 0.9101283655772866021 ) ) ;
#104621 = CARTESIAN_POINT ( 'NONE',  ( -1.201851678989727383E-14, 5.618750000682818602, -1.732050807568863648 ) ) ;
#104622 = CARTESIAN_POINT ( 'NONE',  ( 7.623762449586013901, 7.788811034138823253, 1.040834085586084257E-14 ) ) ;
#104623 = CARTESIAN_POINT ( 'NONE',  ( 4.323548078123999439, -1.973147536489193499, 0.5946332991794788247 ) ) ;
#104624 = AXIS2_PLACEMENT_3D ( 'NONE', #153490, #169727, #20264 ) ;
#104626 = CARTESIAN_POINT ( 'NONE',  ( 1.065666191918061445, -1.167978014494171823, 1.423405568861766168 ) ) ;
#104625 = CARTESIAN_POINT ( 'NONE',  ( -5.554036483092550824, 9.631459663583308739, -0.7998128361456231517 ) ) ;
#104627 = CARTESIAN_POINT ( 'NONE',  ( 1.364683531249988535, 5.405208333674750953, -0.7879004041258300672 ) ) ;
#104628 = SURFACE_SIDE_STYLE ('',( #136060 ) ) ;
#104629 = CARTESIAN_POINT ( 'NONE',  ( 1.500000000000035971, 7.750000000000000000, 10.64483442802187696 ) ) ;
#104630 = CARTESIAN_POINT ( 'NONE',  ( 10.99943592164172657, -8.407420853759269619, -0.1113975120798851026 ) ) ;
#104631 = CARTESIAN_POINT ( 'NONE',  ( 0.7334016978863610037, 0.1661181961954381059, 2.200687262777756725 ) ) ;
#104632 = CARTESIAN_POINT ( 'NONE',  ( 3.708526512723071544, -0.9128432734063509635, -2.070237398927244676 ) ) ;
#104633 = CARTESIAN_POINT ( 'NONE',  ( -7.917598520700757980, 9.299915031314755609, 1.082531754730558626 ) ) ;
#104634 = CARTESIAN_POINT ( 'NONE',  ( 3.111360644411143017, 1.430921235420354654, 1.110905701166440940 ) ) ;
#104635 = CARTESIAN_POINT ( 'NONE',  ( 3.995261062014230813, -0.3217480215693402368, 1.888325751980689082 ) ) ;
#104636 = CARTESIAN_POINT ( 'NONE',  ( 5.687960312649480876, -1.310561514506687564, -1.602779375087557412 ) ) ;
#104637 = CARTESIAN_POINT ( 'NONE',  ( -1.364683531250010295, 4.342708333674753618, 0.7879004041258379498 ) ) ;
#104638 = CARTESIAN_POINT ( 'NONE',  ( 3.362146542844654196, 0.8852860682435258477, 1.761578244261922332 ) ) ;
#104639 = CARTESIAN_POINT ( 'NONE',  ( 1.553604983729965472, 0.5615451523532221101, -1.842721482554928514 ) ) ;
#104640 = CARTESIAN_POINT ( 'NONE',  ( 3.643291952642300213, -1.415932857957047375, -1.222571138756740838 ) ) ;
#104641 = CARTESIAN_POINT ( 'NONE',  ( 3.809432652880593739, 1.978559473273227232, 1.187534574604662607 ) ) ;
#104642 = CARTESIAN_POINT ( 'NONE',  ( 3.613571450151699782, 0.4543224947703514149, -1.804596983994880333 ) ) ;
#104643 = CARTESIAN_POINT ( 'NONE',  ( 1.364683531249988535, 3.863541667008087543, 0.7879004041258500513 ) ) ;
#104644 = AXIS2_PLACEMENT_3D ( 'NONE', #191449, #139538, #43114 ) ;
#104645 = DIRECTION ( 'NONE',  ( -0.05872483221476467591, -7.952201780260630618E-17, 0.9982742078614211811 ) ) ;
#104646 = CARTESIAN_POINT ( 'NONE',  ( 1.682391906368089662, -1.125439293035620292, 1.779948400507038953 ) ) ;
#104647 = CARTESIAN_POINT ( 'NONE',  ( 4.324687812634897988, 4.147816657603229373, 0.7216878364870317197 ) ) ;
#104649 = CARTESIAN_POINT ( 'NONE',  ( 1.500000000000001332, 8.875000000000001776, 0.000000000000000000 ) ) ;
#104648 = CARTESIAN_POINT ( 'NONE',  ( -1.001543065824772872E-14, 5.634375000341415252, 1.575800808251672791 ) ) ;
#104650 = CARTESIAN_POINT ( 'NONE',  ( 1.290813828370756866, 4.079998697030315924, 0.4579576469030108843 ) ) ;
#104651 = CARTESIAN_POINT ( 'NONE',  ( -9.602438852202270780, -9.449361760816694655, 0.1964824153909955906 ) ) ;
#104652 = CARTESIAN_POINT ( 'NONE',  ( 0.3342475891858322501, -1.084071894752016041, -1.704023929676929727 ) ) ;
#104653 = CARTESIAN_POINT ( 'NONE',  ( -1.201851678989727383E-14, 0.8218750003414171390, 1.575800808251672791 ) ) ;
#104654 = CARTESIAN_POINT ( 'NONE',  ( -3.307826292054310890, 5.842585859829892314, -1.082531754730549967 ) ) ;
#104655 = CARTESIAN_POINT ( 'NONE',  ( 6.322179702674084467, 6.270297829408224111, 1.040834085586084257E-14 ) ) ;
#104656 = ORIENTED_EDGE ( 'NONE', *, *, #193595, .T. ) ;
#104657 = CARTESIAN_POINT ( 'NONE',  ( 1.159701560084012595, 0.4228694819443152286, -2.119656415666733906 ) ) ;
#104658 = DIRECTION ( 'NONE',  ( 0.000000000000000000, -0.7999999999999973799, -0.6000000000000034195 ) ) ;
#104659 = EDGE_CURVE ( 'NONE', #96352, #152273, #126775, .T. ) ;
#104662 = DIRECTION ( 'NONE',  ( 0.6507913734559651608, 0.7592566023652994600, 1.725633230170963543E-31 ) ) ;
#104661 = CARTESIAN_POINT ( 'NONE',  ( 6.559000000000036579, 7.629137130509070275, 2.600000000000001421 ) ) ;
#104660 = CARTESIAN_POINT ( 'NONE',  ( 5.682802662783380754, 6.658966523782627434, 1.199719254218452935 ) ) ;
#104663 = CARTESIAN_POINT ( 'NONE',  ( 11.86145016429273191, 13.40000000000000036, 1.099999999999996758 ) ) ;
#104664 = CARTESIAN_POINT ( 'NONE',  ( 6.280482454654814362, -0.5424645211669875122, -1.942098458069536848 ) ) ;
#104665 = CARTESIAN_POINT ( 'NONE',  ( -6.887178846062105286, 10.97886638714038554, -0.7216878364870267237 ) ) ;
#104666 = CARTESIAN_POINT ( 'NONE',  ( -0.05867695357848409787, -1.698172713885632401, -1.384993232510664640 ) ) ;
#104667 = DIRECTION ( 'NONE',  ( -1.000000000000000000, 7.771561172376094797E-16, -3.330669073875481454E-16 ) ) ;
#104669 = CARTESIAN_POINT ( 'NONE',  ( -1.364683531250014514, 12.08854166700806765, -0.7879004041258335089 ) ) ;
#104668 = CARTESIAN_POINT ( 'NONE',  ( 0.07556134207191073093, -0.004209888912004143384, -2.244269416743961187 ) ) ;
#104670 = CARTESIAN_POINT ( 'NONE',  ( -9.982881178363895103, 10.54111621771303753, 1.040834085586084257E-14 ) ) ;
#104671 = CARTESIAN_POINT ( 'NONE',  ( -6.195713011320804320, 7.291048603704809672, -1.082531754730543083 ) ) ;
#104672 = CARTESIAN_POINT ( 'NONE',  ( -1.402160292154681736E-14, 1.509375000341420359, -1.575800808251659024 ) ) ;
#104673 = CARTESIAN_POINT ( 'NONE',  ( -2.788906526875773208E-15, 9.437499999999998224, -1.499999999999998446 ) ) ;
#104674 = STYLED_ITEM ( 'NONE', ( #25945 ), #175851 ) ;
#104675 = CARTESIAN_POINT ( 'NONE',  ( -1.500000000000015099, 9.979166666666671404, -0.8660254037844309360 ) ) ;
#104676 = CARTESIAN_POINT ( 'NONE',  ( 2.472937804810691809, 0.08526638500995675773, -1.722893361390212874 ) ) ;
#104677 = CARTESIAN_POINT ( 'NONE',  ( 5.564695703766185275, 5.456842840674144490, 0.000000000000000000 ) ) ;
#104678 = CARTESIAN_POINT ( 'NONE',  ( 2.125891686596991903, 1.023501848097716493, -1.443529828085978739 ) ) ;
#104679 = CARTESIAN_POINT ( 'NONE',  ( 2.561191855132368467, -1.672464352163150147, 1.120165047906955147 ) ) ;
#104680 = CARTESIAN_POINT ( 'NONE',  ( 5.807716119225245777, -0.5415507062403871474, 2.139171552897000339 ) ) ;
#104681 = ORIENTED_EDGE ( 'NONE', *, *, #201896, .F. ) ;
#104682 = CARTESIAN_POINT ( 'NONE',  ( 4.254169105220822367, 0.8597269205913078416, -1.827796444439087287 ) ) ;
#104683 = CARTESIAN_POINT ( 'NONE',  ( -7.747558435566414659, 8.003516027774422170, -0.7998128361456362523 ) ) ;
#104685 = CARTESIAN_POINT ( 'NONE',  ( 3.655875201264874974, 1.122517324909186431, 1.674876314423722423 ) ) ;
#104684 = CARTESIAN_POINT ( 'NONE',  ( 4.547591073264711348, -1.938359017324686961, 0.8602097090630378418 ) ) ;
#104687 = ORIENTED_EDGE ( 'NONE', *, *, #178265, .F. ) ;
#104686 = CARTESIAN_POINT ( 'NONE',  ( 4.711091175174894730, 1.502108783192051877, -1.012348896329213765 ) ) ;
#104688 = CARTESIAN_POINT ( 'NONE',  ( 4.736594563127852098, 6.619389305106191834, -1.599625672291273171 ) ) ;
#104689 = ORIENTED_EDGE ( 'NONE', *, *, #100082, .T. ) ;
#104690 = CARTESIAN_POINT ( 'NONE',  ( 0.9185735243398345240, 1.726912363944958617, 0.7195956246372690046 ) ) ;
#104691 = CARTESIAN_POINT ( 'NONE',  ( -10.91944941500665678, -9.999999999999994671, 0.1017788107271379444 ) ) ;
#104692 = CARTESIAN_POINT ( 'NONE',  ( -0.1759689521645991239, -0.7750936178016191169, -1.636263868569738600 ) ) ;
#104693 = CARTESIAN_POINT ( 'NONE',  ( -4.437596350374534815, 4.071617251725375475, -0.7998128361456221525 ) ) ;
#104694 = CARTESIAN_POINT ( 'NONE',  ( -10.32649671959996596, 5.020010808682577874, -7.354824260697566451 ) ) ;
#104695 = CARTESIAN_POINT ( 'NONE',  ( 0.4359479416626659276, -6.334709917115469935, 9.855659161987908590 ) ) ;
#104696 = CARTESIAN_POINT ( 'NONE',  ( -0.6823417656250212460, 3.113541667008084879, 1.181850606188767472 ) ) ;
#104697 = CARTESIAN_POINT ( 'NONE',  ( 0.1758378621803426134, 1.891278220088285833, -0.2826890867150752551 ) ) ;
#104698 = ADVANCED_FACE ( 'NONE', ( #44388 ), #77934, .T. ) ;
#104699 = CARTESIAN_POINT ( 'NONE',  ( 6.373741612200162443, 8.529394195690610303, 1.443375672974065660 ) ) ;
#104700 = CARTESIAN_POINT ( 'NONE',  ( -4.340018570150318666, 6.156717313299049366, -1.443375672974066548 ) ) ;
#104701 = CARTESIAN_POINT ( 'NONE',  ( -6.394605727500880299, 7.489403432619674561, -1.199719254218452047 ) ) ;
#104702 = CARTESIAN_POINT ( 'NONE',  ( 3.990573222356631256, -1.218298518170106925, 1.735533685479621502 ) ) ;
#104704 = CARTESIAN_POINT ( 'NONE',  ( -10.60630588279735242, 5.715763139788331948, 4.896273837757428637 ) ) ;
#104703 = CARTESIAN_POINT ( 'NONE',  ( -0.02968770228140016343, 0.2527710104786498047, -1.861515397111657144 ) ) ;
#104706 = EDGE_CURVE ( 'NONE', #138593, #17304, #213613, .T. ) ;
#104705 = CARTESIAN_POINT ( 'NONE',  ( 5.553970887368382847, 1.969207887765548559, -0.09415503477229987539 ) ) ;
#104707 = CARTESIAN_POINT ( 'NONE',  ( -0.6823417656250003738, 0.7177083336747519526, -1.181850606188749264 ) ) ;
#104708 = CARTESIAN_POINT ( 'NONE',  ( 0.6330651387380836770, 1.861715503769780566, 0.7666268175344230773 ) ) ;
#104709 = ORIENTED_EDGE ( 'NONE', *, *, #93908, .T. ) ;
#104710 = CARTESIAN_POINT ( 'NONE',  ( 0.01740989766754827417, -1.933669582450600499, 0.8627405663345076858 ) ) ;
#104712 = ADVANCED_FACE ( 'NONE', ( #134188 ), #30216, .T. ) ;
#104711 = CARTESIAN_POINT ( 'NONE',  ( 11.05144304286076640, 8.019042783312965383, 4.564752377278145978 ) ) ;
#104713 = CARTESIAN_POINT ( 'NONE',  ( 1.609917502266303480, 0.6029389078928657497, -1.980602105166151095 ) ) ;
#104714 = ORIENTED_EDGE ( 'NONE', *, *, #77470, .T. ) ;
#104715 = CARTESIAN_POINT ( 'NONE',  ( 3.881377115262159894, 7.750300077773022878, 0.7998128361456271485 ) ) ;
#104716 = CARTESIAN_POINT ( 'NONE',  ( 4.389807875774629942, 8.343469298370917997, 0.7998128361456271485 ) ) ;
#104717 = ORIENTED_EDGE ( 'NONE', *, *, #129217, .F. ) ;
#104719 = CARTESIAN_POINT ( 'NONE',  ( 6.166260936116925606, 6.088392601758203071, 0.7998128361456341429 ) ) ;
#104718 = CARTESIAN_POINT ( 'NONE',  ( 4.874988757033254849, 1.950858131582337007, -0.7520741601412093136 ) ) ;
#104722 = ORIENTED_EDGE ( 'NONE', *, *, #100023, .T. ) ;
#104721 = CARTESIAN_POINT ( 'NONE',  ( 1.875370188833940244, 0.3090493442242334132, -1.784726349569294213 ) ) ;
#104720 = CARTESIAN_POINT ( 'NONE',  ( 3.539906422930443775, 0.8216601389946125433, -1.630302437610211541 ) ) ;
#104723 = CARTESIAN_POINT ( 'NONE',  ( 0.3769810270647707684, 3.049942316455285685, -0.4288785890453113980 ) ) ;
#104724 = DIRECTION ( 'NONE',  ( 0.6762880771785059197, 1.295290445962756284E-12, 0.7366372490352354196 ) ) ;
#104725 = CARTESIAN_POINT ( 'NONE',  ( 4.735508036034060453, -2.019198892066270457, 0.8907332283012432406 ) ) ;
#104726 = CARTESIAN_POINT ( 'NONE',  ( 6.421758314367153275, 10.64380180007036891, -0.7998128361456291469 ) ) ;
#104727 = CARTESIAN_POINT ( 'NONE',  ( -1.364683531250000748, 9.171875000341403350, 0.000000000000000000 ) ) ;
#104728 = CARTESIAN_POINT ( 'NONE',  ( 3.018110381800835018, -1.909997030407738938, 0.09613604992317337228 ) ) ;
#104729 = AXIS2_PLACEMENT_3D ( 'NONE', #199319, #116023, #19509 ) ;
#104730 = CARTESIAN_POINT ( 'NONE',  ( 6.611572464958476836, 10.86525164242692298, 0.7998128361456462443 ) ) ;
#104731 = CARTESIAN_POINT ( 'NONE',  ( 5.986797818411375260, 1.994257276370488219, 0.5558945855626205024 ) ) ;
#104732 = AXIS2_PLACEMENT_3D ( 'NONE', #49252, #165120, #16712 ) ;
#104733 = LINE ( 'NONE', #202181, #132088 ) ;
#104734 = CARTESIAN_POINT ( 'NONE',  ( 6.216381822182693639, 2.044192415450503120, 0.7905562269360306704 ) ) ;
#104735 = CARTESIAN_POINT ( 'NONE',  ( 5.011754246625688580, 8.023990808224052529, -1.135194352273690255 ) ) ;
#104736 = CARTESIAN_POINT ( 'NONE',  ( -3.531151798259720476, 15.47001910837518857, -11.47749989083732203 ) ) ;
#104737 = ORIENTED_EDGE ( 'NONE', *, *, #5273, .F. ) ;
#104738 = FACE_OUTER_BOUND ( 'NONE', #86058, .T. ) ;
#104739 = CARTESIAN_POINT ( 'NONE',  ( 3.128041797164154758, 1.042111378005972311, -1.553157497896196393 ) ) ;
#104740 = CARTESIAN_POINT ( 'NONE',  ( 1.642778471875000035, -1.363541666188707646, -2.845375778867859751 ) ) ;
#104741 = CARTESIAN_POINT ( 'NONE',  ( 6.509000000000010999, 0.004788705324892603143, 2.000274819378269786 ) ) ;
#104742 = ADVANCED_FACE ( 'NONE', ( #70192 ), #182535, .T. ) ;
#104743 = CARTESIAN_POINT ( 'NONE',  ( -7.537970219518083326, 9.817384560903001045, -1.443375672974059665 ) ) ;
#104744 = CARTESIAN_POINT ( 'NONE',  ( 4.573896719763862251, 6.429575154514868274, -1.599625672291273171 ) ) ;
#104745 = CARTESIAN_POINT ( 'NONE',  ( 6.877786287229037399, -2.009644702432196617, 0.4970176993947388322 ) ) ;
#104746 = CARTESIAN_POINT ( 'NONE',  ( 0.6675924852559199651, 1.356316336250670496, 1.492241973137248934 ) ) ;
#104747 = CARTESIAN_POINT ( 'NONE',  ( -10.13202086811422475, 10.71511252242175161, -0.7998128361456291469 ) ) ;
#104748 = CARTESIAN_POINT ( 'NONE',  ( 5.996449078994045223, 10.21788403546024782, 0.7998128361456331437 ) ) ;
#104749 = SURFACE_STYLE_USAGE ( .BOTH. , #188106 ) ;
#104750 = CARTESIAN_POINT ( 'NONE',  ( 1.324469081069843623, 2.112754910877081560, 0.5817525768514880680 ) ) ;
#104751 = CARTESIAN_POINT ( 'NONE',  ( 4.705575438601840688, -0.4840451379145363497, 1.760283039881085809 ) ) ;
#104752 = CARTESIAN_POINT ( 'NONE',  ( -4.192495815123836955, 5.914331089109674089, -1.599625672291256295 ) ) ;
#104753 = CARTESIAN_POINT ( 'NONE',  ( 6.549997609177859559, 6.814287763561861944, 0.000000000000000000 ) ) ;
#104754 = CARTESIAN_POINT ( 'NONE',  ( 4.175548122884573665, 3.973820352894515295, 1.214306433183764966E-14 ) ) ;
#104755 = CARTESIAN_POINT ( 'NONE',  ( -6.303615075710993665, 6.318915441276411471, -0.7998128361456362523 ) ) ;
#104756 = CARTESIAN_POINT ( 'NONE',  ( 3.379006598303866848, 4.965260336153046516, -1.599625672291262513 ) ) ;
#104757 = CARTESIAN_POINT ( 'NONE',  ( 5.252858170651868441, 5.093032385374103299, -0.7998128361456481317 ) ) ;
#104758 = ORIENTED_EDGE ( 'NONE', *, *, #169187, .F. ) ;
#104760 = CARTESIAN_POINT ( 'NONE',  ( 6.117445361114795865, 1.676175193246462802, 1.114809878595341308 ) ) ;
#104759 = CARTESIAN_POINT ( 'NONE',  ( 3.263068207883256466, 1.795673413606920565, -0.4063787724192802209 ) ) ;
#104761 = CARTESIAN_POINT ( 'NONE',  ( 1.722429217803717938, -1.971362081364759655, -1.181495133065799230 ) ) ;
#104763 = CARTESIAN_POINT ( 'NONE',  ( 6.895372015613538075, -1.753720159772365284, 0.8792710811909019153 ) ) ;
#104762 = CARTESIAN_POINT ( 'NONE',  ( 3.714570900464274850, 6.317121236308204324, 1.082531754730558626 ) ) ;
#104764 = CARTESIAN_POINT ( 'NONE',  ( -3.893162665418476109, 7.693773542963529444, 1.040834085586084257E-14 ) ) ;
#104765 = FACE_OUTER_BOUND ( 'NONE', #122081, .T. ) ;
#104766 = CARTESIAN_POINT ( 'NONE',  ( 3.269685606991072468, 0.4601866041431811327, -1.856093204100267124 ) ) ;
#104767 = CARTESIAN_POINT ( 'NONE',  ( -9.378489572351046633, 11.96465713920816043, -1.599625672291263179 ) ) ;
#104768 = CARTESIAN_POINT ( 'NONE',  ( 6.357275476766607980, 6.835366726881293431, -0.6123070361637416026 ) ) ;
#104769 = CARTESIAN_POINT ( 'NONE',  ( -6.780486220610184134, 9.003929572168926754, -1.443375672974066548 ) ) ;
#104771 = CARTESIAN_POINT ( 'NONE',  ( 1.604156678829884886, -0.6703249191640224813, -1.746612230856612769 ) ) ;
#104770 = CARTESIAN_POINT ( 'NONE',  ( 2.507466893629331395, -2.067604658949507179, 0.3094350269009105703 ) ) ;
#104772 = CARTESIAN_POINT ( 'NONE',  ( 1.897814322125553010, 0.1948091626960517242, 2.006652841580962132 ) ) ;
#104773 = CARTESIAN_POINT ( 'NONE',  ( 7.890482213473377193, 11.18901776815221716, -1.082531754730543083 ) ) ;
#104774 = CARTESIAN_POINT ( 'NONE',  ( -0.6823417656249969321, 4.280208333674755394, -1.181850606188749264 ) ) ;
#104775 = CARTESIAN_POINT ( 'NONE',  ( 2.805909833680774845, 1.258924587927259253, -1.202001966437598268 ) ) ;
#104776 = CIRCLE ( 'NONE', #146379, 0.5000000000000007772 ) ;
#104777 = CARTESIAN_POINT ( 'NONE',  ( 4.497554271431305040, 6.270232621468402989, -1.599625672291256295 ) ) ;
#104779 = CARTESIAN_POINT ( 'NONE',  ( -0.004779991008855831794, 3.496248221084442775, -2.003420919873224904 ) ) ;
#104778 = CARTESIAN_POINT ( 'NONE',  ( -0.4000000000000305533, 3.099999999999943245, 0.3423093779009872550 ) ) ;
#104780 = CARTESIAN_POINT ( 'NONE',  ( 4.406709194360526993, 1.330975820509268104, -1.097133727364963729 ) ) ;
#104781 = CARTESIAN_POINT ( 'NONE',  ( 3.386445149735781257, -0.4294187885149694517, -2.148908265708626697 ) ) ;
#104782 = CARTESIAN_POINT ( 'NONE',  ( 0.1934855802202296304, 1.507424494634423517, 0.8570536861387479943 ) ) ;
#104783 = FACE_OUTER_BOUND ( 'NONE', #18363, .T. ) ;
#104784 = CARTESIAN_POINT ( 'NONE',  ( -10.28140399934106242, 4.005782094233665269, -7.421933058660648008 ) ) ;
#104785 = CARTESIAN_POINT ( 'NONE',  ( 4.170888513267295039, 1.539375584636338390, -1.531221199927160770 ) ) ;
#104786 = CARTESIAN_POINT ( 'NONE',  ( 2.015964598666186269, -0.8597642540715648707, -1.610575774528985704 ) ) ;
#104787 = CARTESIAN_POINT ( 'NONE',  ( 0.4089400952669055567, -1.579117232646386704, 1.163831224039679979 ) ) ;
#104788 = CARTESIAN_POINT ( 'NONE',  ( 4.188735998470741073, 1.634407174013367214, -1.345997343221926545 ) ) ;
#104789 = DIRECTION ( 'NONE',  ( 0.000000000000000000, -1.000000000000000000, 0.000000000000000000 ) ) ;
#104790 = ORIENTED_EDGE ( 'NONE', *, *, #93999, .T. ) ;
#104792 = CARTESIAN_POINT ( 'NONE',  ( -1.364683531250012516, 2.301041667008087988, -0.7879004041258289570 ) ) ;
#104791 = CARTESIAN_POINT ( 'NONE',  ( 4.862941710081361002, 0.2263591102839345448, -2.281146386033555462 ) ) ;
#104793 = DIRECTION ( 'NONE',  ( 0.7592566023653004592, -0.6507913734559639396, -0.000000000000000000 ) ) ;
#104794 = CARTESIAN_POINT ( 'NONE',  ( 9.134442807305049428, 11.67993591332117376, 1.599625672291281386 ) ) ;
#104795 = CARTESIAN_POINT ( 'NONE',  ( 0.1707708301344288138, 0.8156354886642532831, 1.957547177562010354 ) ) ;
#104796 = CARTESIAN_POINT ( 'NONE',  ( -5.910991785878170646, 7.919243054989755670, -1.443375672974059665 ) ) ;
#104797 = CARTESIAN_POINT ( 'NONE',  ( 2.236732156574683827, 5.553345249405011508, 1.040834085586084257E-14 ) ) ;
#104798 = CIRCLE ( 'NONE', #11537, 0.05000000000000008604 ) ;
#104799 = CARTESIAN_POINT ( 'NONE',  ( -4.731432421044865499, 8.463828891286912182, -0.7216878364870257245 ) ) ;
#104800 = STYLED_ITEM ( 'NONE', ( #207847 ), #111664 ) ;
#104801 = CARTESIAN_POINT ( 'NONE',  ( -10.99962150373186631, -9.999999999999880984, 0.09125116240080800856 ) ) ;
#104802 = ORIENTED_EDGE ( 'NONE', *, *, #132407, .F. ) ;
#104803 = CARTESIAN_POINT ( 'NONE',  ( 4.904922738988922504, -1.081064280317966420, -1.701948707654332704 ) ) ;
#104805 = CARTESIAN_POINT ( 'NONE',  ( 3.643474114467046387, 1.866637444603681528, -0.8776443792693452428 ) ) ;
#104804 = CARTESIAN_POINT ( 'NONE',  ( 6.322179702674084467, 6.270297829408224111, 1.040834085586084257E-14 ) ) ;
#104807 = CARTESIAN_POINT ( 'NONE',  ( -0.2411972340276386517, 4.090764154511560058, -2.455280512047691044 ) ) ;
#104806 = CARTESIAN_POINT ( 'NONE',  ( 7.452141709366786770, 8.723195411463290583, 1.199719254218452047 ) ) ;
#104808 = CARTESIAN_POINT ( 'NONE',  ( 6.851666526859736983, 9.086973262793417661, -1.599625672291269396 ) ) ;
#104809 = CARTESIAN_POINT ( 'NONE',  ( -3.285556943750000070, -1.159374999522042815, 0.000000000000000000 ) ) ;
#104810 =( NAMED_UNIT ( * ) SI_UNIT ( $, .STERADIAN. ) SOLID_ANGLE_UNIT ( ) );
#104811 = CARTESIAN_POINT ( 'NONE',  ( 6.263654578238285531, 1.123272483274835087, 1.881548979392036802 ) ) ;
#104812 = CARTESIAN_POINT ( 'NONE',  ( 4.078750125433938223, -0.7691220382576718917, 1.864168106189521890 ) ) ;
#104813 = CARTESIAN_POINT ( 'NONE',  ( 3.210337823311388394, 1.665856106666419034, 0.7845605768846477535 ) ) ;
#104814 = CARTESIAN_POINT ( 'NONE',  ( 6.844168616800228477, 6.879284895888727824, -0.7998128361456281477 ) ) ;
#104815 = CARTESIAN_POINT ( 'NONE',  ( 0.5863794435163689478, -0.2038549220112067795, -1.712615276990290480 ) ) ;
#104816 = VECTOR ( 'NONE', #120308, 1000.000000000000000 ) ;
#104817 = CARTESIAN_POINT ( 'NONE',  ( -4.274898507010545856, 3.881803101134051470, -0.7998128361456221525 ) ) ;
#104818 = CARTESIAN_POINT ( 'NONE',  ( 0.9854702925387841539, -2.298851036028260353, 0.006955682198207107335 ) ) ;
#104819 = CARTESIAN_POINT ( 'NONE',  ( -5.215082642750900277, 9.236013516518044142, 0.000000000000000000 ) ) ;
#104820 = CARTESIAN_POINT ( 'NONE',  ( 6.368092757517858082, 1.156555634672886246, 1.944455297613384204 ) ) ;
#104821 = CARTESIAN_POINT ( 'NONE',  ( 3.211649026191341072, -0.4105298382788050704, 2.065488094592916823 ) ) ;
#104822 = CARTESIAN_POINT ( 'NONE',  ( -4.502189528189771472, 7.410248995266807803, -1.199719254218453823 ) ) ;
#104823 = CARTESIAN_POINT ( 'NONE',  ( 7.344766530301147789, 9.591980256816594164, 1.599625672291281386 ) ) ;
#104824 = CARTESIAN_POINT ( 'NONE',  ( 5.031484404002867450, 8.884165881396448583, 0.7216878364870317197 ) ) ;
#104825 = CARTESIAN_POINT ( 'NONE',  ( -6.039267359883488950, 9.133230122250985517, 1.199719254218452047 ) ) ;
#104826 = CARTESIAN_POINT ( 'NONE',  ( 5.436456408955479880, 9.286356877182658565, -0.7216878364870267237 ) ) ;
#104827 = CARTESIAN_POINT ( 'NONE',  ( 4.650497622768338779, 7.104022005431295916, 1.360104839701151480 ) ) ;
#104828 = AXIS2_PLACEMENT_3D ( 'NONE', #143397, #109860, #14399 ) ;
#104829 = CARTESIAN_POINT ( 'NONE',  ( -4.238895582566952314, 8.097128612970093897, 1.040834085586084257E-14 ) ) ;
#104830 = CARTESIAN_POINT ( 'NONE',  ( 4.394933515450586192, -2.155188642370196916, -0.5379869938199193236 ) ) ;
#104831 = CARTESIAN_POINT ( 'NONE',  ( 2.836070844659248191, 2.175002134116140518, 0.2674123886829762875 ) ) ;
#104832 = CARTESIAN_POINT ( 'NONE',  ( -6.388916700537716764, 8.476822122092563916, 1.599625672291283607 ) ) ;
#104833 = CARTESIAN_POINT ( 'NONE',  ( -3.959863383643135393, 6.777535159962392086, 1.199719254218452935 ) ) ;
#104834 = CARTESIAN_POINT ( 'NONE',  ( 5.810985101215744741, -1.547553103248515027, 1.205733875218002238 ) ) ;
#104835 = CARTESIAN_POINT ( 'NONE',  ( 1.364683531249988757, 1.634375000341421691, 0.000000000000000000 ) ) ;
#104836 = CARTESIAN_POINT ( 'NONE',  ( -4.719646871332968452, 5.639247783710797712, 1.082531754730549078 ) ) ;
#104837 = CARTESIAN_POINT ( 'NONE',  ( -6.073689629242160493, 8.109057205581079231, -1.443375672974059665 ) ) ;
#104838 = CARTESIAN_POINT ( 'NONE',  ( 4.236665939827915395, 1.302216991916404387, -1.673619383358643908 ) ) ;
#104839 = CARTESIAN_POINT ( 'NONE',  ( -3.688700311369816909, 6.461178242310183784, -1.199719254218450271 ) ) ;
#104840 = VERTEX_POINT ( 'NONE', #116897 ) ;
#104841 = CARTESIAN_POINT ( 'NONE',  ( 5.998930166150279852, 1.769978137569449883, -1.240765152474863520 ) ) ;
#104842 = CARTESIAN_POINT ( 'NONE',  ( 5.819474248763732760, 7.812472595022922128, -1.599625672291262513 ) ) ;
#104843 = CARTESIAN_POINT ( 'NONE',  ( 4.897927690869709139, -0.6253142351902387652, -1.731941863025769246 ) ) ;
#104844 = CARTESIAN_POINT ( 'NONE',  ( -5.852179643265606579, 6.035944939585320412, -0.4116468081218557784 ) ) ;
#104845 = CARTESIAN_POINT ( 'NONE',  ( 1.364683531249988757, 0.9468750003414211358, 0.000000000000000000 ) ) ;
#104846 = CARTESIAN_POINT ( 'NONE',  ( 0.2216635874392547945, 1.664573546290064598, 0.5083179512348577900 ) ) ;
#104847 = CARTESIAN_POINT ( 'NONE',  ( 6.827182134110238110, 6.038038905730811479, 2.505852844092556264 ) ) ;
#104848 = CARTESIAN_POINT ( 'NONE',  ( -0.5512317429218814846, 7.510131493957778126, 1.922545642343826078 ) ) ;
#104849 = CARTESIAN_POINT ( 'NONE',  ( 5.851953751776640900, 5.929626919935292229, -0.4658998429906337502 ) ) ;
#104850 = ADVANCED_FACE ( 'NONE', ( #53976 ), #183963, .T. ) ;
#104851 = CARTESIAN_POINT ( 'NONE',  ( 3.995124980148881288, 1.827535992889782523, -1.154293374375232828 ) ) ;
#104852 = CARTESIAN_POINT ( 'NONE',  ( -4.111146893441842920, 5.819424013814012753, 1.599625672291267398 ) ) ;
#104853 = CARTESIAN_POINT ( 'NONE',  ( -6.358410854684783509, 9.401601182898824405, -1.082531754730537976 ) ) ;
#104854 = CARTESIAN_POINT ( 'NONE',  ( 3.450221060135277629, 2.161883445724331665, 0.001893877739161941697 ) ) ;
#104855 =( BOUNDED_SURFACE ( )  B_SPLINE_SURFACE ( 1, 2, ( 
 ( #211733, #182430, #31943, #113260, #48213, #33001, #148883, #12469, #114325, #79614, #66524, #78544, #99079, #16722, #145733, #132667, #14596, #146784, #212799, #30888, #165131, #116436, #98027, #64437, #15662, #130581, #456, #95899, #178198, #81749, #147831, #213849, #198673, #161952, #29815, #63371, #195507, #47144, #65468, #179265, #50318, #96966, #163014, #49262, #34057, #131619, #82807, #197618, #160875, #115383, #181377, #144662, #210676, #62304, #128463, #194431, #46072, #39141, #189645, #56457, #54327, #107404, #83869, #157170, #7682, #106322, #1529, #105223, #122618, #171263, #6611, #120466, #188580, #173427, #172345, #104146, #166191, #74844, #22856, #23935, #149960, #121540, #170194, #70534, #41296, #124742, #203740, #187510, #140944, #137721, #88971, #136653, #57525, #155026, #40212, #17781, #72691, #73766, #91110, #90039, #138786, #5528, #25008, #206958, #156097, #204805, #87888, #139861, #205892, #58587, #202677, #123684, #186438, #8763, #38075, #21779, #153962, #190701, #100130, #55385, #71608, #26074, #13015, #28220, #93247, #193909, #27142, #159281, #143080, #10880, #158237, #43424, #44490, #130067, #76955, #63911, #61788, #209074, #144153, #129003, #30362, #108474, #78030, #175552, #162499, #174497, #194980, #112738, #60710, #14070, #110608, #176608, #94312, #126874, #46616, #212276, #210145, #92186, #192832, #109548, #9827, #178748, #42363, #160353, #11956, #80158, #127954, #45556, #75903, #211216, #111672, #177678, #142007, #29289, #161433, #96448, #95382, #79092, #145210, #146264, #208022, #62842, #59648, #125807, #191769, #214373, #19408, #113805, #165677, #147311, #118059, #81229, #47692, #163558, #149427, #150511, #148373, #114855, #179806, #166747, #181905, #32477, #133209, #180855, #98550, #82279, #164613, #97502, #197102, #198159, #69210, #16198, #3141, #1009, #66004, #83341, #68143, #184044, #31425, #17266, #132153, #101741, #15143, #134277, #51935, #49792, #167809, #115918, #33539, #99611, #67073, #200284, #151573, #199213, #50860, #116984, #182984, #35661, #131114, #213337, #48742, #34601, #64962, #100669, #18342, #85487, #84422, #2072, #196060, #8497, #54064, #139601, #120198, #41029, #136392, #203476, #121274, #70276, #22600, #154765, #71344, #156909, #137461, #7417, #88707, #86558, #205624, #119120, #189387, #39954, #138522, #36726, #55129, #6349, #187249, #38877, #152621, #72420, #57263, #204545, #202408, #201344, #107139, #104961, #56193, #123425, #20471, #122356, #173165, #24744, #103883, #135330, #73499, #171002, #90845, #188312, #106061, #168868, #172083, #52984, #185100, #102812, #4208, #186174, #37808, #23676, #89787, #155833, #169932, #21515, #153698, #87627, #5267, #210948, #61518, #62574, #96178, #60447, #208817, #58326, #178477, #30088, #44222, #190440, #194710, #127683, #176348, #29027, #10620, #126605, #124482, #46350, #9569, #177410, #42100, #92982, #162229 ),
 ( #27955, #192568, #59387, #76695, #159027, #112467, #206698, #110345, #25810, #128736, #174238, #140683, #108214, #94048, #95109, #26879, #207760, #91920, #45286, #160088, #125543, #11691, #191505, #43170, #175292, #109283, #157981, #75646, #142811, #74580, #77764, #141753, #143886, #209879, #193644, #161159, #111406, #12746, #78819, #144941, #134017, #79888, #166477, #84157, #147054, #200024, #82020, #148111, #214115, #98290, #18069, #183789, #181644, #65742, #33271, #131889, #1812, #163289, #179542, #80963, #213075, #31163, #197897, #114601, #51676, #164351, #97236, #49526, #67870, #14871, #64705, #130848, #196845, #48483, #115649, #180592, #117797, #15936, #32216, #116715, #101475, #99356, #150244, #165406, #35397, #17003, #83078, #149157, #735, #66801, #132942, #198947, #13816, #50590, #100408, #182715, #34333, #145998, #212009, #63651, #129806, #195785, #47423, #113538, #186988, #103624, #71083, #118856, #38619, #23411, #170747, #168607, #19145, #139336, #169676, #88447, #151309, #185909, #20209, #135069, #39683, #189133, #53803, #37544, #205367, #202143, #87369, #2877, #122090, #153439, #104696, #85220, #21263, #72157, #155575, #154507, #5010, #70012, #89523, #57001, #121021, #137201, #152366, #203224, #54868, #123173, #68947, #22333, #184841, #7158, #52723, #201082, #36470, #6087, #188052, #119933, #86297, #102543, #138265, #204279, #3945, #55935, #136128, #105793, #171818, #73229, #40772, #167546, #109023, #194466, #157720, #128497, #126356, #59130, #208560, #193401, #94857, #172903, #142554, #25557, #12505, #24476, #45044, #177156, #91668, #78577, #175041, #26627, #92728, #191248, #111157, #62338, #60195, #158774, #192314, #43973, #42913, #110091, #58067, #10369, #127431, #28775, #206440, #176101, #160910, #144699, #75392, #106875, #210710, #76447, #90589, #27701, #93797, #140425, #159837, #156649, #8242, #74326, #124231, #190190, #173985, #11437, #77513, #61269, #41847, #107957, #125289, #9316, #143634, #141504, #209628, #207511, #67623, #31980, #180354, #29849, #149990, #1562, #15697, #161987, #166226, #33033, #147865, #489, #196605, #98058, #95931, #17816, #195544, #148915, #13577, #64472, #133767, #46108, #14631, #82839, #112226, #130613, #48245, #99111, #81782, #66557, #79650, #178234, #212835, #83900, #165161, #16756, #114359, #115415, #182462, #132699, #164112, #198705, #80725, #50350, #116470, #34091, #113294, #145766, #211767, #179302, #63405, #30923, #129558, #47180, #96999, #163052, #146816, #100162, #213881, #65503, #197653, #181407, #131650, #49300, #2627, #68699, #35142, #168362, #169425, #167302, #171554, #52477, #70826, #3688, #38358, #39427, #118604, #21008, #55672, #19957, #86042, #186736, #151064, #104436, #134821, #200826, #170485, #202969, #184592, #36210, #121828, #101218, #105520, #102289, #88181, #18889, #69765, #155315, #199775, #152117, #22069, #89265, #135871, #201890, #154253 ) ),
 .UNSPECIFIED., .F., .F., .T. ) 
 B_SPLINE_SURFACE_WITH_KNOTS ( ( 2, 2 ),
 ( 3, 2, 2, 2, 2, 2, 2, 2, 2, 2, 2, 2, 2, 2, 2, 2, 2, 2, 2, 2, 2, 2, 2, 2, 2, 2, 2, 2, 2, 2, 2, 2, 2, 2, 2, 2, 2, 2, 2, 2, 2, 2, 2, 2, 2, 2, 2, 2, 2, 2, 2, 2, 2, 2, 2, 2, 2, 2, 2, 2, 2, 2, 2, 2, 2, 2, 2, 2, 2, 2, 2, 2, 2, 2, 2, 2, 2, 2, 2, 2, 2, 2, 2, 2, 2, 2, 2, 2, 2, 2, 2, 2, 2, 2, 2, 2, 2, 2, 2, 2, 2, 2, 2, 2, 2, 2, 2, 2, 2, 2, 2, 2, 2, 2, 2, 2, 2, 2, 2, 2, 2, 2, 2, 2, 2, 2, 2, 2, 2, 2, 2, 2, 2, 2, 2, 2, 2, 2, 2, 2, 2, 2, 2, 2, 2, 2, 2, 2, 2, 2, 2, 2, 2, 2, 2, 2, 2, 2, 2, 2, 2, 2, 2, 2, 2, 2, 2, 2, 3 ),
 ( 0.000000000000000000, 1.000000000000000000 ),
 ( 0.000000000000000000, 0.005952380952380952051, 0.01190476190476190410, 0.01785714285714285615, 0.02380952380952380820, 0.02976190476190476025, 0.03571428571428571230, 0.04166666666666666435, 0.04761904761904761640, 0.05357142857142856845, 0.05952380952380952051, 0.06547619047619047949, 0.07142857142857142461, 0.07738095238095238360, 0.08333333333333332871, 0.08928571428571428770, 0.09523809523809523281, 0.1011904761904761918, 0.1071428571428571369, 0.1130952380952380959, 0.1190476190476190410, 0.1250000000000000000, 0.1309523809523809590, 0.1369047619047619180, 0.1428571428571428492, 0.1488095238095238082, 0.1547619047619047672, 0.1607142857142857262, 0.1666666666666666574, 0.1726190476190476164, 0.1785714285714285754, 0.1845238095238095344, 0.1904761904761904656, 0.1964285714285714246, 0.2023809523809523836, 0.2083333333333333426, 0.2142857142857142738, 0.2202380952380952328, 0.2261904761904761918, 0.2321428571428571508, 0.2380952380952380820, 0.2440476190476190410, 0.2500000000000000000, 0.2559523809523809312, 0.2619047619047619180, 0.2678571428571428492, 0.2738095238095238360, 0.2797619047619047672, 0.2857142857142856984, 0.2916666666666666852, 0.2976190476190476164, 0.3035714285714285476, 0.3095238095238095344, 0.3154761904761904656, 0.3214285714285714524, 0.3273809523809523836, 0.3333333333333333148, 0.3392857142857143016, 0.3452380952380952328, 0.3511904761904761640, 0.3571428571428571508, 0.3630952380952380820, 0.3690476190476190688, 0.3750000000000000000, 0.3809523809523809312, 0.3869047619047619180, 0.3928571428571428492, 0.3988095238095238360, 0.4047619047619047672, 0.4107142857142856984, 0.4166666666666666852, 0.4226190476190476164, 0.4285714285714285476, 0.4345238095238095344, 0.4404761904761904656, 0.4464285714285714524, 0.4523809523809523836, 0.4583333333333333148, 0.4642857142857143016, 0.4702380952380952328, 0.4761904761904761640, 0.4821428571428571508, 0.4880952380952380820, 0.4940476190476190688, 0.5000000000000000000, 0.5059523809523809312, 0.5119047619047618625, 0.5178571428571429047, 0.5238095238095238360, 0.5297619047619047672, 0.5357142857142856984, 0.5416666666666666297, 0.5476190476190476719, 0.5535714285714286031, 0.5595238095238095344, 0.5654761904761904656, 0.5714285714285713969, 0.5773809523809523281, 0.5833333333333333703, 0.5892857142857143016, 0.5952380952380952328, 0.6011904761904761640, 0.6071428571428570953, 0.6130952380952381375, 0.6190476190476190688, 0.6250000000000000000, 0.6309523809523809312, 0.6369047619047618625, 0.6428571428571429047, 0.6488095238095238360, 0.6547619047619047672, 0.6607142857142856984, 0.6666666666666666297, 0.6726190476190476719, 0.6785714285714286031, 0.6845238095238095344, 0.6904761904761904656, 0.6964285714285713969, 0.7023809523809523281, 0.7083333333333333703, 0.7142857142857143016, 0.7202380952380952328, 0.7261904761904761640, 0.7321428571428570953, 0.7380952380952381375, 0.7440476190476190688, 0.7500000000000000000, 0.7559523809523809312, 0.7619047619047618625, 0.7678571428571429047, 0.7738095238095238360, 0.7797619047619047672, 0.7857142857142856984, 0.7916666666666666297, 0.7976190476190476719, 0.8035714285714286031, 0.8095238095238095344, 0.8154761904761904656, 0.8214285714285713969, 0.8273809523809523281, 0.8333333333333333703, 0.8392857142857143016, 0.8452380952380952328, 0.8511904761904761640, 0.8571428571428570953, 0.8630952380952381375, 0.8690476190476190688, 0.8750000000000000000, 0.8809523809523809312, 0.8869047619047618625, 0.8928571428571429047, 0.8988095238095238360, 0.9047619047619047672, 0.9107142857142856984, 0.9166666666666666297, 0.9226190476190476719, 0.9285714285714286031, 0.9345238095238095344, 0.9404761904761904656, 0.9464285714285713969, 0.9523809523809523281, 0.9583333333333333703, 0.9642857142857143016, 0.9702380952380952328, 0.9761904761904761640, 0.9821428571428570953, 0.9880952380952381375, 0.9940476190476190688, 1.000000000000000000 ),
 .UNSPECIFIED. ) 
 GEOMETRIC_REPRESENTATION_ITEM ( )  RATIONAL_B_SPLINE_SURFACE ( (
 ( 1.000000000000000000, 0.8660254037844387076, 1.000000000000000000, 0.8660254037844387076, 1.000000000000000000, 0.8660254037844387076, 1.000000000000000000, 0.8660254037844387076, 1.000000000000000000, 0.8660254037844387076, 1.000000000000000000, 0.8660254037844387076, 1.000000000000000000, 0.8660254037844387076, 1.000000000000000000, 0.8660254037844387076, 1.000000000000000000, 0.8660254037844387076, 1.000000000000000000, 0.8660254037844387076, 1.000000000000000000, 0.8660254037844387076, 1.000000000000000000, 0.8660254037844387076, 1.000000000000000000, 0.8660254037844387076, 1.000000000000000000, 0.8660254037844387076, 1.000000000000000000, 0.8660254037844387076, 1.000000000000000000, 0.8660254037844387076, 1.000000000000000000, 0.8660254037844387076, 1.000000000000000000, 0.8660254037844387076, 1.000000000000000000, 0.8660254037844387076, 1.000000000000000000, 0.8660254037844387076, 1.000000000000000000, 0.8660254037844387076, 1.000000000000000000, 0.8660254037844387076, 1.000000000000000000, 0.8660254037844387076, 1.000000000000000000, 0.8660254037844387076, 1.000000000000000000, 0.8660254037844387076, 1.000000000000000000, 0.8660254037844387076, 1.000000000000000000, 0.8660254037844387076, 1.000000000000000000, 0.8660254037844387076, 1.000000000000000000, 0.8660254037844387076, 1.000000000000000000, 0.8660254037844387076, 1.000000000000000000, 0.8660254037844387076, 1.000000000000000000, 0.8660254037844387076, 1.000000000000000000, 0.8660254037844387076, 1.000000000000000000, 0.8660254037844387076, 1.000000000000000000, 0.8660254037844387076, 1.000000000000000000, 0.8660254037844387076, 1.000000000000000000, 0.8660254037844387076, 1.000000000000000000, 0.8660254037844387076, 1.000000000000000000, 0.8660254037844387076, 1.000000000000000000, 0.8660254037844387076, 1.000000000000000000, 0.8660254037844387076, 1.000000000000000000, 0.8660254037844387076, 1.000000000000000000, 0.8660254037844387076, 1.000000000000000000, 0.8660254037844387076, 1.000000000000000000, 0.8660254037844387076, 1.000000000000000000, 0.8660254037844387076, 1.000000000000000000, 0.8660254037844387076, 1.000000000000000000, 0.8660254037844387076, 1.000000000000000000, 0.8660254037844387076, 1.000000000000000000, 0.8660254037844387076, 1.000000000000000000, 0.8660254037844387076, 1.000000000000000000, 0.8660254037844387076, 1.000000000000000000, 0.8660254037844387076, 1.000000000000000000, 0.8660254037844387076, 1.000000000000000000, 0.8660254037844387076, 1.000000000000000000, 0.8660254037844387076, 1.000000000000000000, 0.8660254037844387076, 1.000000000000000000, 0.8660254037844387076, 1.000000000000000000, 0.8660254037844387076, 1.000000000000000000, 0.8660254037844387076, 1.000000000000000000, 0.8660254037844387076, 1.000000000000000000, 0.8660254037844387076, 1.000000000000000000, 0.8660254037844387076, 1.000000000000000000, 0.8660254037844387076, 1.000000000000000000, 0.8660254037844387076, 1.000000000000000000, 0.8660254037844387076, 1.000000000000000000, 0.8660254037844387076, 1.000000000000000000, 0.8660254037844387076, 1.000000000000000000, 0.8660254037844387076, 1.000000000000000000, 0.8660254037844387076, 1.000000000000000000, 0.8660254037844387076, 1.000000000000000000, 0.8660254037844387076, 1.000000000000000000, 0.8660254037844387076, 1.000000000000000000, 0.8660254037844387076, 1.000000000000000000, 0.8660254037844387076, 1.000000000000000000, 0.8660254037844387076, 1.000000000000000000, 0.8660254037844387076, 1.000000000000000000, 0.8660254037844387076, 1.000000000000000000, 0.8660254037844387076, 1.000000000000000000, 0.8660254037844387076, 1.000000000000000000, 0.8660254037844387076, 1.000000000000000000, 0.8660254037844387076, 1.000000000000000000, 0.8660254037844387076, 1.000000000000000000, 0.8660254037844387076, 1.000000000000000000, 0.8660254037844387076, 1.000000000000000000, 0.8660254037844387076, 1.000000000000000000, 0.8660254037844387076, 1.000000000000000000, 0.8660254037844387076, 1.000000000000000000, 0.8660254037844387076, 1.000000000000000000, 0.8660254037844387076, 1.000000000000000000, 0.8660254037844387076, 1.000000000000000000, 0.8660254037844387076, 1.000000000000000000, 0.8660254037844387076, 1.000000000000000000, 0.8660254037844387076, 1.000000000000000000, 0.8660254037844387076, 1.000000000000000000, 0.8660254037844387076, 1.000000000000000000, 0.8660254037844387076, 1.000000000000000000, 0.8660254037844387076, 1.000000000000000000, 0.8660254037844387076, 1.000000000000000000, 0.8660254037844387076, 1.000000000000000000, 0.8660254037844387076, 1.000000000000000000, 0.8660254037844387076, 1.000000000000000000, 0.8660254037844387076, 1.000000000000000000, 0.8660254037844387076, 1.000000000000000000, 0.8660254037844387076, 1.000000000000000000, 0.8660254037844387076, 1.000000000000000000, 0.8660254037844387076, 1.000000000000000000, 0.8660254037844387076, 1.000000000000000000, 0.8660254037844387076, 1.000000000000000000, 0.8660254037844387076, 1.000000000000000000, 0.8660254037844387076, 1.000000000000000000, 0.8660254037844387076, 1.000000000000000000, 0.8660254037844387076, 1.000000000000000000, 0.8660254037844387076, 1.000000000000000000, 0.8660254037844387076, 1.000000000000000000, 0.8660254037844387076, 1.000000000000000000, 0.8660254037844387076, 1.000000000000000000, 0.8660254037844387076, 1.000000000000000000, 0.8660254037844387076, 1.000000000000000000, 0.8660254037844387076, 1.000000000000000000, 0.8660254037844387076, 1.000000000000000000, 0.8660254037844387076, 1.000000000000000000, 0.8660254037844387076, 1.000000000000000000, 0.8660254037844387076, 1.000000000000000000, 0.8660254037844387076, 1.000000000000000000, 0.8660254037844387076, 1.000000000000000000, 0.8660254037844387076, 1.000000000000000000, 0.8660254037844387076, 1.000000000000000000, 0.8660254037844387076, 1.000000000000000000, 0.8660254037844387076, 1.000000000000000000, 0.8660254037844387076, 1.000000000000000000, 0.8660254037844387076, 1.000000000000000000, 0.8660254037844387076, 1.000000000000000000, 0.8660254037844387076, 1.000000000000000000, 0.8660254037844387076, 1.000000000000000000, 0.8660254037844387076, 1.000000000000000000, 0.8660254037844387076, 1.000000000000000000, 0.8660254037844387076, 1.000000000000000000, 0.8660254037844387076, 1.000000000000000000, 0.8660254037844387076, 1.000000000000000000, 0.8660254037844387076, 1.000000000000000000, 0.8660254037844387076, 1.000000000000000000, 0.8660254037844387076, 1.000000000000000000, 0.8660254037844387076, 1.000000000000000000, 0.8660254037844387076, 1.000000000000000000, 0.8660254037844387076, 1.000000000000000000, 0.8660254037844387076, 1.000000000000000000, 0.8660254037844387076, 1.000000000000000000, 0.8660254037844387076, 1.000000000000000000, 0.8660254037844387076, 1.000000000000000000, 0.8660254037844387076, 1.000000000000000000, 0.8660254037844387076, 1.000000000000000000, 0.8660254037844387076, 1.000000000000000000, 0.8660254037844387076, 1.000000000000000000, 0.8660254037844387076, 1.000000000000000000, 0.8660254037844387076, 1.000000000000000000, 0.8660254037844387076, 1.000000000000000000, 0.8660254037844387076, 1.000000000000000000, 0.8660254037844387076, 1.000000000000000000, 0.8660254037844387076, 1.000000000000000000, 0.8660254037844387076, 1.000000000000000000, 0.8660254037844387076, 1.000000000000000000, 0.8660254037844387076, 1.000000000000000000, 0.8660254037844387076, 1.000000000000000000, 0.8660254037844387076, 1.000000000000000000, 0.8660254037844387076, 1.000000000000000000, 0.8660254037844387076, 1.000000000000000000, 0.8660254037844387076, 1.000000000000000000),
 ( 1.000000000000000000, 0.8660254037844387076, 1.000000000000000000, 0.8660254037844387076, 1.000000000000000000, 0.8660254037844387076, 1.000000000000000000, 0.8660254037844387076, 1.000000000000000000, 0.8660254037844387076, 1.000000000000000000, 0.8660254037844387076, 1.000000000000000000, 0.8660254037844387076, 1.000000000000000000, 0.8660254037844387076, 1.000000000000000000, 0.8660254037844387076, 1.000000000000000000, 0.8660254037844387076, 1.000000000000000000, 0.8660254037844387076, 1.000000000000000000, 0.8660254037844387076, 1.000000000000000000, 0.8660254037844387076, 1.000000000000000000, 0.8660254037844387076, 1.000000000000000000, 0.8660254037844387076, 1.000000000000000000, 0.8660254037844387076, 1.000000000000000000, 0.8660254037844387076, 1.000000000000000000, 0.8660254037844387076, 1.000000000000000000, 0.8660254037844387076, 1.000000000000000000, 0.8660254037844387076, 1.000000000000000000, 0.8660254037844387076, 1.000000000000000000, 0.8660254037844387076, 1.000000000000000000, 0.8660254037844387076, 1.000000000000000000, 0.8660254037844387076, 1.000000000000000000, 0.8660254037844387076, 1.000000000000000000, 0.8660254037844387076, 1.000000000000000000, 0.8660254037844387076, 1.000000000000000000, 0.8660254037844387076, 1.000000000000000000, 0.8660254037844387076, 1.000000000000000000, 0.8660254037844387076, 1.000000000000000000, 0.8660254037844387076, 1.000000000000000000, 0.8660254037844387076, 1.000000000000000000, 0.8660254037844387076, 1.000000000000000000, 0.8660254037844387076, 1.000000000000000000, 0.8660254037844387076, 1.000000000000000000, 0.8660254037844387076, 1.000000000000000000, 0.8660254037844387076, 1.000000000000000000, 0.8660254037844387076, 1.000000000000000000, 0.8660254037844387076, 1.000000000000000000, 0.8660254037844387076, 1.000000000000000000, 0.8660254037844387076, 1.000000000000000000, 0.8660254037844387076, 1.000000000000000000, 0.8660254037844387076, 1.000000000000000000, 0.8660254037844387076, 1.000000000000000000, 0.8660254037844387076, 1.000000000000000000, 0.8660254037844387076, 1.000000000000000000, 0.8660254037844387076, 1.000000000000000000, 0.8660254037844387076, 1.000000000000000000, 0.8660254037844387076, 1.000000000000000000, 0.8660254037844387076, 1.000000000000000000, 0.8660254037844387076, 1.000000000000000000, 0.8660254037844387076, 1.000000000000000000, 0.8660254037844387076, 1.000000000000000000, 0.8660254037844387076, 1.000000000000000000, 0.8660254037844387076, 1.000000000000000000, 0.8660254037844387076, 1.000000000000000000, 0.8660254037844387076, 1.000000000000000000, 0.8660254037844387076, 1.000000000000000000, 0.8660254037844387076, 1.000000000000000000, 0.8660254037844387076, 1.000000000000000000, 0.8660254037844387076, 1.000000000000000000, 0.8660254037844387076, 1.000000000000000000, 0.8660254037844387076, 1.000000000000000000, 0.8660254037844387076, 1.000000000000000000, 0.8660254037844387076, 1.000000000000000000, 0.8660254037844387076, 1.000000000000000000, 0.8660254037844387076, 1.000000000000000000, 0.8660254037844387076, 1.000000000000000000, 0.8660254037844387076, 1.000000000000000000, 0.8660254037844387076, 1.000000000000000000, 0.8660254037844387076, 1.000000000000000000, 0.8660254037844387076, 1.000000000000000000, 0.8660254037844387076, 1.000000000000000000, 0.8660254037844387076, 1.000000000000000000, 0.8660254037844387076, 1.000000000000000000, 0.8660254037844387076, 1.000000000000000000, 0.8660254037844387076, 1.000000000000000000, 0.8660254037844387076, 1.000000000000000000, 0.8660254037844387076, 1.000000000000000000, 0.8660254037844387076, 1.000000000000000000, 0.8660254037844387076, 1.000000000000000000, 0.8660254037844387076, 1.000000000000000000, 0.8660254037844387076, 1.000000000000000000, 0.8660254037844387076, 1.000000000000000000, 0.8660254037844387076, 1.000000000000000000, 0.8660254037844387076, 1.000000000000000000, 0.8660254037844387076, 1.000000000000000000, 0.8660254037844387076, 1.000000000000000000, 0.8660254037844387076, 1.000000000000000000, 0.8660254037844387076, 1.000000000000000000, 0.8660254037844387076, 1.000000000000000000, 0.8660254037844387076, 1.000000000000000000, 0.8660254037844387076, 1.000000000000000000, 0.8660254037844387076, 1.000000000000000000, 0.8660254037844387076, 1.000000000000000000, 0.8660254037844387076, 1.000000000000000000, 0.8660254037844387076, 1.000000000000000000, 0.8660254037844387076, 1.000000000000000000, 0.8660254037844387076, 1.000000000000000000, 0.8660254037844387076, 1.000000000000000000, 0.8660254037844387076, 1.000000000000000000, 0.8660254037844387076, 1.000000000000000000, 0.8660254037844387076, 1.000000000000000000, 0.8660254037844387076, 1.000000000000000000, 0.8660254037844387076, 1.000000000000000000, 0.8660254037844387076, 1.000000000000000000, 0.8660254037844387076, 1.000000000000000000, 0.8660254037844387076, 1.000000000000000000, 0.8660254037844387076, 1.000000000000000000, 0.8660254037844387076, 1.000000000000000000, 0.8660254037844387076, 1.000000000000000000, 0.8660254037844387076, 1.000000000000000000, 0.8660254037844387076, 1.000000000000000000, 0.8660254037844387076, 1.000000000000000000, 0.8660254037844387076, 1.000000000000000000, 0.8660254037844387076, 1.000000000000000000, 0.8660254037844387076, 1.000000000000000000, 0.8660254037844387076, 1.000000000000000000, 0.8660254037844387076, 1.000000000000000000, 0.8660254037844387076, 1.000000000000000000, 0.8660254037844387076, 1.000000000000000000, 0.8660254037844387076, 1.000000000000000000, 0.8660254037844387076, 1.000000000000000000, 0.8660254037844387076, 1.000000000000000000, 0.8660254037844387076, 1.000000000000000000, 0.8660254037844387076, 1.000000000000000000, 0.8660254037844387076, 1.000000000000000000, 0.8660254037844387076, 1.000000000000000000, 0.8660254037844387076, 1.000000000000000000, 0.8660254037844387076, 1.000000000000000000, 0.8660254037844387076, 1.000000000000000000, 0.8660254037844387076, 1.000000000000000000, 0.8660254037844387076, 1.000000000000000000, 0.8660254037844387076, 1.000000000000000000, 0.8660254037844387076, 1.000000000000000000, 0.8660254037844387076, 1.000000000000000000, 0.8660254037844387076, 1.000000000000000000, 0.8660254037844387076, 1.000000000000000000, 0.8660254037844387076, 1.000000000000000000, 0.8660254037844387076, 1.000000000000000000, 0.8660254037844387076, 1.000000000000000000, 0.8660254037844387076, 1.000000000000000000, 0.8660254037844387076, 1.000000000000000000, 0.8660254037844387076, 1.000000000000000000, 0.8660254037844387076, 1.000000000000000000, 0.8660254037844387076, 1.000000000000000000, 0.8660254037844387076, 1.000000000000000000, 0.8660254037844387076, 1.000000000000000000, 0.8660254037844387076, 1.000000000000000000, 0.8660254037844387076, 1.000000000000000000, 0.8660254037844387076, 1.000000000000000000, 0.8660254037844387076, 1.000000000000000000, 0.8660254037844387076, 1.000000000000000000, 0.8660254037844387076, 1.000000000000000000, 0.8660254037844387076, 1.000000000000000000, 0.8660254037844387076, 1.000000000000000000, 0.8660254037844387076, 1.000000000000000000, 0.8660254037844387076, 1.000000000000000000, 0.8660254037844387076, 1.000000000000000000, 0.8660254037844387076, 1.000000000000000000, 0.8660254037844387076, 1.000000000000000000, 0.8660254037844387076, 1.000000000000000000, 0.8660254037844387076, 1.000000000000000000, 0.8660254037844387076, 1.000000000000000000, 0.8660254037844387076, 1.000000000000000000, 0.8660254037844387076, 1.000000000000000000, 0.8660254037844387076, 1.000000000000000000, 0.8660254037844387076, 1.000000000000000000) ) ) 
 REPRESENTATION_ITEM ( '' )  SURFACE ( )  );
#104856 = CARTESIAN_POINT ( 'NONE',  ( 4.569576162043214929, 1.912950159424832375, -0.4759120794774750474 ) ) ;
#104857 = CARTESIAN_POINT ( 'NONE',  ( 3.584998556975723005, 1.101681934899124915, -1.338793912720330770 ) ) ;
#104858 = CARTESIAN_POINT ( 'NONE',  ( 0.6619992422990974568, 1.085049530943157148, 1.904046507712559455 ) ) ;
#104859 = CARTESIAN_POINT ( 'NONE',  ( 0.7457024085506950284, -1.977219658456253359, 1.189539768987533330 ) ) ;
#104860 = CARTESIAN_POINT ( 'NONE',  ( 4.112614458092584968, 1.460029904434188008, -1.454618372460781295 ) ) ;
#104861 = CARTESIAN_POINT ( 'NONE',  ( 5.267111086673036624, 1.870628123453799363, -0.5216035295831971119 ) ) ;
#104862 = CARTESIAN_POINT ( 'NONE',  ( -8.310784975052689205, 8.798263347090697906, -0.7216878364870267237 ) ) ;
#104863 = CARTESIAN_POINT ( 'NONE',  ( -4.471156797456668386, 8.438376373666578445, -0.7998128361456362523 ) ) ;
#104864 = CYLINDRICAL_SURFACE ( 'NONE', #74973, 1.250000000000000000 ) ;
#104865 = CARTESIAN_POINT ( 'NONE',  ( -3.156015896931072540, 6.904045323053366268, 0.000000000000000000 ) ) ;
#104866 = CARTESIAN_POINT ( 'NONE',  ( -7.578644679914719795, 9.864838098032418401, 1.443375672974090751 ) ) ;
#104867 = CARTESIAN_POINT ( 'NONE',  ( 3.751171811254182753, -1.805526059370649028, 1.268566889074909554 ) ) ;
#104868 = CARTESIAN_POINT ( 'NONE',  ( 1.642778471875000035, -3.813541666188708490, -2.845375778867859751 ) ) ;
#104869 = VERTEX_POINT ( 'NONE', #18250 ) ;
#104870 = CARTESIAN_POINT ( 'NONE',  ( 1.059155247252058896, 1.517088508067988117, 1.077460967357747990 ) ) ;
#104871 =( BOUNDED_SURFACE ( )  B_SPLINE_SURFACE ( 3, 3, ( 
 ( #51819, #99493, #100550, #133089, #4090, #3024, #168753, #68016, #149302, #151452, #53944, #19288, #165550, #85370, #82156, #33414, #17143, #86441, #50733, #119005, #201229, #120081, #166623, #883, #184983, #116859, #152506, #136272, #37692, #70161, #83220, #214250, #198039, #18215, #66949, #134157, #35543, #183931, #101620, #84299, #150384, #1955, #117937, #191389, #169820, #206580, #55013, #170886, #104841, #190326, #71228, #122237, #89662, #23555, #188196, #140568, #41985, #88590, #58209, #22479, #103769, #107017, #105940, #171964, #40911, #38760, #21407, #155714, #139480, #87517, #157862, #74463, #138406, #108094, #153582, #124368, #25696, #39832, #187131, #7297, #73375, #75527, #173041, #205510, #72300, #57141, #5151, #123308, #91804, #59267, #189272, #174123, #9455, #141638, #8380, #207647, #137343, #154647, #125423, #203361, #121162, #6229, #204425, #24624, #56080, #90731, #156794, #46245, #163188, #159980, #43055, #113432, #45184, #145897, #11582, #126494, #78713, #77654, #111298, #210847, #13711, #158915, #194601, #96069, #12643, #143776, #44111, #209771, #142696, #130748, #146953, #192457, #76585, #79784, #162122, #61411, #109168, #175181, #62473, #128635, #47319, #177302, #127574, #28916, #10511, #26767, #112362, #14772, #92869, #212968, #193542, #31059, #80863, #110232, #211907, #161047, #129700, #208706, #95001, #63544, #64608, #178375, #195682, #29984, #27842, #60333, #93939, #144841, #179439, #176240, #97135, #50489, #81917, #199916, #51563, #200967, #100300, #151197, #84044, #115546, #166366, #3827, #33169, #69900, #98195, #198842, #17957, #196742, #16894, #134959, #164243, #214015, #15831, #34227, #181541, #2768, #150132, #52614, #68839, #114495, #19031, #48382, #180492, #102429, #148004, #117688, #82975, #1705, #116610, #66691, #85111, #67759, #20097, #183680, #182603, #118743, #133910, #184727, #36351, #624, #35285, #101361, #168498, #32110, #167439, #65637, #86185, #152254, #131785, #197789, #49426, #99251, #165299, #149048, #132838, #21147, #171695, #70969, #72038, #104582, #190079, #189014, #8127, #39566, #120899, #123060, #25442, #139213, #137079, #205244, #136011, #87251, #153316, #140308, #170627, #24359, #40657, #91548, #138151, #186872, #106758, #22213, #156536, #107840, #157606, #172786, #4891, #202024, #169565, #88326, #206326, #105668, #7036, #155453, #73113, #53684, #56885, #90469, #204160, #9202, #119815, #74213, #203104, #54749, #38504, #57951, #103505, #154390, #121970, #55815, #5968, #124116, #41731, #187936, #173867, #23294, #89404, #185795, #37428, #143517, #159724, #76336, #27584, #195431, #142443, #126240, #92621, #160795, #113178, #29733, #45995, #109980, #127316, #209513, #179182, #158663, #208450, #193286, #61154, #75274, #44931, #11322, #60083, #93682, #47061, #192202, #43864, #112115, #94748, #178118, #125174, #111039, #177046, #59018, #129449, #95815, #175990, #161873, #191135, #13461, #211651, #77401, #10261, #28662, #12387, #30805, #78466, #144585, #210599, #62228, #207399, #128386, #63288, #96885, #194353, #79537, #145655, #162934, #141389, #42801, #108909, #174932, #26512, #203648, #170101, #202582, #130503, #370, #153871, #81662, #98993, #17698, #137631, #131534, #14515, #87797, #16640, #120372, #197536, #97943, #50234, #49181, #82724, #182345, #54234, #196490, #166113 ),
 ( #70445, #115299, #80608, #146702, #33974, #100049, #21687, #148801, #181289, #66444, #48132, #212717, #83785, #55299, #64357, #187418, #32916, #5440, #121449, #163999, #136561, #132585, #104055, #114245, #165048, #186347, #39049, #149879, #71519, #1445, #213766, #180242, #65387, #198588, #116355, #105134, #37982, #31866, #15574, #147748, #174402, #175459, #74748, #125710, #58495, #89951, #7588, #189554, #107308, #204713, #23843, #141917, #205798, #8667, #91016, #208984, #188489, #57428, #109453, #72595, #40119, #56363, #140851, #156001, #191669, #206863, #27043, #43334, #88881, #207929, #192738, #22764, #76865, #138696, #25980, #123590, #124651, #24910, #41201, #59551, #190608, #60620, #158143, #157078, #93152, #173332, #159189, #10790, #42266, #108379, #92087, #142984, #154934, #9734, #171174, #75809, #126781, #44393, #122526, #106230, #6519, #172256, #73673, #139772, #210055, #146172, #45461, #46525, #79001, #164528, #163471, #197020, #13986, #95289, #97416, #214289, #113718, #111578, #179722, #110514, #61694, #127863, #114773, #145117, #213255, #15051, #65923, #112647, #161338, #81144, #211123, #131030, #82197, #132070, #147229, #193813, #176514, #144060, #62747, #180770, #80069, #195970, #129982, #47604, #28126, #31339, #64884, #178656, #198081, #94220, #48656, #177586, #29200, #12921, #32398, #77939, #128907, #96353, #30267, #194888, #98464, #16114, #162408, #148291, #212187, #63824, #160260, #11861, #117975, #134193, #50774, #1992, #169855, #116902, #166665, #182901, #18255, #149345, #137380, #153619, #133130, #83259, #20394, #102733, #150427, #49708, #181823, #3060, #69130, #53981, #51855, #68056, #183968, #17184, #33455, #52906, #21443, #99532, #5191, #200202, #37727, #87551, #199129, #168789, #167727, #136309, #165592, #84339, #86478, #71266, #201265, #202330, #135252, #34517, #924, #100590, #35579, #101659, #115837, #152542, #19328, #66992, #119039, #185022, #120117, #85406, #4128, #151491, #36648, #70196, #186097, #103806, #59306, #38797, #155753, #123344, #203396, #55049, #90768, #7338, #58246, #173080, #124403, #104878, #205544, #189309, #170921, #9493, #190361, #172004, #108132, #22517, #42023, #157899, #89703, #72339, #73415, #139518, #141674, #156829, #40948, #105981, #57182, #88628, #24661, #91841, #121199, #8416, #25731, #174159, #187168, #75565, #207686, #204463, #23594, #154684, #6268, #138445, #56117, #107054, #206618, #122274, #74502, #140606, #188232, #39872, #18496, #84574, #2224, #68299, #82433, #198306, #185258, #49946, #48890, #169023, #148523, #150662, #116067, #199370, #17415, #167960, #89, #115010, #66154, #149581, #53143, #166903, #134433, #200435, #52082, #181007, #118209, #19566, #51016, #136545, #32627, #151726, #132299, #182057, #33687, #135475, #16353, #67229, #34745, #183140, #133363, #85640, #201497, #99764, #3298, #165831, #184196, #117137, #98704, #100818, #35819, #83499, #1165, #20621, #101895, #69366, #119273, #36882, #102965, #86709, #152778, #4360, #70429, #164763, #25965, #5425, #22747, #140835, #104039, #71504, #21672, #40103, #187401, #157063, #23829, #206848, #74730, #120355, #24894, #9719, #54217, #108363, #170085, #205782, #88865, #106215, #56349, #72579, #91000, #89934, #92070, #189538, #122511, #124636, #204699, #8651, #190593, #6504, #172241, #57411, #87780 ),
 ( #155985, #173315, #153854, #139758, #41186, #7573, #105117, #203631, #171157, #137615, #75795, #158128, #55283, #121432, #58480, #107293, #154920, #202565, #186332, #73658, #123576, #42250, #188472, #138680, #174387, #39033, #37966, #145101, #47586, #125694, #97397, #191653, #163453, #94203, #129962, #113700, #10774, #46505, #45445, #13967, #43318, #176497, #112628, #15033, #78982, #80051, #161318, #126761, #109436, #192721, #28108, #77920, #31321, #178638, #210036, #27027, #211105, #62729, #146154, #111560, #96334, #29181, #60602, #177568, #141903, #44375, #207913, #175442, #144039, #95270, #59534, #93135, #128890, #61676, #30250, #12902, #162390, #159174, #127844, #194871, #76848, #195950, #212170, #160243, #63804, #142967, #179704, #208970, #11843, #110498, #193796, #149326, #52888, #18236, #116883, #49690, #83241, #213235, #100572, #3043, #36629, #34498, #19309, #183950, #119023, #200184, #35560, #197004, #82179, #51837, #185005, #85388, #117955, #48639, #66973, #69112, #148273, #165572, #114757, #133112, #182882, #147210, #151472, #904, #101641, #198061, #164511, #166645, #115818, #199109, #84320, #167707, #180754, #150406, #134176, #50754, #181805, #214272, #33438, #32381, #168771, #102714, #16095, #98447, #135234, #201247, #99515, #81125, #64867, #1973, #68036, #131012, #65905, #17167, #132051, #202312, #4110, #23575, #140586, #156810, #87534, #104860, #53961, #6250, #122254, #86461, #90750, #22497, #123325, #137362, #103787, #56098, #203379, #88609, #188213, #205527, #136291, #171983, #73396, #204444, #55032, #21425, #121180, #120099, #108112, #124384, #169838, #186077, #57162, #139499, #187149, #20376, #152525, #39853, #105959, #24640, #154664, #38778, #72319, #37711, #70179, #89684, #206598, #153601, #190342, #170904, #8397, #58226, #5173, #189288, #138425, #107034, #71246, #155733, #40930, #42004, #7318, #173060, #74481, #161882, #9472, #13469, #63297, #113187, #66453, #81671, #30815, #59285, #180251, #31875, #181299, #80618, #131543, #64366, #95823, #146711, #198597, #79545, #50244, #75545, #179191, #212727, #174139, #25713, #97954, #96894, #147757, #196499, #213775, #141654, #162943, #130512, #157879, #16649, #65397, #211659, #49190, #207666, #197545, #99002, #195440, #43072, #47070, #14524, #148810, #114255, #48142, #145663, #164008, #91822, #15584, #165057, #132595, #115309, #32926, #82734, #379, #125444, #191405, #109185, #178126, #29741, #129457, #54507, #87001, #17707, #102189, #166122, #101109, #2520, #52376, #5715, #20905, #184487, #1454, #119569, #185556, #120651, #19855, #70720, #3586, #35035, #85942, #137907, #167195, #203926, #83794, #118505, #152015, #116364, #182354, #37185, #36104, #153073, #135769, #4650, #149889, #168256, #69661, #100058, #170379, #136833, #150956, #202859, #67519, #186630, #38257, #134719, #199665, #200725, #201792, #88074, #53432, #103260, #84868, #169321, #33982, #104331, #21966, #71792, #154148, #133664, #51311, #117437, #183434, #18782, #68593, #56644, #26259, #27331, #208205, #92375, #171455, #41481, #191947, #122808, #140051, #89160, #107592, #157358, #121728, #125990, #57710, #158412, #172536, #138977, #91300, #24120, #123867, #8947, #10012, #23044, #207149, #108657, #25196, #90223, #188767, #156287, #155213, #143271, #159473, #205000, #6794, #76088, #174685, #7871, #55574 ),
 ( #39322, #11071, #73959, #43613, #175738, #40407, #142190, #173624, #59837, #105417, #206076, #109731, #77150, #58772, #93433, #75027, #106509, #124927, #72871, #189832, #187693, #141139, #190888, #42554, #14264, #28408, #144342, #131303, #210342, #209261, #115053, #94502, #30556, #61981, #145408, #177871, #48935, #47890, #81422, #112929, #194099, #196246, #98747, #212469, #128135, #64113, #60906, #160540, #12146, #213524, #29483, #97695, #114002, #164804, #211408, #45748, #179997, #95574, #15333, #181051, #16396, #31621, #78219, #127065, #111866, #161624, #65147, #178942, #80355, #146454, #130255, #193027, #163753, #147503, #63038, #82475, #44679, #197294, #13217, #79290, #129205, #32667, #176793, #195182, #46815, #96635, #162689, #110791, #20659, #133407, #103006, #149624, #52124, #2266, #148565, #68342, #18538, #1206, #100861, #54258, #67268, #199412, #166945, #84615, #182099, #51057, #119313, #183182, #200478, #134475, #186370, #165872, #34786, #86750, #49989, #17458, #33729, #118253, #117181, #169062, #184234, #152821, #4397, #66199, #185299, #170126, #131, #120395, #116107, #151768, #150704, #35858, #101937, #168002, #36923, #19608, #38005, #135515, #85680, #70468, #3338, #136585, #202605, #69408, #201537, #104077, #53185, #21711, #132343, #198349, #99807, #83543, #58518, #122551, #139795, #7614, #125733, #105158, #188512, #26002, #203673, #171197, #121473, #205823, #72621, #42291, #123615, #92111, #174426, #5463, #124673, #109474, #153894, #207953, #55322, #91040, #40142, #57455, #156025, #172279, #190630, #189578, #191694, #74772, #73697, #9758, #89973, #108402, #75833, #106255, #41226, #157100, #187444, #22787, #206886, #107331, #173355, #24937, #8689, #39072, #88904, #141940, #154957, #87822, #59576, #6543, #140875, #138720, #23866, #56387, #43354, #158167, #175482, #71543, #204738, #137653, #131047, #30289, #28148, #96374, #27070, #192760, #126804, #31357, #61716, #129999, #80087, #197037, #29221, #11884, #146191, #210077, #47622, #213271, #48672, #212206, #44417, #93177, #60642, #127884, #97432, #145139, #112666, #46546, #178674, #159211, #162426, #63842, #95311, #114789, #10812, #195989, #110537, #94243, #160282, #113734, #209005, #45485, #12943, #161360, #111601, #179740, #163487, #77960, #15069, #144081, #211145, #79022, #76887, #62767, #177609, #193835, #128931, #81161, #194908, #14003, #147244, #143007, #64900, #176537, #181836, #133144, #86490, #33471, #17198, #199144, #116917, #214305, #99545, #151504, #942, #18272, #100604, #4141, #198095, #67007, #119051, #82213, #49722, #65936, #84354, #165608, #135265, #2006, #185036, #52920, #98478, #3072, #202341, #32412, #152554, #148306, #183983, #50788, #150444, #34533, #182917, #69144, #68072, #70211, #167742, #166680, #102746, #134208, #201279, #168802, #200217, #51869, #35594, #132085, #115851, #85420, #117990, #101672, #19341, #36661, #83272, #149360, #20407, #136323, #180789, #53993, #164544, #16129, #55061, #56129, #88641, #174176, #173095, #206632, #23608, #104894, #107070, #9510, #123358, #121212, #189323, #120132, #71278, #5205, #124419, #154698, #8429, #24676, #75582, #122288, #170933, #90782, #6281, #140620, #91859, #141691, #156845, #137392, #186109, #153632, #72353, #190378, #89716, #205558, #139533, #57198, #37742, #40963, #74517, #188245, #207705 ),
 ( #58263, #42037, #22532, #105996, #7351, #103818, #108150, #39886, #25747, #138457, #203409, #155767, #204476, #172017, #73430, #157915, #21456, #169865, #87564, #187181, #38808, #60385, #27895, #158968, #147002, #163238, #142751, #92922, #30033, #112412, #160031, #59325, #191444, #12689, #78765, #63594, #61459, #11633, #193589, #26818, #43109, #62522, #179489, #109224, #14820, #77706, #47369, #31111, #208760, #178424, #177353, #145945, #175234, #93990, #96119, #80912, #210895, #211956, #144888, #44162, #10562, #110282, #143826, #209823, #125482, #162174, #127625, #76637, #128684, #194653, #129749, #28967, #13760, #161101, #192510, #95050, #126549, #176291, #45233, #111348, #46297, #79836, #195734, #113482, #97184, #679, #183729, #18009, #35337, #48431, #132887, #34277, #196790, #52665, #101416, #33218, #85165, #114546, #167489, #135008, #16944, #81966, #83023, #66745, #184781, #150186, #100350, #181589, #198890, #130796, #84099, #201021, #168550, #166416, #151249, #19084, #36407, #117738, #2817, #180538, #214059, #68889, #102486, #118794, #20149, #32161, #50536, #86234, #65687, #149098, #98238, #1755, #67812, #99302, #116659, #164293, #133959, #213020, #64655, #199967, #15882, #148053, #131835, #197842, #49475, #115595, #165349, #182657, #51615, #90520, #123109, #53737, #138202, #74261, #4942, #22266, #185848, #204214, #39615, #3881, #8177, #154442, #40702, #54805, #21200, #187990, #120953, #6022, #105719, #189067, #119869, #89455, #205298, #122023, #186924, #153371, #38555, #37480, #25493, #41779, #87302, #103557, #106806, #56936, #104632, #152305, #69952, #171748, #23344, #156583, #72092, #170679, #55866, #169616, #136064, #155507, #57999, #202077, #107892, #88375, #140354, #124163, #71018, #172835, #7089, #24406, #137131, #73162, #206372, #173920, #139268, #190125, #203160, #76379, #141437, #142487, #192246, #27628, #195476, #210644, #159768, #191180, #94792, #160840, #95863, #209557, #46040, #193330, #10305, #61202, #113225, #208494, #179229, #207443, #93728, #127360, #91600, #157651, #12432, #11367, #62270, #111084, #128431, #59062, #77446, #44976, #75320, #145700, #194397, #126287, #178164, #125221, #112161, #13510, #110022, #174975, #176036, #143564, #63336, #42848, #9249, #108955, #43908, #161919, #177090, #28706, #78512, #144629, #26557, #29779, #79582, #211699, #92664, #158708, #129495, #60129, #47109, #31915, #117481, #212768, #49232, #16691, #165100, #115351, #67562, #183472, #15630, #199711, #97993, #148849, #99045, #30855, #82777, #181342, #164051, #197588, #150997, #81717, #147799, #32969, #422, #64404, #213817, #1496, #65435, #66494, #132634, #68636, #48182, #131586, #35079, #146750, #114294, #130548, #198640, #50288, #51357, #116407, #101150, #167236, #162982, #133705, #52419, #96932, #2565, #196539, #34026, #182397, #100100, #166160, #17747, #18824, #83836, #134760, #149927, #84909, #200768, #118545, #14562, #80659, #180292, #91074, #190664, #88938, #56423, #92148, #157135, #8726, #140909, #206922, #6576, #122584, #109508, #188546, #184527, #93212, #72656, #74808, #40176, #123650, #156059, #27105, #26036, #59613, #58551, #172310, #174460, #76918, #42324, #106290, #108440, #36148, #138752, #204770, #191731, #7647, #75866, #158202, #143044, #189612, #23899, #9791, #73732, #207985, #159244, #209039, #141973 ),
 ( #125769, #43387, #154991, #173389, #175515, #90005, #57489, #139828, #24972, #124705, #102229, #10844, #41258, #60675, #205857, #107368, #168300, #22823, #128966, #80123, #97466, #28182, #63879, #179774, #96411, #29256, #127918, #95348, #11922, #214340, #16164, #210111, #160318, #163522, #31391, #12982, #126838, #44453, #146228, #212245, #131083, #194946, #79056, #46582, #94277, #110570, #130033, #32448, #176572, #82249, #145174, #114823, #98517, #61751, #15109, #30327, #213308, #77995, #161398, #81198, #148340, #196024, #64933, #47660, #111636, #144117, #177647, #211179, #62805, #192795, #147276, #112701, #193871, #113771, #197072, #48709, #162461, #180821, #14037, #45520, #164579, #178711, #116953, #153670, #181872, #68108, #101706, #65970, #132119, #69178, #134244, #36696, #85454, #102781, #115887, #200251, #167778, #49761, #120167, #168838, #100638, #152589, #33508, #20442, #202380, #84391, #149395, #150478, #51903, #37778, #3107, #19374, #34567, #118025, #198129, #151539, #165645, #135298, #977, #2038, #166715, #186143, #119090, #4176, #184013, #50826, #52952, #169900, #201312, #67043, #185070, #99581, #17233, #83308, #70245, #18305, #86524, #136360, #21489, #35628, #182952, #54030, #103852, #87599, #133180, #199180, #124454, #104930, #71314, #38847, #106032, #9541, #123394, #90815, #24713, #156879, #137426, #8466, #190413, #7388, #92955, #203445, #108183, #170972, #72393, #6319, #91894, #187218, #23647, #205596, #139569, #89755, #42069, #157950, #204514, #174209, #138493, #189358, #73468, #5238, #57233, #155805, #56162, #172054, #125515, #122326, #188283, #40998, #107109, #22571, #39924, #25782, #173132, #74552, #140653, #43145, #88677, #206666, #75616, #121248, #154736, #58298, #141727, #207735, #59358, #191477, #109258, #175266, #55099, #26851, #180569, #10595, #64683, #126582, #162205, #45262, #62551, #12722, #28999, #47402, #194685, #196821, #145975, #78795, #80940, #161134, #113514, #147032, #177385, #128714, #13792, #60422, #27929, #63628, #46327, #112443, #178456, #30065, #192543, #94023, #213054, #160062, #159002, #130829, #96154, #79866, #211987, #76671, #129782, #195763, #144918, #32191, #142786, #179522, #110316, #11666, #77740, #31141, #44196, #95086, #210925, #97216, #163268, #14850, #48463, #143861, #114577, #209854, #208792, #176323, #61492, #127657, #193621, #111382, #50569, #3917, #165382, #149132, #116691, #34308, #131866, #16975, #68922, #132918, #150218, #18045, #136098, #115625, #198923, #36444, #214090, #181620, #197873, #1790, #83056, #52697, #133994, #102518, #184814, #15915, #135043, #119907, #164325, #69986, #65718, #101448, #182690, #67847, #166455, #100383, #201056, #200000, #202114, #85197, #84132, #20181, #51650, #118828, #86268, #117773, #183764, #167521, #49505, #33249, #2853, #35374, #19118, #151282, #168581, #99333, #713, #152339, #66777, #98267, #53774, #185882, #81998, #148085, #188024, #6059, #91635, #90558, #124198, #155548, #22302, #24445, #141470, #40737, #38591, #106843, #37517, #203195, #137171, #41816, #72130, #140391, #156620, #207477, #39653, #88413, #8210, #138237, #58034, #9285, #59097, #74295, #54841, #103593, #71055, #204251, #107929, #7127, #73200, #55903, #105762, #169650, #56973, #173953, #125257, #205335, #190162, #206410, #75358, #25527, #157687, #153408, #104668 ),
 ( #139306, #21235, #87340, #171787, #4977, #154481, #120992, #123147, #122060, #23382, #189104, #186959, #170716, #172874, #89494, #160876, #93760, #192279, #159799, #76409, #64438, #80694, #60164, #10335, #161953, #29816, #77480, #191217, #108989, #144663, #210677, #195508, #193365, #143599, #111120, #158741, #175008, #194432, #96967, #26594, #146785, #209591, #179266, #163015, #126318, #95900, #94825, #63372, #92695, #11402, #13544, #212800, #128464, #129528, #62305, #176067, #142519, #27665, #61237, #127393, #42880, #79615, #45010, #208528, #46073, #112194, #47145, #12470, #145734, #78545, #110055, #178199, #43939, #177123, #28740, #211734, #113261, #30889, #14597, #68669, #34058, #16723, #1530, #116437, #67593, #114326, #148884, #132668, #48214, #101184, #133738, #115384, #199745, #180322, #51391, #35113, #33002, #81750, #99080, #82808, #18858, #100131, #2600, #131620, #130582, #31944, #457, #50319, #196572, #98028, #117512, #182431, #167273, #149961, #84942, #147832, #166192, #17782, #213850, #164082, #151031, #66525, #15663, #197619, #65469, #49263, #83870, #198674, #183505, #181378, #165132, #46775, #145369, #78177, #111826, #27289, #129162, #31579, #65108, #62993, #47848, #212427, #147463, #14219, #64069, #11031, #110754, #80314, #81379, #113959, #146414, #77109, #95536, #97653, #176752, #194055, #143233, #161585, #211368, #175699, #179956, #177828, #130213, #12107, #192985, #195139, #196206, #15294, #209223, #112889, #44639, #45707, #144305, #163712, #162646, #213484, #13173, #94462, #96596, #131264, #178901, #28367, #30515, #109695, #60865, #127027, #197251, #210299, #93396, #159432, #160502, #29445, #61939, #128097, #79251, #209662, #143669, #210743, #79683, #46143, #178271, #141535, #177192, #176136, #144732, #107991, #92763, #28808, #13608, #61303, #62367, #77546, #42947, #174020, #109056, #158808, #208596, #162019, #94892, #126388, #157753, #127465, #193436, #128529, #27736, #12537, #159871, #191281, #93830, #60228, #10404, #192347, #25589, #41880, #45080, #111189, #160944, #194498, #145796, #112257, #29881, #207543, #78610, #11475, #95965, #91701, #76477, #58103, #124262, #190221, #9351, #75423, #175073, #59163, #26660, #142588, #44005, #125321, #110124, #65537, #97032, #521, #66589, #1594, #115449, #166260, #99146, #130646, #181439, #18922, #48278, #85007, #113329, #213914, #33068, #211802, #63440, #132733, #131683, #182495, #16789, #34123, #47214, #197685, #165196, #195578, #51455, #100194, #32010, #83935, #179336, #17850, #133801, #15730, #80760, #81815, #49330, #183570, #148950, #82872, #180386, #198736, #129590, #50383, #199811, #167336, #116504, #150025, #67655, #35176, #117575, #101253, #30957, #212868, #163086, #14667, #146849, #64503, #196638, #114391, #98093, #164145, #147898, #184627, #136976, #38394, #2662, #6931, #153213, #39460, #53577, #188903, #103398, #105555, #169458, #104474, #121862, #52509, #88216, #204056, #120791, #119711, #152152, #185693, #36244, #24253, #40545, #19993, #102323, #187833, #55708, #37323, #151098, #68735, #170521, #22103, #155348, #186768, #134856, #200862, #154287, #4783, #171590, #5861, #23183, #118642, #70861, #71933, #168396, #205137, #89297, #21045, #73010, #86077, #139109, #56780, #87142, #3722, #203003, #54643, #122946, #138043, #106649, #172676, #69797, #135906, #201924 ) ),
 .UNSPECIFIED., .T., .F., .F. ) 
 B_SPLINE_SURFACE_WITH_KNOTS ( ( 4, 3, 4 ),
 ( 4, 1, 1, 1, 1, 1, 1, 1, 1, 1, 1, 1, 1, 1, 1, 1, 1, 1, 1, 1, 1, 1, 1, 1, 1, 1, 1, 1, 1, 1, 1, 1, 1, 1, 1, 1, 1, 1, 1, 1, 1, 1, 1, 1, 1, 1, 1, 1, 1, 1, 1, 1, 1, 1, 1, 1, 1, 1, 1, 1, 1, 1, 1, 1, 1, 1, 1, 1, 1, 1, 1, 1, 1, 1, 1, 1, 1, 1, 1, 1, 1, 1, 1, 1, 1, 1, 1, 1, 1, 1, 1, 1, 1, 1, 1, 1, 1, 1, 1, 1, 1, 1, 1, 1, 1, 1, 1, 1, 1, 1, 1, 1, 1, 1, 1, 1, 1, 1, 1, 1, 1, 1, 1, 1, 1, 1, 1, 1, 1, 1, 1, 1, 1, 1, 1, 1, 1, 1, 1, 1, 1, 1, 1, 1, 1, 1, 1, 1, 1, 1, 1, 1, 1, 1, 1, 1, 1, 1, 1, 1, 1, 1, 1, 1, 1, 1, 1, 1, 1, 1, 1, 1, 1, 1, 1, 1, 1, 1, 1, 1, 1, 1, 1, 1, 1, 1, 1, 1, 1, 1, 1, 1, 1, 1, 1, 1, 1, 1, 1, 1, 1, 1, 1, 1, 1, 1, 1, 1, 1, 1, 1, 1, 1, 1, 1, 1, 1, 1, 1, 1, 1, 1, 1, 1, 1, 1, 1, 1, 1, 1, 1, 1, 1, 1, 1, 1, 1, 1, 1, 1, 1, 1, 1, 1, 1, 1, 1, 1, 1, 1, 1, 1, 1, 1, 1, 1, 1, 1, 1, 1, 1, 1, 1, 1, 1, 1, 1, 1, 1, 1, 1, 1, 1, 1, 1, 1, 1, 1, 1, 1, 1, 1, 1, 1, 1, 1, 1, 1, 1, 1, 1, 1, 1, 1, 1, 1, 1, 1, 1, 1, 1, 1, 1, 1, 1, 1, 1, 1, 1, 1, 1, 1, 1, 1, 1, 1, 1, 1, 1, 1, 1, 1, 1, 1, 1, 1, 1, 1, 1, 1, 1, 1, 1, 1, 1, 1, 1, 1, 1, 1, 1, 1, 1, 1, 1, 1, 1, 1, 1, 1, 1, 1, 1, 1, 1, 1, 1, 1, 1, 1, 1, 1, 1, 1, 1, 1, 1, 1, 1, 1, 1, 1, 1, 1, 1, 1, 1, 1, 1, 1, 1, 1, 1, 1, 4 ),
 ( 0.000000000000000000, 0.5000000000000000000, 1.000000000000000000 ),
 ( 0.000000000000000000, 0.002599909708945224215, 0.005208776875251038344, 0.007813105021672143990, 0.01041684075506122895, 0.01302033053878596733, 0.01562516449037322508, 0.01822901888718816976, 0.02083333248856494152, 0.02343767784666880849, 0.02604151204071371642, 0.02864616705684025488, 0.03124974664057501156, 0.03385445107693609706, 0.03645811663825353210, 0.03906264587105176544, 0.04166673705245293319, 0.04427082116499847508, 0.04687535697974040683, 0.04947901875943551409, 0.05208372524935509645, 0.05468730636643894666, 0.05729195276349181160, 0.05989578571700067411, 0.06250012971910297310, 0.06510448174046053194, 0.06770830932160050442, 0.07031296016926287529, 0.07291653972921435800, 0.07552124384959360559, 0.07812490789241745281, 0.08072943556986492131, 0.08333352577934262373, 0.08593760861062926804, 0.08854214333088818167, 0.09114580385899402615, 0.09375050919907033931, 0.09635408915385039463, 0.09895873428887830281, 0.1015625661591952889, 0.1041669088510773916, 0.1067712598504420435, 0.1093750861808121810, 0.1119797359579501050, 0.1145833143474069837, 0.1171880172914337714, 0.1197916802446672702, 0.1223962066585842084, 0.1250002958591681090, 0.1276043774339237491, 0.1302089111537957367, 0.1328125705047451810, 0.1354172747579587832, 0.1380208536162275679, 0.1406254975582941213, 0.1432293284131295197, 0.1458336698625422867, 0.1484380199076493767, 0.1510418450546419100, 0.1536464938294531402, 0.1562500711155297428, 0.1588547729514310503, 0.1614584348822658832, 0.1640629601007041471, 0.1666670483599762276, 0.1692711287458052438, 0.1718756615333107141, 0.1744793197742946778, 0.1770840230088624179, 0.1796876008377196188, 0.1822922436549848091, 0.1848960735616705098, 0.1875004138364584350, 0.1901047629951247708, 0.1927085870260826783, 0.1953132348667029061, 0.1979168111164897881, 0.2005215119124719170, 0.2031251728880697216, 0.2057296969790492203, 0.2083337843645647058, 0.2109378636290424602, 0.2135423955521746908, 0.2161460527503557827, 0.2187507550344668650, 0.2213543319009846355, 0.2239589736615800464, 0.2265628026874214052, 0.2291671418554001027, 0.2317714901954165685, 0.2343753131776551424, 0.2369799601521939414, 0.2395835354327550959, 0.2421882352569974250, 0.2447918953444941648, 0.2473964183760076208, 0.2500005049552969649, 0.2526045831659717300, 0.2552091142926994904, 0.2578127705152143956, 0.2604174719170327390, 0.2630210478882585856, 0.2656256886602897938, 0.2682295168725681855, 0.2708338550015275126, 0.2734382025906618163, 0.2760420245914711468, 0.2786466707680146371, 0.2812502451463897990, 0.2838549440670474211, 0.2864586033335557724, 0.2890631253735708728, 0.2916672112141422968, 0.2942712884385379479, 0.2968758188368077477, 0.2994794741507696423, 0.3020841747384366283, 0.3046877498813952978, 0.3072923897329448151, 0.3098962171989202430, 0.3125005543566263810, 0.3151049012626256918, 0.3177087223492732204, 0.3203133677958864278, 0.3229169413390938770, 0.3255216394243000688, 0.3281252979369121969, 0.3307298190533745630, 0.3333339042227165261, 0.3359379805283350118, 0.3385425102660742369, 0.3411461647385755636, 0.3437508645802123675, 0.3463544389619092612, 0.3489590779610384774, 0.3515629047479519320, 0.3541672410021501904, 0.3567715872927431642, 0.3593754075324762653, 0.3619800523172059803, 0.3645836250922447341, 0.3671883224101137877, 0.3697919802359038166, 0.3723965004967392245, 0.3750005850623230885, 0.3776046605166471504, 0.3802091896617659783, 0.3828128433598806946, 0.3854175425235913388, 0.3880211162110140388, 0.3906257544257662473, 0.3932295806008425099, 0.3958339160192597128, 0.3984382617621595180, 0.4010420812222079689, 0.4036467254130849946, 0.4062502974869375283, 0.4088549941055670267, 0.4114586513115932598, 0.4140631707847102772, 0.4166672548139925825, 0.4192713294844879757, 0.4218758581048823730, 0.4244795110956688933, 0.4270842096495421902, 0.4296877827096635682, 0.4322924202080664635, 0.4348962458385162155, 0.4375005804888632555, 0.4401049257517701263, 0.4427087444993486054, 0.4453133881643903114, 0.4479169596040251111, 0.4505216555914985932, 0.4531253122448062887, 0.4557298309980991058, 0.4583339145585244578, 0.4609379885126426157, 0.4635425166761967808, 0.4661461690266998081, 0.4687508670388120247, 0.4713544395385928509, 0.4739590763886608604, 0.4765629015416836811, 0.4791672354916582388, 0.4817715803422617515, 0.4843753984445725025, 0.4869800416517858221, 0.4895836125241597725, 0.4921883079485492862, 0.4947919641161733773, 0.4973964822175238609, 0.5000005653765271507, 0.5026046386817077938, 0.5052091664562964324, 0.5078128182335502894, 0.5104175157719683664, 0.5130210877783591972, 0.5156257240480961457, 0.5182295487908826770, 0.5208338821081714975, 0.5234382266141532902, 0.5260420441383883983, 0.5286466869557716608, 0.5312502573278325979, 0.5338549522572011430, 0.5364586080061681805, 0.5390631255234488162, 0.5416672083484578293, 0.5442712810721315186, 0.5468758085256230084, 0.5494794597966533578, 0.5520841569294364648, 0.5546877285093810839, 0.5572923642667827471, 0.5598961886665174692, 0.5625005214187991376, 0.5651048656478350196, 0.5677086826611791315, 0.5703133251567252815, 0.5729168950954143247, 0.5755215895978186280, 0.5781252449951498340, 0.5807297619962258350, 0.5833338445546641937, 0.5859379167642547737, 0.5885424439645127181, 0.5911460947963396162, 0.5937507915915425372, 0.5963543628119793993, 0.5989589981250363904, 0.6015628222488997867, 0.6041671545038470592, 0.6067714985236103420, 0.6093753150932430529, 0.6119799573349418154, 0.6145835269071964202, 0.6171882210506893784, 0.6197918761634028106, 0.6223963927161352272, 0.6250004750754242222, 0.6276045468383509851, 0.6302090738532378777, 0.6328127243128783830, 0.6354174208385534595, 0.6380209917664191321, 0.6406256267031188445, 0.6432294506182901772, 0.6458337824435727015, 0.6484381263217364744, 0.6510419425148348260, 0.6536465845706755928, 0.6562501538434313275, 0.6588548476960643940, 0.6614585025911776661, 0.6640630187634258830, 0.6666671009909873602, 0.6692711723746683772, 0.6718756992720475996, 0.6744793494265174383, 0.6770840457507175669, 0.6796876164529486175, 0.6822922510812780006, 0.6848960748549377531, 0.6875004063182246217, 0.6901047501224634173, 0.6927085660062048955, 0.6953132079441787239, 0.6979167769843723779, 0.7005214706141982273, 0.7031251253587310623, 0.7057296412183544643, 0.7083337233816132672, 0.7109377944534676086, 0.7135423213012055399, 0.7161459712175226588, 0.7187506674083037339, 0.7213542379518396164, 0.7239588723397878400, 0.7265626960391206035, 0.7291670272080824633, 0.7317713710060759214, 0.7343751866476402324, 0.7369798285357428425, 0.7395833974103146469, 0.7421880908853900616, 0.7447917455463664016, 0.7473962611612280371, 0.7500003433276148934, 0.7526044141550642941, 0.7552089410210337528, 0.7578125907662203176, 0.7604172868916432293, 0.7630208573434285046, 0.7656254915589897347, 0.7682293152511859846, 0.7708336461934980344, 0.7734379900529331220, 0.7760418055195050790, 0.7786464474257392965, 0.7812500162016354777, 0.7838547095900232353, 0.7864583642344741277, 0.7890628796724428184, 0.7916669619093961163, 0.7942710325598689725, 0.7968755595119511037, 0.7994792091530360523, 0.8020839052811703507, 0.8046874757081575735, 0.8072921098193328593, 0.8098959335715922858, 0.8125002643549369408, 0.8151046083435100620, 0.8177084237022821389, 0.8203130656946604482, 0.8229166344388356702, 0.8255213278086077633, 0.8281249825035741363, 0.8307294978325265866, 0.8333335802074958165, 0.8359376507484286289, 0.8385421778545157911, 0.8411458274585372763, 0.8437505236574627254, 0.8463540941266142204, 0.8489587282014147140, 0.8515625520809478877, 0.8541668827730166669, 0.8567712269584367712, 0.8593750422766117669, 0.8619796844231587540, 0.8645832532025788941, 0.8671879466218186394, 0.8697916014343529678, 0.8723961167221769841, 0.8750001993026245151, 0.8776042698014647758, 0.8802087971294628721, 0.8828124467634709260, 0.8854171431012803906, 0.8880207136795719158, 0.8906253477860208712, 0.8932291718600525732, 0.8958335025285494302, 0.8984378469785403443, 0.9010416623233333810, 0.9036463046920883979, 0.9062498735737328781, 0.9088545671105374701, 0.9114582221077071056, 0.9140627374223044832, 0.9166668202757080053, 0.9192708907999164181, 0.9218754184177497812, 0.9244790681488107564, 0.9270837646936044285, 0.9296873354480212903, 0.9322919696541906998, 0.9348957939899811276, 0.9375001247025137596, 0.9401044694846933947, 0.9427082849236875228, 0.9453129275835465695, 0.9479164966330613229, 0.9505211903504858784, 0.9531248456066239161, 0.9557293610412391782, 0.9583334441921064206, 0.9609375147049603605, 0.9635420428945489224, 0.9661456931510739032, 0.9687503890924937799, 0.9713539588735070618, 0.9739585961357111188, 0.9765624261165479769, 0.9791667493207181217, 0.9817710620974646751, 0.9843748983037424738, 0.9869797303524157073, 0.9895832060093603388, 0.9921869237806116848, 0.9947912468131487884, 0.9974000922265050528, 0.9999999999999998890 ),
 .UNSPECIFIED. ) 
 GEOMETRIC_REPRESENTATION_ITEM ( )  RATIONAL_B_SPLINE_SURFACE ( (
 ( 1.000000000000000000, 1.000000000000000000, 1.000000000000000000, 0.9999999999999997780, 1.000000000000000000, 1.000000000000000444, 0.9999999999999996669, 0.9999999999999996669, 1.000000000000000444, 1.000000000000000000, 1.000000000000000000, 1.000000000000000000, 1.000000000000000222, 1.000000000000000222, 0.9999999999999997780, 1.000000000000000000, 1.000000000000000222, 1.000000000000000000, 1.000000000000000222, 0.9999999999999994449, 1.000000000000000222, 0.9999999999999997780, 1.000000000000000444, 1.000000000000000000, 1.000000000000000000, 1.000000000000000222, 0.9999999999999997780, 1.000000000000000222, 1.000000000000000000, 1.000000000000000222, 0.9999999999999997780, 1.000000000000000000, 1.000000000000000000, 0.9999999999999997780, 1.000000000000000000, 1.000000000000000000, 1.000000000000000222, 1.000000000000000000, 0.9999999999999997780, 1.000000000000000222, 0.9999999999999997780, 1.000000000000000000, 0.9999999999999997780, 1.000000000000000444, 0.9999999999999996669, 1.000000000000000222, 1.000000000000000000, 1.000000000000000000, 1.000000000000000444, 0.9999999999999996669, 1.000000000000000222, 1.000000000000000444, 1.000000000000000000, 0.9999999999999997780, 1.000000000000000444, 1.000000000000000222, 1.000000000000000000, 1.000000000000000000, 1.000000000000000222, 1.000000000000000000, 1.000000000000000222, 0.9999999999999997780, 1.000000000000000222, 1.000000000000000000, 1.000000000000000000, 1.000000000000000444, 0.9999999999999996669, 1.000000000000000000, 0.9999999999999997780, 1.000000000000000222, 0.9999999999999996669, 1.000000000000000000, 1.000000000000000222, 0.9999999999999997780, 1.000000000000000444, 0.9999999999999997780, 1.000000000000000000, 0.9999999999999997780, 1.000000000000000222, 0.9999999999999996669, 1.000000000000000000, 1.000000000000000222, 0.9999999999999996669, 1.000000000000000444, 0.9999999999999997780, 1.000000000000000000, 1.000000000000000222, 0.9999999999999996669, 1.000000000000000222, 1.000000000000000000, 0.9999999999999997780, 1.000000000000000222, 0.9999999999999997780, 1.000000000000000000, 1.000000000000000222, 0.9999999999999997780, 1.000000000000000000, 1.000000000000000000, 0.9999999999999997780, 1.000000000000000000, 1.000000000000000222, 0.9999999999999997780, 1.000000000000000000, 1.000000000000000000, 1.000000000000000000, 0.9999999999999997780, 1.000000000000000222, 0.9999999999999997780, 0.9999999999999997780, 1.000000000000000444, 1.000000000000000000, 1.000000000000000000, 0.9999999999999997780, 1.000000000000000222, 1.000000000000000000, 1.000000000000000000, 1.000000000000000000, 1.000000000000000000, 1.000000000000000222, 1.000000000000000222, 0.9999999999999997780, 1.000000000000000000, 0.9999999999999997780, 1.000000000000000444, 0.9999999999999996669, 1.000000000000000666, 1.000000000000000000, 0.9999999999999997780, 1.000000000000000222, 1.000000000000000000, 1.000000000000000000, 1.000000000000000000, 0.9999999999999994449, 1.000000000000000666, 0.9999999999999996669, 1.000000000000000000, 1.000000000000000222, 0.9999999999999997780, 1.000000000000000222, 0.9999999999999997780, 1.000000000000000222, 0.9999999999999996669, 1.000000000000000444, 1.000000000000000000, 1.000000000000000222, 0.9999999999999996669, 1.000000000000000000, 1.000000000000000222, 0.9999999999999997780, 1.000000000000000000, 0.9999999999999997780, 1.000000000000000000, 1.000000000000000000, 1.000000000000000222, 0.9999999999999997780, 1.000000000000000222, 0.9999999999999997780, 1.000000000000000000, 1.000000000000000000, 1.000000000000000222, 0.9999999999999997780, 1.000000000000000444, 1.000000000000000000, 0.9999999999999997780, 1.000000000000000000, 1.000000000000000000, 1.000000000000000222, 0.9999999999999997780, 1.000000000000000222, 1.000000000000000000, 1.000000000000000000, 1.000000000000000000, 1.000000000000000222, 1.000000000000000000, 0.9999999999999997780, 1.000000000000000000, 1.000000000000000000, 1.000000000000000000, 1.000000000000000444, 0.9999999999999996669, 1.000000000000000222, 1.000000000000000000, 1.000000000000000222, 0.9999999999999997780, 1.000000000000000000, 0.9999999999999997780, 1.000000000000000000, 0.9999999999999997780, 1.000000000000000000, 1.000000000000000444, 0.9999999999999994449, 1.000000000000000444, 1.000000000000000000, 1.000000000000000222, 1.000000000000000222, 0.9999999999999997780, 1.000000000000000222, 0.9999999999999997780, 1.000000000000000222, 1.000000000000000222, 1.000000000000000222, 0.9999999999999997780, 1.000000000000000000, 1.000000000000000444, 0.9999999999999996669, 1.000000000000000000, 0.9999999999999997780, 1.000000000000000222, 1.000000000000000222, 1.000000000000000000, 0.9999999999999997780, 1.000000000000000222, 0.9999999999999997780, 1.000000000000000222, 0.9999999999999997780, 0.9999999999999997780, 1.000000000000000000, 1.000000000000000000, 1.000000000000000000, 1.000000000000000000, 1.000000000000000000, 1.000000000000000222, 1.000000000000000000, 1.000000000000000000, 1.000000000000000222, 1.000000000000000000, 0.9999999999999997780, 1.000000000000000000, 1.000000000000000000, 1.000000000000000000, 0.9999999999999997780, 1.000000000000000000, 0.9999999999999997780, 1.000000000000000000, 1.000000000000000222, 0.9999999999999996669, 1.000000000000000444, 1.000000000000000000, 0.9999999999999997780, 1.000000000000000222, 1.000000000000000000, 0.9999999999999997780, 1.000000000000000222, 1.000000000000000000, 1.000000000000000222, 1.000000000000000000, 0.9999999999999997780, 1.000000000000000222, 1.000000000000000000, 1.000000000000000000, 1.000000000000000222, 1.000000000000000000, 1.000000000000000000, 1.000000000000000222, 0.9999999999999997780, 0.9999999999999996669, 1.000000000000000444, 0.9999999999999994449, 1.000000000000000444, 0.9999999999999997780, 1.000000000000000222, 1.000000000000000000, 1.000000000000000000, 1.000000000000000000, 1.000000000000000000, 1.000000000000000444, 0.9999999999999996669, 1.000000000000000444, 1.000000000000000000, 0.9999999999999997780, 1.000000000000000444, 0.9999999999999994449, 1.000000000000000444, 0.9999999999999997780, 0.9999999999999997780, 1.000000000000000222, 1.000000000000000444, 0.9999999999999997780, 1.000000000000000444, 0.9999999999999997780, 1.000000000000000000, 1.000000000000000444, 0.9999999999999997780, 0.9999999999999997780, 1.000000000000000000, 1.000000000000000000, 1.000000000000000000, 0.9999999999999997780, 1.000000000000000444, 1.000000000000000222, 0.9999999999999997780, 1.000000000000000444, 1.000000000000000000, 1.000000000000000222, 1.000000000000000000, 1.000000000000000000, 1.000000000000000222, 0.9999999999999997780, 1.000000000000000222, 1.000000000000000222, 0.9999999999999997780, 1.000000000000000222, 1.000000000000000000, 1.000000000000000000, 1.000000000000000222, 0.9999999999999997780, 1.000000000000000444, 0.9999999999999997780, 0.9999999999999997780, 1.000000000000000222, 0.9999999999999997780, 1.000000000000000000, 1.000000000000000000, 0.9999999999999997780, 1.000000000000000222, 0.9999999999999996669, 1.000000000000000444, 0.9999999999999997780, 1.000000000000000222, 1.000000000000000222, 0.9999999999999997780, 1.000000000000000222, 0.9999999999999997780, 1.000000000000000000, 0.9999999999999997780, 1.000000000000000444, 0.9999999999999996669, 1.000000000000000222, 0.9999999999999996669, 1.000000000000000444, 1.000000000000000000, 0.9999999999999997780, 1.000000000000000222, 0.9999999999999996669, 1.000000000000000222, 1.000000000000000222, 0.9999999999999996669, 1.000000000000000444, 1.000000000000000222, 0.9999999999999997780, 1.000000000000000222, 0.9999999999999997780, 1.000000000000000222, 1.000000000000000000, 1.000000000000000222, 0.9999999999999996669, 1.000000000000000444, 1.000000000000000000, 1.000000000000000000, 1.000000000000000222, 0.9999999999999997780, 0.9999999999999997780, 1.000000000000000444, 1.000000000000000000, 1.000000000000000000, 0.9999999999999996669, 1.000000000000000000, 1.000000000000000222, 1.000000000000000000, 1.000000000000000000, 1.000000000000000222, 0.9999999999999997780, 1.000000000000000000, 0.9999999999999997780, 0.9999999999999997780, 1.000000000000000222, 0.9999999999999997780, 1.000000000000000000, 1.000000000000000000, 0.9999999999999997780, 1.000000000000000222, 1.000000000000000000, 1.000000000000000222, 1.000000000000000000, 1.000000000000000444, 1.000000000000000000, 1.000000000000000000, 0.9999999999999997780, 0.9999999999999997780, 1.000000000000000222, 1.000000000000000000, 1.000000000000000000, 1.000000000000000000, 0.9999999999999997780, 1.000000000000000222, 1.000000000000000000, 1.000000000000000000),
 ( 0.3333333333333333703, 0.3333333333333333703, 0.3333333333333333703, 0.3333333333333333148, 0.3333333333333334259, 0.3333333333333334814, 0.3333333333333332593, 0.3333333333333332593, 0.3333333333333334814, 0.3333333333333333703, 0.3333333333333333703, 0.3333333333333334259, 0.3333333333333334259, 0.3333333333333334259, 0.3333333333333332593, 0.3333333333333334259, 0.3333333333333334259, 0.3333333333333333703, 0.3333333333333334259, 0.3333333333333332038, 0.3333333333333334259, 0.3333333333333333148, 0.3333333333333334259, 0.3333333333333333703, 0.3333333333333333703, 0.3333333333333334259, 0.3333333333333333148, 0.3333333333333334259, 0.3333333333333333703, 0.3333333333333333703, 0.3333333333333333148, 0.3333333333333334259, 0.3333333333333333703, 0.3333333333333333703, 0.3333333333333333148, 0.3333333333333333148, 0.3333333333333334259, 0.3333333333333333148, 0.3333333333333334259, 0.3333333333333333703, 0.3333333333333333703, 0.3333333333333333703, 0.3333333333333332593, 0.3333333333333334814, 0.3333333333333332593, 0.3333333333333333703, 0.3333333333333333703, 0.3333333333333333703, 0.3333333333333335369, 0.3333333333333332593, 0.3333333333333333703, 0.3333333333333335369, 0.3333333333333333703, 0.3333333333333333703, 0.3333333333333335369, 0.3333333333333333703, 0.3333333333333334259, 0.3333333333333334259, 0.3333333333333333703, 0.3333333333333333703, 0.3333333333333333703, 0.3333333333333333703, 0.3333333333333333703, 0.3333333333333333148, 0.3333333333333334259, 0.3333333333333334814, 0.3333333333333333148, 0.3333333333333333703, 0.3333333333333333148, 0.3333333333333334259, 0.3333333333333332593, 0.3333333333333334259, 0.3333333333333333703, 0.3333333333333334259, 0.3333333333333333703, 0.3333333333333333703, 0.3333333333333333703, 0.3333333333333333148, 0.3333333333333334814, 0.3333333333333332038, 0.3333333333333334259, 0.3333333333333334259, 0.3333333333333333148, 0.3333333333333334259, 0.3333333333333333703, 0.3333333333333333148, 0.3333333333333333703, 0.3333333333333333148, 0.3333333333333334814, 0.3333333333333333148, 0.3333333333333333148, 0.3333333333333334259, 0.3333333333333333148, 0.3333333333333333148, 0.3333333333333334814, 0.3333333333333333148, 0.3333333333333334259, 0.3333333333333333703, 0.3333333333333333148, 0.3333333333333333703, 0.3333333333333334259, 0.3333333333333333148, 0.3333333333333334259, 0.3333333333333333148, 0.3333333333333333703, 0.3333333333333333148, 0.3333333333333333703, 0.3333333333333333703, 0.3333333333333333148, 0.3333333333333334259, 0.3333333333333334259, 0.3333333333333333148, 0.3333333333333333703, 0.3333333333333333703, 0.3333333333333334259, 0.3333333333333333703, 0.3333333333333333703, 0.3333333333333334259, 0.3333333333333333703, 0.3333333333333334259, 0.3333333333333333148, 0.3333333333333333703, 0.3333333333333333148, 0.3333333333333335369, 0.3333333333333333148, 0.3333333333333335369, 0.3333333333333333703, 0.3333333333333332593, 0.3333333333333334259, 0.3333333333333334259, 0.3333333333333333148, 0.3333333333333333703, 0.3333333333333333148, 0.3333333333333335369, 0.3333333333333333148, 0.3333333333333333703, 0.3333333333333333703, 0.3333333333333334259, 0.3333333333333334259, 0.3333333333333333703, 0.3333333333333334259, 0.3333333333333332593, 0.3333333333333334814, 0.3333333333333333148, 0.3333333333333333703, 0.3333333333333333148, 0.3333333333333333148, 0.3333333333333334259, 0.3333333333333332593, 0.3333333333333333148, 0.3333333333333333703, 0.3333333333333333148, 0.3333333333333333703, 0.3333333333333334259, 0.3333333333333333703, 0.3333333333333334259, 0.3333333333333333148, 0.3333333333333333703, 0.3333333333333333703, 0.3333333333333333703, 0.3333333333333333148, 0.3333333333333335369, 0.3333333333333333148, 0.3333333333333333703, 0.3333333333333333148, 0.3333333333333334259, 0.3333333333333334259, 0.3333333333333333703, 0.3333333333333334259, 0.3333333333333333703, 0.3333333333333333703, 0.3333333333333334259, 0.3333333333333333703, 0.3333333333333333703, 0.3333333333333333703, 0.3333333333333334259, 0.3333333333333333148, 0.3333333333333333148, 0.3333333333333335369, 0.3333333333333333148, 0.3333333333333334259, 0.3333333333333333148, 0.3333333333333334259, 0.3333333333333333703, 0.3333333333333333148, 0.3333333333333333148, 0.3333333333333333703, 0.3333333333333333148, 0.3333333333333334259, 0.3333333333333334259, 0.3333333333333332038, 0.3333333333333335369, 0.3333333333333333703, 0.3333333333333334259, 0.3333333333333334259, 0.3333333333333333703, 0.3333333333333334259, 0.3333333333333332593, 0.3333333333333334814, 0.3333333333333333703, 0.3333333333333334259, 0.3333333333333333148, 0.3333333333333333148, 0.3333333333333335369, 0.3333333333333332593, 0.3333333333333333703, 0.3333333333333332593, 0.3333333333333335369, 0.3333333333333333703, 0.3333333333333333703, 0.3333333333333333703, 0.3333333333333334259, 0.3333333333333332593, 0.3333333333333334814, 0.3333333333333332593, 0.3333333333333333703, 0.3333333333333333703, 0.3333333333333333703, 0.3333333333333334259, 0.3333333333333333148, 0.3333333333333334259, 0.3333333333333334259, 0.3333333333333333703, 0.3333333333333333148, 0.3333333333333334259, 0.3333333333333333148, 0.3333333333333333703, 0.3333333333333333148, 0.3333333333333333703, 0.3333333333333333703, 0.3333333333333333148, 0.3333333333333333703, 0.3333333333333333703, 0.3333333333333333703, 0.3333333333333334259, 0.3333333333333333703, 0.3333333333333333703, 0.3333333333333334814, 0.3333333333333332593, 0.3333333333333333703, 0.3333333333333334259, 0.3333333333333333148, 0.3333333333333334259, 0.3333333333333333703, 0.3333333333333334814, 0.3333333333333333703, 0.3333333333333333148, 0.3333333333333334259, 0.3333333333333333703, 0.3333333333333333703, 0.3333333333333333703, 0.3333333333333334259, 0.3333333333333333148, 0.3333333333333334259, 0.3333333333333333148, 0.3333333333333333148, 0.3333333333333335369, 0.3333333333333332038, 0.3333333333333335369, 0.3333333333333333148, 0.3333333333333333703, 0.3333333333333334259, 0.3333333333333333703, 0.3333333333333333148, 0.3333333333333333703, 0.3333333333333334259, 0.3333333333333333703, 0.3333333333333334259, 0.3333333333333333148, 0.3333333333333333703, 0.3333333333333334259, 0.3333333333333333148, 0.3333333333333333703, 0.3333333333333333703, 0.3333333333333333148, 0.3333333333333334259, 0.3333333333333334259, 0.3333333333333333703, 0.3333333333333335369, 0.3333333333333333148, 0.3333333333333333703, 0.3333333333333333703, 0.3333333333333333148, 0.3333333333333333703, 0.3333333333333333703, 0.3333333333333333703, 0.3333333333333333148, 0.3333333333333333703, 0.3333333333333334814, 0.3333333333333333703, 0.3333333333333333703, 0.3333333333333335369, 0.3333333333333333703, 0.3333333333333333703, 0.3333333333333334259, 0.3333333333333334259, 0.3333333333333333703, 0.3333333333333333703, 0.3333333333333333703, 0.3333333333333333703, 0.3333333333333333148, 0.3333333333333334259, 0.3333333333333333703, 0.3333333333333333703, 0.3333333333333333703, 0.3333333333333333148, 0.3333333333333334814, 0.3333333333333333148, 0.3333333333333333148, 0.3333333333333334814, 0.3333333333333333148, 0.3333333333333333148, 0.3333333333333334259, 0.3333333333333333148, 0.3333333333333334259, 0.3333333333333333148, 0.3333333333333334259, 0.3333333333333332593, 0.3333333333333335369, 0.3333333333333333148, 0.3333333333333333148, 0.3333333333333334259, 0.3333333333333333703, 0.3333333333333333703, 0.3333333333333333148, 0.3333333333333334259, 0.3333333333333333148, 0.3333333333333334259, 0.3333333333333333148, 0.3333333333333334259, 0.3333333333333334259, 0.3333333333333333703, 0.3333333333333334259, 0.3333333333333333703, 0.3333333333333333703, 0.3333333333333334259, 0.3333333333333333148, 0.3333333333333335369, 0.3333333333333334259, 0.3333333333333333148, 0.3333333333333333703, 0.3333333333333333148, 0.3333333333333334814, 0.3333333333333333703, 0.3333333333333333703, 0.3333333333333332593, 0.3333333333333334814, 0.3333333333333333703, 0.3333333333333333148, 0.3333333333333334259, 0.3333333333333332593, 0.3333333333333334814, 0.3333333333333333703, 0.3333333333333334259, 0.3333333333333333703, 0.3333333333333333148, 0.3333333333333333703, 0.3333333333333334259, 0.3333333333333333703, 0.3333333333333334259, 0.3333333333333333703, 0.3333333333333333703, 0.3333333333333333148, 0.3333333333333333148, 0.3333333333333333703, 0.3333333333333333703, 0.3333333333333333703, 0.3333333333333333703, 0.3333333333333333703, 0.3333333333333333148, 0.3333333333333334814, 0.3333333333333333148, 0.3333333333333334814, 0.3333333333333333703, 0.3333333333333334259, 0.3333333333333334259, 0.3333333333333333703, 0.3333333333333332593, 0.3333333333333333703, 0.3333333333333333703, 0.3333333333333333703, 0.3333333333333333148, 0.3333333333333333703, 0.3333333333333332593, 0.3333333333333334259, 0.3333333333333333703, 0.3333333333333333703),
 ( 0.3333333333333333703, 0.3333333333333333703, 0.3333333333333333703, 0.3333333333333333148, 0.3333333333333334259, 0.3333333333333334814, 0.3333333333333332593, 0.3333333333333332593, 0.3333333333333334814, 0.3333333333333333703, 0.3333333333333333703, 0.3333333333333334259, 0.3333333333333334259, 0.3333333333333334259, 0.3333333333333332593, 0.3333333333333334259, 0.3333333333333334259, 0.3333333333333333703, 0.3333333333333334259, 0.3333333333333332038, 0.3333333333333334259, 0.3333333333333333148, 0.3333333333333334259, 0.3333333333333333703, 0.3333333333333333703, 0.3333333333333334259, 0.3333333333333333148, 0.3333333333333334259, 0.3333333333333333703, 0.3333333333333333703, 0.3333333333333333148, 0.3333333333333334259, 0.3333333333333333703, 0.3333333333333333703, 0.3333333333333333148, 0.3333333333333333148, 0.3333333333333334259, 0.3333333333333333148, 0.3333333333333334259, 0.3333333333333333703, 0.3333333333333333703, 0.3333333333333333703, 0.3333333333333332593, 0.3333333333333334814, 0.3333333333333332593, 0.3333333333333333703, 0.3333333333333333703, 0.3333333333333333703, 0.3333333333333335369, 0.3333333333333332593, 0.3333333333333333703, 0.3333333333333335369, 0.3333333333333333703, 0.3333333333333333703, 0.3333333333333335369, 0.3333333333333333703, 0.3333333333333334259, 0.3333333333333334259, 0.3333333333333333703, 0.3333333333333333703, 0.3333333333333333703, 0.3333333333333333703, 0.3333333333333333703, 0.3333333333333333148, 0.3333333333333334259, 0.3333333333333334814, 0.3333333333333333148, 0.3333333333333333703, 0.3333333333333333148, 0.3333333333333334259, 0.3333333333333332593, 0.3333333333333334259, 0.3333333333333333703, 0.3333333333333334259, 0.3333333333333333703, 0.3333333333333333703, 0.3333333333333333703, 0.3333333333333333148, 0.3333333333333334814, 0.3333333333333332038, 0.3333333333333334259, 0.3333333333333334259, 0.3333333333333333148, 0.3333333333333334259, 0.3333333333333333703, 0.3333333333333333148, 0.3333333333333333703, 0.3333333333333333148, 0.3333333333333334814, 0.3333333333333333148, 0.3333333333333333148, 0.3333333333333334259, 0.3333333333333333148, 0.3333333333333333148, 0.3333333333333334814, 0.3333333333333333148, 0.3333333333333334259, 0.3333333333333333703, 0.3333333333333333148, 0.3333333333333333703, 0.3333333333333334259, 0.3333333333333333148, 0.3333333333333334259, 0.3333333333333333148, 0.3333333333333333703, 0.3333333333333333148, 0.3333333333333333703, 0.3333333333333333703, 0.3333333333333333148, 0.3333333333333334259, 0.3333333333333334259, 0.3333333333333333148, 0.3333333333333333703, 0.3333333333333333703, 0.3333333333333334259, 0.3333333333333333703, 0.3333333333333333703, 0.3333333333333334259, 0.3333333333333333703, 0.3333333333333334259, 0.3333333333333333148, 0.3333333333333333703, 0.3333333333333333148, 0.3333333333333335369, 0.3333333333333333148, 0.3333333333333335369, 0.3333333333333333703, 0.3333333333333332593, 0.3333333333333334259, 0.3333333333333334259, 0.3333333333333333148, 0.3333333333333333703, 0.3333333333333333148, 0.3333333333333335369, 0.3333333333333333148, 0.3333333333333333703, 0.3333333333333333703, 0.3333333333333334259, 0.3333333333333334259, 0.3333333333333333703, 0.3333333333333334259, 0.3333333333333332593, 0.3333333333333334814, 0.3333333333333333148, 0.3333333333333333703, 0.3333333333333333148, 0.3333333333333333148, 0.3333333333333334259, 0.3333333333333332593, 0.3333333333333333148, 0.3333333333333333703, 0.3333333333333333148, 0.3333333333333333703, 0.3333333333333334259, 0.3333333333333333703, 0.3333333333333334259, 0.3333333333333333148, 0.3333333333333333703, 0.3333333333333333703, 0.3333333333333333703, 0.3333333333333333148, 0.3333333333333335369, 0.3333333333333333148, 0.3333333333333333703, 0.3333333333333333148, 0.3333333333333334259, 0.3333333333333334259, 0.3333333333333333703, 0.3333333333333334259, 0.3333333333333333703, 0.3333333333333333703, 0.3333333333333334259, 0.3333333333333333703, 0.3333333333333333703, 0.3333333333333333703, 0.3333333333333334259, 0.3333333333333333148, 0.3333333333333333148, 0.3333333333333335369, 0.3333333333333333148, 0.3333333333333334259, 0.3333333333333333148, 0.3333333333333334259, 0.3333333333333333703, 0.3333333333333333148, 0.3333333333333333148, 0.3333333333333333703, 0.3333333333333333148, 0.3333333333333334259, 0.3333333333333334259, 0.3333333333333332038, 0.3333333333333335369, 0.3333333333333333703, 0.3333333333333334259, 0.3333333333333334259, 0.3333333333333333703, 0.3333333333333334259, 0.3333333333333332593, 0.3333333333333334814, 0.3333333333333333703, 0.3333333333333334259, 0.3333333333333333148, 0.3333333333333333148, 0.3333333333333335369, 0.3333333333333332593, 0.3333333333333333703, 0.3333333333333332593, 0.3333333333333335369, 0.3333333333333333703, 0.3333333333333333703, 0.3333333333333333703, 0.3333333333333334259, 0.3333333333333332593, 0.3333333333333334814, 0.3333333333333332593, 0.3333333333333333703, 0.3333333333333333703, 0.3333333333333333703, 0.3333333333333334259, 0.3333333333333333148, 0.3333333333333334259, 0.3333333333333334259, 0.3333333333333333703, 0.3333333333333333148, 0.3333333333333334259, 0.3333333333333333148, 0.3333333333333333703, 0.3333333333333333148, 0.3333333333333333703, 0.3333333333333333703, 0.3333333333333333148, 0.3333333333333333703, 0.3333333333333333703, 0.3333333333333333703, 0.3333333333333334259, 0.3333333333333333703, 0.3333333333333333703, 0.3333333333333334814, 0.3333333333333332593, 0.3333333333333333703, 0.3333333333333334259, 0.3333333333333333148, 0.3333333333333334259, 0.3333333333333333703, 0.3333333333333334814, 0.3333333333333333703, 0.3333333333333333148, 0.3333333333333334259, 0.3333333333333333703, 0.3333333333333333703, 0.3333333333333333703, 0.3333333333333334259, 0.3333333333333333148, 0.3333333333333334259, 0.3333333333333333148, 0.3333333333333333148, 0.3333333333333335369, 0.3333333333333332038, 0.3333333333333335369, 0.3333333333333333148, 0.3333333333333333703, 0.3333333333333334259, 0.3333333333333333703, 0.3333333333333333148, 0.3333333333333333703, 0.3333333333333334259, 0.3333333333333333703, 0.3333333333333334259, 0.3333333333333333148, 0.3333333333333333703, 0.3333333333333334259, 0.3333333333333333148, 0.3333333333333333703, 0.3333333333333333703, 0.3333333333333333148, 0.3333333333333334259, 0.3333333333333334259, 0.3333333333333333703, 0.3333333333333335369, 0.3333333333333333148, 0.3333333333333333703, 0.3333333333333333703, 0.3333333333333333148, 0.3333333333333333703, 0.3333333333333333703, 0.3333333333333333703, 0.3333333333333333148, 0.3333333333333333703, 0.3333333333333334814, 0.3333333333333333703, 0.3333333333333333703, 0.3333333333333335369, 0.3333333333333333703, 0.3333333333333333703, 0.3333333333333334259, 0.3333333333333334259, 0.3333333333333333703, 0.3333333333333333703, 0.3333333333333333703, 0.3333333333333333703, 0.3333333333333333148, 0.3333333333333334259, 0.3333333333333333703, 0.3333333333333333703, 0.3333333333333333703, 0.3333333333333333148, 0.3333333333333334814, 0.3333333333333333148, 0.3333333333333333148, 0.3333333333333334814, 0.3333333333333333148, 0.3333333333333333148, 0.3333333333333334259, 0.3333333333333333148, 0.3333333333333334259, 0.3333333333333333148, 0.3333333333333334259, 0.3333333333333332593, 0.3333333333333335369, 0.3333333333333333148, 0.3333333333333333148, 0.3333333333333334259, 0.3333333333333333703, 0.3333333333333333703, 0.3333333333333333148, 0.3333333333333334259, 0.3333333333333333148, 0.3333333333333334259, 0.3333333333333333148, 0.3333333333333334259, 0.3333333333333334259, 0.3333333333333333703, 0.3333333333333334259, 0.3333333333333333703, 0.3333333333333333703, 0.3333333333333334259, 0.3333333333333333148, 0.3333333333333335369, 0.3333333333333334259, 0.3333333333333333148, 0.3333333333333333703, 0.3333333333333333148, 0.3333333333333334814, 0.3333333333333333703, 0.3333333333333333703, 0.3333333333333332593, 0.3333333333333334814, 0.3333333333333333703, 0.3333333333333333148, 0.3333333333333334259, 0.3333333333333332593, 0.3333333333333334814, 0.3333333333333333703, 0.3333333333333334259, 0.3333333333333333703, 0.3333333333333333148, 0.3333333333333333703, 0.3333333333333334259, 0.3333333333333333703, 0.3333333333333334259, 0.3333333333333333703, 0.3333333333333333703, 0.3333333333333333148, 0.3333333333333333148, 0.3333333333333333703, 0.3333333333333333703, 0.3333333333333333703, 0.3333333333333333703, 0.3333333333333333703, 0.3333333333333333148, 0.3333333333333334814, 0.3333333333333333148, 0.3333333333333334814, 0.3333333333333333703, 0.3333333333333334259, 0.3333333333333334259, 0.3333333333333333703, 0.3333333333333332593, 0.3333333333333333703, 0.3333333333333333703, 0.3333333333333333703, 0.3333333333333333148, 0.3333333333333333703, 0.3333333333333332593, 0.3333333333333334259, 0.3333333333333333703, 0.3333333333333333703),
 ( 1.000000000000000000, 1.000000000000000000, 1.000000000000000000, 0.9999999999999997780, 1.000000000000000000, 1.000000000000000444, 0.9999999999999996669, 0.9999999999999996669, 1.000000000000000444, 1.000000000000000000, 1.000000000000000000, 1.000000000000000000, 1.000000000000000222, 1.000000000000000222, 0.9999999999999997780, 1.000000000000000000, 1.000000000000000222, 1.000000000000000000, 1.000000000000000222, 0.9999999999999994449, 1.000000000000000222, 0.9999999999999997780, 1.000000000000000444, 1.000000000000000000, 1.000000000000000000, 1.000000000000000222, 0.9999999999999997780, 1.000000000000000222, 1.000000000000000000, 1.000000000000000222, 0.9999999999999997780, 1.000000000000000000, 1.000000000000000000, 0.9999999999999997780, 1.000000000000000000, 1.000000000000000000, 1.000000000000000222, 1.000000000000000000, 0.9999999999999997780, 1.000000000000000222, 0.9999999999999997780, 1.000000000000000000, 0.9999999999999997780, 1.000000000000000444, 0.9999999999999996669, 1.000000000000000222, 1.000000000000000000, 1.000000000000000000, 1.000000000000000444, 0.9999999999999996669, 1.000000000000000222, 1.000000000000000444, 1.000000000000000000, 0.9999999999999997780, 1.000000000000000444, 1.000000000000000222, 1.000000000000000000, 1.000000000000000000, 1.000000000000000222, 1.000000000000000000, 1.000000000000000222, 0.9999999999999997780, 1.000000000000000222, 1.000000000000000000, 1.000000000000000000, 1.000000000000000444, 0.9999999999999996669, 1.000000000000000000, 0.9999999999999997780, 1.000000000000000222, 0.9999999999999996669, 1.000000000000000000, 1.000000000000000222, 0.9999999999999997780, 1.000000000000000444, 0.9999999999999997780, 1.000000000000000000, 0.9999999999999997780, 1.000000000000000222, 0.9999999999999996669, 1.000000000000000000, 1.000000000000000222, 0.9999999999999996669, 1.000000000000000444, 0.9999999999999997780, 1.000000000000000000, 1.000000000000000222, 0.9999999999999996669, 1.000000000000000222, 1.000000000000000000, 0.9999999999999997780, 1.000000000000000222, 0.9999999999999997780, 1.000000000000000000, 1.000000000000000222, 0.9999999999999997780, 1.000000000000000000, 1.000000000000000000, 0.9999999999999997780, 1.000000000000000000, 1.000000000000000222, 0.9999999999999997780, 1.000000000000000000, 1.000000000000000000, 1.000000000000000000, 0.9999999999999997780, 1.000000000000000222, 0.9999999999999997780, 0.9999999999999997780, 1.000000000000000444, 1.000000000000000000, 1.000000000000000000, 0.9999999999999997780, 1.000000000000000222, 1.000000000000000000, 1.000000000000000000, 1.000000000000000000, 1.000000000000000000, 1.000000000000000222, 1.000000000000000222, 0.9999999999999997780, 1.000000000000000000, 0.9999999999999997780, 1.000000000000000444, 0.9999999999999996669, 1.000000000000000666, 1.000000000000000000, 0.9999999999999997780, 1.000000000000000222, 1.000000000000000000, 1.000000000000000000, 1.000000000000000000, 0.9999999999999994449, 1.000000000000000666, 0.9999999999999996669, 1.000000000000000000, 1.000000000000000222, 0.9999999999999997780, 1.000000000000000222, 0.9999999999999997780, 1.000000000000000222, 0.9999999999999996669, 1.000000000000000444, 1.000000000000000000, 1.000000000000000222, 0.9999999999999996669, 1.000000000000000000, 1.000000000000000222, 0.9999999999999997780, 1.000000000000000000, 0.9999999999999997780, 1.000000000000000000, 1.000000000000000000, 1.000000000000000222, 0.9999999999999997780, 1.000000000000000222, 0.9999999999999997780, 1.000000000000000000, 1.000000000000000000, 1.000000000000000222, 0.9999999999999997780, 1.000000000000000444, 1.000000000000000000, 0.9999999999999997780, 1.000000000000000000, 1.000000000000000000, 1.000000000000000222, 0.9999999999999997780, 1.000000000000000222, 1.000000000000000000, 1.000000000000000000, 1.000000000000000000, 1.000000000000000222, 1.000000000000000000, 0.9999999999999997780, 1.000000000000000000, 1.000000000000000000, 1.000000000000000000, 1.000000000000000444, 0.9999999999999996669, 1.000000000000000222, 1.000000000000000000, 1.000000000000000222, 0.9999999999999997780, 1.000000000000000000, 0.9999999999999997780, 1.000000000000000000, 0.9999999999999997780, 1.000000000000000000, 1.000000000000000444, 0.9999999999999994449, 1.000000000000000444, 1.000000000000000000, 1.000000000000000222, 1.000000000000000222, 0.9999999999999997780, 1.000000000000000222, 0.9999999999999997780, 1.000000000000000222, 1.000000000000000222, 1.000000000000000222, 0.9999999999999997780, 1.000000000000000000, 1.000000000000000444, 0.9999999999999996669, 1.000000000000000000, 0.9999999999999997780, 1.000000000000000222, 1.000000000000000222, 1.000000000000000000, 0.9999999999999997780, 1.000000000000000222, 0.9999999999999997780, 1.000000000000000222, 0.9999999999999997780, 0.9999999999999997780, 1.000000000000000000, 1.000000000000000000, 1.000000000000000000, 1.000000000000000000, 1.000000000000000000, 1.000000000000000222, 1.000000000000000000, 1.000000000000000000, 1.000000000000000222, 1.000000000000000000, 0.9999999999999997780, 1.000000000000000000, 1.000000000000000000, 1.000000000000000000, 0.9999999999999997780, 1.000000000000000000, 0.9999999999999997780, 1.000000000000000000, 1.000000000000000222, 0.9999999999999996669, 1.000000000000000444, 1.000000000000000000, 0.9999999999999997780, 1.000000000000000222, 1.000000000000000000, 0.9999999999999997780, 1.000000000000000222, 1.000000000000000000, 1.000000000000000222, 1.000000000000000000, 0.9999999999999997780, 1.000000000000000222, 1.000000000000000000, 1.000000000000000000, 1.000000000000000222, 1.000000000000000000, 1.000000000000000000, 1.000000000000000222, 0.9999999999999997780, 0.9999999999999996669, 1.000000000000000444, 0.9999999999999994449, 1.000000000000000444, 0.9999999999999997780, 1.000000000000000222, 1.000000000000000000, 1.000000000000000000, 1.000000000000000000, 1.000000000000000000, 1.000000000000000444, 0.9999999999999996669, 1.000000000000000444, 1.000000000000000000, 0.9999999999999997780, 1.000000000000000444, 0.9999999999999994449, 1.000000000000000444, 0.9999999999999997780, 0.9999999999999997780, 1.000000000000000222, 1.000000000000000444, 0.9999999999999997780, 1.000000000000000444, 0.9999999999999997780, 1.000000000000000000, 1.000000000000000444, 0.9999999999999997780, 0.9999999999999997780, 1.000000000000000000, 1.000000000000000000, 1.000000000000000000, 0.9999999999999997780, 1.000000000000000444, 1.000000000000000222, 0.9999999999999997780, 1.000000000000000444, 1.000000000000000000, 1.000000000000000222, 1.000000000000000000, 1.000000000000000000, 1.000000000000000222, 0.9999999999999997780, 1.000000000000000222, 1.000000000000000222, 0.9999999999999997780, 1.000000000000000222, 1.000000000000000000, 1.000000000000000000, 1.000000000000000222, 0.9999999999999997780, 1.000000000000000444, 0.9999999999999997780, 0.9999999999999997780, 1.000000000000000222, 0.9999999999999997780, 1.000000000000000000, 1.000000000000000000, 0.9999999999999997780, 1.000000000000000222, 0.9999999999999996669, 1.000000000000000444, 0.9999999999999997780, 1.000000000000000222, 1.000000000000000222, 0.9999999999999997780, 1.000000000000000222, 0.9999999999999997780, 1.000000000000000000, 0.9999999999999997780, 1.000000000000000444, 0.9999999999999996669, 1.000000000000000222, 0.9999999999999996669, 1.000000000000000444, 1.000000000000000000, 0.9999999999999997780, 1.000000000000000222, 0.9999999999999996669, 1.000000000000000222, 1.000000000000000222, 0.9999999999999996669, 1.000000000000000444, 1.000000000000000222, 0.9999999999999997780, 1.000000000000000222, 0.9999999999999997780, 1.000000000000000222, 1.000000000000000000, 1.000000000000000222, 0.9999999999999996669, 1.000000000000000444, 1.000000000000000000, 1.000000000000000000, 1.000000000000000222, 0.9999999999999997780, 0.9999999999999997780, 1.000000000000000444, 1.000000000000000000, 1.000000000000000000, 0.9999999999999996669, 1.000000000000000000, 1.000000000000000222, 1.000000000000000000, 1.000000000000000000, 1.000000000000000222, 0.9999999999999997780, 1.000000000000000000, 0.9999999999999997780, 0.9999999999999997780, 1.000000000000000222, 0.9999999999999997780, 1.000000000000000000, 1.000000000000000000, 0.9999999999999997780, 1.000000000000000222, 1.000000000000000000, 1.000000000000000222, 1.000000000000000000, 1.000000000000000444, 1.000000000000000000, 1.000000000000000000, 0.9999999999999997780, 0.9999999999999997780, 1.000000000000000222, 1.000000000000000000, 1.000000000000000000, 1.000000000000000000, 0.9999999999999997780, 1.000000000000000222, 1.000000000000000000, 1.000000000000000000),
 ( 0.3333333333333333703, 0.3333333333333333703, 0.3333333333333333703, 0.3333333333333333148, 0.3333333333333334259, 0.3333333333333334814, 0.3333333333333332593, 0.3333333333333332593, 0.3333333333333334814, 0.3333333333333333703, 0.3333333333333333703, 0.3333333333333334259, 0.3333333333333334259, 0.3333333333333334259, 0.3333333333333332593, 0.3333333333333334259, 0.3333333333333334259, 0.3333333333333333703, 0.3333333333333334259, 0.3333333333333332038, 0.3333333333333334259, 0.3333333333333333148, 0.3333333333333334259, 0.3333333333333333703, 0.3333333333333333703, 0.3333333333333334259, 0.3333333333333333148, 0.3333333333333334259, 0.3333333333333333703, 0.3333333333333333703, 0.3333333333333333148, 0.3333333333333334259, 0.3333333333333333703, 0.3333333333333333703, 0.3333333333333333148, 0.3333333333333333148, 0.3333333333333334259, 0.3333333333333333148, 0.3333333333333334259, 0.3333333333333333703, 0.3333333333333333703, 0.3333333333333333703, 0.3333333333333332593, 0.3333333333333334814, 0.3333333333333332593, 0.3333333333333333703, 0.3333333333333333703, 0.3333333333333333703, 0.3333333333333335369, 0.3333333333333332593, 0.3333333333333333703, 0.3333333333333335369, 0.3333333333333333703, 0.3333333333333333703, 0.3333333333333335369, 0.3333333333333333703, 0.3333333333333334259, 0.3333333333333334259, 0.3333333333333333703, 0.3333333333333333703, 0.3333333333333333703, 0.3333333333333333703, 0.3333333333333333703, 0.3333333333333333148, 0.3333333333333334259, 0.3333333333333334814, 0.3333333333333333148, 0.3333333333333333703, 0.3333333333333333148, 0.3333333333333334259, 0.3333333333333332593, 0.3333333333333334259, 0.3333333333333333703, 0.3333333333333334259, 0.3333333333333333703, 0.3333333333333333703, 0.3333333333333333703, 0.3333333333333333148, 0.3333333333333334814, 0.3333333333333332038, 0.3333333333333334259, 0.3333333333333334259, 0.3333333333333333148, 0.3333333333333334259, 0.3333333333333333703, 0.3333333333333333148, 0.3333333333333333703, 0.3333333333333333148, 0.3333333333333334814, 0.3333333333333333148, 0.3333333333333333148, 0.3333333333333334259, 0.3333333333333333148, 0.3333333333333333148, 0.3333333333333334814, 0.3333333333333333148, 0.3333333333333334259, 0.3333333333333333703, 0.3333333333333333148, 0.3333333333333333703, 0.3333333333333334259, 0.3333333333333333148, 0.3333333333333334259, 0.3333333333333333148, 0.3333333333333333703, 0.3333333333333333148, 0.3333333333333333703, 0.3333333333333333703, 0.3333333333333333148, 0.3333333333333334259, 0.3333333333333334259, 0.3333333333333333148, 0.3333333333333333703, 0.3333333333333333703, 0.3333333333333334259, 0.3333333333333333703, 0.3333333333333333703, 0.3333333333333334259, 0.3333333333333333703, 0.3333333333333334259, 0.3333333333333333148, 0.3333333333333333703, 0.3333333333333333148, 0.3333333333333335369, 0.3333333333333333148, 0.3333333333333335369, 0.3333333333333333703, 0.3333333333333332593, 0.3333333333333334259, 0.3333333333333334259, 0.3333333333333333148, 0.3333333333333333703, 0.3333333333333333148, 0.3333333333333335369, 0.3333333333333333148, 0.3333333333333333703, 0.3333333333333333703, 0.3333333333333334259, 0.3333333333333334259, 0.3333333333333333703, 0.3333333333333334259, 0.3333333333333332593, 0.3333333333333334814, 0.3333333333333333148, 0.3333333333333333703, 0.3333333333333333148, 0.3333333333333333148, 0.3333333333333334259, 0.3333333333333332593, 0.3333333333333333148, 0.3333333333333333703, 0.3333333333333333148, 0.3333333333333333703, 0.3333333333333334259, 0.3333333333333333703, 0.3333333333333334259, 0.3333333333333333148, 0.3333333333333333703, 0.3333333333333333703, 0.3333333333333333703, 0.3333333333333333148, 0.3333333333333335369, 0.3333333333333333148, 0.3333333333333333703, 0.3333333333333333148, 0.3333333333333334259, 0.3333333333333334259, 0.3333333333333333703, 0.3333333333333334259, 0.3333333333333333703, 0.3333333333333333703, 0.3333333333333334259, 0.3333333333333333703, 0.3333333333333333703, 0.3333333333333333703, 0.3333333333333334259, 0.3333333333333333148, 0.3333333333333333148, 0.3333333333333335369, 0.3333333333333333148, 0.3333333333333334259, 0.3333333333333333148, 0.3333333333333334259, 0.3333333333333333703, 0.3333333333333333148, 0.3333333333333333148, 0.3333333333333333703, 0.3333333333333333148, 0.3333333333333334259, 0.3333333333333334259, 0.3333333333333332038, 0.3333333333333335369, 0.3333333333333333703, 0.3333333333333334259, 0.3333333333333334259, 0.3333333333333333703, 0.3333333333333334259, 0.3333333333333332593, 0.3333333333333334814, 0.3333333333333333703, 0.3333333333333334259, 0.3333333333333333148, 0.3333333333333333148, 0.3333333333333335369, 0.3333333333333332593, 0.3333333333333333703, 0.3333333333333332593, 0.3333333333333335369, 0.3333333333333333703, 0.3333333333333333703, 0.3333333333333333703, 0.3333333333333334259, 0.3333333333333332593, 0.3333333333333334814, 0.3333333333333332593, 0.3333333333333333703, 0.3333333333333333703, 0.3333333333333333703, 0.3333333333333334259, 0.3333333333333333148, 0.3333333333333334259, 0.3333333333333334259, 0.3333333333333333703, 0.3333333333333333148, 0.3333333333333334259, 0.3333333333333333148, 0.3333333333333333703, 0.3333333333333333148, 0.3333333333333333703, 0.3333333333333333703, 0.3333333333333333148, 0.3333333333333333703, 0.3333333333333333703, 0.3333333333333333703, 0.3333333333333334259, 0.3333333333333333703, 0.3333333333333333703, 0.3333333333333334814, 0.3333333333333332593, 0.3333333333333333703, 0.3333333333333334259, 0.3333333333333333148, 0.3333333333333334259, 0.3333333333333333703, 0.3333333333333334814, 0.3333333333333333703, 0.3333333333333333148, 0.3333333333333334259, 0.3333333333333333703, 0.3333333333333333703, 0.3333333333333333703, 0.3333333333333334259, 0.3333333333333333148, 0.3333333333333334259, 0.3333333333333333148, 0.3333333333333333148, 0.3333333333333335369, 0.3333333333333332038, 0.3333333333333335369, 0.3333333333333333148, 0.3333333333333333703, 0.3333333333333334259, 0.3333333333333333703, 0.3333333333333333148, 0.3333333333333333703, 0.3333333333333334259, 0.3333333333333333703, 0.3333333333333334259, 0.3333333333333333148, 0.3333333333333333703, 0.3333333333333334259, 0.3333333333333333148, 0.3333333333333333703, 0.3333333333333333703, 0.3333333333333333148, 0.3333333333333334259, 0.3333333333333334259, 0.3333333333333333703, 0.3333333333333335369, 0.3333333333333333148, 0.3333333333333333703, 0.3333333333333333703, 0.3333333333333333148, 0.3333333333333333703, 0.3333333333333333703, 0.3333333333333333703, 0.3333333333333333148, 0.3333333333333333703, 0.3333333333333334814, 0.3333333333333333703, 0.3333333333333333703, 0.3333333333333335369, 0.3333333333333333703, 0.3333333333333333703, 0.3333333333333334259, 0.3333333333333334259, 0.3333333333333333703, 0.3333333333333333703, 0.3333333333333333703, 0.3333333333333333703, 0.3333333333333333148, 0.3333333333333334259, 0.3333333333333333703, 0.3333333333333333703, 0.3333333333333333703, 0.3333333333333333148, 0.3333333333333334814, 0.3333333333333333148, 0.3333333333333333148, 0.3333333333333334814, 0.3333333333333333148, 0.3333333333333333148, 0.3333333333333334259, 0.3333333333333333148, 0.3333333333333334259, 0.3333333333333333148, 0.3333333333333334259, 0.3333333333333332593, 0.3333333333333335369, 0.3333333333333333148, 0.3333333333333333148, 0.3333333333333334259, 0.3333333333333333703, 0.3333333333333333703, 0.3333333333333333148, 0.3333333333333334259, 0.3333333333333333148, 0.3333333333333334259, 0.3333333333333333148, 0.3333333333333334259, 0.3333333333333334259, 0.3333333333333333703, 0.3333333333333334259, 0.3333333333333333703, 0.3333333333333333703, 0.3333333333333334259, 0.3333333333333333148, 0.3333333333333335369, 0.3333333333333334259, 0.3333333333333333148, 0.3333333333333333703, 0.3333333333333333148, 0.3333333333333334814, 0.3333333333333333703, 0.3333333333333333703, 0.3333333333333332593, 0.3333333333333334814, 0.3333333333333333703, 0.3333333333333333148, 0.3333333333333334259, 0.3333333333333332593, 0.3333333333333334814, 0.3333333333333333703, 0.3333333333333334259, 0.3333333333333333703, 0.3333333333333333148, 0.3333333333333333703, 0.3333333333333334259, 0.3333333333333333703, 0.3333333333333334259, 0.3333333333333333703, 0.3333333333333333703, 0.3333333333333333148, 0.3333333333333333148, 0.3333333333333333703, 0.3333333333333333703, 0.3333333333333333703, 0.3333333333333333703, 0.3333333333333333703, 0.3333333333333333148, 0.3333333333333334814, 0.3333333333333333148, 0.3333333333333334814, 0.3333333333333333703, 0.3333333333333334259, 0.3333333333333334259, 0.3333333333333333703, 0.3333333333333332593, 0.3333333333333333703, 0.3333333333333333703, 0.3333333333333333703, 0.3333333333333333148, 0.3333333333333333703, 0.3333333333333332593, 0.3333333333333334259, 0.3333333333333333703, 0.3333333333333333703),
 ( 0.3333333333333333703, 0.3333333333333333703, 0.3333333333333333703, 0.3333333333333333148, 0.3333333333333334259, 0.3333333333333334814, 0.3333333333333332593, 0.3333333333333332593, 0.3333333333333334814, 0.3333333333333333703, 0.3333333333333333703, 0.3333333333333334259, 0.3333333333333334259, 0.3333333333333334259, 0.3333333333333332593, 0.3333333333333334259, 0.3333333333333334259, 0.3333333333333333703, 0.3333333333333334259, 0.3333333333333332038, 0.3333333333333334259, 0.3333333333333333148, 0.3333333333333334259, 0.3333333333333333703, 0.3333333333333333703, 0.3333333333333334259, 0.3333333333333333148, 0.3333333333333334259, 0.3333333333333333703, 0.3333333333333333703, 0.3333333333333333148, 0.3333333333333334259, 0.3333333333333333703, 0.3333333333333333703, 0.3333333333333333148, 0.3333333333333333148, 0.3333333333333334259, 0.3333333333333333148, 0.3333333333333334259, 0.3333333333333333703, 0.3333333333333333703, 0.3333333333333333703, 0.3333333333333332593, 0.3333333333333334814, 0.3333333333333332593, 0.3333333333333333703, 0.3333333333333333703, 0.3333333333333333703, 0.3333333333333335369, 0.3333333333333332593, 0.3333333333333333703, 0.3333333333333335369, 0.3333333333333333703, 0.3333333333333333703, 0.3333333333333335369, 0.3333333333333333703, 0.3333333333333334259, 0.3333333333333334259, 0.3333333333333333703, 0.3333333333333333703, 0.3333333333333333703, 0.3333333333333333703, 0.3333333333333333703, 0.3333333333333333148, 0.3333333333333334259, 0.3333333333333334814, 0.3333333333333333148, 0.3333333333333333703, 0.3333333333333333148, 0.3333333333333334259, 0.3333333333333332593, 0.3333333333333334259, 0.3333333333333333703, 0.3333333333333334259, 0.3333333333333333703, 0.3333333333333333703, 0.3333333333333333703, 0.3333333333333333148, 0.3333333333333334814, 0.3333333333333332038, 0.3333333333333334259, 0.3333333333333334259, 0.3333333333333333148, 0.3333333333333334259, 0.3333333333333333703, 0.3333333333333333148, 0.3333333333333333703, 0.3333333333333333148, 0.3333333333333334814, 0.3333333333333333148, 0.3333333333333333148, 0.3333333333333334259, 0.3333333333333333148, 0.3333333333333333148, 0.3333333333333334814, 0.3333333333333333148, 0.3333333333333334259, 0.3333333333333333703, 0.3333333333333333148, 0.3333333333333333703, 0.3333333333333334259, 0.3333333333333333148, 0.3333333333333334259, 0.3333333333333333148, 0.3333333333333333703, 0.3333333333333333148, 0.3333333333333333703, 0.3333333333333333703, 0.3333333333333333148, 0.3333333333333334259, 0.3333333333333334259, 0.3333333333333333148, 0.3333333333333333703, 0.3333333333333333703, 0.3333333333333334259, 0.3333333333333333703, 0.3333333333333333703, 0.3333333333333334259, 0.3333333333333333703, 0.3333333333333334259, 0.3333333333333333148, 0.3333333333333333703, 0.3333333333333333148, 0.3333333333333335369, 0.3333333333333333148, 0.3333333333333335369, 0.3333333333333333703, 0.3333333333333332593, 0.3333333333333334259, 0.3333333333333334259, 0.3333333333333333148, 0.3333333333333333703, 0.3333333333333333148, 0.3333333333333335369, 0.3333333333333333148, 0.3333333333333333703, 0.3333333333333333703, 0.3333333333333334259, 0.3333333333333334259, 0.3333333333333333703, 0.3333333333333334259, 0.3333333333333332593, 0.3333333333333334814, 0.3333333333333333148, 0.3333333333333333703, 0.3333333333333333148, 0.3333333333333333148, 0.3333333333333334259, 0.3333333333333332593, 0.3333333333333333148, 0.3333333333333333703, 0.3333333333333333148, 0.3333333333333333703, 0.3333333333333334259, 0.3333333333333333703, 0.3333333333333334259, 0.3333333333333333148, 0.3333333333333333703, 0.3333333333333333703, 0.3333333333333333703, 0.3333333333333333148, 0.3333333333333335369, 0.3333333333333333148, 0.3333333333333333703, 0.3333333333333333148, 0.3333333333333334259, 0.3333333333333334259, 0.3333333333333333703, 0.3333333333333334259, 0.3333333333333333703, 0.3333333333333333703, 0.3333333333333334259, 0.3333333333333333703, 0.3333333333333333703, 0.3333333333333333703, 0.3333333333333334259, 0.3333333333333333148, 0.3333333333333333148, 0.3333333333333335369, 0.3333333333333333148, 0.3333333333333334259, 0.3333333333333333148, 0.3333333333333334259, 0.3333333333333333703, 0.3333333333333333148, 0.3333333333333333148, 0.3333333333333333703, 0.3333333333333333148, 0.3333333333333334259, 0.3333333333333334259, 0.3333333333333332038, 0.3333333333333335369, 0.3333333333333333703, 0.3333333333333334259, 0.3333333333333334259, 0.3333333333333333703, 0.3333333333333334259, 0.3333333333333332593, 0.3333333333333334814, 0.3333333333333333703, 0.3333333333333334259, 0.3333333333333333148, 0.3333333333333333148, 0.3333333333333335369, 0.3333333333333332593, 0.3333333333333333703, 0.3333333333333332593, 0.3333333333333335369, 0.3333333333333333703, 0.3333333333333333703, 0.3333333333333333703, 0.3333333333333334259, 0.3333333333333332593, 0.3333333333333334814, 0.3333333333333332593, 0.3333333333333333703, 0.3333333333333333703, 0.3333333333333333703, 0.3333333333333334259, 0.3333333333333333148, 0.3333333333333334259, 0.3333333333333334259, 0.3333333333333333703, 0.3333333333333333148, 0.3333333333333334259, 0.3333333333333333148, 0.3333333333333333703, 0.3333333333333333148, 0.3333333333333333703, 0.3333333333333333703, 0.3333333333333333148, 0.3333333333333333703, 0.3333333333333333703, 0.3333333333333333703, 0.3333333333333334259, 0.3333333333333333703, 0.3333333333333333703, 0.3333333333333334814, 0.3333333333333332593, 0.3333333333333333703, 0.3333333333333334259, 0.3333333333333333148, 0.3333333333333334259, 0.3333333333333333703, 0.3333333333333334814, 0.3333333333333333703, 0.3333333333333333148, 0.3333333333333334259, 0.3333333333333333703, 0.3333333333333333703, 0.3333333333333333703, 0.3333333333333334259, 0.3333333333333333148, 0.3333333333333334259, 0.3333333333333333148, 0.3333333333333333148, 0.3333333333333335369, 0.3333333333333332038, 0.3333333333333335369, 0.3333333333333333148, 0.3333333333333333703, 0.3333333333333334259, 0.3333333333333333703, 0.3333333333333333148, 0.3333333333333333703, 0.3333333333333334259, 0.3333333333333333703, 0.3333333333333334259, 0.3333333333333333148, 0.3333333333333333703, 0.3333333333333334259, 0.3333333333333333148, 0.3333333333333333703, 0.3333333333333333703, 0.3333333333333333148, 0.3333333333333334259, 0.3333333333333334259, 0.3333333333333333703, 0.3333333333333335369, 0.3333333333333333148, 0.3333333333333333703, 0.3333333333333333703, 0.3333333333333333148, 0.3333333333333333703, 0.3333333333333333703, 0.3333333333333333703, 0.3333333333333333148, 0.3333333333333333703, 0.3333333333333334814, 0.3333333333333333703, 0.3333333333333333703, 0.3333333333333335369, 0.3333333333333333703, 0.3333333333333333703, 0.3333333333333334259, 0.3333333333333334259, 0.3333333333333333703, 0.3333333333333333703, 0.3333333333333333703, 0.3333333333333333703, 0.3333333333333333148, 0.3333333333333334259, 0.3333333333333333703, 0.3333333333333333703, 0.3333333333333333703, 0.3333333333333333148, 0.3333333333333334814, 0.3333333333333333148, 0.3333333333333333148, 0.3333333333333334814, 0.3333333333333333148, 0.3333333333333333148, 0.3333333333333334259, 0.3333333333333333148, 0.3333333333333334259, 0.3333333333333333148, 0.3333333333333334259, 0.3333333333333332593, 0.3333333333333335369, 0.3333333333333333148, 0.3333333333333333148, 0.3333333333333334259, 0.3333333333333333703, 0.3333333333333333703, 0.3333333333333333148, 0.3333333333333334259, 0.3333333333333333148, 0.3333333333333334259, 0.3333333333333333148, 0.3333333333333334259, 0.3333333333333334259, 0.3333333333333333703, 0.3333333333333334259, 0.3333333333333333703, 0.3333333333333333703, 0.3333333333333334259, 0.3333333333333333148, 0.3333333333333335369, 0.3333333333333334259, 0.3333333333333333148, 0.3333333333333333703, 0.3333333333333333148, 0.3333333333333334814, 0.3333333333333333703, 0.3333333333333333703, 0.3333333333333332593, 0.3333333333333334814, 0.3333333333333333703, 0.3333333333333333148, 0.3333333333333334259, 0.3333333333333332593, 0.3333333333333334814, 0.3333333333333333703, 0.3333333333333334259, 0.3333333333333333703, 0.3333333333333333148, 0.3333333333333333703, 0.3333333333333334259, 0.3333333333333333703, 0.3333333333333334259, 0.3333333333333333703, 0.3333333333333333703, 0.3333333333333333148, 0.3333333333333333148, 0.3333333333333333703, 0.3333333333333333703, 0.3333333333333333703, 0.3333333333333333703, 0.3333333333333333703, 0.3333333333333333148, 0.3333333333333334814, 0.3333333333333333148, 0.3333333333333334814, 0.3333333333333333703, 0.3333333333333334259, 0.3333333333333334259, 0.3333333333333333703, 0.3333333333333332593, 0.3333333333333333703, 0.3333333333333333703, 0.3333333333333333703, 0.3333333333333333148, 0.3333333333333333703, 0.3333333333333332593, 0.3333333333333334259, 0.3333333333333333703, 0.3333333333333333703),
 ( 1.000000000000000000, 1.000000000000000000, 1.000000000000000000, 0.9999999999999997780, 1.000000000000000000, 1.000000000000000444, 0.9999999999999996669, 0.9999999999999996669, 1.000000000000000444, 1.000000000000000000, 1.000000000000000000, 1.000000000000000000, 1.000000000000000222, 1.000000000000000222, 0.9999999999999997780, 1.000000000000000000, 1.000000000000000222, 1.000000000000000000, 1.000000000000000222, 0.9999999999999994449, 1.000000000000000222, 0.9999999999999997780, 1.000000000000000444, 1.000000000000000000, 1.000000000000000000, 1.000000000000000222, 0.9999999999999997780, 1.000000000000000222, 1.000000000000000000, 1.000000000000000222, 0.9999999999999997780, 1.000000000000000000, 1.000000000000000000, 0.9999999999999997780, 1.000000000000000000, 1.000000000000000000, 1.000000000000000222, 1.000000000000000000, 0.9999999999999997780, 1.000000000000000222, 0.9999999999999997780, 1.000000000000000000, 0.9999999999999997780, 1.000000000000000444, 0.9999999999999996669, 1.000000000000000222, 1.000000000000000000, 1.000000000000000000, 1.000000000000000444, 0.9999999999999996669, 1.000000000000000222, 1.000000000000000444, 1.000000000000000000, 0.9999999999999997780, 1.000000000000000444, 1.000000000000000222, 1.000000000000000000, 1.000000000000000000, 1.000000000000000222, 1.000000000000000000, 1.000000000000000222, 0.9999999999999997780, 1.000000000000000222, 1.000000000000000000, 1.000000000000000000, 1.000000000000000444, 0.9999999999999996669, 1.000000000000000000, 0.9999999999999997780, 1.000000000000000222, 0.9999999999999996669, 1.000000000000000000, 1.000000000000000222, 0.9999999999999997780, 1.000000000000000444, 0.9999999999999997780, 1.000000000000000000, 0.9999999999999997780, 1.000000000000000222, 0.9999999999999996669, 1.000000000000000000, 1.000000000000000222, 0.9999999999999996669, 1.000000000000000444, 0.9999999999999997780, 1.000000000000000000, 1.000000000000000222, 0.9999999999999996669, 1.000000000000000222, 1.000000000000000000, 0.9999999999999997780, 1.000000000000000222, 0.9999999999999997780, 1.000000000000000000, 1.000000000000000222, 0.9999999999999997780, 1.000000000000000000, 1.000000000000000000, 0.9999999999999997780, 1.000000000000000000, 1.000000000000000222, 0.9999999999999997780, 1.000000000000000000, 1.000000000000000000, 1.000000000000000000, 0.9999999999999997780, 1.000000000000000222, 0.9999999999999997780, 0.9999999999999997780, 1.000000000000000444, 1.000000000000000000, 1.000000000000000000, 0.9999999999999997780, 1.000000000000000222, 1.000000000000000000, 1.000000000000000000, 1.000000000000000000, 1.000000000000000000, 1.000000000000000222, 1.000000000000000222, 0.9999999999999997780, 1.000000000000000000, 0.9999999999999997780, 1.000000000000000444, 0.9999999999999996669, 1.000000000000000666, 1.000000000000000000, 0.9999999999999997780, 1.000000000000000222, 1.000000000000000000, 1.000000000000000000, 1.000000000000000000, 0.9999999999999994449, 1.000000000000000666, 0.9999999999999996669, 1.000000000000000000, 1.000000000000000222, 0.9999999999999997780, 1.000000000000000222, 0.9999999999999997780, 1.000000000000000222, 0.9999999999999996669, 1.000000000000000444, 1.000000000000000000, 1.000000000000000222, 0.9999999999999996669, 1.000000000000000000, 1.000000000000000222, 0.9999999999999997780, 1.000000000000000000, 0.9999999999999997780, 1.000000000000000000, 1.000000000000000000, 1.000000000000000222, 0.9999999999999997780, 1.000000000000000222, 0.9999999999999997780, 1.000000000000000000, 1.000000000000000000, 1.000000000000000222, 0.9999999999999997780, 1.000000000000000444, 1.000000000000000000, 0.9999999999999997780, 1.000000000000000000, 1.000000000000000000, 1.000000000000000222, 0.9999999999999997780, 1.000000000000000222, 1.000000000000000000, 1.000000000000000000, 1.000000000000000000, 1.000000000000000222, 1.000000000000000000, 0.9999999999999997780, 1.000000000000000000, 1.000000000000000000, 1.000000000000000000, 1.000000000000000444, 0.9999999999999996669, 1.000000000000000222, 1.000000000000000000, 1.000000000000000222, 0.9999999999999997780, 1.000000000000000000, 0.9999999999999997780, 1.000000000000000000, 0.9999999999999997780, 1.000000000000000000, 1.000000000000000444, 0.9999999999999994449, 1.000000000000000444, 1.000000000000000000, 1.000000000000000222, 1.000000000000000222, 0.9999999999999997780, 1.000000000000000222, 0.9999999999999997780, 1.000000000000000222, 1.000000000000000222, 1.000000000000000222, 0.9999999999999997780, 1.000000000000000000, 1.000000000000000444, 0.9999999999999996669, 1.000000000000000000, 0.9999999999999997780, 1.000000000000000222, 1.000000000000000222, 1.000000000000000000, 0.9999999999999997780, 1.000000000000000222, 0.9999999999999997780, 1.000000000000000222, 0.9999999999999997780, 0.9999999999999997780, 1.000000000000000000, 1.000000000000000000, 1.000000000000000000, 1.000000000000000000, 1.000000000000000000, 1.000000000000000222, 1.000000000000000000, 1.000000000000000000, 1.000000000000000222, 1.000000000000000000, 0.9999999999999997780, 1.000000000000000000, 1.000000000000000000, 1.000000000000000000, 0.9999999999999997780, 1.000000000000000000, 0.9999999999999997780, 1.000000000000000000, 1.000000000000000222, 0.9999999999999996669, 1.000000000000000444, 1.000000000000000000, 0.9999999999999997780, 1.000000000000000222, 1.000000000000000000, 0.9999999999999997780, 1.000000000000000222, 1.000000000000000000, 1.000000000000000222, 1.000000000000000000, 0.9999999999999997780, 1.000000000000000222, 1.000000000000000000, 1.000000000000000000, 1.000000000000000222, 1.000000000000000000, 1.000000000000000000, 1.000000000000000222, 0.9999999999999997780, 0.9999999999999996669, 1.000000000000000444, 0.9999999999999994449, 1.000000000000000444, 0.9999999999999997780, 1.000000000000000222, 1.000000000000000000, 1.000000000000000000, 1.000000000000000000, 1.000000000000000000, 1.000000000000000444, 0.9999999999999996669, 1.000000000000000444, 1.000000000000000000, 0.9999999999999997780, 1.000000000000000444, 0.9999999999999994449, 1.000000000000000444, 0.9999999999999997780, 0.9999999999999997780, 1.000000000000000222, 1.000000000000000444, 0.9999999999999997780, 1.000000000000000444, 0.9999999999999997780, 1.000000000000000000, 1.000000000000000444, 0.9999999999999997780, 0.9999999999999997780, 1.000000000000000000, 1.000000000000000000, 1.000000000000000000, 0.9999999999999997780, 1.000000000000000444, 1.000000000000000222, 0.9999999999999997780, 1.000000000000000444, 1.000000000000000000, 1.000000000000000222, 1.000000000000000000, 1.000000000000000000, 1.000000000000000222, 0.9999999999999997780, 1.000000000000000222, 1.000000000000000222, 0.9999999999999997780, 1.000000000000000222, 1.000000000000000000, 1.000000000000000000, 1.000000000000000222, 0.9999999999999997780, 1.000000000000000444, 0.9999999999999997780, 0.9999999999999997780, 1.000000000000000222, 0.9999999999999997780, 1.000000000000000000, 1.000000000000000000, 0.9999999999999997780, 1.000000000000000222, 0.9999999999999996669, 1.000000000000000444, 0.9999999999999997780, 1.000000000000000222, 1.000000000000000222, 0.9999999999999997780, 1.000000000000000222, 0.9999999999999997780, 1.000000000000000000, 0.9999999999999997780, 1.000000000000000444, 0.9999999999999996669, 1.000000000000000222, 0.9999999999999996669, 1.000000000000000444, 1.000000000000000000, 0.9999999999999997780, 1.000000000000000222, 0.9999999999999996669, 1.000000000000000222, 1.000000000000000222, 0.9999999999999996669, 1.000000000000000444, 1.000000000000000222, 0.9999999999999997780, 1.000000000000000222, 0.9999999999999997780, 1.000000000000000222, 1.000000000000000000, 1.000000000000000222, 0.9999999999999996669, 1.000000000000000444, 1.000000000000000000, 1.000000000000000000, 1.000000000000000222, 0.9999999999999997780, 0.9999999999999997780, 1.000000000000000444, 1.000000000000000000, 1.000000000000000000, 0.9999999999999996669, 1.000000000000000000, 1.000000000000000222, 1.000000000000000000, 1.000000000000000000, 1.000000000000000222, 0.9999999999999997780, 1.000000000000000000, 0.9999999999999997780, 0.9999999999999997780, 1.000000000000000222, 0.9999999999999997780, 1.000000000000000000, 1.000000000000000000, 0.9999999999999997780, 1.000000000000000222, 1.000000000000000000, 1.000000000000000222, 1.000000000000000000, 1.000000000000000444, 1.000000000000000000, 1.000000000000000000, 0.9999999999999997780, 0.9999999999999997780, 1.000000000000000222, 1.000000000000000000, 1.000000000000000000, 1.000000000000000000, 0.9999999999999997780, 1.000000000000000222, 1.000000000000000000, 1.000000000000000000) ) ) 
 REPRESENTATION_ITEM ( '' )  SURFACE ( )  );
#104872 = CARTESIAN_POINT ( 'NONE',  ( -0.02919842301641034990, 1.352617229779122132, -2.329362550481127947 ) ) ;
#104873 = CARTESIAN_POINT ( 'NONE',  ( 1.499999999999990896, 5.556250000682820378, 1.214306433183764966E-14 ) ) ;
#104875 = CARTESIAN_POINT ( 'NONE',  ( 6.925078400183521055, 0.5534609092465185842, 2.295239920751692253 ) ) ;
#104874 = CARTESIAN_POINT ( 'NONE',  ( -6.204128743306504212, 7.035606015609114472, -1.046755002246579469 ) ) ;
#104876 = CARTESIAN_POINT ( 'NONE',  ( 6.369096972855497363, 1.760372669148374758, -0.5393517311068628528 ) ) ;
#104877 = ORIENTED_EDGE ( 'NONE', *, *, #191207, .T. ) ;
#104878 = CARTESIAN_POINT ( 'NONE',  ( 2.571226905367568261, 0.1023410288747768487, -2.058482174549924437 ) ) ;
#104879 = CARTESIAN_POINT ( 'NONE',  ( -4.757329562667670667E-14, 0.5781250003414447614, -1.570758158831812246 ) ) ;
#104880 = CARTESIAN_POINT ( 'NONE',  ( -5.696397096036042385, 9.797547045350714967, -0.7998128361456231517 ) ) ;
#104881 = CARTESIAN_POINT ( 'NONE',  ( 11.06299035296667732, 13.75683704376094774, -0.9087041361035911313 ) ) ;
#104882 = DIRECTION ( 'NONE',  ( -0.000000000000000000, -1.000000000000000000, -0.000000000000000000 ) ) ;
#104883 = CARTESIAN_POINT ( 'NONE',  ( 3.551346171775753735, 6.230655402791975384, 1.199719254218462483 ) ) ;
#104884 = CARTESIAN_POINT ( 'NONE',  ( 1.077108160694364214, -0.04970969036830223675, -2.060456431261459276 ) ) ;
#104885 =( BOUNDED_CURVE ( )  B_SPLINE_CURVE ( 2, ( #64794, #148201, #32306, #16022, #130938 ),
 .UNSPECIFIED., .F., .T. ) 
 B_SPLINE_CURVE_WITH_KNOTS ( ( 3, 2, 3 ),
 ( 0.01092446968156914403, 0.01250000000000000069, 0.01386088777671200430 ),
 .UNSPECIFIED. ) 
 CURVE ( )  GEOMETRIC_REPRESENTATION_ITEM ( )  RATIONAL_B_SPLINE_CURVE ( ( 0.9369925407309227516, 0.9493405508230843282, 1.000000000000000000, 0.9562421463088759399, 0.9410680661649852841 ) ) 
 REPRESENTATION_ITEM ( '' )  );
#104887 = CARTESIAN_POINT ( 'NONE',  ( 0.6823417656249969321, 13.27604166700806232, -1.181850606188757036 ) ) ;
#104886 = CARTESIAN_POINT ( 'NONE',  ( 4.897706171852771462, 4.871974472535213430, 0.6676900015689657408 ) ) ;
#104888 = CARTESIAN_POINT ( 'NONE',  ( 5.361359679200154105, 8.342337828120466980, 1.199719254218462483 ) ) ;
#104889 =( GEOMETRIC_REPRESENTATION_CONTEXT ( 3 ) GLOBAL_UNCERTAINTY_ASSIGNED_CONTEXT ( ( #160505 ) ) GLOBAL_UNIT_ASSIGNED_CONTEXT ( ( #102376, #55761, #138097 ) ) REPRESENTATION_CONTEXT ( 'NONE', 'WORKASPACE' ) );
#104890 = B_SPLINE_CURVE_WITH_KNOTS ( 'NONE', 3,
 ( #81136, #64877, #193806, #147222, #213246, #161330, #145110, #45455, #95282, #128900, #28119, #178649, #111571, #208977, #126773, #177579, #160253, #96346, #192731, #194881, #44385, #46517, #12914, #112640, #30260, #110507, #162401, #176507, #212042, #126638, #46383, #77799 ),
 .UNSPECIFIED., .F., .F.,
 ( 4, 2, 2, 2, 2, 2, 2, 2, 2, 2, 2, 2, 2, 2, 2, 4 ),
 ( 2.873115300368997076E-17, 0.001171507007196520090, 0.001757260510794765715, 0.002343014014393011990, 0.002928767517991258482, 0.003514521021589504975, 0.004100274525187751901, 0.004686028028785998827, 0.005271781532384244885, 0.005857535035982492679, 0.006443288539580738737, 0.007029042043178984796, 0.007614795546777232589, 0.008200549050375479515, 0.008786302553973725574, 0.009372056057571971632 ),
 .UNSPECIFIED. ) ;
#104891 = CARTESIAN_POINT ( 'NONE',  ( 11.92619526913699879, 12.69999999999999929, -1.328859060402686199 ) ) ;
#104892 = CIRCLE ( 'NONE', #149880, 2.025000000000006573 ) ;
#104893 = CARTESIAN_POINT ( 'NONE',  ( 5.373716497573798101, 2.127666891504222058, -0.5857064233696291922 ) ) ;
#104894 = CARTESIAN_POINT ( 'NONE',  ( 0.7730135719010817752, -2.035059957909639561, -0.7290066412228360937 ) ) ;
#104895 = CARTESIAN_POINT ( 'NONE',  ( -4.690757960648240577, 6.495636925554817864, 1.443375672974064550 ) ) ;
#104896 = CARTESIAN_POINT ( 'NONE',  ( 6.416260824072121061, -1.810972107014690913, 0.05430519662179972284 ) ) ;
#104897 = CARTESIAN_POINT ( 'NONE',  ( 0.7609543035823238544, -0.05432987398422234326, -2.015980609757315190 ) ) ;
#104898 = CARTESIAN_POINT ( 'NONE',  ( 6.983858524370772258, 9.241197259889668558, 1.443375672974063439 ) ) ;
#104899 = CARTESIAN_POINT ( 'NONE',  ( 1.353307579497017965, -1.032721833433938530, 2.053394521917959015 ) ) ;
#104900 = DIRECTION ( 'NONE',  ( -0.000000000000000000, -1.000000000000000000, -0.000000000000000000 ) ) ;
#104901 = CARTESIAN_POINT ( 'NONE',  ( 6.586579894266019863, -1.172543786506787145, 1.511232097859278145 ) ) ;
#104902 = CARTESIAN_POINT ( 'NONE',  ( 1.973319494866377699, 1.790917844098998124, -0.5403536831049270406 ) ) ;
#104903 = CARTESIAN_POINT ( 'NONE',  ( 2.325407997918966796, -1.497503195670712328, -1.350734289967000512 ) ) ;
#104905 = CARTESIAN_POINT ( 'NONE',  ( 2.310781476690497271, 5.467761476598782977, -0.5169845646830224517 ) ) ;
#104904 = CARTESIAN_POINT ( 'NONE',  ( -1.364683531250014514, 1.238541667008091096, -0.7879004041258289570 ) ) ;
#104906 = B_SPLINE_CURVE_WITH_KNOTS ( 'NONE', 3,
 ( #35114, #101185, #120729, #2601 ),
 .UNSPECIFIED., .F., .F.,
 ( 4, 4 ),
 ( 0.000000000000000000, 0.0004037790303856098246 ),
 .UNSPECIFIED. ) ;
#104908 = CARTESIAN_POINT ( 'NONE',  ( 4.899102953068730670, 1.751457851224359041, -1.169261236274852012 ) ) ;
#104907 = CARTESIAN_POINT ( 'NONE',  ( -8.636707547105197946, 10.03491254549959777, -1.199719254218446718 ) ) ;
#104909 = CARTESIAN_POINT ( 'NONE',  ( 8.281332899848809603, 8.555976559445431562, 0.7998128361456481317 ) ) ;
#104911 = CARTESIAN_POINT ( 'NONE',  ( -6.690058733339450114, 9.892486724616283311, 1.199719254218452047 ) ) ;
#104910 = CARTESIAN_POINT ( 'NONE',  ( 3.386504508363381571, 7.172948703057747011, -0.7998128361456362523 ) ) ;
#104912 = CARTESIAN_POINT ( 'NONE',  ( 0.06269018847613376522, -7.008739397177144781, -9.499801640457381069 ) ) ;
#104913 = CARTESIAN_POINT ( 'NONE',  ( 4.676038720085195166, 1.997217120926295442, -0.3003719491122060492 ) ) ;
#104914 = CARTESIAN_POINT ( 'NONE',  ( 1.364683531249988535, 4.405208333674754506, -0.7879004041258300672 ) ) ;
#104915 = CARTESIAN_POINT ( 'NONE',  ( 6.250444628687981563, -2.052375444028589957, -0.2060817263721328174 ) ) ;
#104916 = CARTESIAN_POINT ( 'NONE',  ( 9.083599731475983319, 11.62061899152058686, 1.443375672974076540 ) ) ;
#104917 = CARTESIAN_POINT ( 'NONE',  ( 5.413408226029434722, -0.3230527293765028674, 2.137217106551466905 ) ) ;
#104918 = CARTESIAN_POINT ( 'NONE',  ( 7.035755370848908896, 7.173079118937375931, 0.7998128361456352531 ) ) ;
#104919 = CARTESIAN_POINT ( 'NONE',  ( 1.364683531249988757, -0.3031249996585799744, 0.000000000000000000 ) ) ;
#104921 = CARTESIAN_POINT ( 'NONE',  ( 8.876521693626907350, 3.555461883994700756, 7.992456032239036112 ) ) ;
#104920 = CARTESIAN_POINT ( 'NONE',  ( 6.527324610336440180, 6.579909898339485252, 0.7998128361456331437 ) ) ;
#104922 = CARTESIAN_POINT ( 'NONE',  ( 7.822691444960700125, 10.14955932391940330, -1.443375672974058777 ) ) ;
#104924 = CARTESIAN_POINT ( 'NONE',  ( -0.1172869779874923940, -7.889939693150851419, 10.99948653685772548 ) ) ;
#104923 = CARTESIAN_POINT ( 'NONE',  ( 1.944024895830529731, 1.496304202470769340, 1.573470141065239414 ) ) ;
#104926 = CARTESIAN_POINT ( 'NONE',  ( 1.557894219809667247, -1.301531972126177772, 1.302644501960325885 ) ) ;
#104925 = CARTESIAN_POINT ( 'NONE',  ( -4.121315508874255684, 7.752025827087861920, -0.7216878364870267237 ) ) ;
#104927 = CARTESIAN_POINT ( 'NONE',  ( 0.6823417656249899377, 3.926041667008085767, -1.181850606188754593 ) ) ;
#104928 = CARTESIAN_POINT ( 'NONE',  ( 3.351304529449970371, 0.5305821810032870234, -2.126252377916526992 ) ) ;
#104929 = CARTESIAN_POINT ( 'NONE',  ( 6.983263157960386991, 3.689421308571324776, 2.567857239638075217 ) ) ;
#104930 = CARTESIAN_POINT ( 'NONE',  ( 4.258826902089789535, -1.679047235397194804, 1.516690725115140692 ) ) ;
#104931 = CARTESIAN_POINT ( 'NONE',  ( -5.530836599371015794, 8.540060901653093950, 1.199719254218452047 ) ) ;
#104932 = DIRECTION ( 'NONE',  ( -0.9366510587354612838, 0.000000000000000000, 0.3502638921866474409 ) ) ;
#104933 = CARTESIAN_POINT ( 'NONE',  ( 6.330867959801246059, 6.852818249511213544, -0.6651261847785728820 ) ) ;
#104934 = AXIS2_PLACEMENT_3D ( 'NONE', #69698, #203959, #56680 ) ;
#104935 = CARTESIAN_POINT ( 'NONE',  ( -6.009258394948636914E-15, 14.18750000000000355, -1.732050807568875195 ) ) ;
#104936 = CARTESIAN_POINT ( 'NONE',  ( 4.258669648468268676, 7.982548666606070320, 0.7216878364870257245 ) ) ;
#104937 = CARTESIAN_POINT ( 'NONE',  ( 5.712081065023381754, -0.7967057657092267986, -1.580296573674238259 ) ) ;
#104938 =( BOUNDED_CURVE ( )  B_SPLINE_CURVE ( 2, ( #39968, #126616, #142822, #207771, #172098 ),
 .UNSPECIFIED., .F., .T. ) 
 B_SPLINE_CURVE_WITH_KNOTS ( ( 3, 2, 3 ),
 ( 0.2230065254996309865, 0.2250000000000000056, 0.2273705207416776009 ),
 .UNSPECIFIED. ) 
 CURVE ( )  GEOMETRIC_REPRESENTATION_ITEM ( )  RATIONAL_B_SPLINE_CURVE ( ( 0.9512353381494595972, 0.9679510070496450957, 1.000000000000000000, 0.9618892528975757639, 0.9454606617520617817 ) ) 
 REPRESENTATION_ITEM ( '' )  );
#104939 = CARTESIAN_POINT ( 'NONE',  ( 7.639129486296027061, 10.99973593639901814, 1.199719254218460707 ) ) ;
#104940 = CARTESIAN_POINT ( 'NONE',  ( 1.817543918834242378, -0.2582919827684154179, 2.089997942319920199 ) ) ;
#104942 = CARTESIAN_POINT ( 'NONE',  ( -1.500000000000013101, 2.629166666666687746, -0.8660254037844313801 ) ) ;
#104941 = CARTESIAN_POINT ( 'NONE',  ( 1.364683531250000303, 11.50520833367472839, -0.7879004041258355073 ) ) ;
#104943 = CARTESIAN_POINT ( 'NONE',  ( 1.275766937089892750, -1.922257851437941811, 0.4282784019480969651 ) ) ;
#104944 = CARTESIAN_POINT ( 'NONE',  ( 2.969872605471105320, 6.605953636083950364, 7.500000000000000000 ) ) ;
#104945 = CARTESIAN_POINT ( 'NONE',  ( 0.1331565106231328843, 0.003911343561965873426, -1.946049565259087455 ) ) ;
#104947 = VERTEX_POINT ( 'NONE', #84334 ) ;
#104946 = CARTESIAN_POINT ( 'NONE',  ( 5.537325978022108686, -0.03587880057049273180, 1.811405195203552587 ) ) ;
#104948 = CARTESIAN_POINT ( 'NONE',  ( 6.860062538834778678, 8.066123052471139587, -1.082531754730543083 ) ) ;
#104949 = CARTESIAN_POINT ( 'NONE',  ( 1.364683531249986537, -1.073958332991911790, 0.7879004041258500513 ) ) ;
#104950 = CARTESIAN_POINT ( 'NONE',  ( 4.715616592392388284, -1.834479983729628616, 0.3652084810651031743 ) ) ;
#104951 = AXIS2_PLACEMENT_3D ( 'NONE', #62715, #163440, #17152 ) ;
#104952 = ORIENTED_EDGE ( 'NONE', *, *, #56424, .F. ) ;
#104953 = CARTESIAN_POINT ( 'NONE',  ( 6.051642586050197892, 1.563818258945087969, 1.356687170345115989 ) ) ;
#104954 = CARTESIAN_POINT ( 'NONE',  ( 1.224999999999953015, 1.854166666666720698, 0.7072540797572656190 ) ) ;
#104955 = CARTESIAN_POINT ( 'NONE',  ( -4.950135482320926705, 6.868520377498098739, -1.443375672974066548 ) ) ;
#104956 = CARTESIAN_POINT ( 'NONE',  ( 0.2739938332866619364, -2.030697503880642518, 0.4024348779970430834 ) ) ;
#104957 = CARTESIAN_POINT ( 'NONE',  ( 1.499999999999987566, -0.9749999999999827693, 0.000000000000000000 ) ) ;
#104958 = CARTESIAN_POINT ( 'NONE',  ( 6.414979237560321401, 10.63589287712906462, 1.040834085586084257E-14 ) ) ;
#104959 = CARTESIAN_POINT ( 'NONE',  ( -9.341731535015849630, 10.85744053139533349, 1.199719254218462483 ) ) ;
#104960 = CARTESIAN_POINT ( 'NONE',  ( 7.042534447655770080, 7.180988041878682004, -0.7998128361456341429 ) ) ;
#104961 = CARTESIAN_POINT ( 'NONE',  ( 1.364683531249986537, -0.1364583329919154264, 0.7879004041258500513 ) ) ;
#104962 = CARTESIAN_POINT ( 'NONE',  ( 1.499999999999987121, 0.7958333333333510451, -0.8660254037844253849 ) ) ;
#104964 = CARTESIAN_POINT ( 'NONE',  ( 4.635998460869027227, 7.496083073400806818, -1.199719254218452047 ) ) ;
#104963 = CARTESIAN_POINT ( 'NONE',  ( 5.494571831323358246, 1.932540981948445147, 0.3370517209014682325 ) ) ;
#104965 = CARTESIAN_POINT ( 'NONE',  ( 2.460314346279086628, 1.556669099887195484, 1.281166478716524892 ) ) ;
#104966 = CARTESIAN_POINT ( 'NONE',  ( 1.084637062511527361, 2.838621193390831188, -1.105835307554789759 ) ) ;
#104967 = AXIS2_PLACEMENT_3D ( 'NONE', #20590, #151694, #50984 ) ;
#104968 = CARTESIAN_POINT ( 'NONE',  ( 0.6619992422990974568, 1.085049530943157148, 1.904046507712559455 ) ) ;
#104969 = DIRECTION ( 'NONE',  ( -0.000000000000000000, -1.000000000000000000, -0.000000000000000000 ) ) ;
#104970 = CARTESIAN_POINT ( 'NONE',  ( 1.985418980784030119, 1.286400883397397221, 1.358229366437320618 ) ) ;
#104971 = CARTESIAN_POINT ( 'NONE',  ( 0.6823417656249917140, 4.842708333674755394, 1.181850606188765695 ) ) ;
#104972 = CARTESIAN_POINT ( 'NONE',  ( 3.902593620319398937, -1.991888969257959774, -0.2912845021679384971 ) ) ;
#104973 = CARTESIAN_POINT ( 'NONE',  ( -8.158255747121117452, 10.54105100977322174, 1.599625672291295375 ) ) ;
#104975 = CARTESIAN_POINT ( 'NONE',  ( 4.763340612834221943, 1.975027209670917161, -0.7632558447715469541 ) ) ;
#104974 = CARTESIAN_POINT ( 'NONE',  ( -4.934804725694224459, 6.780358151441803649, -1.443375672974053447 ) ) ;
#104977 = EDGE_CURVE ( 'NONE', #210054, #195556, #37722, .T. ) ;
#104976 = CARTESIAN_POINT ( 'NONE',  ( -3.672734859294646270E-15, -9.900000000000005684, -9.579665964948937074 ) ) ;
#104978 = CARTESIAN_POINT ( 'NONE',  ( 5.758279222819879806, -2.070544812512797428, -0.003756845764937844813 ) ) ;
#104980 = CARTESIAN_POINT ( 'NONE',  ( 6.720655732516636505, 1.219515403015670296, 2.385684514189966521 ) ) ;
#104979 = CARTESIAN_POINT ( 'NONE',  ( 0.7848512634026264534, 1.842159585024247148, -0.9888006619010838438 ) ) ;
#104982 = EDGE_LOOP ( 'NONE', ( #91397, #172478, #142590, #121455 ) ) ;
#104981 = CARTESIAN_POINT ( 'NONE',  ( 6.721730220878607831, -1.769880579078547012, 0.4471725050417332814 ) ) ;
#104983 = CARTESIAN_POINT ( 'NONE',  ( 7.019370843573166319, 9.212351955633947043, 1.599625672291281386 ) ) ;
#104984 = FACE_OUTER_BOUND ( 'NONE', #147347, .T. ) ;
#104985 = CARTESIAN_POINT ( 'NONE',  ( -9.748179543381699119, 3.057003318903428912, 6.445181705109019887 ) ) ;
#104986 = CARTESIAN_POINT ( 'NONE',  ( 7.334597914868727919, 9.580116872145431728, -1.443375672974058777 ) ) ;
#104987 = CARTESIAN_POINT ( 'NONE',  ( -0.6823417656250003738, 12.71354166700806942, 1.181850606188754593 ) ) ;
#104988 = CARTESIAN_POINT ( 'NONE',  ( -0.1051951494144076904, -0.1375245761873785666, -1.781266614511106683 ) ) ;
#104989 = CARTESIAN_POINT ( 'NONE',  ( -6.832419346282942563, 10.05857410638369487, 1.199719254218453823 ) ) ;
#104990 = CARTESIAN_POINT ( 'NONE',  ( 4.008406971134620633, 7.828225232965717595, 0.7998128361456321445 ) ) ;
#104991 = DIRECTION ( 'NONE',  ( -5.578564026256490882E-16, -1.000000000000000000, -9.066213480720158442E-32 ) ) ;
#104992 = CARTESIAN_POINT ( 'NONE',  ( 3.836594282542920009, 4.538743420130594508, 1.082531754730560403 ) ) ;
#104993 = CARTESIAN_POINT ( 'NONE',  ( 4.760321332173959696, 4.726332107057286791, 0.000000000000000000 ) ) ;
#104994 = CARTESIAN_POINT ( 'NONE',  ( 3.063252641683779753, 5.661212951017999373, 1.199719254218450271 ) ) ;
#104995 = ORIENTED_EDGE ( 'NONE', *, *, #148616, .F. ) ;
#104996 = CARTESIAN_POINT ( 'NONE',  ( 6.204703874486805049, 1.882480396761162744, 0.7231267579426368108 ) ) ;
#104997 = CARTESIAN_POINT ( 'NONE',  ( 0.08289510313583270396, -1.381697626658566547, 1.608636130391014163 ) ) ;
#104998 = LINE ( 'NONE', #3179, #206082 ) ;
#104999 = CARTESIAN_POINT ( 'NONE',  ( -0.1399997263889594112, -0.002789056014654289761, -2.000146600338557956 ) ) ;
#105000 = ADVANCED_FACE ( 'NONE', ( #66987 ), #140970, .T. ) ;
#105001 = CARTESIAN_POINT ( 'NONE',  ( -5.924549939491850381, 6.014322472269677533, 0.000000000000000000 ) ) ;
#105002 = CARTESIAN_POINT ( 'NONE',  ( 4.369805582306193870, 3.992528022312320957, 1.214306433183764966E-14 ) ) ;
#105003 = CARTESIAN_POINT ( 'NONE',  ( 3.924621296410530480, -1.326038130087652922, 1.456277141313151224 ) ) ;
#105004 = CARTESIAN_POINT ( 'NONE',  ( 4.148064665909578785, 0.9530284220014314522, 1.777003606838889915 ) ) ;
#105005 = CARTESIAN_POINT ( 'NONE',  ( -7.366157530926372488, 7.488271962369228874, -0.7998128361456291469 ) ) ;
#105006 = CARTESIAN_POINT ( 'NONE',  ( 4.875033280109006384, 2.045454206080063120, -0.7869404205859964474 ) ) ;
#105007 = CARTESIAN_POINT ( 'NONE',  ( -0.6823417656250003738, 3.030208333674754062, -1.181850606188749264 ) ) ;
#105008 = CARTESIAN_POINT ( 'NONE',  ( 3.188414472400236566, -1.897621675979482614, -0.3308535721826404985 ) ) ;
#105009 = CARTESIAN_POINT ( 'NONE',  ( -7.640183256500752584, 8.872300873127729304, -1.199719254218446718 ) ) ;
#105010 = CARTESIAN_POINT ( 'NONE',  ( -0.02988540731099428513, 0.2551080090007939449, -1.761437810625957834 ) ) ;
#105011 = CARTESIAN_POINT ( 'NONE',  ( 0.01274299142895937362, -0.9473294304004549193, -1.991142614049784099 ) ) ;
#105012 = FILL_AREA_STYLE ('',( #25860 ) ) ;
#105013 = CARTESIAN_POINT ( 'NONE',  ( -1.247849810309911822, 13.37576698399836594, 0.5524780460566154350 ) ) ;
#105014 = CARTESIAN_POINT ( 'NONE',  ( 3.798255590122797898, 7.583048621785260401, -0.7998128361456221525 ) ) ;
#105015 = ORIENTED_EDGE ( 'NONE', *, *, #23723, .F. ) ;
#105016 = CARTESIAN_POINT ( 'NONE',  ( 5.099275172515607579, 5.121778254122544283, -0.7216878364870458196 ) ) ;
#105017 = ORIENTED_EDGE ( 'NONE', *, *, #130874, .F. ) ;
#105018 = CARTESIAN_POINT ( 'NONE',  ( 5.190276988288149873, 1.015767153246112775, -1.687157232322311629 ) ) ;
#105019 = ORIENTED_EDGE ( 'NONE', *, *, #84508, .F. ) ;
#105021 = CARTESIAN_POINT ( 'NONE',  ( 4.002593568968414672, -1.991494762441379462, -0.2932518702276361022 ) ) ;
#105020 = CARTESIAN_POINT ( 'NONE',  ( 0.5033352851749985923, -1.932590057610440226, 0.1917435184634954937 ) ) ;
#105022 = CARTESIAN_POINT ( 'NONE',  ( 5.483857608503296177, 2.120574376644312586, 0.8868611222285858187 ) ) ;
#105024 = CARTESIAN_POINT ( 'NONE',  ( 3.660865129197692358, 1.469539745679597553, -1.141665872729610287 ) ) ;
#105023 = FILL_AREA_STYLE ('',( #73563 ) ) ;
#105025 = CARTESIAN_POINT ( 'NONE',  ( -1.642778471875000035, -0.8677083328553769626, -2.845375778867859751 ) ) ;
#105026 = CARTESIAN_POINT ( 'NONE',  ( -10.41272866534590591, -5.796408561411221072, -4.392600644672434268E-13 ) ) ;
#105027 = FACE_OUTER_BOUND ( 'NONE', #121198, .T. ) ;
#105028 = CARTESIAN_POINT ( 'NONE',  ( -6.693975156845199059, 8.832723654451292816, 1.599625672291283607 ) ) ;
#105029 = CARTESIAN_POINT ( 'NONE',  ( -4.584065335196305213, 6.441438539186039591, 1.443375672974058777 ) ) ;
#105030 = CARTESIAN_POINT ( 'NONE',  ( 5.776921370525399446, 1.931409454660049319, -0.8010388902379047549 ) ) ;
#105031 = CARTESIAN_POINT ( 'NONE',  ( 5.585596099150174965, 7.539614753807099667, -1.443375672974057666 ) ) ;
#105032 = ORIENTED_EDGE ( 'NONE', *, *, #105908, .T. ) ;
#105033 = FILL_AREA_STYLE ('',( #56269 ) ) ;
#105034 = CARTESIAN_POINT ( 'NONE',  ( 4.744428268735178200, 8.268600469562487731, 0.7448146739494916346 ) ) ;
#105035 = CARTESIAN_POINT ( 'NONE',  ( 0.9260630535584664091, 1.089557764695957554, -1.464779044915397455 ) ) ;
#105036 = CARTESIAN_POINT ( 'NONE',  ( -4.629219384062206011, 7.488174150459498968, -1.199719254218452047 ) ) ;
#105037 = CIRCLE ( 'NONE', #80908, 0.07999999999999946043 ) ;
#105038 = CARTESIAN_POINT ( 'NONE',  ( 2.812812116114179251, 0.9611239539163253243, -1.443176275507858319 ) ) ;
#105039 = CARTESIAN_POINT ( 'NONE',  ( -10.36939107341403776, 1.813436143228261521, -6.039542801432668639 ) ) ;
#105040 = CARTESIAN_POINT ( 'NONE',  ( -5.010594053901753497, 4.810390915832282843, -0.2947457133052544531 ) ) ;
#105041 = CARTESIAN_POINT ( 'NONE',  ( -6.555530967407501741, 7.606873202518897870, 1.199719254218450271 ) ) ;
#105042 = CARTESIAN_POINT ( 'NONE',  ( -5.786256696412555911, 6.075953140482280190, 0.5845640519336701146 ) ) ;
#105044 = CIRCLE ( 'NONE', #163798, 4.000000000000000000 ) ;
#105043 = CARTESIAN_POINT ( 'NONE',  ( 6.561400879130542485, 1.800260439488234443, 1.213256210689506176 ) ) ;
#105045 = CARTESIAN_POINT ( 'NONE',  ( 5.109893933574640279, -1.816543354971979163, 0.1824992186492402357 ) ) ;
#105046 = CARTESIAN_POINT ( 'NONE',  ( 3.625789200213443753, 1.914935786268581852, -0.4253726038727227432 ) ) ;
#105047 = B_SPLINE_CURVE_WITH_KNOTS ( 'NONE', 3,
 ( #170254, #86880, #21839, #121597 ),
 .UNSPECIFIED., .F., .F.,
 ( 4, 4 ),
 ( 3.338216057386796243E-18, 0.0006335992342243239534 ),
 .UNSPECIFIED. ) ;
#105048 = CARTESIAN_POINT ( 'NONE',  ( -1.225000000000004086, -0.9166666659838483833, 0.7072540797572737237 ) ) ;
#105049 = CARTESIAN_POINT ( 'NONE',  ( -7.967387826325084355, 12.44703623068796361, 0.7998128361456481317 ) ) ;
#105050 = CARTESIAN_POINT ( 'NONE',  ( 7.450369105909416589, 8.650851030771185890, -1.199719254218441611 ) ) ;
#105051 = CARTESIAN_POINT ( 'NONE',  ( 3.862070080935349203, 0.7130468835700142227, -1.997148454185311506 ) ) ;
#105052 = ADVANCED_FACE ( 'NONE', ( #153614 ), #206612, .F. ) ;
#105053 = CARTESIAN_POINT ( 'NONE',  ( 5.671053392266061977, 9.838255734277600695, 0.7998128361456331437 ) ) ;
#105054 = CARTESIAN_POINT ( 'NONE',  ( -8.597841969360544567, 13.18256606422934674, 0.7998128361456341429 ) ) ;
#105055 = CARTESIAN_POINT ( 'NONE',  ( 2.079047829753433163, 1.930162853665925216, 0.7490395704240898622 ) ) ;
#105057 = CARTESIAN_POINT ( 'NONE',  ( 0.6823417656249882723, -0.8447916663252494907, 1.181850606188755259 ) ) ;
#105056 = SURFACE_SIDE_STYLE ('',( #36819 ) ) ;
#105059 = VERTEX_POINT ( 'NONE', #9487 ) ;
#105058 = CARTESIAN_POINT ( 'NONE',  ( 4.600346979525781421, -1.047586700562872286, 1.958737397810013325 ) ) ;
#105060 = CARTESIAN_POINT ( 'NONE',  ( 2.303761666418477461, 1.498124540730429333, -1.743551778261544838 ) ) ;
#105062 = CARTESIAN_POINT ( 'NONE',  ( 6.403195902773025416, -1.745507933166186465, 1.098531482539546023 ) ) ;
#105061 = CARTESIAN_POINT ( 'NONE',  ( 8.920901888111986366, 12.39117405523060889, 1.082531754730546636 ) ) ;
#105064 = CARTESIAN_POINT ( 'NONE',  ( -1.737499999999997824, -0.9916666666666684726, 3.009438278150925683 ) ) ;
#105063 = CARTESIAN_POINT ( 'NONE',  ( 5.560252395380198998, 9.501061871336672127, 0.7216878364870317197 ) ) ;
#105065 = CARTESIAN_POINT ( 'NONE',  ( 1.734723475976807094E-15, 14.99962766111844736, 11.68000013863625774 ) ) ;
#105066 = CARTESIAN_POINT ( 'NONE',  ( 0.000000000000000000, 5.999999999999998224, 0.000000000000000000 ) ) ;
#105067 = DIRECTION ( 'NONE',  ( 0.000000000000000000, 0.000000000000000000, 1.000000000000000000 ) ) ;
#105068 = CARTESIAN_POINT ( 'NONE',  ( 3.375170810042011915, -1.688748480992762868, -0.8973671847329609541 ) ) ;
#105069 = CARTESIAN_POINT ( 'NONE',  ( 1.737499999999999378, -1.166666666666666519, -3.009438278150925683 ) ) ;
#105070 = CARTESIAN_POINT ( 'NONE',  ( 4.084733067335220902, -0.1695706708978762522, -1.716391344981627709 ) ) ;
#105071 = CARTESIAN_POINT ( 'NONE',  ( 1.991423064788412800, -0.4370762659771566527, 1.968445590580846893 ) ) ;
#105072 = CARTESIAN_POINT ( 'NONE',  ( 4.254688019566841284, 2.229798712500128843, -0.5580973643144919727 ) ) ;
#105073 = CARTESIAN_POINT ( 'NONE',  ( 3.831548730252303248, -2.092150397999822165, 0.8615055239265239084 ) ) ;
#105074 = CARTESIAN_POINT ( 'NONE',  ( 6.322895070704796616, 1.964426112044151518, 0.7597984924697271936 ) ) ;
#105075 = CARTESIAN_POINT ( 'NONE',  ( -6.305950844131887223, 6.529566537674873494, 0.000000000000000000 ) ) ;
#105076 = ORIENTED_EDGE ( 'NONE', *, *, #188776, .T. ) ;
#105077 = CARTESIAN_POINT ( 'NONE',  ( 4.200303217096891473, -0.5537481437246688509, -1.680960689856024537 ) ) ;
#105079 = CARTESIAN_POINT ( 'NONE',  ( 1.289493641233057319, 1.738593318175378766, 1.494007209952723958 ) ) ;
#105078 = CARTESIAN_POINT ( 'NONE',  ( 5.905458427204159477, 9.047396044116986502, 1.199719254218452047 ) ) ;
#105080 = CARTESIAN_POINT ( 'NONE',  ( 5.824118960990139371, 1.775556191179916699, 0.4867722729226392486 ) ) ;
#105081 = CARTESIAN_POINT ( 'NONE',  ( -3.598799709423620374, 6.286017863381107240, 1.199719254218464037 ) ) ;
#105082 = CARTESIAN_POINT ( 'NONE',  ( 5.314472526525434226, 2.023830839259177949, 0.8410439265160508659 ) ) ;
#105083 = CARTESIAN_POINT ( 'NONE',  ( -5.655686355556086120, 6.627330832017406692, 1.199719254218452935 ) ) ;
#105084 = FACE_OUTER_BOUND ( 'NONE', #5300, .T. ) ;
#105085 = CARTESIAN_POINT ( 'NONE',  ( -7.334597915313094241, 9.580116872663850813, 1.040834085586084257E-14 ) ) ;
#105086 = CARTESIAN_POINT ( 'NONE',  ( 6.057099581687969803, 1.694805161836069107, -1.188877858866774107 ) ) ;
#105087 = CARTESIAN_POINT ( 'NONE',  ( 1.094935803221647186, 1.780670018850015079, 0.9462964651613046119 ) ) ;
#105088 = CARTESIAN_POINT ( 'NONE',  ( -1.500000000000015099, -1.297916665983847029, 0.8660254037844403729 ) ) ;
#105089 = CARTESIAN_POINT ( 'NONE',  ( 4.178288987252887665, -1.108116244417625573, 1.575729328202896573 ) ) ;
#105090 = CARTESIAN_POINT ( 'NONE',  ( 0.6823417656249969321, 10.77604166700806765, -1.181850606188757036 ) ) ;
#105091 = CARTESIAN_POINT ( 'NONE',  ( 0.7564555125054818197, 0.8934716743186126298, -2.033981271184843731 ) ) ;
#105092 = VERTEX_POINT ( 'NONE', #124397 ) ;
#105093 = CARTESIAN_POINT ( 'NONE',  ( 1.435115314734431324, 7.268684689231784901, -4.324912918975645226 ) ) ;
#105094 = CARTESIAN_POINT ( 'NONE',  ( 3.379006598303866848, 4.965260336153046516, -1.599625672291262513 ) ) ;
#105095 = CARTESIAN_POINT ( 'NONE',  ( 11.33772463945036790, 13.40000000000000036, -3.680000000000002824 ) ) ;
#105096 = CARTESIAN_POINT ( 'NONE',  ( 3.876876046179563051, 7.339504906929419370, -0.7537628779380199928 ) ) ;
#105097 = CARTESIAN_POINT ( 'NONE',  ( 9.768581443174442214, 11.88588759030453268, -6.891829356553425434 ) ) ;
#105098 = CARTESIAN_POINT ( 'NONE',  ( 2.453501617077270325, 1.514643136537169310, 1.246875331876770021 ) ) ;
#105100 = CARTESIAN_POINT ( 'NONE',  ( 1.364683531249988535, 2.176041667008087543, 0.7879004041258500513 ) ) ;
#105099 = CARTESIAN_POINT ( 'NONE',  ( 3.974511587100456822, 7.788680618259193444, 1.040834085586084257E-14 ) ) ;
#105101 = EDGE_CURVE ( 'NONE', #114840, #12663, #72334, .T. ) ;
#105102 = DIRECTION ( 'NONE',  ( 8.881784197001252323E-15, 0.000000000000000000, -1.000000000000000000 ) ) ;
#105103 = CIRCLE ( 'NONE', #84200, 6.329999999999995630 ) ;
#105104 = CARTESIAN_POINT ( 'NONE',  ( 0.3267250850040852583, -1.348467290049197853, 1.560915443186759122 ) ) ;
#105105 = CARTESIAN_POINT ( 'NONE',  ( -9.806625181386236179, 10.33548422123910449, -0.7998128361456291469 ) ) ;
#105106 = CARTESIAN_POINT ( 'NONE',  ( -5.382223794500852421, 5.381608636446842731, -0.7216878364870197293 ) ) ;
#105107 = CARTESIAN_POINT ( 'NONE',  ( 0.3041012005207919255, -0.5996659824250392123, 2.181524510355018265 ) ) ;
#105109 = ORIENTED_EDGE ( 'NONE', *, *, #62295, .F. ) ;
#105108 = CARTESIAN_POINT ( 'NONE',  ( -5.555090253297260361, 7.504024600312024340, 1.599625672291269396 ) ) ;
#105110 = CARTESIAN_POINT ( 'NONE',  ( -0.7500000000000006661, -1.110416665983847473, -1.299038105676652011 ) ) ;
#105111 = CARTESIAN_POINT ( 'NONE',  ( 1.563515255687727645, 1.843751956470768283, -0.3144994141817195055 ) ) ;
#105112 = CARTESIAN_POINT ( 'NONE',  ( 6.819718782980952909, -1.336886906709513712, 1.104006757392479887 ) ) ;
#105113 = AXIS2_PLACEMENT_3D ( 'NONE', #103592, #151281, #169649 ) ;
#105115 = CARTESIAN_POINT ( 'NONE',  ( 3.650093349144762023, 0.7902683543556283663, 2.044282924279612779 ) ) ;
#105114 = CARTESIAN_POINT ( 'NONE',  ( 1.360316468749981800, 1.744791667008098290, 0.7853790794158680422 ) ) ;
#105116 = CARTESIAN_POINT ( 'NONE',  ( 5.508889292638126989, 1.751971812537992834, -1.501964572959401778 ) ) ;
#105117 = CARTESIAN_POINT ( 'NONE',  ( 6.837187436585446143, -1.842956594435873896, 0.9222261209423606720 ) ) ;
#105118 = CARTESIAN_POINT ( 'NONE',  ( 2.712754350931959380, -0.1900897480172674958, 1.932619341894822540 ) ) ;
#105119 = CARTESIAN_POINT ( 'NONE',  ( -5.544921637864838715, 6.531792001339513654, -1.082531754730543971 ) ) ;
#105120 = ADVANCED_FACE ( 'NONE', ( #58242 ), #114316, .T. ) ;
#105121 = CARTESIAN_POINT ( 'NONE',  ( -0.1104750535120248289, 7.629137130509052511, -2.703481013110929254 ) ) ;
#105122 = CARTESIAN_POINT ( 'NONE',  ( 4.665414256878284149, 6.536345614481700927, -1.443375672974068769 ) ) ;
#105123 = CARTESIAN_POINT ( 'NONE',  ( 1.224999999999948797, 2.895833333333310389, -0.7072540797573237947 ) ) ;
#105124 = CARTESIAN_POINT ( 'NONE',  ( 3.815077410725797424, 1.076317812134291119, -1.704938119663282903 ) ) ;
#105125 = CARTESIAN_POINT ( 'NONE',  ( -4.894130264408873110, 5.772535398974209642, -1.082531754730543971 ) ) ;
#105126 = CARTESIAN_POINT ( 'NONE',  ( -6.791708605802965870, 6.888357893050385705, -0.7998128361456362523 ) ) ;
#105127 = CARTESIAN_POINT ( 'NONE',  ( 8.550388431712704573, 13.12720360364021133, 0.000000000000000000 ) ) ;
#105129 = CARTESIAN_POINT ( 'NONE',  ( -1.499999999999993339, 10.64264068711930733, 1.232676135170975238E-14 ) ) ;
#105128 = CARTESIAN_POINT ( 'NONE',  ( 0.6799654140086827114, -1.016662149479659494, 1.516215539243186639 ) ) ;
#105130 = CARTESIAN_POINT ( 'NONE',  ( -4.776215253764153346, 8.794277906025310898, -0.7998128361456362523 ) ) ;
#105131 = CARTESIAN_POINT ( 'NONE',  ( -5.829079699232685208, 5.765290835385048496, 0.000000000000000000 ) ) ;
#105132 = CARTESIAN_POINT ( 'NONE',  ( -10.76112648294250462, 4.189587671054875173, 6.709456861673908534 ) ) ;
#105133 = ORIENTED_EDGE ( 'NONE', *, *, #201199, .T. ) ;
#105134 = CARTESIAN_POINT ( 'NONE',  ( 6.227427239534573999, -1.941376443541954488, 0.6920112976290059281 ) ) ;
#105135 = CARTESIAN_POINT ( 'NONE',  ( -6.983858524370814003, 9.241197259889665006, 1.443375672974064550 ) ) ;
#105136 = CARTESIAN_POINT ( 'NONE',  ( -1.500000000000001110, 11.80208333401612997, 0.8660254037844418162 ) ) ;
#105137 = CARTESIAN_POINT ( 'NONE',  ( -1.162044386198238738E-15, 2.937500000000009326, -1.225000000000010525 ) ) ;
#105138 = CARTESIAN_POINT ( 'NONE',  ( -8.676328237741483207, 12.20980114641871062, -1.199719254218446718 ) ) ;
#105139 = CARTESIAN_POINT ( 'NONE',  ( 5.233071810066631357, 1.866936204443689462, 0.7709723521613828234 ) ) ;
#105141 = ORIENTED_EDGE ( 'NONE', *, *, #142740, .T. ) ;
#105140 = CARTESIAN_POINT ( 'NONE',  ( 6.270221287042929248, 2.215581787426896376, -0.1604564985231044516 ) ) ;
#105142 = CARTESIAN_POINT ( 'NONE',  ( -5.725286006720766707, 9.901527117808042178, 0.7998128361456291469 ) ) ;
#105143 = CARTESIAN_POINT ( 'NONE',  ( 7.142447996300871793, 7.227277505306155092, 0.7998128361456341429 ) ) ;
#105144 = CARTESIAN_POINT ( 'NONE',  ( 5.137599278355773791, -1.455842209265911569, -1.458961989641535117 ) ) ;
#105145 = CARTESIAN_POINT ( 'NONE',  ( 3.832657856672665009, 0.6767144645295587457, -1.899618369658891748 ) ) ;
#105146 = ORIENTED_EDGE ( 'NONE', *, *, #15931, .F. ) ;
#105147 = CYLINDRICAL_SURFACE ( 'NONE', #24621, 0.3999999999999997446 ) ;
#105148 = CARTESIAN_POINT ( 'NONE',  ( 2.367870383881045981, 5.914265881169853856, 0.000000000000000000 ) ) ;
#105150 = EDGE_LOOP ( 'NONE', ( #151990, #76634, #145780, #54395, #105019, #177993, #5335, #87354, #17446, #38638, #83444, #150729, #30681 ) ) ;
#105149 = CARTESIAN_POINT ( 'NONE',  ( -6.282224075085783177, 8.422623735723785643, 1.599625672291269396 ) ) ;
#105151 = CARTESIAN_POINT ( 'NONE',  ( 5.880365472892705725, 7.167286867907723291, -1.140585135024022811 ) ) ;
#105152 = CARTESIAN_POINT ( 'NONE',  ( 4.534529724472468715, 1.956261425488527106, -0.4871295050740409582 ) ) ;
#105153 = CARTESIAN_POINT ( 'NONE',  ( 3.503688343963583307, -0.7473321665184139428, -1.682825604429179833 ) ) ;
#105154 = EDGE_CURVE ( 'NONE', #72609, #205917, #79822, .T. ) ;
#105155 = CARTESIAN_POINT ( 'NONE',  ( -3.023105066167323329, 5.702484939155337607, -2.500000000000000444 ) ) ;
#105156 = CARTESIAN_POINT ( 'NONE',  ( 2.034188542434863578, -1.509292173632442280, -1.745791301847523513 ) ) ;
#105157 = CARTESIAN_POINT ( 'NONE',  ( 4.573896719763862251, 6.429575154514868274, -1.599625672291273171 ) ) ;
#105158 = CARTESIAN_POINT ( 'NONE',  ( 4.183022562662654487, -0.2072598778708051315, -2.151613130492259440 ) ) ;
#105159 = CARTESIAN_POINT ( 'NONE',  ( 6.598014311344812199, 10.84943379654430906, 1.040834085586084257E-14 ) ) ;
#105160 = CARTESIAN_POINT ( 'NONE',  ( -5.545448523189368650, 6.428443684264421698, -1.199719254218446718 ) ) ;
#105161 = CARTESIAN_POINT ( 'NONE',  ( 3.462589497157672724, 1.809959297682335100, 1.416443637550690804 ) ) ;
#105162 = CARTESIAN_POINT ( 'NONE',  ( -0.7499999999999972244, 4.139583334016149863, -1.299038105676652899 ) ) ;
#105163 = CARTESIAN_POINT ( 'NONE',  ( 2.500682550815761740, 1.503739811390795378, -1.112508705057350999 ) ) ;
#105164 = CARTESIAN_POINT ( 'NONE',  ( 0.2277241186354854174, -1.209499947282626220, -1.557479245376863330 ) ) ;
#105167 = ADVANCED_FACE ( 'NONE', ( #69244 ), #14998, .T. ) ;
#105166 = CARTESIAN_POINT ( 'NONE',  ( -5.901542003698421190, 10.10715911428198055, 0.000000000000000000 ) ) ;
#105165 = CARTESIAN_POINT ( 'NONE',  ( -0.6823417656250212460, 5.051041667008086655, 1.181850606188767472 ) ) ;
#105169 = CARTESIAN_POINT ( 'NONE',  ( 1.629795212970772456, -2.077151576879713080, 0.7458654493318407352 ) ) ;
#105168 = CARTESIAN_POINT ( 'NONE',  ( -6.274726165026268454, 6.214935368819085149, 0.7998128361456341429 ) ) ;
#105170 = ORIENTED_EDGE ( 'NONE', *, *, #63569, .F. ) ;
#105171 = PLANE ( 'NONE',  #109323 ) ;
#105172 = CARTESIAN_POINT ( 'NONE',  ( 6.328958779480917229, 6.278206752349526631, 0.7998128361456341429 ) ) ;
#105173 = CARTESIAN_POINT ( 'NONE',  ( -5.436983294280064882, 6.301900917203534291, 1.199719254218450271 ) ) ;
#105174 = CARTESIAN_POINT ( 'NONE',  ( -8.081892667527540652, -5.200000000000006395, 7.462104991928527831 ) ) ;
#105175 = CARTESIAN_POINT ( 'NONE',  ( 6.086792475191005636, -0.2889037430471863566, -1.950060635722290936 ) ) ;
#105176 = EDGE_CURVE ( 'NONE', #202848, #43527, #136426, .T. ) ;
#105177 = CARTESIAN_POINT ( 'NONE',  ( 6.129535273836777876, -2.175136813519952916, 0.7712226964542520102 ) ) ;
#105178 = CARTESIAN_POINT ( 'NONE',  ( 0.6429252097494702056, -0.2364460082661112295, -1.947484529462916836 ) ) ;
#105179 = CARTESIAN_POINT ( 'NONE',  ( 2.834894798709301611, -1.972450601023918448, -0.6029180858937719378 ) ) ;
#105180 = CARTESIAN_POINT ( 'NONE',  ( 6.073689629242148058, 8.109057205581079231, -1.443375672974057666 ) ) ;
#105181 = CARTESIAN_POINT ( 'NONE',  ( 5.993586425693011144, 9.150212042353954800, -1.199719254218452047 ) ) ;
#105182 = CARTESIAN_POINT ( 'NONE',  ( 8.066738210006692000, 8.513542121203711233, 0.7216878364870458196 ) ) ;
#105183 = CARTESIAN_POINT ( 'NONE',  ( -1.201851678989727383E-14, 3.634375000341422357, 1.575800808251672791 ) ) ;
#105184 = DIRECTION ( 'NONE',  ( -0.000000000000000000, -1.000000000000000000, -0.000000000000000000 ) ) ;
#105185 = CARTESIAN_POINT ( 'NONE',  ( 5.680503174001485078, 6.689970460165617361, -1.082531754730543083 ) ) ;
#105186 = CARTESIAN_POINT ( 'NONE',  ( 6.303213947599001443, -1.837614076384209261, 1.156103312670229810 ) ) ;
#105188 = CARTESIAN_POINT ( 'NONE',  ( 4.704558828624370470, 1.604442792107749760, 0.9031527321438773681 ) ) ;
#105187 = FACE_OUTER_BOUND ( 'NONE', #110857, .T. ) ;
#105189 = CARTESIAN_POINT ( 'NONE',  ( 9.532262708098283355, -8.048696291100949196, -0.1899713450103259760 ) ) ;
#105190 = CARTESIAN_POINT ( 'NONE',  ( 6.269083535738129598, 2.097726667780253074, -0.6343229546324488100 ) ) ;
#105191 = DIRECTION ( 'NONE',  ( -0.9999753971658824625, 0.000000000000000000, 0.007014632059889242682 ) ) ;
#105192 = CARTESIAN_POINT ( 'NONE',  ( -4.119138978170663989, 7.660627806941648466, 0.7993094217999627826 ) ) ;
#105193 = LINE ( 'NONE', #84652, #182754 ) ;
#105194 = CARTESIAN_POINT ( 'NONE',  ( 5.966021608595377224, 7.209656400309186530, 1.216315744458285719 ) ) ;
#105195 = CARTESIAN_POINT ( 'NONE',  ( 0.3285747216504387724, 1.318609938922534752, -1.385187620709791512 ) ) ;
#105196 = CARTESIAN_POINT ( 'NONE',  ( 1.779799802231885275, -0.9501279348179264561, 1.492983415055911367 ) ) ;
#105197 = CARTESIAN_POINT ( 'NONE',  ( 0.1176276963383571517, -0.5100272734060510293, 1.842954807014775653 ) ) ;
#105199 = CARTESIAN_POINT ( 'NONE',  ( 3.392102565403580350, -0.7792391910043224845, -1.750150251150209391 ) ) ;
#105198 = CARTESIAN_POINT ( 'NONE',  ( -9.992522908471816123, 11.61669713376064372, 1.199719254218462483 ) ) ;
#105200 = LINE ( 'NONE', #100903, #74446 ) ;
#105201 = CARTESIAN_POINT ( 'NONE',  ( 4.615651692036619735, 0.4336440386765746946, -1.921039654613013292 ) ) ;
#105202 = CARTESIAN_POINT ( 'NONE',  ( 6.539320575229290000, 0.004092658091040673150, 2.003502637948690879 ) ) ;
#105203 = CARTESIAN_POINT ( 'NONE',  ( -3.755772246185468788, 4.340488027759846545, -1.199719254218452047 ) ) ;
#105204 = CARTESIAN_POINT ( 'NONE',  ( 3.238977024203249400, -1.650389259550872456, 0.8806316622528218563 ) ) ;
#105206 = ORIENTED_EDGE ( 'NONE', *, *, #168035, .F. ) ;
#105205 = CARTESIAN_POINT ( 'NONE',  ( 6.357991264096761519, 1.719682601729131566, -0.1347253291539267650 ) ) ;
#105208 = CARTESIAN_POINT ( 'NONE',  ( 3.145128448690309053, 4.692402494937224056, -1.443375672974057666 ) ) ;
#105207 = CARTESIAN_POINT ( 'NONE',  ( 1.787996309160574837, 1.523479866092191548, 1.596893430481533649 ) ) ;
#105209 = CARTESIAN_POINT ( 'NONE',  ( 1.364683531249988535, 3.717708333674750953, -0.7879004041258239610 ) ) ;
#105210 = CARTESIAN_POINT ( 'NONE',  ( 0.2036765287981847083, -1.593398458586914757, -1.309455759714562850 ) ) ;
#105211 = CARTESIAN_POINT ( 'NONE',  ( 7.070740804726770357, 8.207951346058097286, 1.199719254218462483 ) ) ;
#105212 = CARTESIAN_POINT ( 'NONE',  ( -6.849482339516217877, -6.938199013094648038, 6.234224025626350141 ) ) ;
#105213 = DIRECTION ( 'NONE',  ( 0.000000000000000000, 1.000000000000000000, 0.000000000000000000 ) ) ;
#105214 = CARTESIAN_POINT ( 'NONE',  ( -3.795392936821753604, 6.515376628678959392, -1.199719254218452047 ) ) ;
#105215 = CARTESIAN_POINT ( 'NONE',  ( -7.834948813059765094, -6.306565840633504116, -7.720982910014320133 ) ) ;
#105216 = EDGE_LOOP ( 'NONE', ( #167295, #78748, #87281, #168856 ) ) ;
#105217 = CARTESIAN_POINT ( 'NONE',  ( 2.734898984476673789, -1.980466496001157317, -0.6033880717724803278 ) ) ;
#105218 = CARTESIAN_POINT ( 'NONE',  ( 0.7499999999999902300, 4.566666666666691299, -1.299038105676658228 ) ) ;
#105219 = CARTESIAN_POINT ( 'NONE',  ( 3.960953433486789521, 7.772862772376584850, -0.7998128361456221525 ) ) ;
#105220 = CARTESIAN_POINT ( 'NONE',  ( -6.419388467533182485, 6.810688026658763938, -0.4840902626340077841 ) ) ;
#105221 = CARTESIAN_POINT ( 'NONE',  ( 0.8561247329088355063, 0.8163843618401511737, -1.847503835822896789 ) ) ;
#105222 = DIRECTION ( 'NONE',  ( 0.000000000000000000, 8.546850786086437571E-32, 1.000000000000000000 ) ) ;
#105223 = CARTESIAN_POINT ( 'NONE',  ( 1.364683531249988535, 4.363541667008090208, 0.7879004041258500513 ) ) ;
#105224 = ORIENTED_EDGE ( 'NONE', *, *, #68596, .T. ) ;
#105226 = CARTESIAN_POINT ( 'NONE',  ( 9.910647101909615841, 10.66476916175714607, 0.000000000000000000 ) ) ;
#105225 = CARTESIAN_POINT ( 'NONE',  ( 0.1747926744264677590, 6.948552888299643904, -2.450368216405907962 ) ) ;
#105227 = CARTESIAN_POINT ( 'NONE',  ( 5.554064478179312481, 1.779353385700060075, -0.9478964821433707444 ) ) ;
#105228 = CARTESIAN_POINT ( 'NONE',  ( 5.436718845459293625, -1.505851745483515858, 1.184076087961029700 ) ) ;
#105229 = FACE_OUTER_BOUND ( 'NONE', #181497, .T. ) ;
#105230 = CARTESIAN_POINT ( 'NONE',  ( 3.984055765753656164, -2.167877601896048390, -0.3204034371554059235 ) ) ;
#105231 = CARTESIAN_POINT ( 'NONE',  ( 1.499999999999987121, 2.327083334016154303, -0.8660254037844262731 ) ) ;
#105232 = CARTESIAN_POINT ( 'NONE',  ( 2.179812656587180264, 1.874749209517186710, -0.3766967574026017229 ) ) ;
#105233 = CARTESIAN_POINT ( 'NONE',  ( -5.032047568966410367, 9.022472597102808578, 1.214306433183764966E-14 ) ) ;
#105234 = CARTESIAN_POINT ( 'NONE',  ( 5.490689023410166847, 5.508151403507724808, -0.7216878364870207285 ) ) ;
#105236 = CARTESIAN_POINT ( 'NONE',  ( 0.5972800738224989248, -0.2930464221381040013, 1.994874516246990748 ) ) ;
#105235 =( LENGTH_UNIT ( ) NAMED_UNIT ( * ) SI_UNIT ( .MILLI., .METRE. ) );
#105238 = ADVANCED_FACE ( 'NONE', ( #148411 ), #199250, .T. ) ;
#105237 = CARTESIAN_POINT ( 'NONE',  ( -8.012344526598182026E-15, 11.10937500034139802, -1.575800808251669460 ) ) ;
#105240 = CARTESIAN_POINT ( 'NONE',  ( -4.945692173934974178, 8.992000979557944973, 0.000000000000000000 ) ) ;
#105239 = CARTESIAN_POINT ( 'NONE',  ( 5.917560222199001352, -1.216239291071326001, -1.822900893127032962 ) ) ;
#105242 = VERTEX_POINT ( 'NONE', #84455 ) ;
#105241 = CARTESIAN_POINT ( 'NONE',  ( 2.783889825318270450, -0.8885198777363271239, 1.478144978849999847 ) ) ;
#105243 = SURFACE_STYLE_FILL_AREA ( #187529 ) ;
#105244 = CARTESIAN_POINT ( 'NONE',  ( 6.958359152311676787, 9.141171649162195934, -1.599625672291262513 ) ) ;
#105245 = CARTESIAN_POINT ( 'NONE',  ( 5.508690485854129903, 5.321227076451600091, 1.040834085586084257E-14 ) ) ;
#105246 = CARTESIAN_POINT ( 'NONE',  ( -1.335881052060646557, 13.37576698399828423, -0.3319583403691591106 ) ) ;
#105247 = CARTESIAN_POINT ( 'NONE',  ( 0.1390251588108057101, -0.1389306544097475005, -1.930426113910483688 ) ) ;
#105248 = CARTESIAN_POINT ( 'NONE',  ( 6.980013479859856318, -8.233136965322191969, -6.444907381559382031 ) ) ;
#105249 = CARTESIAN_POINT ( 'NONE',  ( 6.193377243344257543, 6.120028293523423812, -0.7998128361456281477 ) ) ;
#105250 = CARTESIAN_POINT ( 'NONE',  ( 2.026920941591049630, 3.691791674785623201, -11.39597588158938990 ) ) ;
#105251 = ORIENTED_EDGE ( 'NONE', *, *, #112850, .F. ) ;
#105252 = CARTESIAN_POINT ( 'NONE',  ( -3.673896439623323129, 4.156855427197417185, 1.000000000000009548 ) ) ;
#105253 = VERTEX_POINT ( 'NONE', #198193 ) ;
#105254 = CARTESIAN_POINT ( 'NONE',  ( 4.107922266221023300, -0.6895048676278795474, 1.675321109400946806 ) ) ;
#105255 = EDGE_LOOP ( 'NONE', ( #85746, #117314 ) ) ;
#105256 = CARTESIAN_POINT ( 'NONE',  ( 8.866142388332804103, 12.43125098877526113, -1.199719254218446718 ) ) ;
#105257 = CARTESIAN_POINT ( 'NONE',  ( 3.790386463472274148, 6.579812086429759788, 1.199719254218452047 ) ) ;
#105258 = CARTESIAN_POINT ( 'NONE',  ( 3.791515551631476910, 1.704436734775734985, -0.6137984976519753610 ) ) ;
#105259 = CARTESIAN_POINT ( 'NONE',  ( 6.170369307550806148, 10.21286493553572328, 0.7216878364870317197 ) ) ;
#105260 = CARTESIAN_POINT ( 'NONE',  ( 5.098048262872540981, 4.912420826298216525, -0.06541299864657826313 ) ) ;
#105261 = CARTESIAN_POINT ( 'NONE',  ( 5.740253418993177981, 6.070215967746060315, 0.6401420356763661834 ) ) ;
#105263 = CARTESIAN_POINT ( 'NONE',  ( -1.364683531250000748, 14.10937500034140157, 0.000000000000000000 ) ) ;
#105262 = CARTESIAN_POINT ( 'NONE',  ( 4.826513810146395578, -1.216237885654298800, 1.408704720340781869 ) ) ;
#105264 = ADVANCED_FACE ( 'NONE', ( #73530 ), #65038, .T. ) ;
#105265 = CARTESIAN_POINT ( 'NONE',  ( 3.110843951327123325, 0.04995152196871639055, 1.915135415325731394 ) ) ;
#105266 = STYLED_ITEM ( 'NONE', ( #98421 ), #116367 ) ;
#105267 = FACE_OUTER_BOUND ( 'NONE', #13561, .T. ) ;
#105268 = CARTESIAN_POINT ( 'NONE',  ( -10.71026998871754721, 6.055660674263378951, 4.667787751035539223 ) ) ;
#105269 = DIRECTION ( 'NONE',  ( -5.551115123125764829E-17, 0.000000000000000000, 1.000000000000000000 ) ) ;
#105270 = SPHERICAL_SURFACE ( 'NONE', #108647, 0.08000000000000000167 ) ;
#105271 = AXIS2_PLACEMENT_3D ( 'NONE', #71054, #68921, #133993 ) ;
#105272 = CARTESIAN_POINT ( 'NONE',  ( 7.131225611108096274, 8.382479970123348778, 1.082531754730558626 ) ) ;
#105273 = CARTESIAN_POINT ( 'NONE',  ( -2.916975605234527702, 6.554888639415577423, 1.040834085586084257E-14 ) ) ;
#105274 =( NAMED_UNIT ( * ) PLANE_ANGLE_UNIT ( ) SI_UNIT ( $, .RADIAN. ) );
#105275 = CARTESIAN_POINT ( 'NONE',  ( 1.623107816722869412, -1.968041427791475728, 0.7057566781872460782 ) ) ;
#105276 = CARTESIAN_POINT ( 'NONE',  ( 6.852720297064418986, 6.959538199522133262, 0.7998128361456331437 ) ) ;
#105277 = CARTESIAN_POINT ( 'NONE',  ( 6.510771785681003010, 1.426997308145862453, -1.294280627073117529 ) ) ;
#105278 = CARTESIAN_POINT ( 'NONE',  ( -3.567766978690493307, 7.314145241780881435, 1.040834085586084257E-14 ) ) ;
#105279 = CARTESIAN_POINT ( 'NONE',  ( 2.010518257881420023, 1.354885872097401078, -1.223726681998098087 ) ) ;
#105280 = CARTESIAN_POINT ( 'NONE',  ( 1.506454395378247121E-16, 4.400000000000001243, 2.250000000000000000 ) ) ;
#105281 = CARTESIAN_POINT ( 'NONE',  ( 0.8438408207818194340, -1.215224102361469161, -1.476598726422105656 ) ) ;
#105282 = B_SPLINE_CURVE_WITH_KNOTS ( 'NONE', 3,
 ( #133796, #119705, #199805, #2656 ),
 .UNSPECIFIED., .F., .F.,
 ( 4, 4 ),
 ( 0.000000000000000000, 6.033646489354555479E-05 ),
 .UNSPECIFIED. ) ;
#105283 = CARTESIAN_POINT ( 'NONE',  ( 1.662492070209736994, -0.7059575147525645189, -1.838877744480153620 ) ) ;
#105284 = CARTESIAN_POINT ( 'NONE',  ( 3.895986966309549882, -0.6120611862858457153, -1.843141947886927978 ) ) ;
#105285 = EDGE_LOOP ( 'NONE', ( #104032, #93184, #94869, #136140 ) ) ;
#105286 = CARTESIAN_POINT ( 'NONE',  ( 3.160134022698241729, 2.806877976488725501, 2.466440901444043377 ) ) ;
#105288 = CARTESIAN_POINT ( 'NONE',  ( 6.034019871906543209, 1.107478494666002344, 1.495390754572333725 ) ) ;
#105287 = CARTESIAN_POINT ( 'NONE',  ( -5.167592825464113915, 6.057888380243431570, 1.199719254218452935 ) ) ;
#105290 = CARTESIAN_POINT ( 'NONE',  ( 3.691739789689612472, 1.995538565534977549, -0.7177698711837015022 ) ) ;
#105289 = CARTESIAN_POINT ( 'NONE',  ( 3.223806664999388172, 6.983134552466421674, -0.7998128361456362523 ) ) ;
#105291 = CARTESIAN_POINT ( 'NONE',  ( 0.3602790413719210716, -9.063128419003717795, -9.630430012830139219 ) ) ;
#105292 = CARTESIAN_POINT ( 'NONE',  ( 7.723341061279088038, 12.16231500480096983, -0.7998128361456291469 ) ) ;
#105293 = CARTESIAN_POINT ( 'NONE',  ( -6.099189001301292379, 8.209082816308541197, 1.599625672291263179 ) ) ;
#105294 = SURFACE_STYLE_FILL_AREA ( #72758 ) ;
#105295 = ORIENTED_EDGE ( 'NONE', *, *, #123377, .F. ) ;
#105296 = CARTESIAN_POINT ( 'NONE',  ( 4.877901405866606588, 8.912911750144889567, 0.7998128361456341429 ) ) ;
#105297 = CARTESIAN_POINT ( 'NONE',  ( 11.33772463945037146, 10.89999999999998259, 3.599999999999999201 ) ) ;
#105298 = CARTESIAN_POINT ( 'NONE',  ( 3.492628380820805400, -0.3572889717703279788, -1.790209119249221548 ) ) ;
#105299 = CARTESIAN_POINT ( 'NONE',  ( 3.497640442201256139, 7.024404915969360452, 1.040834085586084257E-14 ) ) ;
#105300 = CARTESIAN_POINT ( 'NONE',  ( -9.083599731475995753, 11.62061899152058686, 1.443375672974064550 ) ) ;
#105301 = CARTESIAN_POINT ( 'NONE',  ( -4.702355942707336034, 8.355867970554191615, 0.6817663069898479700 ) ) ;
#105302 = CARTESIAN_POINT ( 'NONE',  ( -11.94105721237523099, 12.69999999999999929, -1.187919463087249827 ) ) ;
#105303 = CARTESIAN_POINT ( 'NONE',  ( 4.170664822833985319, -1.745344833062393075, -0.6735866001992969476 ) ) ;
#105304 = CARTESIAN_POINT ( 'NONE',  ( 7.065770611016287006, 11.39514947949436774, 1.040834085586084257E-14 ) ) ;
#105305 = CARTESIAN_POINT ( 'NONE',  ( 1.646969920108354524, -1.627708819445686572, 1.030247865989121880 ) ) ;
#105306 = CARTESIAN_POINT ( 'NONE',  ( 6.772321408939014020, -0.9219223515295159599, -1.731591420108986812 ) ) ;
#105307 = CARTESIAN_POINT ( 'NONE',  ( 0.6823417656249934904, 9.255208333674728394, 1.181850606188764807 ) ) ;
#105308 = CARTESIAN_POINT ( 'NONE',  ( -5.605406444246153974, 8.627059054007450101, -1.199719254218440723 ) ) ;
#105309 = CARTESIAN_POINT ( 'NONE',  ( 4.955668840994886359, 5.740367388370866131, 1.199719254218462483 ) ) ;
#105310 = ADVANCED_FACE ( 'NONE', ( #153729, #122388 ), #6382, .F. ) ;
#105311 = CARTESIAN_POINT ( 'NONE',  ( -3.960390268523300339, 7.634556056670224855, 1.214306433183764966E-14 ) ) ;
#105312 = CARTESIAN_POINT ( 'NONE',  ( -0.0001774970986804374768, -2.075397304607224047, 0.4179963677126071753 ) ) ;
#105313 = AXIS2_PLACEMENT_3D ( 'NONE', #128132, #162686, #123074 ) ;
#105314 = CARTESIAN_POINT ( 'NONE',  ( 9.673906298550626559, 11.24497775551929557, 1.199719254218452047 ) ) ;
#105315 = CARTESIAN_POINT ( 'NONE',  ( 11.92619526913700057, 13.52781666661241466, 1.328859060402684644 ) ) ;
#105316 = CARTESIAN_POINT ( 'NONE',  ( 4.733297664174529906, 0.005294743050891088411, -2.070434559870132585 ) ) ;
#105319 = B_SPLINE_CURVE_WITH_KNOTS ( 'NONE', 3,
 ( #54236, #34765, #4376, #68321 ),
 .UNSPECIFIED., .F., .F.,
 ( 4, 4 ),
 ( 0.000000000000000000, 8.505390838612172152E-05 ),
 .UNSPECIFIED. ) ;
#105318 = CARTESIAN_POINT ( 'NONE',  ( -1.364683531249997417, 3.071875000341423245, 1.214306433183764966E-14 ) ) ;
#105317 = CARTESIAN_POINT ( 'NONE',  ( 0.4328342922346357646, -1.301571265828086688, -1.302605208699902928 ) ) ;
#105320 = CARTESIAN_POINT ( 'NONE',  ( 5.010469735608720221, -2.183386834666663390, 0.7190086036765501731 ) ) ;
#105321 = CARTESIAN_POINT ( 'NONE',  ( 5.653386867218496370, 9.539442411822841805, 1.040834085586084257E-14 ) ) ;
#105323 = DIRECTION ( 'NONE',  ( 0.000000000000000000, 1.000000000000000000, -3.330669073875479482E-16 ) ) ;
#105322 = CARTESIAN_POINT ( 'NONE',  ( 4.421367491832270957, 6.251624388594711590, 1.443375672974058777 ) ) ;
#105324 = CARTESIAN_POINT ( 'NONE',  ( 0.8675860333910101474, 2.207824459889203172, -0.6162223019612712571 ) ) ;
#105325 = CARTESIAN_POINT ( 'NONE',  ( 5.026762865062591068, 4.898582544318342613, 0.2131414487870288976 ) ) ;
#105326 = CARTESIAN_POINT ( 'NONE',  ( -7.286581212701773502, 7.465709267765667789, 0.7998128361456341429 ) ) ;
#105327 = CARTESIAN_POINT ( 'NONE',  ( 4.470608273529505183, -0.001430698596973853159, -1.942124712226586558 ) ) ;
#105328 = VERTEX_POINT ( 'NONE', #104993 ) ;
#105330 = CARTESIAN_POINT ( 'NONE',  ( 7.253248993186720561, 10.44557901115111065, 1.082531754730558626 ) ) ;
#105329 = CIRCLE ( 'NONE', #167602, 10.25000000000000000 ) ;
#105331 = EDGE_LOOP ( 'NONE', ( #147594, #93494, #86324, #153113 ) ) ;
#105332 = CARTESIAN_POINT ( 'NONE',  ( 6.011958326525193463, -0.6379227081053112647, 1.803018720113582773 ) ) ;
#105333 = CARTESIAN_POINT ( 'NONE',  ( 5.964077395145577221, -1.074666730956087335, 1.706109649615504154 ) ) ;
#105335 = CARTESIAN_POINT ( 'NONE',  ( -1.386567914617467867, 8.090296256147714971, -10.72428812184711511 ) ) ;
#105334 = CARTESIAN_POINT ( 'NONE',  ( -9.154780037725563702, 11.70366268214508487, 1.599625672291281386 ) ) ;
#105336 = CARTESIAN_POINT ( 'NONE',  ( -3.285556943749998737, -0.8677083328553740760, 1.896917185911908499 ) ) ;
#105338 = CARTESIAN_POINT ( 'NONE',  ( 0.7777615046654516862, -0.9880915000441170548, 1.468120464595161989 ) ) ;
#105337 = CARTESIAN_POINT ( 'NONE',  ( 2.484421436082083101, -0.3582009261528392163, -2.059553721446294894 ) ) ;
#105339 = CARTESIAN_POINT ( 'NONE',  ( 11.33772463945037146, 10.09088423488572062, 3.599999999999998757 ) ) ;
#105341 = CARTESIAN_POINT ( 'NONE',  ( 4.681715291062889861, -1.083280430520225046, 2.020132927424389102 ) ) ;
#105340 = CARTESIAN_POINT ( 'NONE',  ( 4.947799714344386146, 4.737130853015369958, -0.7998128361456481317 ) ) ;
#105342 = CARTESIAN_POINT ( 'NONE',  ( 1.833560160614732704, 1.721085009045751901, 0.2571270737643116533 ) ) ;
#105343 = ADVANCED_FACE ( 'NONE', ( #139633 ), #37170, .T. ) ;
#105344 = CARTESIAN_POINT ( 'NONE',  ( 4.111146893441827821, 5.819424013814004759, 1.599625672291267398 ) ) ;
#105345 = CARTESIAN_POINT ( 'NONE',  ( 5.387385936583817703, 7.378645907471495846, -1.599625672291283607 ) ) ;
#105346 = CARTESIAN_POINT ( 'NONE',  ( 2.073226780758777643, 1.288078611216292302, -1.160843940205048774 ) ) ;
#105347 = CARTESIAN_POINT ( 'NONE',  ( -1.360316468750018659, 2.401041667008069425, -0.7853790794159061228 ) ) ;
#105348 = CARTESIAN_POINT ( 'NONE',  ( 1.767777038385684785, -1.847514956963384414, 0.2233714002321494363 ) ) ;
#105349 = CARTESIAN_POINT ( 'NONE',  ( 1.961612892103332229, 1.804449789391232795, 1.207184914618843807 ) ) ;
#105350 = CARTESIAN_POINT ( 'NONE',  ( 6.498435699651741615, 6.475929825882159818, -0.7998128361456281477 ) ) ;
#105351 = CARTESIAN_POINT ( 'NONE',  ( 4.663296154398564042, 1.879804967172087782, -0.7303043177912388328 ) ) ;
#105352 = CARTESIAN_POINT ( 'NONE',  ( 3.281250000000002665, 0.7852924748301588487, 1.895863743164012849 ) ) ;
#105353 = CARTESIAN_POINT ( 'NONE',  ( -1.500000000000013101, 3.410416667349487785, -0.8660254037844313801 ) ) ;
#105354 = CARTESIAN_POINT ( 'NONE',  ( 1.043825456435763410, 0.7835056195745603302, -1.760039731681047215 ) ) ;
#105355 = CARTESIAN_POINT ( 'NONE',  ( -1.364683531250014514, 13.83854166700806765, -0.7879004041258335089 ) ) ;
#105356 = CARTESIAN_POINT ( 'NONE',  ( 4.869482922584397855, -1.877140712267670430, -1.187567259214457271 ) ) ;
#105357 = ORIENTED_EDGE ( 'NONE', *, *, #182948, .F. ) ;
#105358 = CARTESIAN_POINT ( 'NONE',  ( -0.2110808730067300354, 7.629137130509040077, -2.397154524934116182 ) ) ;
#105359 = CARTESIAN_POINT ( 'NONE',  ( -1.500000000000001332, 0.6500000000000255573, 0.000000000000000000 ) ) ;
#105360 = CARTESIAN_POINT ( 'NONE',  ( 6.076025397218672630, 10.24044673006381245, -0.7998128361456291469 ) ) ;
#105361 = EDGE_CURVE ( 'NONE', #86356, #199688, #138553, .T. ) ;
#105362 = CARTESIAN_POINT ( 'NONE',  ( 1.364683531249986537, -0.1364583329919154264, 0.7879004041258500513 ) ) ;
#105363 = CARTESIAN_POINT ( 'NONE',  ( 0.1533981569187261029, 0.3862642299664406642, 2.187325829255863940 ) ) ;
#105364 = CARTESIAN_POINT ( 'NONE',  ( 5.283633159863808437, -1.863482887291990409, 0.6137318589548645953 ) ) ;
#105365 = CARTESIAN_POINT ( 'NONE',  ( 8.107412671292022921, 12.40247251657532956, 0.7216878364870438212 ) ) ;
#105366 = CARTESIAN_POINT ( 'NONE',  ( -1.354873262373948339, 3.923680654322774686, -0.6436764175676684685 ) ) ;
#105367 = CARTESIAN_POINT ( 'NONE',  ( 0.1811626231076196580, -0.1537715369321658587, -2.127283700313627346 ) ) ;
#105368 = CLOSED_SHELL ( 'NONE', ( #29079, #151949 ) ) ;
#105369 = CARTESIAN_POINT ( 'NONE',  ( -5.207740401424942434, 6.208690235484773723, 1.082531754730549078 ) ) ;
#105370 = CARTESIAN_POINT ( 'NONE',  ( 3.244635591053147916, -2.031700879476082466, -0.3553325473293292847 ) ) ;
#105371 = CARTESIAN_POINT ( 'NONE',  ( -5.717788096661253761, 7.693838750903348789, 1.599625672291269396 ) ) ;
#105372 = CARTESIAN_POINT ( 'NONE',  ( -1.500000000000011324, 2.952083334016149418, 0.8660254037844403729 ) ) ;
#105373 = CARTESIAN_POINT ( 'NONE',  ( 1.364683531249990311, 4.946875000341417916, 1.214306433183764966E-14 ) ) ;
#105374 = CARTESIAN_POINT ( 'NONE',  ( 5.342975940791072631, -1.604858128155508101, 0.9606422304059699657 ) ) ;
#105375 = CARTESIAN_POINT ( 'NONE',  ( 3.691823404346205706, 1.489760995587570358, 0.8873103889329400085 ) ) ;
#105376 = CARTESIAN_POINT ( 'NONE',  ( 3.596946774904510757, -0.5014486528964605672, 1.666646126512297821 ) ) ;
#105377 = CARTESIAN_POINT ( 'NONE',  ( 1.312523894619976650, 1.535058519010788602, -1.702700526841523399 ) ) ;
#105378 = CARTESIAN_POINT ( 'NONE',  ( -0.6823417656249969321, 4.030208333674754506, -1.181850606188749264 ) ) ;
#105379 = CARTESIAN_POINT ( 'NONE',  ( 4.212501570603551571, 1.912301062189927015, 0.8455808105151915166 ) ) ;
#105380 = CARTESIAN_POINT ( 'NONE',  ( 5.929623787841700633, 0.9553189508899215809, -1.690649115374833311 ) ) ;
#105381 = EDGE_CURVE ( 'NONE', #133382, #180856, #74508, .T. ) ;
#105383 = ORIENTED_EDGE ( 'NONE', *, *, #189331, .F. ) ;
#105382 = CARTESIAN_POINT ( 'NONE',  ( 8.739888343381572611, 14.93516617432513982, 8.229140924179734640 ) ) ;
#105384 = CARTESIAN_POINT ( 'NONE',  ( 1.037732671793228700, -1.587836052788630603, 1.242728777923551409 ) ) ;
#105385 = CARTESIAN_POINT ( 'NONE',  ( 0.5805319366703353134, 1.050441701016215923, 1.842106252469346117 ) ) ;
#105386 = FILL_AREA_STYLE ('',( #7840 ) ) ;
#105387 = CARTESIAN_POINT ( 'NONE',  ( 6.311172677262812059, 1.158691452862798954, -1.650079838712660063 ) ) ;
#105388 = CARTESIAN_POINT ( 'NONE',  ( -9.176171038350775078, 9.599954387697719582, -0.7998128361456291469 ) ) ;
#105389 = CARTESIAN_POINT ( 'NONE',  ( 4.645640190976921602, 8.571663989448405019, 1.040834085586084257E-14 ) ) ;
#105390 = CARTESIAN_POINT ( 'NONE',  ( 2.824977599723184074, 1.534285384246200090, -1.463936014953904463 ) ) ;
#105391 = CARTESIAN_POINT ( 'NONE',  ( 4.125493313500066428, -1.746467973620144942, 0.5319596651164605339 ) ) ;
#105392 = ORIENTED_EDGE ( 'NONE', *, *, #41220, .F. ) ;
#105393 = CARTESIAN_POINT ( 'NONE',  ( -3.146901051703345331, 6.685485303713597283, 0.000000000000000000 ) ) ;
#105394 = AXIS2_PLACEMENT_3D ( 'NONE', #31500, #198227, #130138 ) ;
#105395 = UNCERTAINTY_MEASURE_WITH_UNIT (LENGTH_MEASURE( 1.000000000000000082E-05 ), #20061, 'distance_accuracy_value', 'NONE');
#105396 = CARTESIAN_POINT ( 'NONE',  ( -0.1980946632348522529, -8.057097448493959035, -9.531438498077047683 ) ) ;
#105397 = CARTESIAN_POINT ( 'NONE',  ( -1.642778471875000035, -0.2552083328553750308, -2.845375778867859751 ) ) ;
#105398 = CARTESIAN_POINT ( 'NONE',  ( -7.019370843573183194, 9.212351955633947043, 1.599625672291283607 ) ) ;
#105399 = CARTESIAN_POINT ( 'NONE',  ( 2.408468576312505771, -2.014670991514801113, -0.1442217307643048063 ) ) ;
#105400 = CARTESIAN_POINT ( 'NONE',  ( 5.456176519787153012, 2.204477245749701719, -0.1032804940204190558 ) ) ;
#105401 = CARTESIAN_POINT ( 'NONE',  ( -4.339491684825780737, 7.220434844675483355, -1.199719254218455378 ) ) ;
#105402 = CARTESIAN_POINT ( 'NONE',  ( 3.449909520549806707, -0.7582208578979282576, 1.699682486939468440 ) ) ;
#105403 = CARTESIAN_POINT ( 'NONE',  ( 2.758194185376297902, 5.305311418659259814, 1.199719254218452047 ) ) ;
#105404 = DIRECTION ( 'NONE',  ( 0.000000000000000000, 0.000000000000000000, -1.000000000000000000 ) ) ;
#105405 = ORIENTED_EDGE ( 'NONE', *, *, #24501, .F. ) ;
#105406 = EDGE_LOOP ( 'NONE', ( #81806, #110666, #27893, #55850, #92496 ) ) ;
#105407 = CARTESIAN_POINT ( 'NONE',  ( -4.253507506385335368, 5.985511395581417204, 1.599625672291267398 ) ) ;
#105408 = CARTESIAN_POINT ( 'NONE',  ( -7.296259222448620463, 11.66405285949874759, 0.7998128361456481317 ) ) ;
#105409 = CARTESIAN_POINT ( 'NONE',  ( 4.617693566336190436, -1.789886777702164089, 0.3589094947460610974 ) ) ;
#105411 = CARTESIAN_POINT ( 'NONE',  ( -4.712932107567791462, 7.040231785572885315, -1.411385885297003373 ) ) ;
#105410 = CARTESIAN_POINT ( 'NONE',  ( -5.178288325776719603, 5.006034233019745372, 0.000000000000000000 ) ) ;
#105412 = CARTESIAN_POINT ( 'NONE',  ( 6.606590233575550641, 6.765807905838774339, 0.03828827652692379235 ) ) ;
#105413 = CARTESIAN_POINT ( 'NONE',  ( 1.071195256775770543, 1.317505809736085665, -1.127239923523750909 ) ) ;
#105414 = CARTESIAN_POINT ( 'NONE',  ( 0.5150585655138568697, -0.9269755740852363424, -1.472709990541859693 ) ) ;
#105415 = CARTESIAN_POINT ( 'NONE',  ( 5.303480822065511191, 1.883932040028640786, 1.332532017187069817 ) ) ;
#105416 = CARTESIAN_POINT ( 'NONE',  ( 3.393283585170187688, 7.180857625999046867, 0.7998128361456271485 ) ) ;
#105417 = CARTESIAN_POINT ( 'NONE',  ( 6.784453917077649443, -2.118420112955111456, -0.4290502581522498415 ) ) ;
#105418 = CARTESIAN_POINT ( 'NONE',  ( 6.063521013809720195, 8.097193820909906137, 1.599625672291281386 ) ) ;
#105419 = CARTESIAN_POINT ( 'NONE',  ( 5.905696578591778767, 0.4397782949263558949, 2.255800006528754675 ) ) ;
#105420 = CARTESIAN_POINT ( 'NONE',  ( -1.159304781898771619, -3.232243495192086424, 3.077805119331097572 ) ) ;
#105422 = AXIS2_PLACEMENT_3D ( 'NONE', #115197, #49077, #181190 ) ;
#105421 = CARTESIAN_POINT ( 'NONE',  ( -5.912237504011027767, 9.055304967058290799, 1.199719254218454489 ) ) ;
#105423 = CARTESIAN_POINT ( 'NONE',  ( 6.280143113937574739, -0.9989825818290422044, 1.581392243879369053 ) ) ;
#105424 =( GEOMETRIC_REPRESENTATION_CONTEXT ( 3 ) GLOBAL_UNCERTAINTY_ASSIGNED_CONTEXT ( ( #167474 ) ) GLOBAL_UNIT_ASSIGNED_CONTEXT ( ( #30665, #62088, #129314 ) ) REPRESENTATION_CONTEXT ( 'NONE', 'WORKASPACE' ) );
#105427 = ADVANCED_FACE ( 'NONE', ( #8529 ), #206728, .F. ) ;
#105426 = CARTESIAN_POINT ( 'NONE',  ( -2.810282979782591006, 6.500690253046801814, 0.000000000000000000 ) ) ;
#105425 = CARTESIAN_POINT ( 'NONE',  ( 3.006014587165442453, -0.7710369221427433306, 1.750240277048662030 ) ) ;
#105428 = CARTESIAN_POINT ( 'NONE',  ( 4.969440760808212509, 0.2186952961555181096, -2.196011921426939129 ) ) ;
#105429 = CARTESIAN_POINT ( 'NONE',  ( 5.067619284625084930, 1.424172025040346679, 1.566925857267987832 ) ) ;
#105430 = CARTESIAN_POINT ( 'NONE',  ( 1.224999999999959233, 1.166666667349521624, 0.7072540797572417492 ) ) ;
#105431 = CARTESIAN_POINT ( 'NONE',  ( 6.983263157960366563, 2.446371134953594151, 2.328889586965996905 ) ) ;
#105432 = CARTESIAN_POINT ( 'NONE',  ( 4.706088717274906408, 5.623429937309770921, 1.082531754730549078 ) ) ;
#105433 = CARTESIAN_POINT ( 'NONE',  ( -5.194182247366913252, 7.153241603385088965, 1.443375672974058777 ) ) ;
#105434 = CARTESIAN_POINT ( 'NONE',  ( 5.584674446412367210, -1.345185468269005424, 1.639207791927596247 ) ) ;
#105435 = ADVANCED_FACE ( 'NONE', ( #7453 ), #124511, .T. ) ;
#105436 = CARTESIAN_POINT ( 'NONE',  ( 2.696638560983040112, -2.301352489519994382, -0.1704845361689636130 ) ) ;
#105437 = CARTESIAN_POINT ( 'NONE',  ( 3.701569118832209515, -1.483977648892897960, -1.283320388228793130 ) ) ;
#105438 = CARTESIAN_POINT ( 'NONE',  ( 6.983263157960404754, -0.005959781318053481922, 2.045923054782183392 ) ) ;
#105439 = CARTESIAN_POINT ( 'NONE',  ( 4.053524740805938720, 3.831459740469437936, 1.214306433183764966E-14 ) ) ;
#105440 = CARTESIAN_POINT ( 'NONE',  ( 5.228604516725597229, 6.129068686715179126, -1.199719254218450271 ) ) ;
#105441 = EDGE_LOOP ( 'NONE', ( #133357, #157481, #146581, #17873, #145318, #102532, #199518, #31492, #134757, #203572, #107980, #131361, #177709 ) ) ;
#105442 = CARTESIAN_POINT ( 'NONE',  ( 5.542203953035277131, 0.8216685229280199509, 1.841735684200429990 ) ) ;
#105444 = CARTESIAN_POINT ( 'NONE',  ( 1.469576158976824144E-15, 15.51887838114830132, 12.00000000000000178 ) ) ;
#105443 = AXIS2_PLACEMENT_3D ( 'NONE', #212686, #62197, #198562 ) ;
#105445 = CARTESIAN_POINT ( 'NONE',  ( 3.379888771869215436, -2.093702847677909595, 0.5742949676477026033 ) ) ;
#105446 = CARTESIAN_POINT ( 'NONE',  ( 5.890091390494168522, 5.836471141856793388, 0.000000000000000000 ) ) ;
#105447 = CARTESIAN_POINT ( 'NONE',  ( 0.7211286721200690364, 1.601891702520108485, -1.389630591760198541 ) ) ;
#105448 = CARTESIAN_POINT ( 'NONE',  ( -0.7500000000000215383, 2.222916667349486453, 1.299038105676671107 ) ) ;
#105449 = CARTESIAN_POINT ( 'NONE',  ( -3.543819111236696795, 14.48034520802695724, -11.47346693889574176 ) ) ;
#105450 = CARTESIAN_POINT ( 'NONE',  ( 0.1333692844072585093, 7.629137130509075604, -2.653547345224527287 ) ) ;
#105451 = CARTESIAN_POINT ( 'NONE',  ( 5.098657496608274720, 7.938328561423579011, 1.202842226815619142 ) ) ;
#105452 = CARTESIAN_POINT ( 'NONE',  ( 0.6497718435918962143, 0.6490781098625525436, -1.955935974237718256 ) ) ;
#105454 = CARTESIAN_POINT ( 'NONE',  ( 2.876381804795541619, 6.437993120328354024, 0.3511878651327338674 ) ) ;
#105453 = CARTESIAN_POINT ( 'NONE',  ( -8.479735010343349089, 11.98044238112085758, 1.199719254218453823 ) ) ;
#105455 = CARTESIAN_POINT ( 'NONE',  ( -1.364683531250000748, 1.259375000341421469, 0.000000000000000000 ) ) ;
#105456 = DIRECTION ( 'NONE',  ( -0.9999980456341539536, 0.000000000000000000, -0.001977050295949901899 ) ) ;
#105457 = VERTEX_POINT ( 'NONE', #9596 ) ;
#105458 = ADVANCED_FACE ( 'NONE', ( #75673 ), #169964, .F. ) ;
#105459 = CARTESIAN_POINT ( 'NONE',  ( 2.824755571612533434, 1.383597569638248315, -1.320258682893655999 ) ) ;
#105460 = CARTESIAN_POINT ( 'NONE',  ( 5.541803865142582275, 0.7143684798897788069, -1.619465043896466616 ) ) ;
#105461 = VECTOR ( 'NONE', #35951, 1000.000000000000000 ) ;
#105462 = CARTESIAN_POINT ( 'NONE',  ( 6.737475991348287785, 6.825086509519945999, -0.7998128361456481317 ) ) ;
#105463 = CARTESIAN_POINT ( 'NONE',  ( -4.386226389220933441, 5.076017861301227008, -1.199719254218446718 ) ) ;
#105464 = CARTESIAN_POINT ( 'NONE',  ( 0.2108110590392465178, 1.506053368259860248, -1.006445417241896845 ) ) ;
#105466 = CARTESIAN_POINT ( 'NONE',  ( 1.235391793297924812, 0.5527703352327991704, -1.834263772151963456 ) ) ;
#105465 = CARTESIAN_POINT ( 'NONE',  ( 6.770610912236886492, -7.154544010627095219, 6.663994888585879295 ) ) ;
#105467 = CARTESIAN_POINT ( 'NONE',  ( 2.453653613718423276, 1.598880132357576755, 1.315258840600006085 ) ) ;
#105468 = CARTESIAN_POINT ( 'NONE',  ( -0.6823417656250003738, -0.4697916663252491021, -1.181850606188749264 ) ) ;
#105469 = CARTESIAN_POINT ( 'NONE',  ( 6.262560305340551636, -1.321439916381482060, 1.324322166508178356 ) ) ;
#105470 = CARTESIAN_POINT ( 'NONE',  ( 3.070728972534173096, -1.687097908962056803, -0.6982200720766564839 ) ) ;
#105472 = CARTESIAN_POINT ( 'NONE',  ( 6.059270238282111087, 7.038290852966752276, 1.014332888565868229 ) ) ;
#105471 = CARTESIAN_POINT ( 'NONE',  ( 5.233140740401229785, 0.1595256157847015632, 2.201181388321731269 ) ) ;
#105473 = CARTESIAN_POINT ( 'NONE',  ( -1.364683531250014514, -0.2197916663252438285, 0.7879004041258379498 ) ) ;
#105474 = CARTESIAN_POINT ( 'NONE',  ( 4.422371107804410784, 0.9697015505613596487, 1.820508916172391300 ) ) ;
#105475 = CARTESIAN_POINT ( 'NONE',  ( -6.015013705957189316, 10.16926642359206134, 0.7998128361456481317 ) ) ;
#105476 = CARTESIAN_POINT ( 'NONE',  ( 10.05067194643221207, 10.62020544712608938, 0.7998128361456462443 ) ) ;
#105477 = CARTESIAN_POINT ( 'NONE',  ( 4.330940004561544043, 7.140181541042074365, -1.199719254218452047 ) ) ;
#105478 = CARTESIAN_POINT ( 'NONE',  ( 0.8960494714182369869, -0.7788709108395329705, 2.016556642405589184 ) ) ;
#105479 = CARTESIAN_POINT ( 'NONE',  ( 6.531696417657103737, 1.982406992490031383, -0.5971068152322634992 ) ) ;
#105480 = CARTESIAN_POINT ( 'NONE',  ( 1.364683531249986537, 1.717708333674749399, -0.7879004041258239610 ) ) ;
#105481 = CARTESIAN_POINT ( 'NONE',  ( 3.831458500214664387, -1.998831773244442056, 0.8233788064144487162 ) ) ;
#105482 = CARTESIAN_POINT ( 'NONE',  ( 4.776038667982859032, 1.997392889608617716, -0.2983725866285909523 ) ) ;
#105483 = CARTESIAN_POINT ( 'NONE',  ( 6.620655732516650183, -0.005281389526671976913, 2.273887028200880511 ) ) ;
#105484 = CIRCLE ( 'NONE', #22391, 1.500000000000000222 ) ;
#105487 = CARTESIAN_POINT ( 'NONE',  ( 6.236387472606139681, 8.298871356172400127, -1.443375672974057666 ) ) ;
#105486 = CARTESIAN_POINT ( 'NONE',  ( -1.737500000000000266, -0.05833333333333384774, -3.009438278150923907 ) ) ;
#105485 = DIRECTION ( 'NONE',  ( 1.000000000000000000, -0.000000000000000000, -0.000000000000000000 ) ) ;
#105488 = CARTESIAN_POINT ( 'NONE',  ( -5.433785704026946384, 9.561443431331920095, 0.000000000000000000 ) ) ;
#105489 = CARTESIAN_POINT ( 'NONE',  ( 2.641814858895009444, 2.006371511526034546, -0.2024640970367599380 ) ) ;
#105490 = CARTESIAN_POINT ( 'NONE',  ( -5.703176172842872482, 9.805455968292021041, 0.000000000000000000 ) ) ;
#105492 = CARTESIAN_POINT ( 'NONE',  ( -4.241820592029106329, 7.460146341384830571, -0.9904578092340046158 ) ) ;
#105491 = CARTESIAN_POINT ( 'NONE',  ( -4.928552533767591726, 5.708731696605642725, 1.199719254218462483 ) ) ;
#105493 = DIRECTION ( 'NONE',  ( -0.000000000000000000, -1.000000000000000000, -0.000000000000000000 ) ) ;
#105494 = CARTESIAN_POINT ( 'NONE',  ( 6.205323455156911194, 1.660478276859885582, -0.9486371710855368011 ) ) ;
#105495 = CARTESIAN_POINT ( 'NONE',  ( -3.895996091634230218, 7.334980739573080832, 0.5863762202383783206 ) ) ;
#105496 = CARTESIAN_POINT ( 'NONE',  ( 5.463572716182824252, 7.397254140345190798, 1.443375672974062551 ) ) ;
#105498 = CARTESIAN_POINT ( 'NONE',  ( 3.937125189161301719, -1.678018027730580286, -1.117815418662113425 ) ) ;
#105497 = CARTESIAN_POINT ( 'NONE',  ( -8.310784975052682100, 10.71900177569337487, -1.443375672974058777 ) ) ;
#105499 = CARTESIAN_POINT ( 'NONE',  ( 0.7499999999999920064, 4.233333333333352932, 1.299038105676669330 ) ) ;
#105500 = CARTESIAN_POINT ( 'NONE',  ( -1.364683531250010295, 14.94270833367472839, 0.7879004041258445001 ) ) ;
#105501 = CARTESIAN_POINT ( 'NONE',  ( 6.053657651994457822, 0.4959367165196375549, -1.651908409946404976 ) ) ;
#105502 = CARTESIAN_POINT ( 'NONE',  ( 6.008198349511364000, 7.038594824965278995, 1.199719254218453823 ) ) ;
#105503 = CARTESIAN_POINT ( 'NONE',  ( 8.215877900201359552, 11.56864606933486606, -1.082531754730543083 ) ) ;
#105504 = CARTESIAN_POINT ( 'NONE',  ( -11.55950211276791073, 11.29999999999999893, -3.221476510067115662 ) ) ;
#105505 = CARTESIAN_POINT ( 'NONE',  ( 5.852782322939767745, -1.474943281369223369, 1.150351685248012457 ) ) ;
#105506 = FACE_OUTER_BOUND ( 'NONE', #141659, .T. ) ;
#105507 = CARTESIAN_POINT ( 'NONE',  ( 2.588806720547200513, 2.007000696110202043, 0.5072723548179418618 ) ) ;
#105508 = CARTESIAN_POINT ( 'NONE',  ( -2.788906526875773208E-15, 12.46875000068279782, -1.499999999999998446 ) ) ;
#105509 = ORIENTED_EDGE ( 'NONE', *, *, #108367, .F. ) ;
#105510 = CARTESIAN_POINT ( 'NONE',  ( 0.3863424973270003226, -0.6820169105002243937, -1.897691504806876761 ) ) ;
#105511 = CARTESIAN_POINT ( 'NONE',  ( 1.634716215409822260, 1.691188361570634235, 0.6499044650936767198 ) ) ;
#105512 = CARTESIAN_POINT ( 'NONE',  ( 4.624739795592929248, 6.488892076315451618, -1.443375672974068769 ) ) ;
#105513 = DIRECTION ( 'NONE',  ( -1.776356839400250465E-15, 0.000000000000000000, 1.000000000000000000 ) ) ;
#105514 = CARTESIAN_POINT ( 'NONE',  ( 8.907343734053986495, 9.494248565925552441, -0.7216878364870197293 ) ) ;
#105515 = CARTESIAN_POINT ( 'NONE',  ( 8.938903350111612411, 9.323142084752035430, -0.7998128361456221525 ) ) ;
#105517 = CARTESIAN_POINT ( 'NONE',  ( 6.046487378053778450, -1.350936885689631772, 1.358403761460762471 ) ) ;
#105516 = CARTESIAN_POINT ( 'NONE',  ( -5.799137018343247796, 7.788745826199009237, -1.599625672291256295 ) ) ;
#105518 = FACE_OUTER_BOUND ( 'NONE', #28433, .T. ) ;
#105519 = CARTESIAN_POINT ( 'NONE',  ( -4.168895032367330167, 3.976329666238523242, -0.6109567437776577403 ) ) ;
#105520 = CARTESIAN_POINT ( 'NONE',  ( -1.364683531250000748, -0.9281249996585805295, 0.000000000000000000 ) ) ;
#105522 = ORIENTED_EDGE ( 'NONE', *, *, #89482, .F. ) ;
#105521 = CARTESIAN_POINT ( 'NONE',  ( 3.958617665510264949, 5.641473247893851628, -1.443375672974051449 ) ) ;
#105523 = CARTESIAN_POINT ( 'NONE',  ( -7.049876689426097798, 11.16868053773170821, -0.7216878364870267237 ) ) ;
#105524 = CARTESIAN_POINT ( 'NONE',  ( 2.993221558690632556, 1.854768100113469265, -1.110066390340218367 ) ) ;
#105525 = CARTESIAN_POINT ( 'NONE',  ( -7.919371124158132602, 8.411890197705517380, -0.7216878364870338292 ) ) ;
#105526 = CARTESIAN_POINT ( 'NONE',  ( 5.804299160426222848, 7.865044668620976509, -1.443375672974078761 ) ) ;
#105527 = CARTESIAN_POINT ( 'NONE',  ( 0.6684183810189650021, 2.117893379942568988, -0.1100008709709817956 ) ) ;
#105528 = CARTESIAN_POINT ( 'NONE',  ( 5.965807262869927463, 1.798080572464531679, -0.3147057940002598864 ) ) ;
#105529 = CARTESIAN_POINT ( 'NONE',  ( 2.161341668630599955, 0.3408821015241836894, -1.941522824740661290 ) ) ;
#105530 = CARTESIAN_POINT ( 'NONE',  ( 5.062724140118719518, 0.5608846916410530348, 1.828269531156314853 ) ) ;
#105531 = ORIENTED_EDGE ( 'NONE', *, *, #113401, .F. ) ;
#105532 = CARTESIAN_POINT ( 'NONE',  ( -7.120058540175079997, 14.48019278289790002, -9.669703550014270732 ) ) ;
#105533 = CARTESIAN_POINT ( 'NONE',  ( 4.404722228293363351, 0.5232710054461316984, 1.898709409516568192 ) ) ;
#105534 = CARTESIAN_POINT ( 'NONE',  ( 6.567919353034534780, -1.191429365117269157, 1.534444726360333799 ) ) ;
#105535 = ORIENTED_EDGE ( 'NONE', *, *, #105847, .T. ) ;
#105536 = CARTESIAN_POINT ( 'NONE',  ( -4.773352600463090845, 7.726605912919016106, 1.199719254218452935 ) ) ;
#105538 = CARTESIAN_POINT ( 'NONE',  ( 6.725445687907758874, -7.162053774861991684, -6.710127771514625472 ) ) ;
#105537 = CARTESIAN_POINT ( 'NONE',  ( -5.469788628470539926, 5.346117919495872783, -0.7998128361456362523 ) ) ;
#105541 = AXIS2_PLACEMENT_3D ( 'NONE', #204673, #142941, #90973 ) ;
#105540 = CARTESIAN_POINT ( 'NONE',  ( 6.848276988234151652, 7.162280372460873679, -0.7216878364870317197 ) ) ;
#105539 = CARTESIAN_POINT ( 'NONE',  ( 6.286176778230493589, 10.48562334124426698, 0.7998128361456462443 ) ) ;
#105543 = VERTEX_POINT ( 'NONE', #103919 ) ;
#105542 = CARTESIAN_POINT ( 'NONE',  ( 5.109976026518994630, -0.6845719981980763480, 1.785733525123212928 ) ) ;
#105544 = CARTESIAN_POINT ( 'NONE',  ( 0.8334014933106950185, 0.1641056870149599223, 2.200712145998296343 ) ) ;
#105545 = CARTESIAN_POINT ( 'NONE',  ( 1.220146605508150803E-14, 9.718750000682797818, -1.499999999999998446 ) ) ;
#105546 = CARTESIAN_POINT ( 'NONE',  ( 5.742843059509288750, 1.940770921862687182, 0.5345600180575919014 ) ) ;
#105548 =( BOUNDED_SURFACE ( )  B_SPLINE_SURFACE ( 3, 2, ( 
 ( #176838, #13262, #12190 ),
 ( #63083, #78261, #195223 ),
 ( #99853, #81469, #178985 ),
 ( #116157, #148605, #165915 ) ),
 .UNSPECIFIED., .F., .F., .T. ) 
 B_SPLINE_SURFACE_WITH_KNOTS ( ( 4, 4 ),
 ( 3, 3 ),
 ( 0.01090518310586315390, 0.01337341879808987347 ),
 ( 0.000000000000000000, 1.000000000000000000 ),
 .UNSPECIFIED. ) 
 GEOMETRIC_REPRESENTATION_ITEM ( )  RATIONAL_B_SPLINE_SURFACE ( (
 ( 1.000000000000000000, 0.6967468848055796693, 1.000000000000000000),
 ( 1.000000000000000000, 0.6961913616436852248, 1.000000000000000000),
 ( 1.000000000000000000, 0.6955505937921927506, 1.000000000000000000),
 ( 1.000000000000000000, 0.6947640035364115452, 1.000000000000000000) ) ) 
 REPRESENTATION_ITEM ( '' )  SURFACE ( )  );
#105547 = CARTESIAN_POINT ( 'NONE',  ( 0.07661050522435489119, 4.099791711901569435, -2.265836654070508605 ) ) ;
#105549 = CARTESIAN_POINT ( 'NONE',  ( 11.84668730067608600, 19.00000000000000000, 1.319999999999998286 ) ) ;
#105550 = DIRECTION ( 'NONE',  ( -0.000000000000000000, -1.000000000000000000, -0.000000000000000000 ) ) ;
#105551 = CARTESIAN_POINT ( 'NONE',  ( 2.453653613718423276, 1.598880132357576755, 1.315258840600006085 ) ) ;
#105552 = CARTESIAN_POINT ( 'NONE',  ( -6.749261541504576911, 6.768559974710451677, 1.040834085586084257E-14 ) ) ;
#105553 = CARTESIAN_POINT ( 'NONE',  ( -4.652699544748355898, 8.322425126176462129, -0.4365168051920116365 ) ) ;
#105555 = CARTESIAN_POINT ( 'NONE',  ( 0.9894095316701527754, 1.906041449620498929, -1.019753361306941386 ) ) ;
#105554 = CARTESIAN_POINT ( 'NONE',  ( -4.771579997005698459, 7.654261532226910525, -1.199719254218452047 ) ) ;
#105556 = SURFACE_SIDE_STYLE ('',( #57844 ) ) ;
#105557 = EDGE_CURVE ( 'NONE', #135381, #160603, #120495, .T. ) ;
#105558 = CARTESIAN_POINT ( 'NONE',  ( 5.411112705629925301, 5.485588709422586362, 0.000000000000000000 ) ) ;
#105559 = CARTESIAN_POINT ( 'NONE',  ( 7.750016138724922676, -6.480061791515691283, -7.806764249273701495 ) ) ;
#105560 = CARTESIAN_POINT ( 'NONE',  ( -1.364683531250000748, 13.67187500034139980, 0.000000000000000000 ) ) ;
#105562 = CARTESIAN_POINT ( 'NONE',  ( -4.932134020321308654, 8.976183133675331050, 0.7998128361456291469 ) ) ;
#105561 = LINE ( 'NONE', #171594, #207503 ) ;
#105563 = EDGE_CURVE ( 'NONE', #57617, #29485, #118837, .T. ) ;
#105565 = CARTESIAN_POINT ( 'NONE',  ( 4.676219527341594073, 1.289314336954486384, 1.159937944992680547 ) ) ;
#105564 = AXIS2_PLACEMENT_3D ( 'NONE', #195865, #127766, #12822 ) ;
#105566 = CARTESIAN_POINT ( 'NONE',  ( -2.981903720001798597, 5.566305875722335372, -1.199719254218446718 ) ) ;
#105567 = CARTESIAN_POINT ( 'NONE',  ( 2.782155020660907141, -1.188329515115684076, -1.695063343828225877 ) ) ;
#105568 = CARTESIAN_POINT ( 'NONE',  ( 4.710634317702605323, 2.026528413205666013, 0.6131292256000410168 ) ) ;
#105569 = COLOUR_RGB ( '', 0.31764706, 0.68627451, 0.89019608) ;
#105570 = CARTESIAN_POINT ( 'NONE',  ( 6.642605195691581699, 9.837124264027149678, 1.199719254218462483 ) ) ;
#105571 = CARTESIAN_POINT ( 'NONE',  ( 0.09775709102116830751, -9.919835437265270173, 10.99956570265433697 ) ) ;
#105572 = CARTESIAN_POINT ( 'NONE',  ( 2.184365610098043309, 1.138103218778206971, -1.607087707149345901 ) ) ;
#105573 = CARTESIAN_POINT ( 'NONE',  ( 6.039686174407700392, 6.062845369715991417, 0.4964408002013191989 ) ) ;
#105574 = CARTESIAN_POINT ( 'NONE',  ( -1.347971487989957070E-14, -2.712500000000000355, 3.475000000000000089 ) ) ;
#105575 = CARTESIAN_POINT ( 'NONE',  ( 4.400488903878751579, 1.773513045242902209, -1.452268937634313417 ) ) ;
#105576 = CARTESIAN_POINT ( 'NONE',  ( 1.365546509989667534, 1.798985258052044900, -0.3101867277976525505 ) ) ;
#105577 = CARTESIAN_POINT ( 'NONE',  ( 6.364626766972446781, 6.390095747748157251, 0.7998128361456352531 ) ) ;
#105578 = CARTESIAN_POINT ( 'NONE',  ( 6.453317929980448397, 6.631218461173066459, 1.040834085586084257E-14 ) ) ;
#105579 = CARTESIAN_POINT ( 'NONE',  ( -8.843996274815957293, 9.212417163573759282, 1.040834085586084257E-14 ) ) ;
#105580 = CARTESIAN_POINT ( 'NONE',  ( 3.234638274129162827, 1.273785088661258058, -1.559031609643942717 ) ) ;
#105581 = CARTESIAN_POINT ( 'NONE',  ( 3.643363735869999509, 1.775428317022755609, -0.8347113108059034392 ) ) ;
#105582 = CARTESIAN_POINT ( 'NONE',  ( -7.212047647465563038, 10.50147379109678880, -1.199719254218446718 ) ) ;
#105583 = CARTESIAN_POINT ( 'NONE',  ( -5.412729640353771465, 7.337937218544611895, 1.599625672291269396 ) ) ;
#105584 = CARTESIAN_POINT ( 'NONE',  ( 9.000007961041747606, 1.000000000000000888, 7.937244906211794238 ) ) ;
#105586 = CARTESIAN_POINT ( 'NONE',  ( 4.469463222250699808, 1.716395428585426153, -0.4311418314640375615 ) ) ;
#105585 = CARTESIAN_POINT ( 'NONE',  ( 5.595677694052432649, -2.090823719441712747, -0.0008997866532325231618 ) ) ;
#105587 = CARTESIAN_POINT ( 'NONE',  ( -2.314109536355652530, 5.457892750589173225, -0.8025987720412944837 ) ) ;
#105588 = CARTESIAN_POINT ( 'NONE',  ( 0.4280004979528989617, 1.123059939108238314, -1.881669248891951085 ) ) ;
#105589 = CARTESIAN_POINT ( 'NONE',  ( 5.173663570605946838, -0.9624332111635640619, 1.449765197900940938 ) ) ;
#105590 = CARTESIAN_POINT ( 'NONE',  ( 7.670162217029129259, 9.971608557999250166, 1.599625672291281386 ) ) ;
#105591 = CARTESIAN_POINT ( 'NONE',  ( 0.1331715793776913348, 0.7364730991098663582, -2.038600455735229300 ) ) ;
#105592 = ADVANCED_FACE ( 'NONE', ( #30117 ), #47454, .F. ) ;
#105593 = CARTESIAN_POINT ( 'NONE',  ( 6.346320258841911865, 0.3977546830747305528, -2.263887401186816639 ) ) ;
#105594 = CARTESIAN_POINT ( 'NONE',  ( -0.07626876867936756288, -1.353788312843669406, -1.724171373301164767 ) ) ;
#105595 = CARTESIAN_POINT ( 'NONE',  ( 5.764916378462246804, -1.734034293797588999, 0.002837784182162239165 ) ) ;
#105596 = CARTESIAN_POINT ( 'NONE',  ( 2.332911791115964473, 2.140974936812658935, 0.5348262304398290201 ) ) ;
#105597 =( LENGTH_UNIT ( ) NAMED_UNIT ( * ) SI_UNIT ( .MILLI., .METRE. ) );
#105598 = CARTESIAN_POINT ( 'NONE',  ( 5.740740459546420205, -2.117024774779395102, -0.4812451790989195621 ) ) ;
#105599 = CARTESIAN_POINT ( 'NONE',  ( 0.7962977453638077074, -0.9578387366565711547, -1.888411434433327374 ) ) ;
#105601 = CIRCLE ( 'NONE', #116155, 11.54340198673881979 ) ;
#105600 = CARTESIAN_POINT ( 'NONE',  ( 4.093750000000002665, -1.895863743164171611, -0.7852924748297696045 ) ) ;
#105602 = CARTESIAN_POINT ( 'NONE',  ( 6.727182134110234024, -0.002100931800118072384, 2.089081857379895268 ) ) ;
#105603 = CARTESIAN_POINT ( 'NONE',  ( 4.278288924157873652, -1.109688035731031475, 1.574481611047764851 ) ) ;
#105604 = CARTESIAN_POINT ( 'NONE',  ( 1.366231352279376310, 0.6402347118669349246, -2.127050378772620487 ) ) ;
#105605 = EDGE_LOOP ( 'NONE', ( #178000, #168138, #111819, #205720 ) ) ;
#105607 = CARTESIAN_POINT ( 'NONE',  ( 1.499999999999987121, 3.795833333333356929, -0.8660254037844262731 ) ) ;
#105606 = CARTESIAN_POINT ( 'NONE',  ( 1.312523894619976650, 1.535058519010788602, -1.702700526841523399 ) ) ;
#105608 = CARTESIAN_POINT ( 'NONE',  ( 3.822509244049070887, 6.547012320444182798, -1.199719254218452047 ) ) ;
#105609 = CARTESIAN_POINT ( 'NONE',  ( 4.320244504248938355, 8.192035688265757898, 1.040834085586084257E-14 ) ) ;
#105610 = CARTESIAN_POINT ( 'NONE',  ( 3.616091037371416572, -0.6436381315554053906, 2.126022720447027670 ) ) ;
#105611 = CARTESIAN_POINT ( 'NONE',  ( -7.700668062882065179, 10.96756792579566664, -1.082531754730543971 ) ) ;
#105612 = SURFACE_STYLE_FILL_AREA ( #21093 ) ;
#105613 = CARTESIAN_POINT ( 'NONE',  ( 7.809133291791403586, 8.213003049952529722, -0.7216878364870257245 ) ) ;
#105614 = CARTESIAN_POINT ( 'NONE',  ( -9.625925875578284163, 10.33259439770390564, 1.040834085586084257E-14 ) ) ;
#105615 = CARTESIAN_POINT ( 'NONE',  ( 6.861835142292143530, 8.138467433163244280, 1.082531754730549967 ) ) ;
#105616 = STYLED_ITEM ( 'NONE', ( #10624 ), #87466 ) ;
#105617 = EDGE_LOOP ( 'NONE', ( #143072, #33598, #188078, #148435, #132571, #22354, #101776, #13943 ) ) ;
#105618 = CARTESIAN_POINT ( 'NONE',  ( 2.338517726396415863, 0.5350873343827439177, -1.944071628254496087 ) ) ;
#105620 = CARTESIAN_POINT ( 'NONE',  ( 6.883263157960402445, -0.003972766660574957552, 2.046037087719229319 ) ) ;
#105619 = CARTESIAN_POINT ( 'NONE',  ( 7.618792255875527886, 10.97600916757510170, 1.199719254218460707 ) ) ;
#105621 = CARTESIAN_POINT ( 'NONE',  ( -10.86152993230177621, -6.808378554901812763, 0.3183146091066173522 ) ) ;
#105622 = CARTESIAN_POINT ( 'NONE',  ( 5.994113310573177422, 10.00723293906178846, 0.000000000000000000 ) ) ;
#105623 = CARTESIAN_POINT ( 'NONE',  ( 6.356985390939413172, 0.2876776518413763917, -1.716344579348449084 ) ) ;
#105624 = CARTESIAN_POINT ( 'NONE',  ( 0.6823417656249899377, 2.342708333674753618, 1.181850606188767472 ) ) ;
#105625 = CARTESIAN_POINT ( 'NONE',  ( 1.035986422354659320, 1.742213337529074035, 0.3100009841157587154 ) ) ;
#105626 = CARTESIAN_POINT ( 'NONE',  ( 0.5455463417442986129, -1.458554840210561476, 1.392547631435703037 ) ) ;
#105627 = CARTESIAN_POINT ( 'NONE',  ( 0.3800845246329161431, -0.2246070939678334044, -1.827447590993152682 ) ) ;
#105628 = CARTESIAN_POINT ( 'NONE',  ( 4.599361256383265761, -0.6123007911535255365, 2.209042870082494225 ) ) ;
#105629 = CARTESIAN_POINT ( 'NONE',  ( 3.943160212656390051, 0.6185462545997171269, -1.734258544408360470 ) ) ;
#105630 = AXIS2_PLACEMENT_3D ( 'NONE', #18136, #84225, #150313 ) ;
#105631 = EDGE_CURVE ( 'NONE', #198620, #22926, #193069, .T. ) ;
#105632 = CARTESIAN_POINT ( 'NONE',  ( 8.341290820905593151, 10.75459192918846618, 1.599625672291281386 ) ) ;
#105633 = CARTESIAN_POINT ( 'NONE',  ( 6.928203230275520319, 15.00000000000000000, 9.797958971132713302 ) ) ;
#105634 = CARTESIAN_POINT ( 'NONE',  ( 3.258640109524315154, -1.383274205585843797, 1.191454006006509303 ) ) ;
#105635 = CARTESIAN_POINT ( 'NONE',  ( 4.219375079941334761, 1.978050461189932552, 0.3905991720301109082 ) ) ;
#105636 = CARTESIAN_POINT ( 'NONE',  ( -8.992082194361570302, 11.51384853155376220, 1.599625672291269396 ) ) ;
#105638 = CARTESIAN_POINT ( 'NONE',  ( 1.123270288250311610, 3.110197346350006331, 0.7749999999993734123 ) ) ;
#105637 = CARTESIAN_POINT ( 'NONE',  ( 3.239431411193524735, -1.996134195211620721, 1.065073381557869903 ) ) ;
#105639 = CARTESIAN_POINT ( 'NONE',  ( 5.596739085487917542, -0.5086175864091507792, -2.043493955398622219 ) ) ;
#105640 = CARTESIAN_POINT ( 'NONE',  ( 7.910363579994360350, 15.96602505221457058, 9.911917230698591652 ) ) ;
#105641 = CARTESIAN_POINT ( 'NONE',  ( 3.297389726143421740, -1.827171938055579536, 0.9735347560282039403 ) ) ;
#105642 = CARTESIAN_POINT ( 'NONE',  ( 2.703961570921634028, 5.242040035128820108, -1.199719254218446718 ) ) ;
#105643 = CARTESIAN_POINT ( 'NONE',  ( -1.360316468750036645, 2.151041667008108060, -0.7853790794159301036 ) ) ;
#105644 = CARTESIAN_POINT ( 'NONE',  ( 5.988958055669808545, -2.013456733998910231, -0.6654305520411087915 ) ) ;
#105645 = PRODUCT_CONTEXT ( 'NONE', #212288, 'mechanical' ) ;
#105647 = CARTESIAN_POINT ( 'NONE',  ( 0.6449897232218603227, -1.652859335204670543, 0.9894661712252955654 ) ) ;
#105646 = CARTESIAN_POINT ( 'NONE',  ( -7.641992139597101108, 12.06740792950531649, 0.7998128361456481317 ) ) ;
#105648 = UNCERTAINTY_MEASURE_WITH_UNIT (LENGTH_MEASURE( 1.000000000000000082E-05 ), #70788, 'distance_accuracy_value', 'NONE');
#105649 = CARTESIAN_POINT ( 'NONE',  ( 9.121938423896107651, 9.536683004167278099, -0.7998128361456221525 ) ) ;
#105650 = CARTESIAN_POINT ( 'NONE',  ( 3.553645660113312399, 7.160020680191912845, -1.734723475976807094E-15 ) ) ;
#105651 = CARTESIAN_POINT ( 'NONE',  ( 5.275030131637754138, 6.378586025900190748, 1.136986337720545581 ) ) ;
#105652 = CARTESIAN_POINT ( 'NONE',  ( 1.400751299547981610, 7.315968950352358391, 4.333496285527950853 ) ) ;
#105653 = CARTESIAN_POINT ( 'NONE',  ( -5.752737250900127997, 5.605948302338584099, 0.000000000000000000 ) ) ;
#105654 = CARTESIAN_POINT ( 'NONE',  ( 0.5982529507728174822, 1.497540282193830841, 1.640895070279895895 ) ) ;
#105655 = CARTESIAN_POINT ( 'NONE',  ( 2.274573006691050558, -1.296483931956838198, 1.659472957066634669 ) ) ;
#105656 = CARTESIAN_POINT ( 'NONE',  ( -5.029148636026397945, 4.832037928311032182, 0.7998128361456281477 ) ) ;
#105657 = CARTESIAN_POINT ( 'NONE',  ( 9.088043039861931405, 9.497138389460751284, 1.040834085586084257E-14 ) ) ;
#105658 = CARTESIAN_POINT ( 'NONE',  ( 6.965680890820083349, -0.4048625726877760900, 1.822745621051139020 ) ) ;
#105659 = CARTESIAN_POINT ( 'NONE',  ( 7.426115451983150706, 9.686887332112256388, -1.599625672291262513 ) ) ;
#105660 = EDGE_CURVE ( 'NONE', #36910, #41289, #146989, .T. ) ;
#105661 = CARTESIAN_POINT ( 'NONE',  ( 11.89204169242350595, 9.799999999999998934, 0.8046421800351223341 ) ) ;
#105662 = CARTESIAN_POINT ( 'NONE',  ( -7.295696057929500711, 7.684269287105433222, 0.7216878364870317197 ) ) ;
#105663 = CARTESIAN_POINT ( 'NONE',  ( -9.002250809794006159, 10.56534270192358704, -1.082531754730543971 ) ) ;
#105664 = CARTESIAN_POINT ( 'NONE',  ( -6.391719935120312890, 6.567462711928212293, 2.438448603877958032 ) ) ;
#105665 = CARTESIAN_POINT ( 'NONE',  ( -6.563028877466991595, 9.814561569423593923, 1.199719254218452935 ) ) ;
#105667 = CARTESIAN_POINT ( 'NONE',  ( 3.350005920730843911, -0.7974703105717847462, 1.792663495558038056 ) ) ;
#105666 = CARTESIAN_POINT ( 'NONE',  ( -2.954552044183079750E-14, 2.734375000341430884, 1.570758158831788265 ) ) ;
#105668 = CARTESIAN_POINT ( 'NONE',  ( 2.079201547314021070, -0.1057080177612122196, -2.159229931372666389 ) ) ;
#105669 = CARTESIAN_POINT ( 'NONE',  ( 1.118424870118275738, -0.04499623084481922664, 1.840855209834332928 ) ) ;
#105671 = CARTESIAN_POINT ( 'NONE',  ( -5.780146447551155475, 6.079674369897793085, -0.5991446231495625163 ) ) ;
#105670 = CARTESIAN_POINT ( 'NONE',  ( -4.176793841461789114, 7.030620694084159794, -1.199719254218455378 ) ) ;
#105672 = CARTESIAN_POINT ( 'NONE',  ( 3.134399458026761121, -1.534476879465409782, 0.8210378458504956622 ) ) ;
#105673 = CARTESIAN_POINT ( 'NONE',  ( 7.131225611108100715, 7.422110755822004968, 0.7216878364870317197 ) ) ;
#105674 = CARTESIAN_POINT ( 'NONE',  ( -11.36822525729066413, 5.406166865499119289, 5.610767994321700591 ) ) ;
#105675 = CARTESIAN_POINT ( 'NONE',  ( 8.289920859751990889, 11.75899253876431416, 1.199719254218450271 ) ) ;
#105676 = CARTESIAN_POINT ( 'NONE',  ( 0.4796413896344040029, 2.016494124141111399, -0.7793912508547717888 ) ) ;
#105677 = CARTESIAN_POINT ( 'NONE',  ( 3.462267382487670631, 1.587593928739635896, 1.242537129137813556 ) ) ;
#105678 = CARTESIAN_POINT ( 'NONE',  ( -3.752568318859959007, 7.355240624044412812, 0.6449737300090957470 ) ) ;
#105679 = CARTESIAN_POINT ( 'NONE',  ( 0.6730137850648570952, -2.035850703004048246, -0.7271551459356735414 ) ) ;
#105680 = CARTESIAN_POINT ( 'NONE',  ( 2.746899856880557600, -1.639987585725300123, 1.093844759732710781 ) ) ;
#105681 = CARTESIAN_POINT ( 'NONE',  ( 6.609000000000053276, 6.037706995087852135, 2.494900065673964829 ) ) ;
#105682 = CARTESIAN_POINT ( 'NONE',  ( 2.770961567126817737, 1.843342918492569149, -0.6114499264749191365 ) ) ;
#105686 = VERTEX_POINT ( 'NONE', #29055 ) ;
#105685 = ADVANCED_FACE ( 'NONE', ( #45316 ), #59315, .T. ) ;
#105684 = CARTESIAN_POINT ( 'NONE',  ( -5.478903473698260029, 6.525047153136981137, -1.082531754730549967 ) ) ;
#105683 = CARTESIAN_POINT ( 'NONE',  ( -11.07131503167114772, 9.799999999999998934, 0.8043049353970799231 ) ) ;
#105687 = CARTESIAN_POINT ( 'NONE',  ( -4.380693030546956912, 6.204170850428461392, 1.443375672974065660 ) ) ;
#105688 = CARTESIAN_POINT ( 'NONE',  ( 4.549643065837591038, 7.465611455855944101, -1.199719254218452047 ) ) ;
#105689 = CARTESIAN_POINT ( 'NONE',  ( -5.550083779947821760, 7.568460058062819407, -1.599625672291271394 ) ) ;
#105690 = CARTESIAN_POINT ( 'NONE',  ( -5.121948170912633991, 9.197632976031879792, -0.7998128361456362523 ) ) ;
#105691 = CARTESIAN_POINT ( 'NONE',  ( -15.75000000000000000, 12.69999999999999929, 1.099999999999996758 ) ) ;
#105692 = EDGE_CURVE ( 'NONE', #154238, #157478, #118629, .T. ) ;
#105693 = CARTESIAN_POINT ( 'NONE',  ( 5.456226512670824036, 2.305251103711564387, -0.1065007851034898423 ) ) ;
#105694 = DIRECTION ( 'NONE',  ( 1.509903313490213211E-14, 0.000000000000000000, -1.000000000000000000 ) ) ;
#105695 = CARTESIAN_POINT ( 'NONE',  ( 3.643363735869999509, 1.775428317022755609, -0.8347113108059034392 ) ) ;
#105696 = CARTESIAN_POINT ( 'NONE',  ( 8.555358625423188812, 9.940005470203933768, 1.199719254218462483 ) ) ;
#105697 = CARTESIAN_POINT ( 'NONE',  ( 0.8443752267504719411, 0.3905955241953715795, -1.978051186352240309 ) ) ;
#105698 = ORIENTED_EDGE ( 'NONE', *, *, #83989, .F. ) ;
#105699 = CARTESIAN_POINT ( 'NONE',  ( 2.870428589035282751, -2.086819620220676352, -0.3573068958101219827 ) ) ;
#105700 = CARTESIAN_POINT ( 'NONE',  ( -0.7500000000000215383, 0.9729166673494854534, 1.299038105676659116 ) ) ;
#105701 = CARTESIAN_POINT ( 'NONE',  ( -7.718669524881690336, 7.899535955317097624, 0.7998128361456462443 ) ) ;
#105702 = CARTESIAN_POINT ( 'NONE',  ( 2.888418961059231904, 1.578855305991919478, -0.9468669452540460219 ) ) ;
#105703 = EDGE_LOOP ( 'NONE', ( #114619, #145638, #199197, #180448, #95673, #163851, #111423, #5616, #92095, #89966, #111536, #21295, #174255, #147777, #210769, #85147, #157635, #147371, #129798, #193136, #23664, #209179, #185403, #5736, #110909, #100979 ) ) ;
#105704 = CARTESIAN_POINT ( 'NONE',  ( -10.63367255181986160, 11.30037282007833532, 1.040834085586084257E-14 ) ) ;
#105705 = CARTESIAN_POINT ( 'NONE',  ( 9.423147110355582612, 13.09353312253862178, 7.356331950284607402 ) ) ;
#105706 = CARTESIAN_POINT ( 'NONE',  ( 4.377262645480927361, -1.895543854172193399, -0.9507902649282941043 ) ) ;
#105707 = CARTESIAN_POINT ( 'NONE',  ( 0.1988192939417210425, -0.4940924592915455493, 1.773541111592655373 ) ) ;
#105708 = DIRECTION ( 'NONE',  ( 0.000000000000000000, 0.000000000000000000, -1.000000000000000000 ) ) ;
#105709 = CARTESIAN_POINT ( 'NONE',  ( 6.799577732453452761, 7.891594428405881878, -1.199719254218446718 ) ) ;
#105710 = CARTESIAN_POINT ( 'NONE',  ( 6.393551957296131683, 9.616838495890963401, 1.199719254218452047 ) ) ;
#105711 = CARTESIAN_POINT ( 'NONE',  ( 4.393860645892766037, -0.7923225987812362314, 1.902584447174461291 ) ) ;
#105713 = CARTESIAN_POINT ( 'NONE',  ( 1.927068723821170559, -1.203646435588998420, -1.393412863611859454 ) ) ;
#105712 = CARTESIAN_POINT ( 'NONE',  ( -6.581593504430098385, 9.765943957555402122, -1.199719254218440723 ) ) ;
#105714 = CARTESIAN_POINT ( 'NONE',  ( -1.364683531250010295, 5.280208333674758059, 0.7879004041258379498 ) ) ;
#105715 = CARTESIAN_POINT ( 'NONE',  ( -5.823017895876262173, 7.308274721394978357, -1.333157625313810879 ) ) ;
#105716 = CARTESIAN_POINT ( 'NONE',  ( 10.98974895236967164, -7.729832900979586086, -0.4787367839867315844 ) ) ;
#105717 = B_SPLINE_CURVE_WITH_KNOTS ( 'NONE', 3,
 ( #201608, #186442, #38079, #102008, #185375, #183251, #182173, #137725, #67337, #2339, #34854, #33802, #119387, #17528, #118320, #136657, #53257, #104151, #184306, #100929, #19676, #200548, #83616, #68416, #149698, #36995, #134543, #103079, #18610, #70538, #1279, #170199, #168078, #20729, #85756, #133482, #151837, #3413, #169134, #21783, #69479, #135587, #86824, #87892, #152888, #4466, #202682, #120470, #153965, #5532, #71612, #55389, #23938, #76958, #109551, #72694, #121544, #7686, #107408, #173431, #175556, #25011, #188583, #91113, #106325, #125810, #172348, #138789, #40216, #43427, #39146, #90042, #124745, #41300, #9830, #174501, #156100, #105227, #73769, #122622, #42366, #139865, #191772, #205896, #8767, #26078, #190704, #74849, #75906, #27146, #157172, #10883, #159284, #93250, #171267, #143083, #57530, #22861, #123687, #189649, #108477, #140948, #59651, #92192, #158241, #206961, #142010, #209077, #208025, #58590, #187515, #88974, #155029, #6614, #204809, #56460, #110611, #16202, #127959, #144158, #64966, #131119, #78033, #14074, #113811, #44494, #30366, #177682, #130071, #126878, #11960, #145214, #197108, #62847, #180860, #210149, #61792, #147316, #82284, #48747, #32482, #96453, #193913, #213343, #13019, #114860, #45560, #98556, #148377, #179811, #163564, #111675, #31430, #162504, #211221, #29294, #60714, #194985, #176611, #97507, #15148, #164617, #81234, #146269, #80164, #160357, #212281, #192835, #28223, #94316, #46621, #95386, #161438, #79096, #129008, #112742, #63915, #178753, #196066, #47696, #168872, #149432, #167813, #152625, #34605, #185105, #119124, #101746, #85491, #52988, #199219, #68150, #151578, #150515, #4212, #36730, #102817, #84426, #69215, #136396, #20476, #99616, #66009, #181911, #19413, #86563, #166751, #133213, #198163, #70280, #135334, #37812, #202412, #54069, #17270, #3146, #120203, #49797, #184048, #116988, #201348, #186178, #182988, #50866, #103888, #169936, #21520, #87631, #214378, #132158, #83346, #18347, #33543, #100673, #2076, #115923, #165682, #1013, #67078, #134283, #200288, #51939, #118063, #35666, #124485, #189390, #89792, #138526, #109285, #73503, #203480, #190443, #58329, #104965, #55133, #6354, #24747, #42103, #26881, #72424, #157983, #139605, #156912, #171007, #153703, #175295, #38881, #122360, #22604, #5271, #90849, #137466, #23680, #108216, #173169, #9571, #155837, #88711, #205629, #204549, #57266, #39958, #71348, #8502, #106065, #74583, #154770, #174240, #56198, #25813, #121278, #172088, #91923, #141755, #41032, #43173, #191507, #125546, #187254, #188317, #7422, #206702, #123428, #107142, #140686, #75648, #207762, #59389, #146001, #177412, #162231, #14874, #113542, #29029, #195788, #127686, #179545, #47426, #31166, #160090, #142813, #63654, #13818, #130851, #80966, #97239, #110347, #46352, #212011, #76697, #62576, #209882, #79891, #159029, #44225, #95112, #147058, #161162, #213078, #27957, #94050, #64708, #176350, #45288, #126607, #77768, #12748, #208820, #180595, #129809, #10622, #92984, #192570, #112470, #163293, #78822, #11693, #144943, #143888, #61520, #210950, #128738, #60450, #196849, #48486, #193646, #111408, #194712, #178479, #114604, #30091, #96180, #36475, #32220, #1817, #148114, #181649, #165411, #18074, #150249, #164355, #98293, #183793, #15939, #116719, #201086, #51680 ),
 .UNSPECIFIED., .F., .F.,
 ( 4, 1, 1, 1, 1, 1, 1, 1, 1, 1, 1, 1, 1, 1, 1, 1, 1, 1, 1, 1, 1, 1, 1, 1, 1, 1, 1, 1, 1, 1, 1, 1, 1, 1, 1, 1, 1, 1, 1, 1, 1, 1, 1, 1, 1, 1, 1, 1, 1, 1, 1, 1, 1, 1, 1, 1, 1, 1, 1, 1, 1, 1, 1, 1, 1, 1, 1, 1, 1, 1, 1, 1, 1, 1, 1, 1, 1, 1, 1, 1, 1, 1, 1, 1, 1, 1, 1, 1, 1, 1, 1, 1, 1, 1, 1, 1, 1, 1, 1, 1, 1, 1, 1, 1, 1, 1, 1, 1, 1, 1, 1, 1, 1, 1, 1, 1, 1, 1, 1, 1, 1, 1, 1, 1, 1, 1, 1, 1, 1, 1, 1, 1, 1, 1, 1, 1, 1, 1, 1, 1, 1, 1, 1, 1, 1, 1, 1, 1, 1, 1, 1, 1, 1, 1, 1, 1, 1, 1, 1, 1, 1, 1, 1, 1, 1, 1, 1, 1, 1, 1, 1, 1, 1, 1, 1, 1, 1, 1, 1, 1, 1, 1, 1, 1, 1, 1, 1, 1, 1, 1, 1, 1, 1, 1, 1, 1, 1, 1, 1, 1, 1, 1, 1, 1, 1, 1, 1, 1, 1, 1, 1, 1, 1, 1, 1, 1, 1, 1, 1, 1, 1, 1, 1, 1, 1, 1, 1, 1, 1, 1, 1, 1, 1, 1, 1, 1, 1, 1, 1, 1, 1, 1, 1, 1, 1, 1, 1, 1, 1, 1, 1, 1, 1, 1, 1, 1, 1, 1, 1, 1, 1, 1, 1, 1, 1, 1, 1, 1, 1, 1, 1, 1, 1, 1, 1, 1, 1, 1, 1, 1, 1, 1, 1, 1, 1, 1, 1, 1, 1, 1, 1, 1, 1, 1, 1, 1, 1, 1, 1, 1, 1, 1, 1, 1, 1, 1, 1, 1, 1, 1, 1, 1, 1, 1, 1, 1, 1, 1, 1, 1, 1, 1, 1, 1, 1, 1, 1, 1, 1, 1, 1, 1, 1, 1, 1, 1, 1, 1, 1, 1, 1, 1, 1, 1, 1, 1, 1, 1, 1, 1, 1, 1, 1, 1, 1, 1, 1, 1, 1, 1, 1, 1, 1, 1, 1, 1, 1, 1, 1, 1, 1, 1, 1, 1, 1, 1, 1, 1, 1, 1, 1, 1, 1, 1, 4 ),
 ( 0.000000000000000000, 0.002600033395298661284, 0.005208813367820810773, 0.007813200023264601363, 0.01041635779573905213, 0.01302082523971277370, 0.01562491580351430334, 0.01822918961192645723, 0.02083333155136493989, 0.02343746137460561707, 0.02604174567981391505, 0.02864576082122225614, 0.03125012338981237453, 0.03385410379569547823, 0.03645843966640821554, 0.03906250599122108869, 0.04166672065998115043, 0.04427093656960304907, 0.04687500111868234121, 0.04947933663890847350, 0.05208331727515622817, 0.05468767913406928638, 0.05729168951085979872, 0.05989597295159828499, 0.06250011041458469752, 0.06510424634142775169, 0.06770853038940542745, 0.07031253939703428768, 0.07291690072920921362, 0.07552088074063932621, 0.07812521459448035221, 0.08072927904253822395, 0.08333349217322323643, 0.08593770650149938628, 0.08854176936806532061, 0.09114610329512429221, 0.09375008230893774885, 0.09635444258075796797, 0.09895845137230636912, 0.1015627332241899466, 0.1041668691376404637, 0.1067710034717011397, 0.1093752859901425123, 0.1119792934252105548, 0.1145836532378000650, 0.1171876317139315254, 0.1197919640503514460, 0.1223960270027875247, 0.1250002386107842423, 0.1276044514713231270, 0.1302085128224930721, 0.1328128452953424854, 0.1354168228245230532, 0.1380211816480703679, 0.1406251889951717071, 0.1432294693974442978, 0.1458336039016293884, 0.1484377367829480265, 0.1510420179109137340, 0.1536460239143070949, 0.1562503823458506746, 0.1588543594276481397, 0.1614586903853630351, 0.1640627519827278502, 0.1666669622076225599, 0.1692711737400035832, 0.1718752337163205746, 0.1744795648736557347, 0.1770835410591554138, 0.1796878985729436218, 0.1822919046164021839, 0.1848961837081005144, 0.1875003169431251615, 0.1901044485118078553, 0.1927087283883223978, 0.1953127331008320255, 0.1979170902898210183, 0.2005210661182068033, 0.2031253958358791578, 0.2057294562186703923, 0.2083336651999991573, 0.2109378755437518183, 0.2135419342857080849, 0.2161462642661750033, 0.2187502392488957503, 0.2213545955913898966, 0.2239586004719608947, 0.2265628783920732026, 0.2291670104979939837, 0.2317711408940984485, 0.2343754196581391558, 0.2369794232205082452, 0.2395837793053874898, 0.2421877540212369617, 0.2447920826374832270, 0.2473961419461526701, 0.2500003498234057431, 0.2526045591180144934, 0.2552086167660569949, 0.2578129457082574683, 0.2604169196290564980, 0.2630212749386780513, 0.2656252787970727613, 0.2682295556845439854, 0.2708336868013750398, 0.2734378161649161920, 0.2760420939554183439, 0.2786460965083475960, 0.2812504516275206035, 0.2838544253716674404, 0.2864587530250631842, 0.2890628114000217685, 0.2916670183126490179, 0.2942712266975582858, 0.2968752833920936807, 0.2994796114345903981, 0.3020835844342854570, 0.3046879388494173613, 0.3072919418263086455, 0.3098962178200457829, 0.3125003480877632800, 0.3151044765587182606, 0.3177087535145803887, 0.3203127551987332566, 0.3229171094905676220, 0.3255210824038090589, 0.3281254092328941829, 0.3307294668145174810, 0.3333336729019333866, 0.3359378805165532667, 0.3385419363979534357, 0.3411462636792753078, 0.3437502358986498918, 0.3463545895576419231, 0.3489585917936692261, 0.3515628670325462446, 0.3541669965910940188, 0.3567711243094072171, 0.3593754005694961839, 0.3619794015255044517, 0.3645837551283364619, 0.3671877273514386752, 0.3697920534947228832, 0.3723961104233561858, 0.3750003158249449187, 0.3776045228086560845, 0.3802085780172632101, 0.3828129046759103926, 0.3854168762557192984, 0.3880212292968930887, 0.3906252309326675998, 0.3932295055555311003, 0.3958336345448258409, 0.3984377616504144459, 0.4010420373535708016, 0.4036460377220391638, 0.4062503907741795706, 0.4088543624478828686, 0.4114586880438503846, 0.4140627444598136697, 0.4166669493149349202, 0.4192711558070936761, 0.4218752104832254046, 0.4244795366576747386, 0.4270835077386489487, 0.4296878603003031483, 0.4322918614764136302, 0.4348961356220873986, 0.4375002641820237570, 0.4401043908147829753, 0.4427086660998260093, 0.4453126660213379551, 0.4479170186610768045, 0.4505209899261007900, 0.4531253151132156320, 0.4557293711568096706, 0.4583335756048029785, 0.4609377817447468106, 0.4635418360287018591, 0.4661461618574116450, 0.4687501325802634344, 0.4713544848006788190, 0.4739584856576960492, 0.4765627594649867738, 0.4791668877354426925, 0.4817710140352507997, 0.4843752890409837031, 0.4869792886561065681, 0.4895836410217184742, 0.4921876120187673176, 0.4947919369354787933, 0.4973959927469893683, 0.5000001969271801183, 0.5026044028542325792, 0.5052084568862954539, 0.5078127825077110025, 0.5104167530131399344, 0.5130211050305848453, 0.5156251057090676104, 0.5182293793167697116, 0.5208335074376115870, 0.5234376335443351458, 0.5260419084095501185, 0.5286459078588399141, 0.5312502600885893322, 0.5338542309583571566, 0.5364585557431046370, 0.5390626114628084276, 0.5416668155145124564, 0.5442710213679887721, 0.5468750752884355970, 0.5494794008409938924, 0.5520833712696913143, 0.5546877232224267651, 0.5572917238629264691, 0.5598959974098275394, 0.5625001255209155504, 0.5651042515744146844, 0.5677085264378984863, 0.5703125258619060611, 0.5729168780940517847, 0.5755208489772277725, 0.5781251737684461878, 0.5807292295366155432, 0.5833334335991446906, 0.5859376395183565345, 0.5885416934674594369, 0.5911460190895951872, 0.5937499895822500040, 0.5963543416085342885, 0.5989583423516006144, 0.6015626159764864145, 0.6041667442176794633, 0.6067708703578130747, 0.6093751453583519107, 0.6119791448976270587, 0.6145834972704286026, 0.6171874683077025470, 0.6197917932438269384, 0.6223958492007358734, 0.6250000534134032559, 0.6276042595376638555, 0.6302083136556971832, 0.6328126394858472059, 0.6354166101831504321, 0.6380209624212449526, 0.6406249634074311361, 0.6432292372490908683, 0.6458333657602520761, 0.6484374921268833969, 0.6510417674032679125, 0.6536457671983656459, 0.6562501198500874100, 0.6588540911821543222, 0.6614584164016259482, 0.6640624726875546946, 0.6666666771896793131, 0.6692708836583093346, 0.6718749380855545406, 0.6744792642621626477, 0.6770832353048136243, 0.6796875878929879988, 0.6822915892628557133, 0.6848958634600870177, 0.6874999923810890534, 0.6901041191140900866, 0.6927083948051209195, 0.6953123949966061312, 0.6979167480655225075, 0.7005207198330885010, 0.7031250454743595002, 0.7057291022295995031, 0.7083333071605121267, 0.7109375141128444486, 0.7135415689895947544, 0.7161458956511181917, 0.7187498671798290273, 0.7213542202563657524, 0.7239582221504904380, 0.7265624968421051655, 0.7291666263128349090, 0.7317707535520923123, 0.7343750297965853102, 0.7369790305250381035, 0.7395833841494394711, 0.7421873564932268685, 0.7447916826947649227, 0.7473957400596251688, 0.7499999455586733310, 0.7526041531340577073, 0.7552082086006238759, 0.7578125358855373195, 0.7604165080410384414, 0.7630208617442386654, 0.7656248643032155243, 0.7682291396280439555, 0.7708332697884082707, 0.7734373976738285750, 0.7760416746106194585, 0.7786456760166404756, 0.7812500303348380859, 0.7838540033955903041, 0.7864583302958847444, 0.7890623884106959807, 0.7916665946172487534, 0.7942708029550582527, 0.7968748591517740287, 0.7994791871985751364, 0.8020831601216208417, 0.8046875145898089166, 0.8072915179542569097, 0.8098957940511537501, 0.8124999250410844809, 0.8151040537125986418, 0.8177083314805486669, 0.8203123337047645292, 0.8229166888550945025, 0.8255206627735817149, 0.8281249905111484066, 0.8307290495162685806, 0.8333332565697225691, 0.8359374658093579047, 0.8385415228765847884, 0.8411458518237998616, 0.8437498256551729803, 0.8463541810267020127, 0.8489581853372698550, 0.8515624623451190089, 0.8541665943045783083, 0.8567707239021479237, 0.8593750026401490993, 0.8619790058232168484, 0.8645833619440471685, 0.8671873368610717447, 0.8697916655744575287, 0.8723957256102774505, 0.8749999336500613456, 0.8776041439309557601, 0.8802082020090884473, 0.8828125319952765393, 0.8854165068757942070, 0.8880208632890512765, 0.8906248686864229880, 0.8932291467441429988, 0.8958332798131283248, 0.8984374104767501867, 0.9010416903237299380, 0.9036456946063434748, 0.9062500518360779855, 0.9088540278924787108, 0.9114583577202677311, 0.9140624189272162914, 0.9166666280927961985, 0.9192708395544209043, 0.9218748987838942810, 0.9244792299476556341, 0.9270832060181642964, 0.9296875636115721209, 0.9322915702365133228, 0.9348958494830461596, 0.9374999838014769216, 0.9401041156712998115, 0.9427083967663798525, 0.9453124022892170908, 0.9479167607665550666, 0.9505207380999710631, 0.9531250691809918241, 0.9557291317261836783, 0.9583333421310490374, 0.9609375547886240820, 0.9635416155522130710, 0.9661459483928183101, 0.9687499245033458495, 0.9713542829945021051, 0.9739582954330652242, 0.9765625745907361432, 0.9791667024412501474, 0.9817708385604039245, 0.9843751096149007118, 0.9869791944699233266, 0.9895836584107432499, 0.9921868132917668337, 0.9947911946869415489, 0.9973999724172807335, 1.000000000000000000 ),
 .UNSPECIFIED. ) ;
#105718 = CARTESIAN_POINT ( 'NONE',  ( 0.9794701899953797142, -0.05759512415488829418, -2.206297691287119722 ) ) ;
#105719 = CARTESIAN_POINT ( 'NONE',  ( 3.989755448363790258, 1.635235102580555155, 1.563706588500752837 ) ) ;
#105720 = CARTESIAN_POINT ( 'NONE',  ( -8.731087737520713432, 10.24898578427137963, 1.082531754730558626 ) ) ;
#105721 = CARTESIAN_POINT ( 'NONE',  ( 3.920002888225936566, -1.806327840557620412, 0.1390898763422818984 ) ) ;
#105722 = CARTESIAN_POINT ( 'NONE',  ( 4.540194369826378029, 0.7389084316076138803, 1.767693002002197034 ) ) ;
#105724 = EDGE_CURVE ( 'NONE', #129573, #134499, #69440, .T. ) ;
#105723 = CARTESIAN_POINT ( 'NONE',  ( 4.932118098221458524, 1.189261692661430114, 1.694535115018414917 ) ) ;
#105725 = CARTESIAN_POINT ( 'NONE',  ( -1.364683531250012516, 4.301041667008089320, -0.7879004041258300672 ) ) ;
#105726 = CARTESIAN_POINT ( 'NONE',  ( 2.606273030088624765, -0.7529636864501542126, -1.822200628222752972 ) ) ;
#105727 = CARTESIAN_POINT ( 'NONE',  ( 1.571183270939533694, 0.1444824169965253369, -1.921038573443895059 ) ) ;
#105728 = CARTESIAN_POINT ( 'NONE',  ( 4.012460596634464416, 1.323225596166040186, -1.322536486416127977 ) ) ;
#105729 = CARTESIAN_POINT ( 'NONE',  ( 2.983396891919448013, -0.1703749763015352803, -2.301462837838092135 ) ) ;
#105730 = CARTESIAN_POINT ( 'NONE',  ( 4.140933978860473985, -0.1807793374023874688, -1.852226635870577898 ) ) ;
#105731 = CARTESIAN_POINT ( 'NONE',  ( -1.201851678989727383E-14, 4.071875000341425022, 1.575800808251672791 ) ) ;
#105732 = CIRCLE ( 'NONE', #140204, 0.08000000000000040412 ) ;
#105733 = CARTESIAN_POINT ( 'NONE',  ( 6.313256805818848960, 7.394496357324014113, 1.199719254218452047 ) ) ;
#105734 = CARTESIAN_POINT ( 'NONE',  ( 6.287230548435207567, 8.358188277972981695, -1.599625672291262513 ) ) ;
#105735 = DIRECTION ( 'NONE',  ( 0.000000000000000000, 0.000000000000000000, 1.000000000000000000 ) ) ;
#105736 = CARTESIAN_POINT ( 'NONE',  ( 0.6453166446471610973, -1.805311040884694185, 1.084365637629558954 ) ) ;
#105737 = CIRCLE ( 'NONE', #129899, 3.150000000000000799 ) ;
#105738 = B_SPLINE_CURVE_WITH_KNOTS ( 'NONE', 3,
 ( #171137, #191634, #189519, #204680 ),
 .UNSPECIFIED., .F., .F.,
 ( 4, 4 ),
 ( 0.000000000000000000, 0.0006799945003891862041 ),
 .UNSPECIFIED. ) ;
#105739 = CARTESIAN_POINT ( 'NONE',  ( 3.294268137996273715, 5.826768013428865522, -1.082531754730543971 ) ) ;
#105741 = FACE_OUTER_BOUND ( 'NONE', #142693, .T. ) ;
#105740 = CARTESIAN_POINT ( 'NONE',  ( 1.364683531249988535, 5.717708333674752730, -0.7879004041258300672 ) ) ;
#105742 = CARTESIAN_POINT ( 'NONE',  ( -1.879585681373379114, 8.984805382992709255, -0.7749999999999996891 ) ) ;
#105743 = CARTESIAN_POINT ( 'NONE',  ( 1.898838059644195386, -2.080654286433290867, -0.4088066060855889972 ) ) ;
#105744 = CARTESIAN_POINT ( 'NONE',  ( -9.578206935409053102, -9.746166700193986898, 0.1671882239534360770 ) ) ;
#105745 = CARTESIAN_POINT ( 'NONE',  ( 0.9670638486888746277, -1.589497524861957611, 1.246053474203263178 ) ) ;
#105746 = CARTESIAN_POINT ( 'NONE',  ( 1.364683531249988535, 1.363541667008083769, 0.7879004041258500513 ) ) ;
#105747 = CARTESIAN_POINT ( 'NONE',  ( -2.955314298098991266, 6.391691081183366485, 0.7216878364870317197 ) ) ;
#105748 = CARTESIAN_POINT ( 'NONE',  ( 6.159481859310094620, 6.080483678816896109, 1.040834085586084257E-14 ) ) ;
#105749 = VERTEX_POINT ( 'NONE', #166514 ) ;
#105750 = CARTESIAN_POINT ( 'NONE',  ( 0.7202740732663616141, -1.155732025818452913, -1.826486478054230256 ) ) ;
#105751 = CARTESIAN_POINT ( 'NONE',  ( 5.688757509019037428, 5.629766575900002401, 2.420000000000000373 ) ) ;
#105754 = CARTESIAN_POINT ( 'NONE',  ( 4.528060117284244512, 4.385084346360807572, 0.7216878364870317197 ) ) ;
#105753 = CARTESIAN_POINT ( 'NONE',  ( 6.925078400183556582, 1.261064080992575498, 2.068696352333323052 ) ) ;
#105752 = CARTESIAN_POINT ( 'NONE',  ( 6.062430963966053632, 7.101866208495718702, -1.199719254218452047 ) ) ;
#105755 =( BOUNDED_SURFACE ( )  B_SPLINE_SURFACE ( 3, 2, ( 
 ( #110938, #145555, #14417 ),
 ( #210493, #77303, #13364 ),
 ( #194251, #78366, #209409 ),
 ( #93582, #159627, #96789 ),
 ( #130407, #129352, #80506 ),
 ( #146603, #95719, #162839 ) ),
 .UNSPECIFIED., .F., .F., .T. ) 
 B_SPLINE_SURFACE_WITH_KNOTS ( ( 4, 2, 4 ),
 ( 3, 3 ),
 ( 0.000000000000000000, 0.0003754691837024766443, 0.0007509383674049532886 ),
 ( 0.000000000000000000, 1.000000000000000000 ),
 .UNSPECIFIED. ) 
 GEOMETRIC_REPRESENTATION_ITEM ( )  RATIONAL_B_SPLINE_SURFACE ( (
 ( 1.000000000000000000, 0.6711954675835484219, 1.000000000000000000),
 ( 1.000000000000000000, 0.6709646295267019944, 1.000000000000000000),
 ( 1.000000000000000000, 0.6771840716659748294, 1.000000000000000000),
 ( 1.000000000000000000, 0.6927481755866885527, 1.000000000000000000),
 ( 1.000000000000000000, 0.7017972101310294697, 1.000000000000000000),
 ( 1.000000000000000000, 0.7071067811865475727, 1.000000000000000000) ) ) 
 REPRESENTATION_ITEM ( '' )  SURFACE ( )  );
#105756 = DIRECTION ( 'NONE',  ( 0.000000000000000000, -1.000000000000000000, 0.000000000000000000 ) ) ;
#105757 = CARTESIAN_POINT ( 'NONE',  ( 6.034388706570055660, 0.6371486477873434806, 1.913263546360920220 ) ) ;
#105758 = CARTESIAN_POINT ( 'NONE',  ( -7.212574532790087645, 11.35849468832304154, -0.7216878364870267237 ) ) ;
#105759 = EDGE_CURVE ( 'NONE', #123208, #105686, #105987, .T. ) ;
#105760 = CARTESIAN_POINT ( 'NONE',  ( 0.02921319935947005314, -2.001080581411585513, 0.8940957790435491992 ) ) ;
#105761 = DIRECTION ( 'NONE',  ( 0.000000000000000000, -0.3940140829290787461, 0.9191044023687172659 ) ) ;
#105763 = CARTESIAN_POINT ( 'NONE',  ( -1.364683531250000748, 10.60937500034139802, 0.000000000000000000 ) ) ;
#105762 = CARTESIAN_POINT ( 'NONE',  ( 0.2689492781585648418, -1.474829822998312778, 1.715830925988118816 ) ) ;
#105764 = CARTESIAN_POINT ( 'NONE',  ( -7.296259222448620463, 11.66405285949874759, 0.7998128361456481317 ) ) ;
#105766 = CARTESIAN_POINT ( 'NONE',  ( 1.124461781556247431, 0.3751114458506888405, 1.878329865892948813 ) ) ;
#105765 = CARTESIAN_POINT ( 'NONE',  ( -5.626270559546828309, 7.587068290936515247, 1.443375672974064550 ) ) ;
#105767 = CARTESIAN_POINT ( 'NONE',  ( 1.364683531249988757, 0.1968750003414204697, 0.000000000000000000 ) ) ;
#105768 = CARTESIAN_POINT ( 'NONE',  ( 4.450808633097238953, 7.987047222781201938, 2.500000000000000000 ) ) ;
#105769 = CARTESIAN_POINT ( 'NONE',  ( 0.7500000000000006661, 10.08333333333333215, 1.299038105676657340 ) ) ;
#105770 = CARTESIAN_POINT ( 'NONE',  ( 2.613528241349000858, -1.706151288242565567, 0.2525731233022251443 ) ) ;
#105771 = CARTESIAN_POINT ( 'NONE',  ( 5.391302360089590628, 6.318882837306503575, -1.199719254218452047 ) ) ;
#105772 = CARTESIAN_POINT ( 'NONE',  ( 2.512676673363742452, 1.578732364194649573, 0.7999210992828114097 ) ) ;
#105773 = CARTESIAN_POINT ( 'NONE',  ( 2.947904902976675068, -1.353543519239216897, -1.490266562291961749 ) ) ;
#105774 = EDGE_CURVE ( 'NONE', #50087, #28024, #149658, .T. ) ;
#105776 = CIRCLE ( 'NONE', #112599, 4.021913119055696484 ) ;
#105775 = CARTESIAN_POINT ( 'NONE',  ( 5.544034191846948900, 0.8990280053539388971, -2.015528879820461583 ) ) ;
#105777 = VERTEX_POINT ( 'NONE', #134054 ) ;
#105778 = CARTESIAN_POINT ( 'NONE',  ( 4.025652601906283046, -0.3410878217046057204, 1.990599050954243054 ) ) ;
#105779 = CARTESIAN_POINT ( 'NONE',  ( -6.668631453075260396, 8.873432343378178544, -1.599625672291271394 ) ) ;
#105781 = CARTESIAN_POINT ( 'NONE',  ( 4.235953958900400274, 2.015913684659226490, -0.05231418598541925924 ) ) ;
#105780 = CARTESIAN_POINT ( 'NONE',  ( 4.160867320283115234, 0.5667376361006767338, 2.043264482828925033 ) ) ;
#105783 = ORIENTED_EDGE ( 'NONE', *, *, #203843, .T. ) ;
#105782 = CARTESIAN_POINT ( 'NONE',  ( 4.201270403262004294, 1.615401881959299235, -0.8201500932763347018 ) ) ;
#105784 = CARTESIAN_POINT ( 'NONE',  ( 5.306037014901791693, 7.283738832175834510, 1.599625672291269396 ) ) ;
#105785 = ORIENTED_EDGE ( 'NONE', *, *, #148663, .T. ) ;
#105786 = CARTESIAN_POINT ( 'NONE',  ( 1.463515404423965105, 1.843522461416190250, -0.3164952454337774390 ) ) ;
#105787 = CARTESIAN_POINT ( 'NONE',  ( -10.91804383151480806, -9.907361309732431565, 0.1905751639681794174 ) ) ;
#105788 = CARTESIAN_POINT ( 'NONE',  ( 6.234996492879100849, 1.692908850720629799, 0.6451080659017217611 ) ) ;
#105790 = TOROIDAL_SURFACE ( 'NONE', #81157, 2.080000000000000071, 0.08000000000000000167 ) ;
#105789 = CARTESIAN_POINT ( 'NONE',  ( -4.277761160311629673, 4.949475094240346706, 1.199719254218462483 ) ) ;
#105791 = DIRECTION ( 'NONE',  ( 0.000000000000000000, -1.000000000000000000, 0.000000000000000000 ) ) ;
#105792 = CARTESIAN_POINT ( 'NONE',  ( -1.500000000000008216, 8.781250000682797818, 3.469446951953614189E-15 ) ) ;
#105793 = CARTESIAN_POINT ( 'NONE',  ( 1.364683531249988535, 2.426041667008088432, 0.7879004041258500513 ) ) ;
#105794 = LINE ( 'NONE', #155576, #212590 ) ;
#105795 = ORIENTED_EDGE ( 'NONE', *, *, #86135, .T. ) ;
#105796 = AXIS2_PLACEMENT_3D ( 'NONE', #81594, #183357, #182279 ) ;
#105797 = CARTESIAN_POINT ( 'NONE',  ( 5.722950238744187956, 9.690876021928001904, 0.7216878364870317197 ) ) ;
#105798 = CARTESIAN_POINT ( 'NONE',  ( -4.925354943514475003, 8.968274210734028529, 0.000000000000000000 ) ) ;
#105799 = CARTESIAN_POINT ( 'NONE',  ( 4.166350089634453191, 2.120059694336435374, -0.05518752902338577848 ) ) ;
#105801 = CARTESIAN_POINT ( 'NONE',  ( -9.986127180934126102, 5.615481227002261377, 5.966285604742011195 ) ) ;
#105800 = CARTESIAN_POINT ( 'NONE',  ( 2.450294804891584022, 1.972237431424222809, -11.52773071619440692 ) ) ;
#105802 = CARTESIAN_POINT ( 'NONE',  ( 5.571542166969843279, 1.900665388187183114, -0.5230325980125193341 ) ) ;
#105803 = CARTESIAN_POINT ( 'NONE',  ( -0.6823417656250212460, 0.8010416670080899859, 1.181850606188755259 ) ) ;
#105804 = CARTESIAN_POINT ( 'NONE',  ( 1.090090997392887173, 1.202455520763350272, 1.614487003566661638 ) ) ;
#105805 = EDGE_LOOP ( 'NONE', ( #185308, #24555, #130951, #153943 ) ) ;
#105806 = CARTESIAN_POINT ( 'NONE',  ( 0.2107725088618967457, 2.027540257690120029, 0.6097772466436711669 ) ) ;
#105807 = CARTESIAN_POINT ( 'NONE',  ( -0.04945587076000566851, 6.344066507677029065, -3.092088676902647659 ) ) ;
#105808 = CARTESIAN_POINT ( 'NONE',  ( 1.785682506433339478, -1.950172559450613852, 0.6955597780969878796 ) ) ;
#105809 = CARTESIAN_POINT ( 'NONE',  ( 4.854701522145073334, 7.821512988214679218, -1.199719254218450271 ) ) ;
#105810 = CARTESIAN_POINT ( 'NONE',  ( 5.737035277238070385, 6.722237907313067140, -1.199719254218452047 ) ) ;
#105812 = CARTESIAN_POINT ( 'NONE',  ( 6.328958779480917229, 6.278206752349526631, 0.7998128361456341429 ) ) ;
#105811 = CARTESIAN_POINT ( 'NONE',  ( 4.259774723613071856, 0.9852665271268057356, 1.843911019796584450 ) ) ;
#105813 = CARTESIAN_POINT ( 'NONE',  ( 7.198453214212898743, 7.362893269528701268, 0.7998128361456291469 ) ) ;
#105816 = ORIENTED_EDGE ( 'NONE', *, *, #136635, .F. ) ;
#105815 = CARTESIAN_POINT ( 'NONE',  ( 2.121461778293322276, -0.3959642608444019496, 1.767488790605805438 ) ) ;
#105814 = CARTESIAN_POINT ( 'NONE',  ( 2.783998052563033010, -0.9402290988879957734, 1.564698673013890984 ) ) ;
#105817 = CARTESIAN_POINT ( 'NONE',  ( 8.516493047678546091, 13.08765898893368629, -0.7998128361456352531 ) ) ;
#105818 = CARTESIAN_POINT ( 'NONE',  ( 0.000000000000000000, 13.88000000000000078, 0.000000000000000000 ) ) ;
#105819 = CARTESIAN_POINT ( 'NONE',  ( 3.979664642534729513, 2.078844338038158934, -0.7408291028327751437 ) ) ;
#105820 = CARTESIAN_POINT ( 'NONE',  ( 6.958359152311676787, 9.141171649162195934, -1.599625672291262513 ) ) ;
#105821 = LINE ( 'NONE', #192342, #106703 ) ;
#105822 = CARTESIAN_POINT ( 'NONE',  ( 3.000541214264150547, -1.884352459892328024, -0.3246530749497905655 ) ) ;
#105823 = CARTESIAN_POINT ( 'NONE',  ( 6.747154001095143627, 11.02343010125301959, -0.7998128361456291469 ) ) ;
#105824 = CARTESIAN_POINT ( 'NONE',  ( 6.830528382861658088, -1.277203763263988101, 1.630111558092485868 ) ) ;
#105825 = CARTESIAN_POINT ( 'NONE',  ( 1.510814038188205366, 8.678413394653590629, -2.539834060596333210 ) ) ;
#105826 = CARTESIAN_POINT ( 'NONE',  ( 5.952700804540857149, -1.878875186057769486, -1.127905468421293689 ) ) ;
#105827 = CARTESIAN_POINT ( 'NONE',  ( 5.364607279338250656, 7.693244595681929532, -1.319704323257679057 ) ) ;
#105828 = EDGE_LOOP ( 'NONE', ( #47917, #197164, #167685, #21026 ) ) ;
#105829 = EDGE_CURVE ( 'NONE', #117790, #90065, #2914, .T. ) ;
#105830 = DIRECTION ( 'NONE',  ( -1.000000000000000000, 7.771561172376094797E-16, -3.330669073875481454E-16 ) ) ;
#105831 = CARTESIAN_POINT ( 'NONE',  ( 5.086243903782109221, 5.962981304947771122, -1.199719254218452047 ) ) ;
#105832 = CARTESIAN_POINT ( 'NONE',  ( 1.642778471875000035, -1.713541666188707291, -2.845375778867859751 ) ) ;
#105833 = CARTESIAN_POINT ( 'NONE',  ( -0.2409995289980246258, 2.020898751655671788, -2.415740196953279462 ) ) ;
#105834 = CARTESIAN_POINT ( 'NONE',  ( -8.853111120043687166, 9.430977182913531820, 1.040834085586084257E-14 ) ) ;
#105835 = CARTESIAN_POINT ( 'NONE',  ( 3.386504508363381571, 7.172948703057747011, -0.7998128361456362523 ) ) ;
#105836 = CARTESIAN_POINT ( 'NONE',  ( 5.366107254901440804, -2.060797467674013284, 0.1973761227843511823 ) ) ;
#105837 = CARTESIAN_POINT ( 'NONE',  ( 4.494702926938664689, -0.4234472454235098104, -1.879237243589318318 ) ) ;
#105838 = CARTESIAN_POINT ( 'NONE',  ( 0.5972800738224989248, -0.2930464221381040013, 1.994874516246990748 ) ) ;
#105839 = CARTESIAN_POINT ( 'NONE',  ( -9.755255220232635693, 11.33988483081495957, -1.199719254218441611 ) ) ;
#105840 = CARTESIAN_POINT ( 'NONE',  ( 7.075376061485196821, 9.347967719856493218, 1.599625672291268286 ) ) ;
#105841 = CARTESIAN_POINT ( 'NONE',  ( -0.5773502691896470473, -2.500000000000002220, 0.9999999999999991118 ) ) ;
#105842 = CARTESIAN_POINT ( 'NONE',  ( 1.535386672163775668, -1.589036399888818618, -1.509351277865833563 ) ) ;
#105843 = CARTESIAN_POINT ( 'NONE',  ( 5.250558533952181861, 0.5335417292645014964, 1.745990657226546894 ) ) ;
#105844 = CARTESIAN_POINT ( 'NONE',  ( -4.249591082879585535, 7.045274465746411252, 1.199719254218464037 ) ) ;
#105845 = CARTESIAN_POINT ( 'NONE',  ( 6.048345925472183637, 8.149765894507963182, 1.443375672974065660 ) ) ;
#105846 = CARTESIAN_POINT ( 'NONE',  ( 10.58621901417202515, 11.24501035948919991, -0.7998128361456281477 ) ) ;
#105847 = EDGE_CURVE ( 'NONE', #106531, #92739, #47776, .T. ) ;
#105848 = CARTESIAN_POINT ( 'NONE',  ( -4.782994330570982555, 8.802186828966616972, 0.000000000000000000 ) ) ;
#105849 = CARTESIAN_POINT ( 'NONE',  ( 3.842846474469570062, 6.570739089268092137, -1.199719254218452047 ) ) ;
#105850 = CARTESIAN_POINT ( 'NONE',  ( 4.309512724297349884, 6.121127159803966933, 1.599625672291261402 ) ) ;
#105851 = VERTEX_POINT ( 'NONE', #213106 ) ;
#105853 = CARTESIAN_POINT ( 'NONE',  ( -0.02280469861281903335, -1.799075986276091887, -0.9034098368623093567 ) ) ;
#105852 = CARTESIAN_POINT ( 'NONE',  ( 2.893917256732419396, -0.5369380550670297403, -1.761199466696103499 ) ) ;
#105854 = CARTESIAN_POINT ( 'NONE',  ( 2.109147326763362695, 0.8800818102412102384, -2.123382460422203355 ) ) ;
#105856 = CARTESIAN_POINT ( 'NONE',  ( 6.385602409055195494, -1.848352663145738095, 0.6577735930803210174 ) ) ;
#105855 = CARTESIAN_POINT ( 'NONE',  ( 4.717874267875568961, 4.606534188717351874, -0.7216878364870188411 ) ) ;
#105857 = CARTESIAN_POINT ( 'NONE',  ( -6.013204822860843457, 6.974159367214481264, -1.199719254218446718 ) ) ;
#105858 = CARTESIAN_POINT ( 'NONE',  ( 10.93005900490892834, -6.124285369217931319, 9.269928574751062911E-15 ) ) ;
#105859 = CARTESIAN_POINT ( 'NONE',  ( 3.076317393561965208, 0.8638369986560844316, 1.706277067364105893 ) ) ;
#105860 = CARTESIAN_POINT ( 'NONE',  ( -10.32183501870554387, 10.93656236477829502, 0.7998128361456462443 ) ) ;
#105861 = CARTESIAN_POINT ( 'NONE',  ( 0.3970419974134197783, 0.3524218036512065111, 2.039982198586967943 ) ) ;
#105862 = CARTESIAN_POINT ( 'NONE',  ( -5.144392941742557568, 4.966489618313220333, -0.7998128361456362523 ) ) ;
#105864 = CARTESIAN_POINT ( 'NONE',  ( 0.9888773766892227091, 1.651582696977689890, -0.8784067438419729257 ) ) ;
#105863 = CARTESIAN_POINT ( 'NONE',  ( 2.876600747729184615, -0.1562720264073799992, -2.084980456524800019 ) ) ;
#105865 = CARTESIAN_POINT ( 'NONE',  ( 2.389999771189327937, -0.002812746694069029330, 2.016288306988550438 ) ) ;
#105866 = CARTESIAN_POINT ( 'NONE',  ( 9.083599731475992201, 9.699880562917908122, 0.7216878364870438212 ) ) ;
#105867 = ORIENTED_EDGE ( 'NONE', *, *, #6305, .T. ) ;
#105868 = CARTESIAN_POINT ( 'NONE',  ( -1.201851678989727383E-14, 4.759375000341420581, -1.575800808251660134 ) ) ;
#105869 = CARTESIAN_POINT ( 'NONE',  ( 3.192619200838729743, 1.373927285412982036, 1.068286041690246657 ) ) ;
#105870 = CARTESIAN_POINT ( 'NONE',  ( 4.416205349749311004, 6.175325546172740765, 1.599625672291267398 ) ) ;
#105872 = CARTESIAN_POINT ( 'NONE',  ( 0.2075773638182398517, 2.642062557107526022, -2.068677247530675611 ) ) ;
#105871 = CARTESIAN_POINT ( 'NONE',  ( -5.436182321379713578, 6.108390213082993903, 1.083092214668917919 ) ) ;
#105873 = CARTESIAN_POINT ( 'NONE',  ( 2.543205433794017978, -1.277680944696883092, -1.158960206811429750 ) ) ;
#105874 = CARTESIAN_POINT ( 'NONE',  ( 2.665787806004877414, 1.174844384069907655, 1.849873475113596566 ) ) ;
#105875 = CARTESIAN_POINT ( 'NONE',  ( 0.03525962724756306205, -1.394606873943932346, 1.030409205853829668 ) ) ;
#105876 = CARTESIAN_POINT ( 'NONE',  ( 5.004599478379411437, -0.7411955310945415043, -2.078817424605138964 ) ) ;
#105877 = CARTESIAN_POINT ( 'NONE',  ( -9.470156251935129887, 4.005132839944305800, -6.837168546664702085 ) ) ;
#105878 = SURFACE_STYLE_FILL_AREA ( #122175 ) ;
#105879 = CARTESIAN_POINT ( 'NONE',  ( 3.133805249272236804, 2.063032676455050396, -0.6766426178266419234 ) ) ;
#105880 = CARTESIAN_POINT ( 'NONE',  ( 2.174178736149934732, -1.123764393468742684, 1.438770255985911684 ) ) ;
#105881 = DIRECTION ( 'NONE',  ( -0.000000000000000000, -1.000000000000000000, -0.000000000000000000 ) ) ;
#105882 = CARTESIAN_POINT ( 'NONE',  ( 4.030539441936417333, 0.5683090829115284848, 2.039553408600587758 ) ) ;
#105883 = CARTESIAN_POINT ( 'NONE',  ( 6.539320575229228716, 1.281788455817688188, 2.013036689384885225 ) ) ;
#105884 = VERTEX_POINT ( 'NONE', #50626 ) ;
#105886 = CARTESIAN_POINT ( 'NONE',  ( -1.364683531250014514, 1.551041667008084435, -0.7879004041258289570 ) ) ;
#105885 = CARTESIAN_POINT ( 'NONE',  ( 5.056304237002312796, -1.661761009075436002, 1.579303468685322009 ) ) ;
#105887 = LINE ( 'NONE', #190278, #181740 ) ;
#105888 = CARTESIAN_POINT ( 'NONE',  ( 4.376584659113025744, 4.000436945253625254, 0.7998128361456341429 ) ) ;
#105889 = CARTESIAN_POINT ( 'NONE',  ( 0.01256502854718108061, -2.120115106878577294, -0.04748564598491820943 ) ) ;
#105890 = CARTESIAN_POINT ( 'NONE',  ( -4.582292731738899505, 8.289832587096611860, 0.7216878364870458196 ) ) ;
#105891 = AXIS2_PLACEMENT_3D ( 'NONE', #39309, #6782, #105404 ) ;
#105892 = CARTESIAN_POINT ( 'NONE',  ( 5.178851490740207453, 5.144340948726102702, 0.7216878364870317197 ) ) ;
#105893 = CARTESIAN_POINT ( 'NONE',  ( -5.219525951136837705, 9.033271343060892633, -0.7216878364870207285 ) ) ;
#105894 = CARTESIAN_POINT ( 'NONE',  ( 1.868950538045364596, 0.000000000000000000, -0.4856446947087145194 ) ) ;
#105896 = ORIENTED_EDGE ( 'NONE', *, *, #123967, .F. ) ;
#105895 = AXIS2_PLACEMENT_3D ( 'NONE', #172290, #207963, #72635 ) ;
#105897 = CARTESIAN_POINT ( 'NONE',  ( 5.221327349844218091, 1.987046161919112430, 0.3419379449052239450 ) ) ;
#105899 = CARTESIAN_POINT ( 'NONE',  ( 3.467685518289661317, -0.4070155273973393717, 2.021854410566482407 ) ) ;
#105898 = CARTESIAN_POINT ( 'NONE',  ( 5.986088515633498197, 6.942523675449257858, -1.199719254218446718 ) ) ;
#105901 = CARTESIAN_POINT ( 'NONE',  ( -0.1408020194050510487, 6.947782644136224484, -2.695327183700791274 ) ) ;
#105900 = CARTESIAN_POINT ( 'NONE',  ( 0.000000000000000000, -0.5000000000000004441, 0.000000000000000000 ) ) ;
#105902 = CARTESIAN_POINT ( 'NONE',  ( 5.356880090730874677, 5.422317325373725794, 0.7216878364870328300 ) ) ;
#105903 = CARTESIAN_POINT ( 'NONE',  ( -1.642778471875000035, -0.5177083328553738761, -2.845375778867859751 ) ) ;
#105904 = CARTESIAN_POINT ( 'NONE',  ( 2.725000000000005862, 0.000000000000000000, 0.000000000000000000 ) ) ;
#105905 = CARTESIAN_POINT ( 'NONE',  ( 6.140607899229072686, -1.853288307406484758, 1.169240172944140621 ) ) ;
#105906 = CARTESIAN_POINT ( 'NONE',  ( 3.340470361411255418, 0.4872029778183216697, -1.956561305313428978 ) ) ;
#105907 = CARTESIAN_POINT ( 'NONE',  ( 3.579498943475650563, -0.9044721095569520086, 1.603693017070174864 ) ) ;
#105908 = EDGE_CURVE ( 'NONE', #69998, #212421, #130837, .T. ) ;
#105909 = CARTESIAN_POINT ( 'NONE',  ( 5.819474248763732760, 7.812472595022922128, -1.599625672291262513 ) ) ;
#105910 = SURFACE_STYLE_FILL_AREA ( #158883 ) ;
#105911 = CARTESIAN_POINT ( 'NONE',  ( 0.7797844759148920835, -0.9637546898726162548, 1.430169641563599159 ) ) ;
#105912 = CARTESIAN_POINT ( 'NONE',  ( 0.2121463357745425049, 2.202340261784305753, 0.6586529460593565366 ) ) ;
#105913 = CARTESIAN_POINT ( 'NONE',  ( -5.201524489137236529, 9.220195670635433771, 0.7998128361456481317 ) ) ;
#105914 = CARTESIAN_POINT ( 'NONE',  ( 6.596538519236475828, -0.5955016034951933213, -2.182694285642503562 ) ) ;
#105915 = CARTESIAN_POINT ( 'NONE',  ( 1.699976503534783356, -0.7083771898081425711, 1.983499743616623956 ) ) ;
#105916 = CARTESIAN_POINT ( 'NONE',  ( -5.906512197408906317, 6.919960980845699439, -1.199719254218453823 ) ) ;
#105917 = CARTESIAN_POINT ( 'NONE',  ( 6.401421083946654100, 10.62007503124645957, -0.7998128361456291469 ) ) ;
#105918 = CARTESIAN_POINT ( 'NONE',  ( 6.848276988234151652, 7.162280372460873679, -0.7216878364870317197 ) ) ;
#105919 =( NAMED_UNIT ( * ) PLANE_ANGLE_UNIT ( ) SI_UNIT ( $, .RADIAN. ) );
#105920 = CARTESIAN_POINT ( 'NONE',  ( -6.521635583373313061, 7.567328587812373719, -1.199719254218446718 ) ) ;
#105921 = B_SPLINE_CURVE_WITH_KNOTS ( 'NONE', 3,
 ( #198079, #99530, #114771, #47602, #181821, #179720 ),
 .UNSPECIFIED., .F., .F.,
 ( 4, 2, 4 ),
 ( 0.001491904891164481895, 0.001547600839949546002, 0.001603296788734610108 ),
 .UNSPECIFIED. ) ;
#105922 = CARTESIAN_POINT ( 'NONE',  ( 7.768458830506048685, 8.165549511786275971, -0.7216878364870267237 ) ) ;
#105923 = CARTESIAN_POINT ( 'NONE',  ( 5.545980446453017798, 6.390169355917580951, 1.218016560845627483 ) ) ;
#105924 = CARTESIAN_POINT ( 'NONE',  ( -4.303823697334223652, 7.108545849276850959, -1.199719254218452047 ) ) ;
#105926 = CARTESIAN_POINT ( 'NONE',  ( 4.148835382215973588, 2.178989060337086503, 0.4312644480095380040 ) ) ;
#105925 = CARTESIAN_POINT ( 'NONE',  ( 2.162495577681341707, 2.120227376586072854, 0.04728746717985036346 ) ) ;
#105927 = CARTESIAN_POINT ( 'NONE',  ( 2.133021248740565756, -1.956732443736847182, 0.9868821405488172882 ) ) ;
#105928 = CARTESIAN_POINT ( 'NONE',  ( -4.726989112658928072, 8.666571064744069020, 1.040834085586084257E-14 ) ) ;
#105929 = CARTESIAN_POINT ( 'NONE',  ( 6.883263157960364254, 2.447565407927353220, 2.329071302269662080 ) ) ;
#105930 = CARTESIAN_POINT ( 'NONE',  ( -5.743814354044916470, 6.730146830254374990, -1.199719254218453823 ) ) ;
#105931 = CARTESIAN_POINT ( 'NONE',  ( 5.019951445752288244, 1.940773837913706057, -0.2859759768028962146 ) ) ;
#105932 = DIRECTION ( 'NONE',  ( 1.040834085586084257E-15, 1.000000000000000000, -4.622230424712076367E-32 ) ) ;
#105933 = CARTESIAN_POINT ( 'NONE',  ( 1.364683531249988757, 1.884375000341421913, 0.000000000000000000 ) ) ;
#105934 = CARTESIAN_POINT ( 'NONE',  ( 6.610000000000018083, 6.039292104641935666, 2.314898989754467618 ) ) ;
#105936 = CARTESIAN_POINT ( 'NONE',  ( -6.575341312947811545, 6.773579074634973551, 1.040834085586084257E-14 ) ) ;
#105935 = AXIS2_PLACEMENT_3D ( 'NONE', #119656, #51402, #37273 ) ;
#105937 = CARTESIAN_POINT ( 'NONE',  ( 4.131183091185314460, 1.940096312829143299, 0.8565103500411813675 ) ) ;
#105938 = CARTESIAN_POINT ( 'NONE',  ( -4.122561227007127016, 6.967349310553715647, 1.199719254218452935 ) ) ;
#105939 = VERTEX_POINT ( 'NONE', #182751 ) ;
#105940 = CARTESIAN_POINT ( 'NONE',  ( 5.752838164830007983, -1.706859214253673152, 1.326403591387192771 ) ) ;
#105941 = CARTESIAN_POINT ( 'NONE',  ( 6.681470773436232413, 6.689470745297396270, -0.7998128361456281477 ) ) ;
#105942 = CARTESIAN_POINT ( 'NONE',  ( 5.319803798718575116, 1.092037692397327620, -1.482314076171886708 ) ) ;
#105943 = CARTESIAN_POINT ( 'NONE',  ( -5.908080316777766683, 6.002527095666024159, -0.1116623552285273685 ) ) ;
#105944 = CARTESIAN_POINT ( 'NONE',  ( -1.364683531250012516, 1.842708333674749843, 0.7879004041258379498 ) ) ;
#105945 = CARTESIAN_POINT ( 'NONE',  ( 0.01074006189176902708, -1.707493591921129372, 0.3360247309564004525 ) ) ;
#105946 = CARTESIAN_POINT ( 'NONE',  ( 6.727182134110222478, 0.005875948494733079785, 1.810970247402940547 ) ) ;
#105947 = CARTESIAN_POINT ( 'NONE',  ( 0.3999999999999719891, 3.096232863981052574, 2.023857702508392364 ) ) ;
#105948 = CARTESIAN_POINT ( 'NONE',  ( 11.53060642766661736, 7.261346649532379516, 3.356656312893389948 ) ) ;
#105949 = CARTESIAN_POINT ( 'NONE',  ( 4.487301133948972343, 1.932317252032596633, -0.9692046190768679459 ) ) ;
#105950 = CARTESIAN_POINT ( 'NONE',  ( -4.680589345215810049, 6.483773540883647435, -1.599625672291256295 ) ) ;
#105951 = COLOUR_RGB ( '', 0.40784314, 0.44705882, 0.49803922) ;
#105952 = CARTESIAN_POINT ( 'NONE',  ( 6.397814513887354337, 0.1948139983735352188, 2.006652364629394114 ) ) ;
#105953 = CARTESIAN_POINT ( 'NONE',  ( -7.904040366642703930, 10.24446639921506552, 1.443375672974090751 ) ) ;
#105954 = CARTESIAN_POINT ( 'NONE',  ( 3.028364643526501698, 1.202066397148596977, -1.796461956351296019 ) ) ;
#105955 = CARTESIAN_POINT ( 'NONE',  ( 4.376219360443936779, -1.137518282590570751, 1.609873005976544924 ) ) ;
#105956 = CARTESIAN_POINT ( 'NONE',  ( 4.147546876296400065, -0.1688817038796013026, -1.725555368340276008 ) ) ;
#105957 = CARTESIAN_POINT ( 'NONE',  ( 0.3104468679729632807, 1.506874830639578056, -1.591553791636945991 ) ) ;
#105958 = CARTESIAN_POINT ( 'NONE',  ( 1.290513193724596164, -1.035378025537621927, 2.062353807931560645 ) ) ;
#105959 = CARTESIAN_POINT ( 'NONE',  ( 3.532544388643095612, 2.009728383178956523, 0.4550750861811359571 ) ) ;
#105960 = CARTESIAN_POINT ( 'NONE',  ( 5.794467663293456638, 1.585267558806532362, -1.121583357746269050 ) ) ;
#105963 = VERTEX_POINT ( 'NONE', #214146 ) ;
#105962 = ADVANCED_FACE ( 'NONE', ( #68987 ), #179178, .T. ) ;
#105961 = CARTESIAN_POINT ( 'NONE',  ( -8.636180661780668899, 10.13826086257468795, -1.082531754730543083 ) ) ;
#105964 = VECTOR ( 'NONE', #122484, 1000.000000000000000 ) ;
#105965 = CARTESIAN_POINT ( 'NONE',  ( -4.685224601974262271, 7.623789914682047808, -1.199719254218453823 ) ) ;
#105966 = FACE_OUTER_BOUND ( 'NONE', #186162, .T. ) ;
#105968 = ORIENTED_EDGE ( 'NONE', *, *, #144738, .T. ) ;
#105967 = CARTESIAN_POINT ( 'NONE',  ( -4.516801452008150086, 5.298631777878131111, 1.199719254218452935 ) ) ;
#105969 = CARTESIAN_POINT ( 'NONE',  ( -8.310784975052689205, 8.798263347090697906, -0.7216878364870267237 ) ) ;
#105970 = CARTESIAN_POINT ( 'NONE',  ( 3.012930935654754450, 1.599341701681813444, -1.520756135150652222 ) ) ;
#105971 = CARTESIAN_POINT ( 'NONE',  ( 1.642778471875001811, -3.580208332855376430, 2.845375778867859751 ) ) ;
#105972 = ORIENTED_EDGE ( 'NONE', *, *, #166038, .F. ) ;
#105973 = CARTESIAN_POINT ( 'NONE',  ( 1.252544054828262476, -0.4453625992760417707, -1.806759803163625167 ) ) ;
#105974 = CARTESIAN_POINT ( 'NONE',  ( -0.02900071798683095947, 1.997299723774683455, -2.587491137808914488 ) ) ;
#105975 = CARTESIAN_POINT ( 'NONE',  ( 1.499999999999991118, 5.285416667349480235, 0.8660254037844524744 ) ) ;
#105976 = CARTESIAN_POINT ( 'NONE',  ( 4.566373025097719029, 7.183545020864719355, -1.317121582780217404 ) ) ;
#105978 = CARTESIAN_POINT ( 'NONE',  ( -10.99931692196006949, -8.074346042903137288, 0.1488091642035881401 ) ) ;
#105977 = DIRECTION ( 'NONE',  ( 0.6507913734559641616, -0.7592566023653004592, 0.000000000000000000 ) ) ;
#105979 = CARTESIAN_POINT ( 'NONE',  ( 6.140549721451361798, -1.552764191669778304, 0.9890077265983505672 ) ) ;
#105980 = ORIENTED_EDGE ( 'NONE', *, *, #130371, .F. ) ;
#105981 = CARTESIAN_POINT ( 'NONE',  ( 2.254824865002862389, -1.593768082018555354, 1.306595953347834849 ) ) ;
#105982 = CARTESIAN_POINT ( 'NONE',  ( -1.360316468750030650, 0.8697916670080861890, -0.7853790794159041244 ) ) ;
#105983 = EDGE_CURVE ( 'NONE', #113870, #118245, #113524, .T. ) ;
#105984 = CARTESIAN_POINT ( 'NONE',  ( -5.856232286098998152, 8.919689202835742847, 1.199719254218452047 ) ) ;
#105985 =( LENGTH_UNIT ( ) NAMED_UNIT ( * ) SI_UNIT ( .MILLI., .METRE. ) );
#105986 = CARTESIAN_POINT ( 'NONE',  ( 11.86145016429273191, 10.90000000000000036, 1.099999999999996980 ) ) ;
#105987 = B_SPLINE_CURVE_WITH_KNOTS ( 'NONE', 3,
 ( #770, #118895, #98318, #115683 ),
 .UNSPECIFIED., .F., .F.,
 ( 4, 4 ),
 ( 0.0006145506151576765911, 0.0009333549826883593510 ),
 .UNSPECIFIED. ) ;
#105988 = CARTESIAN_POINT ( 'NONE',  ( 4.871457266011829823, 4.577788319968905562, -0.7998128361456221525 ) ) ;
#105989 = CARTESIAN_POINT ( 'NONE',  ( 0.5497720567373615141, 0.6472090466588500401, -1.956683156177397853 ) ) ;
#105991 = CARTESIAN_POINT ( 'NONE',  ( 5.126429434416579056, 0.1410513515392505246, 1.835921608166577013 ) ) ;
#105990 = PLANE ( 'NONE',  #34973 ) ;
#105992 = CARTESIAN_POINT ( 'NONE',  ( 7.156006149914539982, 7.243095351188763686, 1.040834085586084257E-14 ) ) ;
#105993 = CARTESIAN_POINT ( 'NONE',  ( -5.306037014901836990, 7.283738832175834510, 1.599625672291263179 ) ) ;
#105994 =( NAMED_UNIT ( * ) SI_UNIT ( $, .STERADIAN. ) SOLID_ANGLE_UNIT ( ) );
#105995 = CARTESIAN_POINT ( 'NONE',  ( 4.635508124736155366, -2.018492079602551392, 0.8926152185086615454 ) ) ;
#105996 = CARTESIAN_POINT ( 'NONE',  ( 6.889870058830950938, -0.9756824853745720283, 2.038933460117636542 ) ) ;
#105997 = CARTESIAN_POINT ( 'NONE',  ( -6.087247782855839340, 6.204136622861004646, 0.000000000000000000 ) ) ;
#105998 = CARTESIAN_POINT ( 'NONE',  ( 0.5801457039020865292, 0.9447208859736742070, 1.662703529197881558 ) ) ;
#105999 = CARTESIAN_POINT ( 'NONE',  ( 1.024625454658374624, 0.3981145430279106057, 1.976669095394629982 ) ) ;
#106000 = CARTESIAN_POINT ( 'NONE',  ( -6.901817408925782438, -6.554751161430547590, 6.500815859342965908 ) ) ;
#106001 = CARTESIAN_POINT ( 'NONE',  ( 1.388484499181727561, -0.05552238045265603383, 2.297868740670248044 ) ) ;
#106002 = CARTESIAN_POINT ( 'NONE',  ( 6.754772315933175619, -1.444328698515121800, 1.188528157999017454 ) ) ;
#106003 = DIRECTION ( 'NONE',  ( 0.000000000000000000, 0.000000000000000000, -1.000000000000000000 ) ) ;
#106004 = CARTESIAN_POINT ( 'NONE',  ( 11.35610322553117157, 12.48578371070824744, -3.553412924323506861 ) ) ;
#106005 = CARTESIAN_POINT ( 'NONE',  ( 1.322894217037654085, -0.04941562205608432401, 1.870173573632450958 ) ) ;
#106006 = CARTESIAN_POINT ( 'NONE',  ( 2.307827663788959871, -1.164988201124015577, -1.645758576239789051 ) ) ;
#106008 = CARTESIAN_POINT ( 'NONE',  ( 6.639320575229257670, 4.691717626494606996, 2.665852771288126366 ) ) ;
#106007 = CARTESIAN_POINT ( 'NONE',  ( -1.402160292154681736E-14, 0.3218750003414227456, 1.575800808251672791 ) ) ;
#106010 = CARTESIAN_POINT ( 'NONE',  ( 4.793641967770590817, 1.559994068796449529, 1.415095702743226047 ) ) ;
#106009 = CARTESIAN_POINT ( 'NONE',  ( -6.828502922777144768, 11.11833717654868892, 0.7998128361456481317 ) ) ;
#106011 = CARTESIAN_POINT ( 'NONE',  ( 7.690499447449630210, 9.995335326823163058, 1.599625672291281386 ) ) ;
#106013 = CARTESIAN_POINT ( 'NONE',  ( -6.692921386640485082, 10.96015871772258521, -0.7998128361456291469 ) ) ;
#106012 = CARTESIAN_POINT ( 'NONE',  ( 4.923546060418115822, 5.773167154356443120, -1.199719254218452047 ) ) ;
#106015 = CARTESIAN_POINT ( 'NONE',  ( 1.382971907303421233, 3.383593057718003561, -0.2136448034514799310 ) ) ;
#106014 = B_SPLINE_CURVE_WITH_KNOTS ( 'NONE', 3,
 ( #54958, #146352, #196146, #33629, #213425, #65047, #131204, #212364, #179895, #164701, #30452 ),
 .UNSPECIFIED., .F., .F.,
 ( 4, 1, 1, 1, 1, 1, 1, 1, 4 ),
 ( 0.000000000000000000, 0.2256085737580844630, 0.3975982043691296264, 0.5251069566405043298, 0.6172860083021659561, 0.6832860984239963464, 0.7321959383537668398, 0.7728624839797392232, 1.000000000000000000 ),
 .UNSPECIFIED. ) ;
#106016 = CARTESIAN_POINT ( 'NONE',  ( 3.972919405334675691, -1.493746422221740699, 1.359666112553897355 ) ) ;
#106017 = CARTESIAN_POINT ( 'NONE',  ( 1.364683531249990311, 4.613541667008083103, 0.7879004041258500513 ) ) ;
#106018 = CARTESIAN_POINT ( 'NONE',  ( 6.303195905902406970, -1.744534168554587872, 1.100284471152054300 ) ) ;
#106019 = CARTESIAN_POINT ( 'NONE',  ( 7.754900677336718395, 11.99120852362745460, -0.7216878364870267237 ) ) ;
#106020 = CARTESIAN_POINT ( 'NONE',  ( 4.763041337456088264, -1.928505312680216743, -0.9765951867335492809 ) ) ;
#106021 = CARTESIAN_POINT ( 'NONE',  ( 6.387826650694035990, 7.481494509678370264, -1.199719254218452047 ) ) ;
#106022 = CARTESIAN_POINT ( 'NONE',  ( 1.364683531249988757, -0.05312499965857975237, 0.000000000000000000 ) ) ;
#106023 = CARTESIAN_POINT ( 'NONE',  ( 6.017840079619279692, 8.114175741012878973, -1.599625672291281386 ) ) ;
#106024 = CARTESIAN_POINT ( 'NONE',  ( 7.253248993186724114, 9.485209796849769504, 1.443375672974076540 ) ) ;
#106026 = LINE ( 'NONE', #37772, #62655 ) ;
#106025 = CARTESIAN_POINT ( 'NONE',  ( 2.348295082997472250, -0.9299805079447539535, 1.962071136543291683 ) ) ;
#106028 = CARTESIAN_POINT ( 'NONE',  ( 1.417261839328866513, -1.023339270300478221, -1.530466495063505628 ) ) ;
#106027 = CARTESIAN_POINT ( 'NONE',  ( -5.341549334104202629, 7.254893527920112994, 1.443375672974064550 ) ) ;
#106029 = CARTESIAN_POINT ( 'NONE',  ( 0.6823417656249917140, 3.592708333674754506, 1.181850606188765695 ) ) ;
#106030 = CARTESIAN_POINT ( 'NONE',  ( 3.105210138592546798, -0.4252477525170209605, 2.149737936336936883 ) ) ;
#106031 = CARTESIAN_POINT ( 'NONE',  ( 6.983263157960330147, 2.017328405816510628, 2.456467998350126525 ) ) ;
#106032 = CARTESIAN_POINT ( 'NONE',  ( 4.206154751832458238, -2.256696944984788011, 0.1629611055770207317 ) ) ;
#106033 = CARTESIAN_POINT ( 'NONE',  ( -6.287230548435221777, 8.358188277972981695, -1.599625672291263179 ) ) ;
#106034 = CARTESIAN_POINT ( 'NONE',  ( -1.423205080756925867, 7.980384757729337863, -10.65537363484301636 ) ) ;
#106035 = CARTESIAN_POINT ( 'NONE',  ( 6.455362170788604637, 6.771378801287749383, -0.3290997004737963860 ) ) ;
#106036 = CARTESIAN_POINT ( 'NONE',  ( -1.500000000000008216, 13.74999999999999822, 3.469446951953614189E-15 ) ) ;
#106037 = CARTESIAN_POINT ( 'NONE',  ( 6.075462232699553766, 6.260663157670496304, -0.7216878364870458196 ) ) ;
#106038 = CARTESIAN_POINT ( 'NONE',  ( 5.219873587733063758, -0.9469346145933134062, -1.494860035008038324 ) ) ;
#106039 = CARTESIAN_POINT ( 'NONE',  ( 8.446893396513862839, 9.813462703143045474, -1.199719254218445830 ) ) ;
#106040 = CARTESIAN_POINT ( 'NONE',  ( 2.397617287051221791, 1.627147360716905800, 1.336933552532795222 ) ) ;
#106042 = CARTESIAN_POINT ( 'NONE',  ( -1.500000000000015099, 0.6291666666666863028, -0.8660254037844313801 ) ) ;
#106041 = CARTESIAN_POINT ( 'NONE',  ( -0.6823417656250039265, 10.81770833367473550, -1.181850606188755259 ) ) ;
#106043 = CARTESIAN_POINT ( 'NONE',  ( 1.082395645157930852, 1.176005852300557653, -1.579744537442813401 ) ) ;
#106044 = DIRECTION ( 'NONE',  ( 0.6250000000000000000, 1.408756634010579545E-16, -0.7806247497997997886 ) ) ;
#106045 = CARTESIAN_POINT ( 'NONE',  ( 0.3968290921660848070, 0.3316028935436679537, 1.933473477243151439 ) ) ;
#106047 = ORIENTED_EDGE ( 'NONE', *, *, #199503, .F. ) ;
#106046 = CARTESIAN_POINT ( 'NONE',  ( 5.379120748016958053, -1.641329381114923658, -0.7670206631310432233 ) ) ;
#106048 = CARTESIAN_POINT ( 'NONE',  ( 6.805829924380114804, 8.002851668940699881, 1.082531754730558626 ) ) ;
#106050 = CARTESIAN_POINT ( 'NONE',  ( 5.049604242677836474, 0.5861553263475408615, -1.776501995420045610 ) ) ;
#106049 = CIRCLE ( 'NONE', #206333, 11.00000000000000000 ) ;
#106051 = ORIENTED_EDGE ( 'NONE', *, *, #189072, .T. ) ;
#106052 = CARTESIAN_POINT ( 'NONE',  ( 4.821179601816666604, -1.846891146645711412, -0.9356023351853595127 ) ) ;
#106053 = CARTESIAN_POINT ( 'NONE',  ( -1.225000000000058042, 1.520833333333367232, 0.7072540797572596238 ) ) ;
#106054 = CARTESIAN_POINT ( 'NONE',  ( -4.462041952228944730, 7.259447140025469203, -1.082531754730549967 ) ) ;
#106055 = CARTESIAN_POINT ( 'NONE',  ( 0.000000000000000000, 18.91999999999999815, 0.000000000000000000 ) ) ;
#106056 = AXIS2_PLACEMENT_3D ( 'NONE', #205164, #56806, #115229 ) ;
#106057 = CARTESIAN_POINT ( 'NONE',  ( 8.274553823041976841, 8.548067636504127265, 1.040834085586084257E-14 ) ) ;
#106058 = CARTESIAN_POINT ( 'NONE',  ( -9.528683032306089373, 10.01121838064558744, 0.7998128361456462443 ) ) ;
#106059 = CARTESIAN_POINT ( 'NONE',  ( 8.018721507839716267, 8.319872945426633137, -0.7998128361456341429 ) ) ;
#106060 = CARTESIAN_POINT ( 'NONE',  ( 5.094532678321557206, 4.917790403868676385, -0.1305349544365452807 ) ) ;
#106061 = CARTESIAN_POINT ( 'NONE',  ( 0.6823417656249882723, -0.4072916663252490466, 1.181850606188755259 ) ) ;
#106062 = CARTESIAN_POINT ( 'NONE',  ( 1.499999999999989120, 1.525000000000019451, 0.000000000000000000 ) ) ;
#106064 = CARTESIAN_POINT ( 'NONE',  ( 4.313465427442102929, 8.184126765324453601, 0.7998128361456462443 ) ) ;
#106063 = CARTESIAN_POINT ( 'NONE',  ( 5.389097038490845648, 0.1425914310585977562, 1.956722230749983193 ) ) ;
#106065 = CARTESIAN_POINT ( 'NONE',  ( 1.915388525686153143, 0.6297767875703685903, 1.915307412907449436 ) ) ;
#106066 = CARTESIAN_POINT ( 'NONE',  ( -1.201851678989727383E-14, 2.868750000682821266, -1.732050807568863648 ) ) ;
#106067 = CARTESIAN_POINT ( 'NONE',  ( 0.1346727191937693857, 0.3808678606769915209, 2.158067550307264604 ) ) ;
#106068 = CARTESIAN_POINT ( 'NONE',  ( 0.000000000000000000, 13.49999999999999822, 0.000000000000000000 ) ) ;
#106069 = CARTESIAN_POINT ( 'NONE',  ( 2.266681450017640653, -1.708379500633325998, -0.7622673669660309237 ) ) ;
#106070 = CARTESIAN_POINT ( 'NONE',  ( -1.364683531250010295, 4.530208333674754506, 0.7879004041258379498 ) ) ;
#106071 = CARTESIAN_POINT ( 'NONE',  ( 3.674091251731440355, 1.997487462777279621, -0.2507888908306437625 ) ) ;
#106072 = CARTESIAN_POINT ( 'NONE',  ( -7.700141177557535244, 11.07091624287075859, -1.199719254218446718 ) ) ;
#106074 = CARTESIAN_POINT ( 'NONE',  ( 3.234098929720787385, 2.117403153491578927, -0.002560228748609005411 ) ) ;
#106073 = CARTESIAN_POINT ( 'NONE',  ( -4.419594888374909658, 8.100018436505289188, 0.7216878364870458196 ) ) ;
#106075 = CARTESIAN_POINT ( 'NONE',  ( 6.825078400183575589, -0.005632053428735600553, 2.144262460745151255 ) ) ;
#106076 = CARTESIAN_POINT ( 'NONE',  ( 5.178213324540339002, -1.104578422852561914, -1.750899486206449751 ) ) ;
#106077 = CARTESIAN_POINT ( 'NONE',  ( 5.397027666691686321, 8.454226823519094935, 1.199719254218451159 ) ) ;
#106079 = CARTESIAN_POINT ( 'NONE',  ( 6.720655732516649827, 0.5759399164693942419, 2.126764875236677454 ) ) ;
#106078 = CARTESIAN_POINT ( 'NONE',  ( 0.8727377898805768197, -0.05501089605610678251, -2.090203850258448792 ) ) ;
#106081 = ORIENTED_EDGE ( 'NONE', *, *, #11734, .T. ) ;
#106080 = CARTESIAN_POINT ( 'NONE',  ( 0.07661050522433668353, 0.008287133257128471639, -1.710863442170395432 ) ) ;
#106082 = CARTESIAN_POINT ( 'NONE',  ( 5.913327553854682783, 10.05063257947248800, -0.7998128361456291469 ) ) ;
#106083 = DIRECTION ( 'NONE',  ( -1.000000000000000000, 0.000000000000000000, 0.000000000000000000 ) ) ;
#106084 = CARTESIAN_POINT ( 'NONE',  ( -11.88237264505823987, 13.75677038468317015, 0.9087825512662228711 ) ) ;
#106085 = CARTESIAN_POINT ( 'NONE',  ( -10.89402507593495351, 4.580915115640823210, 4.512369680550198936 ) ) ;
#106086 = CARTESIAN_POINT ( 'NONE',  ( 8.229436053370683624, 8.703356271795033905, 0.7216878364870458196 ) ) ;
#106087 = CARTESIAN_POINT ( 'NONE',  ( 1.364683531249996529, 12.77604166700806587, 0.7879004041258403923 ) ) ;
#106088 = CARTESIAN_POINT ( 'NONE',  ( 6.199862383955294654, 1.322219258337012704, 1.381733411008022383 ) ) ;
#106090 = CARTESIAN_POINT ( 'NONE',  ( -8.993135964566285168, 9.386413468282476913, -0.7998128361456291469 ) ) ;
#106089 = AXIS2_PLACEMENT_3D ( 'NONE', #26095, #120489, #88994 ) ;
#106091 = CARTESIAN_POINT ( 'NONE',  ( 5.494078562035752178, 7.432844293840273231, -1.599625672291262513 ) ) ;
#106092 = CARTESIAN_POINT ( 'NONE',  ( -6.794158526849257917, -7.616254850791395192, -7.451274665340245740 ) ) ;
#106093 = CARTESIAN_POINT ( 'NONE',  ( 0.000000000000000000, 14.00000000000000533, 0.000000000000000000 ) ) ;
#106094 = CARTESIAN_POINT ( 'NONE',  ( 2.171277156482887882, 5.684907115872006145, -0.7998128361456291469 ) ) ;
#106095 = EDGE_LOOP ( 'NONE', ( #208194, #36482, #197459 ) ) ;
#106096 = EDGE_CURVE ( 'NONE', #95583, #68014, #127461, .T. ) ;
#106097 = CARTESIAN_POINT ( 'NONE',  ( 6.603150281434943203, -0.1430492952050037847, 1.984088717376513822 ) ) ;
#106098 = CARTESIAN_POINT ( 'NONE',  ( -4.024564264787665380, 7.667365063520641399, 0.3471600818823785128 ) ) ;
#106099 = CARTESIAN_POINT ( 'NONE',  ( 10.95855051086948251, -7.723431457505092190, -0.6286713519883923018 ) ) ;
#106100 = CARTESIAN_POINT ( 'NONE',  ( 0.1399997263886020860, 0.7221123407896400392, -2.083281383436136558 ) ) ;
#106101 = CARTESIAN_POINT ( 'NONE',  ( -5.260200412422208593, 7.159986452624450770, -1.443375672974053447 ) ) ;
#106102 = CARTESIAN_POINT ( 'NONE',  ( 2.333974999846879061, 5.874721266463329705, -0.7998128361456291469 ) ) ;
#106103 = CARTESIAN_POINT ( 'NONE',  ( 3.625798818847306038, 1.922417080405220968, -0.4270903664440502956 ) ) ;
#106104 = CARTESIAN_POINT ( 'NONE',  ( 4.534779904478015489, -1.617806963314952773, 1.203370736114671269 ) ) ;
#106105 = CARTESIAN_POINT ( 'NONE',  ( -7.203459687562382641, 7.298457811777897319, -0.7998128361456291469 ) ) ;
#106106 = CARTESIAN_POINT ( 'NONE',  ( -1.299038105676657340, 7.500000000000000000, 0.7500000000000006661 ) ) ;
#106107 = PRESENTATION_LAYER_ASSIGNMENT (  '', '', ( #47337 ) ) ;
#106108 = CARTESIAN_POINT ( 'NONE',  ( 4.664136352776428573, -1.432711980460563250, 1.658340198327029613 ) ) ;
#106109 = DIRECTION ( 'NONE',  ( 0.000000000000000000, 1.000000000000000000, 0.000000000000000000 ) ) ;
#106110 = CARTESIAN_POINT ( 'NONE',  ( 3.293886989636186868, -0.7820812614263569218, 1.760672275598859748 ) ) ;
#106111 = CARTESIAN_POINT ( 'NONE',  ( -8.453672473320708036, 9.821371626084353323, -1.199719254218446718 ) ) ;
#106112 = CARTESIAN_POINT ( 'NONE',  ( -0.02988540731103071432, 7.629137130509069387, -2.326318838967501357 ) ) ;
#106113 = CARTESIAN_POINT ( 'NONE',  ( 0.1331565106231363538, 2.033293680964400885, -2.362282156872722805 ) ) ;
#106114 = DIRECTION ( 'NONE',  ( -1.000000000000000000, 0.000000000000000000, 0.000000000000000000 ) ) ;
#106115 = CARTESIAN_POINT ( 'NONE',  ( 1.364683531249996529, 12.96354166700806410, 0.7879004041258403923 ) ) ;
#106116 = CARTESIAN_POINT ( 'NONE',  ( 3.811813743736467419, 7.598866467667865443, 1.040834085586084257E-14 ) ) ;
#106117 = CARTESIAN_POINT ( 'NONE',  ( -4.905525160107053750, 6.476373528817804370, -2.499999999999995115 ) ) ;
#106118 = CARTESIAN_POINT ( 'NONE',  ( 4.421367491832270957, 6.251624388594711590, 1.443375672974058777 ) ) ;
#106119 = ORIENTED_EDGE ( 'NONE', *, *, #142360, .T. ) ;
#106121 = CARTESIAN_POINT ( 'NONE',  ( 2.736979112881072762, 1.896321534115693819, 0.6760404272549996874 ) ) ;
#106120 = CARTESIAN_POINT ( 'NONE',  ( 6.603072989126265391, -0.3962418105841297722, 1.804722624154910360 ) ) ;
#106122 = CARTESIAN_POINT ( 'NONE',  ( 4.956595877991936128, 1.698763664877179780, 1.548309420705455741 ) ) ;
#106124 = CARTESIAN_POINT ( 'NONE',  ( 3.221387034570993624, 0.2776250501920934921, -1.840009301959115051 ) ) ;
#106123 = CARTESIAN_POINT ( 'NONE',  ( -5.935437387732586778, 10.14670372898850381, -0.7998128361456362523 ) ) ;
#106125 = CARTESIAN_POINT ( 'NONE',  ( 3.285556943749998737, -0.9552083328553737651, -1.896917185911906500 ) ) ;
#106126 = CARTESIAN_POINT ( 'NONE',  ( 0.02755585400013305097, 7.629137130509076492, -2.789001785468494976 ) ) ;
#106127 = CARTESIAN_POINT ( 'NONE',  ( 6.539320575229249144, 0.007148032025052972194, 1.896977914940492393 ) ) ;
#106128 = CARTESIAN_POINT ( 'NONE',  ( -7.854251061018346469, 8.057714414143200443, -0.7998128361456291469 ) ) ;
#106129 = CARTESIAN_POINT ( 'NONE',  ( -3.838366886444665393, 7.492195444245147939, 0.000000000000000000 ) ) ;
#106130 = CARTESIAN_POINT ( 'NONE',  ( 6.480031082513550089, -2.050496881725831777, -0.4073240614407472315 ) ) ;
#106131 = CARTESIAN_POINT ( 'NONE',  ( 6.656690234629796699, 6.868486149930637552, 1.040834085586084257E-14 ) ) ;
#106132 = ORIENTED_EDGE ( 'NONE', *, *, #23415, .T. ) ;
#106133 = CARTESIAN_POINT ( 'NONE',  ( -3.131570295076647525, 6.597323077657299528, 1.040834085586084257E-14 ) ) ;
#106134 = CARTESIAN_POINT ( 'NONE',  ( 4.674199705399083804, 8.286630605821020623, 0.5482284608372268719 ) ) ;
#106135 = CARTESIAN_POINT ( 'NONE',  ( 6.709587848829112744, -0.3662258548819911086, 1.691549535187387932 ) ) ;
#106136 = CARTESIAN_POINT ( 'NONE',  ( -4.089755892816631544, 7.923132308261379819, -0.7998128361456281477 ) ) ;
#106137 = CARTESIAN_POINT ( 'NONE',  ( 2.320625381698769640, 0.8157257908444032202, -1.530271591396751729 ) ) ;
#106138 = CYLINDRICAL_SURFACE ( 'NONE', #19556, 0.5000000000000000000 ) ;
#106139 = FACE_OUTER_BOUND ( 'NONE', #117087, .T. ) ;
#106140 = CARTESIAN_POINT ( 'NONE',  ( -6.043183783389232566, 8.073467052085995022, 1.599625672291269396 ) ) ;
#106141 = DIRECTION ( 'NONE',  ( 0.000000000000000000, 1.000000000000000000, 0.000000000000000000 ) ) ;
#106142 = CARTESIAN_POINT ( 'NONE',  ( 6.948074912775242140, -0.9353680688231647000, 1.957065181168372581 ) ) ;
#106143 = CARTESIAN_POINT ( 'NONE',  ( 5.883392091387671385, 1.685093539698417242, -0.7030590484573000509 ) ) ;
#106144 = CARTESIAN_POINT ( 'NONE',  ( 3.256644689873238629, -0.5649923015349536115, -1.878667693404307171 ) ) ;
#106145 = CARTESIAN_POINT ( 'NONE',  ( -3.836074819041962236, 7.488154855499102425, 0.1510019874590182165 ) ) ;
#106146 = CARTESIAN_POINT ( 'NONE',  ( -9.317477881089553549, 11.89347683273641820, 1.599625672291281386 ) ) ;
#106147 = CARTESIAN_POINT ( 'NONE',  ( 6.938021921891177612, 9.117444880338284818, -1.599625672291262513 ) ) ;
#106148 = CARTESIAN_POINT ( 'NONE',  ( 3.528090983593739516, -2.088826311502915090, 0.3641918842257965139 ) ) ;
#106149 = CARTESIAN_POINT ( 'NONE',  ( -4.446711195602264688, 4.290177271065136466, -0.7216878364870207285 ) ) ;
#106150 = SURFACE_SIDE_STYLE ('',( #209967 ) ) ;
#106151 = CARTESIAN_POINT ( 'NONE',  ( 1.709917326824461181, 0.6048241955843024487, -1.979901091156407666 ) ) ;
#106153 = CARTESIAN_POINT ( 'NONE',  ( -1.500000000000008216, 15.03125000068279782, 3.469446951953614189E-15 ) ) ;
#106152 = CARTESIAN_POINT ( 'NONE',  ( 0.000000000000000000, 3.481548657788669843, 0.000000000000000000 ) ) ;
#106155 = VERTEX_POINT ( 'NONE', #183824 ) ;
#106154 = CARTESIAN_POINT ( 'NONE',  ( 4.987093027905733500, -2.091254775410257061, -0.7492775906185499268 ) ) ;
#106156 = CARTESIAN_POINT ( 'NONE',  ( 1.530362799304554100, -1.938799508460651522, 1.234721073783265233 ) ) ;
#106158 = CARTESIAN_POINT ( 'NONE',  ( 6.368047018367568590, -2.047660648193879496, 0.2468551644246498589 ) ) ;
#106157 = CARTESIAN_POINT ( 'NONE',  ( 9.910647101909615841, 10.66476916175714607, 0.000000000000000000 ) ) ;
#106160 = CARTESIAN_POINT ( 'NONE',  ( -1.737500000000000266, -0.4083333333333334370, -3.009438278150923907 ) ) ;
#106159 = CARTESIAN_POINT ( 'NONE',  ( 3.553118775233146120, 6.302999783484076524, -1.199719254218453823 ) ) ;
#106161 = CARTESIAN_POINT ( 'NONE',  ( 1.474529836884923328E-15, 14.99975178945622822, 11.68000004620062526 ) ) ;
#106162 = CARTESIAN_POINT ( 'NONE',  ( 6.163598723784101452, 0.9525508894225950263, 1.575581956637741587 ) ) ;
#106163 = CARTESIAN_POINT ( 'NONE',  ( -3.197497122698730099, 6.431928158754200986, 0.6077543439236172684 ) ) ;
#106164 = CARTESIAN_POINT ( 'NONE',  ( 2.900541297466651347, -1.884798985816903860, -0.3226963764228693576 ) ) ;
#106165 = FACE_OUTER_BOUND ( 'NONE', #156477, .T. ) ;
#106166 = CARTESIAN_POINT ( 'NONE',  ( 3.891373129206575410, 1.249378432800802852, 1.189308452707043884 ) ) ;
#106167 = CARTESIAN_POINT ( 'NONE',  ( 2.676970549635893537, 1.727063564601112100, -1.040793759654296213 ) ) ;
#106168 = CARTESIAN_POINT ( 'NONE',  ( 4.412867445986612402, -1.413514171388057239, -1.812631114537610166 ) ) ;
#106169 =( BOUNDED_CURVE ( )  B_SPLINE_CURVE ( 3, ( #124109, #24352, #88319, #156528 ),
 .UNSPECIFIED., .F., .T. ) 
 B_SPLINE_CURVE_WITH_KNOTS ( ( 4, 4 ),
 ( 0.000000000000000000, 0.5000000000000005551 ),
 .UNSPECIFIED. ) 
 CURVE ( )  GEOMETRIC_REPRESENTATION_ITEM ( )  RATIONAL_B_SPLINE_CURVE ( ( 1.000000000000000222, 0.3333333333333327042, 0.3333333333333334259, 1.000000000000000888 ) ) 
 REPRESENTATION_ITEM ( '' )  );
#106170 = CARTESIAN_POINT ( 'NONE',  ( 3.708526512723071544, -0.9128432734063509635, -2.070237398927244676 ) ) ;
#106171 = CARTESIAN_POINT ( 'NONE',  ( 5.953767555512091469, 0.6130212357637642162, -2.014879775860946687 ) ) ;
#106172 = CARTESIAN_POINT ( 'NONE',  ( -6.956742217587851052, 7.288823140040177506, 0.000000000000000000 ) ) ;
#106173 = CARTESIAN_POINT ( 'NONE',  ( 5.044116495868207650, 1.765035602982415242, 0.1300806658623629153 ) ) ;
#106174 = AXIS2_PLACEMENT_3D ( 'NONE', #77237, #162781, #29573 ) ;
#106176 = CARTESIAN_POINT ( 'NONE',  ( 1.096115288130569798, -2.292435215939184534, 0.004638672314880368241 ) ) ;
#106175 = CARTESIAN_POINT ( 'NONE',  ( 7.526711554241970248, 8.810193563817646734, -1.199719254218452047 ) ) ;
#106177 = CARTESIAN_POINT ( 'NONE',  ( 5.683513393433289096, -0.8240744568873883402, 1.646495476055845231 ) ) ;
#106178 = CARTESIAN_POINT ( 'NONE',  ( -3.002240950422295995, 5.590032644546251817, -1.199719254218452935 ) ) ;
#106179 = UNCERTAINTY_MEASURE_WITH_UNIT (LENGTH_MEASURE( 1.000000000000000082E-05 ), #134317, 'distance_accuracy_value', 'NONE');
#106180 = CARTESIAN_POINT ( 'NONE',  ( 6.281208295753298643, 1.508423295503196648, 1.589913042345507455 ) ) ;
#106181 = CARTESIAN_POINT ( 'NONE',  ( -4.796887421136680985, 4.490790167614548523, 1.214306433183764966E-14 ) ) ;
#106182 = CARTESIAN_POINT ( 'NONE',  ( -3.069665630396485323, 15.47024000507179231, 11.60952187717502326 ) ) ;
#106183 =( BOUNDED_CURVE ( )  B_SPLINE_CURVE ( 2, ( #145027, #111489, #211031, #98373, #82108, #214201, #65831 ),
 .UNSPECIFIED., .F., .T. ) 
 B_SPLINE_CURVE_WITH_KNOTS ( ( 3, 2, 2, 3 ),
 ( 0.1625000000000002276, 0.1666666666666669072, 0.1708333333333336146, 0.1750000000000002942 ),
 .UNSPECIFIED. ) 
 CURVE ( )  GEOMETRIC_REPRESENTATION_ITEM ( )  RATIONAL_B_SPLINE_CURVE ( ( 0.9999999999999928946, 0.8660254037844458130, 1.000000000000000000, 0.8660254037844387076, 1.000000000000000000, 0.8660254037844289376, 1.000000000000009770 ) ) 
 REPRESENTATION_ITEM ( '' )  );
#106184 = CARTESIAN_POINT ( 'NONE',  ( 5.775854211382815073, -2.020734006234246927, 0.4499205674863211990 ) ) ;
#106185 = CARTESIAN_POINT ( 'NONE',  ( 0.5324358445358172709, 0.5899921999869184308, 1.928256190492839028 ) ) ;
#106186 = CARTESIAN_POINT ( 'NONE',  ( -1.364683531250010295, 5.488541667008087543, -0.7879004041258300672 ) ) ;
#106187 = CARTESIAN_POINT ( 'NONE',  ( 4.301339506872517759, 1.548173799611574530, 1.146357790588454106 ) ) ;
#106188 = CARTESIAN_POINT ( 'NONE',  ( -1.364683531250000748, 10.10937500034139802, 0.000000000000000000 ) ) ;
#106189 = CARTESIAN_POINT ( 'NONE',  ( -2.657034918598345730, 5.083329257464595408, -1.082531754730543971 ) ) ;
#106190 = CARTESIAN_POINT ( 'NONE',  ( 1.723182734256373916, 1.642088205692782132, -1.496221191757711066 ) ) ;
#106192 = EDGE_LOOP ( 'NONE', ( #167904, #14241, #211233, #107286 ) ) ;
#106191 = CARTESIAN_POINT ( 'NONE',  ( 3.929058411375439874, 6.499999999999999112, -0.7500000000000006661 ) ) ;
#106193 = CARTESIAN_POINT ( 'NONE',  ( -7.055228938194283650, -8.176568542494891290, 6.396834479292372144 ) ) ;
#106194 = CARTESIAN_POINT ( 'NONE',  ( 3.541704441667858472, 5.155074486744371853, -1.599625672291262513 ) ) ;
#106195 = DIRECTION ( 'NONE',  ( 0.000000000000000000, 0.000000000000000000, 1.000000000000000000 ) ) ;
#106196 = CARTESIAN_POINT ( 'NONE',  ( -10.95308175811721085, 9.799999999999982947, 1.799999999999999600 ) ) ;
#106197 = CARTESIAN_POINT ( 'NONE',  ( 9.151390499099949949, 12.66007743471656788, -1.082531754730543971 ) ) ;
#106198 = CARTESIAN_POINT ( 'NONE',  ( 1.715213470010600538, -1.680963409367957295, -1.011360081469035999 ) ) ;
#106199 = CARTESIAN_POINT ( 'NONE',  ( 0.6823417656249882723, 2.988541667008084879, -1.181850606188754593 ) ) ;
#106200 = CARTESIAN_POINT ( 'NONE',  ( -1.201851678989727383E-14, 3.712500000000020339, 1.732050807568877637 ) ) ;
#106201 = CIRCLE ( 'NONE', #192559, 9.500000000000001776 ) ;
#106202 = CARTESIAN_POINT ( 'NONE',  ( 6.215287892896892430, -1.681934637451238279, -1.009743211781432670 ) ) ;
#106203 = CARTESIAN_POINT ( 'NONE',  ( -7.621654909176601045, 12.04368116068139472, 0.7998128361456481317 ) ) ;
#106204 = CARTESIAN_POINT ( 'NONE',  ( -5.870317324592829067, 5.951051088220814300, -0.7216878364870197293 ) ) ;
#106205 = COLOUR_RGB ( '', 0.72549020, 0.75294118, 0.79215686) ;
#106206 = CARTESIAN_POINT ( 'NONE',  ( 0.3216218905449366172, -0.1073394912241855820, 2.260102045549317928 ) ) ;
#106208 = ORIENTED_EDGE ( 'NONE', *, *, #101458, .F. ) ;
#106207 = CARTESIAN_POINT ( 'NONE',  ( -6.555530967407501741, 7.606873202518897870, 1.199719254218450271 ) ) ;
#106209 = CARTESIAN_POINT ( 'NONE',  ( -0.7500000000000249800, -1.027083332650516212, 1.299038105676659116 ) ) ;
#106210 = CARTESIAN_POINT ( 'NONE',  ( 1.405301488743180061, -0.4598193086536165319, 1.813012767170335993 ) ) ;
#106211 = CARTESIAN_POINT ( 'NONE',  ( 0.5274301605363295176, -1.488642097782297835, 0.8892331099567828412 ) ) ;
#106213 = CARTESIAN_POINT ( 'NONE',  ( 4.669572502782517454, 1.262004115398765780, 1.791526714441132873 ) ) ;
#106212 = CARTESIAN_POINT ( 'NONE',  ( -5.758872628492444169E-14, 2.203125000341452200, 1.570758158831754070 ) ) ;
#106214 = CARTESIAN_POINT ( 'NONE',  ( 4.014917937017292715, 1.634369553669342778, -1.629294119824703069 ) ) ;
#106215 = CARTESIAN_POINT ( 'NONE',  ( 0.3212574623711033639, -0.1015677953285927942, 2.058520922655207031 ) ) ;
#106216 = CARTESIAN_POINT ( 'NONE',  ( 2.677597413788167735, -0.9980636400313472878, 1.665709379616100883 ) ) ;
#106217 = CARTESIAN_POINT ( 'NONE',  ( -5.897433631820158340, 5.982686779986042147, 0.7216878364870317197 ) ) ;
#106218 = CARTESIAN_POINT ( 'NONE',  ( -0.4867935908771195419, 7.427453578134552536, -4.536604770845594992 ) ) ;
#106219 = CARTESIAN_POINT ( 'NONE',  ( 5.660427296577901224, 2.118236611397010805, 0.1021076702828054988 ) ) ;
#106220 = CYLINDRICAL_SURFACE ( 'NONE', #119263, 0.2500000000000002220 ) ;
#106221 = CARTESIAN_POINT ( 'NONE',  ( 4.026017654026761150, -1.753031021560845559, 0.9963007555989014108 ) ) ;
#106222 = CARTESIAN_POINT ( 'NONE',  ( -5.897433631820158340, 5.982686779986042147, 0.7216878364870317197 ) ) ;
#106223 = CARTESIAN_POINT ( 'NONE',  ( -5.745623237141265882, 9.925253886631958622, 0.7998128361456291469 ) ) ;
#106224 = DIRECTION ( 'NONE',  ( 0.9988044021632734859, 0.000000000000000000, -0.04888523518676873847 ) ) ;
#106225 = CARTESIAN_POINT ( 'NONE',  ( 0.5744775230259161480, -1.718042477583326066, -0.6180270036199516648 ) ) ;
#106226 = CARTESIAN_POINT ( 'NONE',  ( -5.264308783856126439, 9.363720357799287797, -0.7998128361456362523 ) ) ;
#106227 = CARTESIAN_POINT ( 'NONE',  ( -4.294900800479008574, 8.232744377192641849, 0.000000000000000000 ) ) ;
#106228 = CARTESIAN_POINT ( 'NONE',  ( -9.348561386651960348, 2.999999999999999112, 7.001914024036568485 ) ) ;
#106229 = VERTEX_POINT ( 'NONE', #101512 ) ;
#106230 = CARTESIAN_POINT ( 'NONE',  ( 5.102442524761234388, -0.6923759778164092493, -1.941246359495584883 ) ) ;
#106231 = CARTESIAN_POINT ( 'NONE',  ( -6.902509602688821744, 8.185920970292658083, -1.082531754730549967 ) ) ;
#106232 = ADVANCED_FACE ( 'NONE', ( #114632 ), #81465, .T. ) ;
#106233 = CARTESIAN_POINT ( 'NONE',  ( -5.088387723830502196, 4.830873854090670605, -0.7998128361456221525 ) ) ;
#106234 = CARTESIAN_POINT ( 'NONE',  ( -9.541187415715041809, 12.15447128979948310, -1.599625672291263179 ) ) ;
#106235 = CARTESIAN_POINT ( 'NONE',  ( 6.235022398275627431, 1.885252722396244085, 0.7250032809389771460 ) ) ;
#106237 = ORIENTED_EDGE ( 'NONE', *, *, #207506, .F. ) ;
#106236 = CARTESIAN_POINT ( 'NONE',  ( 6.059279899546098136, -1.878006040282210298, 1.186031488430500769 ) ) ;
#106238 = CARTESIAN_POINT ( 'NONE',  ( -4.167152111353897403, 5.955039778036558040, 1.599625672291270506 ) ) ;
#106239 = CARTESIAN_POINT ( 'NONE',  ( 5.656776405399742025, 7.622658444431597680, -1.599625672291262513 ) ) ;
#106240 = CARTESIAN_POINT ( 'NONE',  ( 4.364173291480280881, 0.9696465702416400267, 1.818514982836361593 ) ) ;
#106241 = CARTESIAN_POINT ( 'NONE',  ( 3.481092415823695774, -2.014232707597499505, -0.09613569647320965861 ) ) ;
#106242 = EDGE_LOOP ( 'NONE', ( #119, #70517, #113826, #13675 ) ) ;
#106243 =( LENGTH_UNIT ( ) NAMED_UNIT ( * ) SI_UNIT ( .MILLI., .METRE. ) );
#106244 = CARTESIAN_POINT ( 'NONE',  ( 2.866659414285625651, 5.431854185720147221, -1.199719254218446718 ) ) ;
#106245 =( GEOMETRIC_REPRESENTATION_CONTEXT ( 3 ) GLOBAL_UNCERTAINTY_ASSIGNED_CONTEXT ( ( #27305 ) ) GLOBAL_UNIT_ASSIGNED_CONTEXT ( ( #197918, #168632, #172929 ) ) REPRESENTATION_CONTEXT ( 'NONE', 'WORKASPACE' ) );
#106246 =( BOUNDED_CURVE ( )  B_SPLINE_CURVE ( 2, ( #125335, #142603, #139385, #60246, #77565, #27753, #172954, #143687, #141550 ),
 .UNSPECIFIED., .F., .T. ) 
 B_SPLINE_CURVE_WITH_KNOTS ( ( 3, 2, 2, 2, 3 ),
 ( 0.3303571428571428492, 0.3333333333333333148, 0.3392857142857143016, 0.3452380952380952328, 0.3482142857142856429 ),
 .UNSPECIFIED. ) 
 CURVE ( )  GEOMETRIC_REPRESENTATION_ITEM ( )  RATIONAL_B_SPLINE_CURVE ( ( 0.9330127018922194093, 0.9330127018922194093, 1.000000000000000000, 0.8660254037844387076, 1.000000000000000000, 0.8660254037844387076, 1.000000000000000000, 0.9330127018922206306, 0.9330127018922194093 ) ) 
 REPRESENTATION_ITEM ( '' )  );
#106248 = ORIENTED_EDGE ( 'NONE', *, *, #173321, .T. ) ;
#106247 = CARTESIAN_POINT ( 'NONE',  ( -6.794571259104023930, 7.956029886156682274, 1.199719254218452047 ) ) ;
#106249 = CARTESIAN_POINT ( 'NONE',  ( 5.258270873920524835, 7.671714958958308017, -1.216365610458163715 ) ) ;
#106250 = CARTESIAN_POINT ( 'NONE',  ( 4.218124927476913477, -1.674631575811252215, -1.122325875776951420 ) ) ;
#106251 = CARTESIAN_POINT ( 'NONE',  ( 3.345483972246702020, 1.841320589717788447, -0.001054884335952021917 ) ) ;
#106252 = CARTESIAN_POINT ( 'NONE',  ( 4.475125623951746512, 4.983947107165113799, -0.9081682986131468516 ) ) ;
#106253 = CARTESIAN_POINT ( 'NONE',  ( 1.524504908422112726, -1.285150704446396341, -1.916548379014111791 ) ) ;
#106254 = CARTESIAN_POINT ( 'NONE',  ( 5.096939404094710468, 4.911127157724081371, 0.000000000000000000 ) ) ;
#106255 = CARTESIAN_POINT ( 'NONE',  ( 3.620547430246877862, 1.374377816306590727, -1.668374205817772182 ) ) ;
#106256 = CARTESIAN_POINT ( 'NONE',  ( 7.910292558569346433, 11.31609285405122556, -1.199719254218446718 ) ) ;
#106257 = CARTESIAN_POINT ( 'NONE',  ( -6.437424008390261854, 6.404749519410410485, 0.7998128361456341429 ) ) ;
#106258 =( GEOMETRIC_REPRESENTATION_CONTEXT ( 3 ) GLOBAL_UNCERTAINTY_ASSIGNED_CONTEXT ( ( #83518 ) ) GLOBAL_UNIT_ASSIGNED_CONTEXT ( ( #149343, #66990, #199127 ) ) REPRESENTATION_CONTEXT ( 'NONE', 'WORKASPACE' ) );
#106259 = CARTESIAN_POINT ( 'NONE',  ( 3.181363629901075463, -1.130666556857576444, -2.000962643106804606 ) ) ;
#106260 = CARTESIAN_POINT ( 'NONE',  ( -2.428612866367529932E-14, 8.999999999999998224, 0.7749999999999996891 ) ) ;
#106261 = CARTESIAN_POINT ( 'NONE',  ( 2.746779440450992649, -1.556306552617524597, 1.037596984913228937 ) ) ;
#106262 = EDGE_CURVE ( 'NONE', #13123, #28052, #93953, .T. ) ;
#106263 = CARTESIAN_POINT ( 'NONE',  ( 6.526250059115050739, 1.135311405967744935, -1.611567521105742751 ) ) ;
#106265 = CARTESIAN_POINT ( 'NONE',  ( -6.563028877466991595, 9.814561569423593923, 1.199719254218452935 ) ) ;
#106264 = CARTESIAN_POINT ( 'NONE',  ( 0.6823417656249899377, 4.176041667008085767, -1.181850606188754593 ) ) ;
#106267 = CARTESIAN_POINT ( 'NONE',  ( 1.401302286655212948, 1.802556353783949517, -1.272968949304439379 ) ) ;
#106266 = CARTESIAN_POINT ( 'NONE',  ( -4.577849422908604637, 8.492574760035358494, -0.7998128361456281477 ) ) ;
#106268 = CARTESIAN_POINT ( 'NONE',  ( 0.000000000000000000, 0.000000000000000000, 0.000000000000000000 ) ) ;
#106269 = CARTESIAN_POINT ( 'NONE',  ( 6.342516933094585418, 6.294024598232139667, 1.040834085586084257E-14 ) ) ;
#106270 = CARTESIAN_POINT ( 'NONE',  ( -6.033542053281340856, 6.997886136038390603, -1.199719254218446718 ) ) ;
#106271 = STYLED_ITEM ( 'NONE', ( #50962 ), #145317 ) ;
#106272 = CARTESIAN_POINT ( 'NONE',  ( 11.97178994924802353, 13.87999993797205356, 0.8322011300497295094 ) ) ;
#106273 = CARTESIAN_POINT ( 'NONE',  ( 6.227413254736037906, -1.856526228437559434, 0.6636957074077839414 ) ) ;
#106274 = CARTESIAN_POINT ( 'NONE',  ( 6.059233210108489587, -1.975957287588899769, -1.191867793525339669 ) ) ;
#106275 = CARTESIAN_POINT ( 'NONE',  ( 0.3265133270617843197, -1.284392789319420913, 1.483054880892266114 ) ) ;
#106276 = CARTESIAN_POINT ( 'NONE',  ( 3.080982041725123910, 1.940567726598545040, 0.6991345639211270502 ) ) ;
#106277 = CARTESIAN_POINT ( 'NONE',  ( 5.829642864196151741, 9.745074408296771296, 0.7216878364870438212 ) ) ;
#106278 = CARTESIAN_POINT ( 'NONE',  ( 6.912678218121202534, 9.158153569265168770, 1.599625672291268286 ) ) ;
#106279 = CARTESIAN_POINT ( 'NONE',  ( 6.222829318548112276, 9.243422724072711816, -1.082531754730537976 ) ) ;
#106280 = CARTESIAN_POINT ( 'NONE',  ( -0.6823417656249969321, 3.280208333674754062, -1.181850606188749264 ) ) ;
#106281 = CARTESIAN_POINT ( 'NONE',  ( -8.795148599269996481, 14.53091781150858885, 8.214862920035907123 ) ) ;
#106282 = CARTESIAN_POINT ( 'NONE',  ( 4.568734577680873876, 6.353276312092901890, -1.443375672974051449 ) ) ;
#106283 = CARTESIAN_POINT ( 'NONE',  ( 5.371592247264787900, -0.3238957681546798528, 2.146784808600268324 ) ) ;
#106285 = CARTESIAN_POINT ( 'NONE',  ( 5.161589042655139181, 0.9124512986629171873, 1.599201395118980740 ) ) ;
#106284 = LINE ( 'NONE', #172305, #21719 ) ;
#106287 = CARTESIAN_POINT ( 'NONE',  ( 3.147653791585713901, 8.920000000000001705, -2.420000000000002149 ) ) ;
#106286 = CARTESIAN_POINT ( 'NONE',  ( 0.4019237886466778820, 9.354914550367425363, 1.500000000000001554 ) ) ;
#106288 = CARTESIAN_POINT ( 'NONE',  ( -2.788906526875773208E-15, 10.93750000000000178, -1.499999999999998446 ) ) ;
#106289 = CARTESIAN_POINT ( 'NONE',  ( 0.6845637836509765872, -0.2226890396202323152, -1.857165095135074218 ) ) ;
#106290 = CARTESIAN_POINT ( 'NONE',  ( 0.4568015506021270156, 0.8674211623492070755, 2.089700042804636837 ) ) ;
#106291 = CARTESIAN_POINT ( 'NONE',  ( -4.144643181316929770, 7.629267798522465505, 0.8581763667485035052 ) ) ;
#106292 = DIRECTION ( 'NONE',  ( -3.330669073875479482E-16, 3.330669073875479482E-16, 1.000000000000000000 ) ) ;
#106293 = CARTESIAN_POINT ( 'NONE',  ( 6.344829475870412239, 6.940264737885684987, 0.8615092103797560297 ) ) ;
#106294 = CARTESIAN_POINT ( 'NONE',  ( -5.289089322662584358, 5.343228095960675716, 0.000000000000000000 ) ) ;
#106295 = CARTESIAN_POINT ( 'NONE',  ( -1.406531590435020185, 3.336988665940368470, -0.01155683023987377767 ) ) ;
#106296 = CARTESIAN_POINT ( 'NONE',  ( 2.307162891426073337, -0.3907249415124186553, 1.725993255813297989 ) ) ;
#106297 = CARTESIAN_POINT ( 'NONE',  ( 6.199863759850236633, 1.389832719217662049, 1.456544111691231658 ) ) ;
#106299 = CARTESIAN_POINT ( 'NONE',  ( 3.409697593026795204, -1.143712931967875601, -1.536527803759838662 ) ) ;
#106298 = CARTESIAN_POINT ( 'NONE',  ( -8.482597663644387609, 13.04811437422715414, -0.7998128361456281477 ) ) ;
#106300 = CARTESIAN_POINT ( 'NONE',  ( 4.017982430692658369, 1.954955499905395522, -0.2386041268068790633 ) ) ;
#106301 = CARTESIAN_POINT ( 'NONE',  ( 6.504167520383483669, -0.8605252283936345448, 1.825738368183300153 ) ) ;
#106302 = CARTESIAN_POINT ( 'NONE',  ( -4.457933580795036654, 4.095344020549286590, -0.7998128361456221525 ) ) ;
#106303 = CARTESIAN_POINT ( 'NONE',  ( 2.588565208901713266, -0.3177388942022137397, -1.843305967786903032 ) ) ;
#106305 = ORIENTED_EDGE ( 'NONE', *, *, #67920, .F. ) ;
#106304 = CARTESIAN_POINT ( 'NONE',  ( 6.111878173048258311, -1.710926958338830017, 0.2183984861162356628 ) ) ;
#106307 = CARTESIAN_POINT ( 'NONE',  ( 4.202664430556257713, 4.965825259479493603, 1.082531754730560403 ) ) ;
#106306 = CARTESIAN_POINT ( 'NONE',  ( 2.403190426070573871, 1.771669130372434564, -1.315670724662293178 ) ) ;
#106308 = CARTESIAN_POINT ( 'NONE',  ( -1.364683531250012516, 3.301041667008084879, -0.7879004041258289570 ) ) ;
#106309 = CARTESIAN_POINT ( 'NONE',  ( 6.197705743426439540, -1.420020466879829302, -1.353909852041992767 ) ) ;
#106310 = CARTESIAN_POINT ( 'NONE',  ( 9.074484886248265880, 9.481320543578137361, 0.7998128361456462443 ) ) ;
#106311 = CARTESIAN_POINT ( 'NONE',  ( -8.631737353394710155, 13.22211067893587533, 1.040834085586084257E-14 ) ) ;
#106312 = DIRECTION ( 'NONE',  ( 0.000000000000000000, 0.000000000000000000, 1.000000000000000000 ) ) ;
#106313 = CARTESIAN_POINT ( 'NONE',  ( -3.578462479003122976, 6.262291094557191684, 1.199719254218464037 ) ) ;
#106314 = DIRECTION ( 'NONE',  ( 0.000000000000000000, 0.000000000000000000, 1.000000000000000000 ) ) ;
#106315 = ORIENTED_EDGE ( 'NONE', *, *, #206779, .T. ) ;
#106316 = CARTESIAN_POINT ( 'NONE',  ( 2.031770498437397876, 1.981864486777328294, -0.5989037013024376410 ) ) ;
#106317 = CARTESIAN_POINT ( 'NONE',  ( 1.499999999999989120, 3.275000000000020783, 1.214306433183764966E-14 ) ) ;
#106318 = CARTESIAN_POINT ( 'NONE',  ( 3.499976210622149253, 7.235056012367825140, 0.7998128361456321445 ) ) ;
#106319 = CARTESIAN_POINT ( 'NONE',  ( 5.388439706788500594, 5.251210844200210559, 0.7998128361456352531 ) ) ;
#106320 = CARTESIAN_POINT ( 'NONE',  ( 0.9791725360285336022, -1.826886329348556881, -0.8614179918085950183 ) ) ;
#106321 = CARTESIAN_POINT ( 'NONE',  ( 1.499999999999990674, 8.673756432004019246, 2.614717076620609149 ) ) ;
#106322 = CARTESIAN_POINT ( 'NONE',  ( 1.364683531249988535, 4.405208333674754506, -0.7879004041258300672 ) ) ;
#106324 = CARTESIAN_POINT ( 'NONE',  ( 8.595506201384004896, 12.01154575404795466, 1.082531754730546636 ) ) ;
#106323 = CARTESIAN_POINT ( 'NONE',  ( 0.07459516483345089710, 7.629137130509094256, -2.355503875070711572 ) ) ;
#106325 = CARTESIAN_POINT ( 'NONE',  ( 5.782577320554741718, -1.967585831723076772, 0.4389650999883643046 ) ) ;
#106326 = CARTESIAN_POINT ( 'NONE',  ( 5.665228803577522676, 1.767359255132592066, -0.7397141715129780248 ) ) ;
#106327 = CARTESIAN_POINT ( 'NONE',  ( 6.639320575229223031, 6.036153810275548537, 2.598155902862766542 ) ) ;
#106328 = CARTESIAN_POINT ( 'NONE',  ( 4.019203527901527018, -2.096847714747759106, 0.6372333828079318474 ) ) ;
#106329 = B_SPLINE_CURVE_WITH_KNOTS ( 'NONE', 3,
 ( #150748, #2309, #21188, #87291, #202065, #153360, #168540, #37468 ),
 .UNSPECIFIED., .F., .F.,
 ( 4, 2, 2, 4 ),
 ( 3.245370453949652856E-18, 0.0002034531274099211061, 0.0004069062548198396100, 0.0008138125096396765096 ),
 .UNSPECIFIED. ) ;
#106331 = VECTOR ( 'NONE', #60621, 1000.000000000000114 ) ;
#106330 = CARTESIAN_POINT ( 'NONE',  ( 1.499999999999987121, 1.577083334016150751, -0.8660254037844253849 ) ) ;
#106332 = CARTESIAN_POINT ( 'NONE',  ( 2.425908952446104827, -1.891012092455180760, 0.2844710172774585488 ) ) ;
#106333 = CARTESIAN_POINT ( 'NONE',  ( -6.417086777969760902, 6.381022750586497594, 0.7998128361456341429 ) ) ;
#106334 = CARTESIAN_POINT ( 'NONE',  ( 3.809477975315569864, 7.388215371269402532, -0.7216878364870197293 ) ) ;
#106336 = CARTESIAN_POINT ( 'NONE',  ( -0.1351500440973339712, -0.1486198258836557429, -1.983738523497140305 ) ) ;
#106335 = CARTESIAN_POINT ( 'NONE',  ( 3.562078172017826727, 7.339166372451206399, -0.2626806445317174665 ) ) ;
#106337 = CARTESIAN_POINT ( 'NONE',  ( -1.364683531250000748, 10.42187500034139802, 0.000000000000000000 ) ) ;
#106339 = CARTESIAN_POINT ( 'NONE',  ( -7.293360289508603600, 7.473618190706972086, 0.000000000000000000 ) ) ;
#106338 = CARTESIAN_POINT ( 'NONE',  ( 6.128506746050899068, 0.2130254606748181456, 2.181202035047181020 ) ) ;
#106341 = ORIENTED_EDGE ( 'NONE', *, *, #136534, .F. ) ;
#106340 = CARTESIAN_POINT ( 'NONE',  ( 2.484998412088899489, 1.578176246201369093, -0.6962595882179720697 ) ) ;
#106342 = CARTESIAN_POINT ( 'NONE',  ( 5.959260761812961604, -1.790568634313693730, 1.135864312162476297 ) ) ;
#106343 = CARTESIAN_POINT ( 'NONE',  ( 8.281332899848809603, 8.555976559445431562, 0.7998128361456481317 ) ) ;
#106344 = CARTESIAN_POINT ( 'NONE',  ( 4.690231075323689325, 7.559354456931247412, 1.199719254218462483 ) ) ;
#106345 = DIRECTION ( 'NONE',  ( -5.578564026256504688E-16, -1.000000000000000000, -9.066213480720158442E-32 ) ) ;
#106346 = CARTESIAN_POINT ( 'NONE',  ( 0.4319881149899909567, 1.126445828788334991, 1.606065282034954578 ) ) ;
#106347 = CARTESIAN_POINT ( 'NONE',  ( 11.35573736746281348, 9.987295855867177607, -3.554362808847921773 ) ) ;
#106348 = CARTESIAN_POINT ( 'NONE',  ( 4.659198344590585350, 8.587481835331020719, 0.7998128361456462443 ) ) ;
#106349 = FACE_OUTER_BOUND ( 'NONE', #182227, .T. ) ;
#106350 = EDGE_LOOP ( 'NONE', ( #197245, #22688 ) ) ;
#106351 = FACE_OUTER_BOUND ( 'NONE', #126934, .T. ) ;
#106352 = ORIENTED_EDGE ( 'NONE', *, *, #19259, .T. ) ;
#106353 = CARTESIAN_POINT ( 'NONE',  ( 2.578518618993036693, -1.248033014721174228, 1.313194663545588003 ) ) ;
#106354 = VERTEX_POINT ( 'NONE', #11595 ) ;
#106355 = CARTESIAN_POINT ( 'NONE',  ( 8.543609354905870035, 13.11929468069890525, 0.7998128361456462443 ) ) ;
#106356 = CARTESIAN_POINT ( 'NONE',  ( 3.413620815590684199, 7.204584394822967752, 0.7998128361456281477 ) ) ;
#106357 = CARTESIAN_POINT ( 'NONE',  ( 4.002463340116116264, -1.792309675113772371, -0.2618007260343068743 ) ) ;
#106358 = CARTESIAN_POINT ( 'NONE',  ( 7.146556367734771875, 8.470642196179646533, 1.082531754730549967 ) ) ;
#106359 = CARTESIAN_POINT ( 'NONE',  ( 5.892675752748299800, 5.976886221469982274, -0.004604801460011270775 ) ) ;
#106360 = ADVANCED_FACE ( 'NONE', ( #9470 ), #40928, .F. ) ;
#106362 = CARTESIAN_POINT ( 'NONE',  ( -1.364683531250000748, 14.35937500034140157, 0.000000000000000000 ) ) ;
#106361 = CARTESIAN_POINT ( 'NONE',  ( 4.984723811273123140, 1.780707155018296239, 0.5408319247705763999 ) ) ;
#106363 = CARTESIAN_POINT ( 'NONE',  ( 2.249496223418820939, 1.878159554852454338, -0.3759676508649934523 ) ) ;
#106364 = CARTESIAN_POINT ( 'NONE',  ( 1.166719304534512558, -1.648536928579244165, -0.7845717211837843763 ) ) ;
#106365 = CARTESIAN_POINT ( 'NONE',  ( 4.663288057535367237, 8.288536188413402783, 0.5084364831346009916 ) ) ;
#106366 = CARTESIAN_POINT ( 'NONE',  ( -10.99931038725301846, 6.873658557531565627, -3.960823121322395224 ) ) ;
#106367 = CIRCLE ( 'NONE', #109794, 12.00000000000000178 ) ;
#106368 = CARTESIAN_POINT ( 'NONE',  ( 4.876420697298537554, 8.045338245374718866, 0.9427337716215690167 ) ) ;
#106369 = CARTESIAN_POINT ( 'NONE',  ( 7.947120472790364154, 14.95225098152464582, 9.881210053433072460 ) ) ;
#106370 = CARTESIAN_POINT ( 'NONE',  ( -3.666689614532284924, 7.355176389186829589, 0.3694189123316319878 ) ) ;
#106371 = DIRECTION ( 'NONE',  ( 0.000000000000000000, 1.000000000000000000, 0.000000000000000000 ) ) ;
#106372 = CARTESIAN_POINT ( 'NONE',  ( 7.185458225562760148, 8.445751353653788485, -1.082531754730543083 ) ) ;
#106373 = CARTESIAN_POINT ( 'NONE',  ( -5.251085567194491155, 5.020688004682002159, -0.7998128361456221525 ) ) ;
#106374 = CARTESIAN_POINT ( 'NONE',  ( 1.218821504741087969, -0.04963993015681333193, 2.090216850290891326 ) ) ;
#106375 = CARTESIAN_POINT ( 'NONE',  ( 0.07680821025393690105, 0.005952109439256307241, -1.810863387344714193 ) ) ;
#106376 = CARTESIAN_POINT ( 'NONE',  ( -4.557512192488103686, 8.468847991211438497, -0.7998128361456281477 ) ) ;
#106377 = CARTESIAN_POINT ( 'NONE',  ( 2.977373796215292856, 1.734057503958493118, -0.5710112477543202170 ) ) ;
#106378 = CARTESIAN_POINT ( 'NONE',  ( 3.071135375186518690, -2.039199700013223815, -0.8442704067812345503 ) ) ;
#106379 = DIRECTION ( 'NONE',  ( 0.6249999999996046496, -1.033735393388932873E-14, 0.7806247498001164242 ) ) ;
#106380 = CARTESIAN_POINT ( 'NONE',  ( 1.125099709691119276, 1.687896996356451629, 0.8989547360247207575 ) ) ;
#106381 = CARTESIAN_POINT ( 'NONE',  ( 1.117558341675929157, 0.3875481960372212931, -1.930861576554385062 ) ) ;
#106382 = CARTESIAN_POINT ( 'NONE',  ( 4.247558953154553230, 1.941557341479711152, -0.05109960196620494388 ) ) ;
#106383 = ORIENTED_EDGE ( 'NONE', *, *, #167891, .T. ) ;
#106384 = CARTESIAN_POINT ( 'NONE',  ( -1.286813488861816790, 3.613591550242559070, -0.5514626414212303596 ) ) ;
#106386 = CARTESIAN_POINT ( 'NONE',  ( 6.895359103435129811, -1.662453150013998515, 0.8363214020891978073 ) ) ;
#106385 = CARTESIAN_POINT ( 'NONE',  ( -5.503684012504701961, 5.385662534202396934, 0.000000000000000000 ) ) ;
#106387 = CARTESIAN_POINT ( 'NONE',  ( 6.059568310664962709, 6.034194215389424798, 0.7998128361456352531 ) ) ;
#106388 = CARTESIAN_POINT ( 'NONE',  ( 0.000000000000000000, -7.473374494045017968, 9.579665964948883783 ) ) ;
#106389 = CARTESIAN_POINT ( 'NONE',  ( -3.231779075379147770, 6.036511184309971689, 7.500000000000000000 ) ) ;
#106390 = CARTESIAN_POINT ( 'NONE',  ( -5.261446130555064826, 8.296048364692991228, 1.199719254218452935 ) ) ;
#106391 = CARTESIAN_POINT ( 'NONE',  ( 2.771223791512751333, 2.080116120148074010, -0.6901165687889164735 ) ) ;
#106392 = CARTESIAN_POINT ( 'NONE',  ( 1.499999999999996891, 11.67708333401613174, -0.8660254037844378194 ) ) ;
#106393 = CARTESIAN_POINT ( 'NONE',  ( 6.068156270568149324, 9.237210194708310951, 1.199719254218452047 ) ) ;
#106394 = CARTESIAN_POINT ( 'NONE',  ( -2.788906526875773208E-15, 12.18750000000000000, -1.499999999999998446 ) ) ;
#106395 = CARTESIAN_POINT ( 'NONE',  ( 3.721172816245840842, -0.1328194893376876962, 1.820914920514608459 ) ) ;
#106396 = CARTESIAN_POINT ( 'NONE',  ( -2.656508033273816238, 5.186677574539687363, -1.199719254218446718 ) ) ;
#106397 = AXIS2_PLACEMENT_3D ( 'NONE', #152792, #55296, #68317 ) ;
#106398 = CARTESIAN_POINT ( 'NONE',  ( -4.973494386576447823, 8.059877448926631160, 1.114414082037382236 ) ) ;
#106399 = CARTESIAN_POINT ( 'NONE',  ( -0.02968770228140017037, 2.049257630910449990, -2.243713227073070637 ) ) ;
#106400 = CARTESIAN_POINT ( 'NONE',  ( 4.733189744967194024, -1.710186631362722531, 0.7584244158565585092 ) ) ;
#106401 = CARTESIAN_POINT ( 'NONE',  ( 8.938903350111612411, 9.323142084752035430, -0.7998128361456221525 ) ) ;
#106403 = EDGE_CURVE ( 'NONE', #79124, #181635, #92759, .T. ) ;
#106402 = CARTESIAN_POINT ( 'NONE',  ( 1.752441099931791868, 0.6037874858934308975, 1.829501483119711169 ) ) ;
#106404 = CARTESIAN_POINT ( 'NONE',  ( 6.332860960579021814, -1.861707940517230764, -0.6185968553879470644 ) ) ;
#106405 = AXIS2_PLACEMENT_3D ( 'NONE', #7675, #140935, #11948 ) ;
#106406 = CARTESIAN_POINT ( 'NONE',  ( -0.7500000000000179856, 14.54166666666666785, 1.299038105676658228 ) ) ;
#106407 = CARTESIAN_POINT ( 'NONE',  ( -5.900823170445743671, 7.907379670318584353, 1.599625672291269396 ) ) ;
#106408 = CARTESIAN_POINT ( 'NONE',  ( 5.034155109375821446, 4.767602470560229122, -0.7998128361456221525 ) ) ;
#106409 = CARTESIAN_POINT ( 'NONE',  ( -4.123088111887291518, 7.824370207261548416, 0.000000000000000000 ) ) ;
#106410 = CARTESIAN_POINT ( 'NONE',  ( -0.1349523647116790404, -0.1509472049114955194, -2.083628827036696052 ) ) ;
#106411 = CARTESIAN_POINT ( 'NONE',  ( -1.225000000000044276, 0.5416666673494865414, -0.7072540797573158011 ) ) ;
#106413 = EDGE_CURVE ( 'NONE', #36647, #108269, #173085, .T. ) ;
#106412 = CARTESIAN_POINT ( 'NONE',  ( 1.394453263437886604E-15, -2.362500000000000266, 3.474999999999999645 ) ) ;
#106414 = CARTESIAN_POINT ( 'NONE',  ( 5.049704560591026237, 1.530381825397047812, 1.394388655583590042 ) ) ;
#106416 = CARTESIAN_POINT ( 'NONE',  ( -1.201851678989727383E-14, 3.009375000341419248, -1.575800808251660134 ) ) ;
#106415 = CARTESIAN_POINT ( 'NONE',  ( 0.9426144736941791669, -1.451487892885485742, -1.132780452900377099 ) ) ;
#106417 = CARTESIAN_POINT ( 'NONE',  ( 4.764420831138592938, 2.145307606383870969, -0.8259888504972175971 ) ) ;
#106418 = CARTESIAN_POINT ( 'NONE',  ( 7.293923454472091450, 7.611924906413328529, 0.7216878364870317197 ) ) ;
#106420 = LINE ( 'NONE', #156200, #35806 ) ;
#106419 = CARTESIAN_POINT ( 'NONE',  ( 5.289089323106923146, 6.303597310780433283, -1.082531754730548412 ) ) ;
#106421 = CARTESIAN_POINT ( 'NONE',  ( 0.7094041017953250927, -0.3309814517665210509, 2.268137058596159328 ) ) ;
#106422 = CARTESIAN_POINT ( 'NONE',  ( 11.55950211276791251, 12.21999999999998288, 3.221476510067110777 ) ) ;
#106423 = CARTESIAN_POINT ( 'NONE',  ( -6.668631453075260396, 8.873432343378178544, -1.599625672291271394 ) ) ;
#106424 = CARTESIAN_POINT ( 'NONE',  ( 4.663973314478016441, -1.267186161278991419, 1.471619509450792229 ) ) ;
#106425 = ORIENTED_EDGE ( 'NONE', *, *, #138826, .F. ) ;
#106426 = CARTESIAN_POINT ( 'NONE',  ( 8.717529583462638954, 12.15390636647303069, 1.082531754730546636 ) ) ;
#106427 = ORIENTED_EDGE ( 'NONE', *, *, #149589, .T. ) ;
#106428 = CARTESIAN_POINT ( 'NONE',  ( 6.328373294368253354, -0.9077179077918960948, -1.683272687665722467 ) ) ;
#106429 = CARTESIAN_POINT ( 'NONE',  ( 1.013767525470328001, -0.7718518339048777710, -1.542633921862639701 ) ) ;
#106430 = CARTESIAN_POINT ( 'NONE',  ( 5.858611323429600226, -1.916351766245901977, -0.6279953093112633500 ) ) ;
#106432 = CARTESIAN_POINT ( 'NONE',  ( -4.161989969715278015, 4.726297878971393196, -7.499999999999991118 ) ) ;
#106431 = CARTESIAN_POINT ( 'NONE',  ( -8.208571938070008400, 11.66408546346865016, -1.199719254218446718 ) ) ;
#106433 = CARTESIAN_POINT ( 'NONE',  ( 3.285556943749998737, -1.392708332855375764, -1.896917185911906500 ) ) ;
#106435 = CARTESIAN_POINT ( 'NONE',  ( 0.8481071238514601429, 0.5083433500535933236, 1.695271877703796504 ) ) ;
#106434 = CARTESIAN_POINT ( 'NONE',  ( 3.064484987736408872, -1.931880230092865025, -0.7996142226951181708 ) ) ;
#106436 = DIRECTION ( 'NONE',  ( 1.276756478318932585E-15, -1.000000000000000000, 1.665334536937738262E-16 ) ) ;
#106438 = CARTESIAN_POINT ( 'NONE',  ( 4.084120828622629595, -2.267077656855093881, -0.3380819097023191055 ) ) ;
#106437 = CARTESIAN_POINT ( 'NONE',  ( 5.096939404094710468, 4.911127157724081371, 0.000000000000000000 ) ) ;
#106439 = CARTESIAN_POINT ( 'NONE',  ( 2.325747778006927557, 1.687818050649522617, 0.4237310505307323449 ) ) ;
#106440 = CARTESIAN_POINT ( 'NONE',  ( 3.083589872104280705, 5.684939719841914929, 1.199719254218450271 ) ) ;
#106441 = CARTESIAN_POINT ( 'NONE',  ( 2.830460552442021438, -1.048868820301660953, -1.842999677239331113 ) ) ;
#106442 = CARTESIAN_POINT ( 'NONE',  ( -4.864214080903581205, 4.879786425613829692, -0.6392378712632117432 ) ) ;
#106443 = CARTESIAN_POINT ( 'NONE',  ( 2.407222047678575283, 0.3756278383273171095, 1.692465640204628974 ) ) ;
#106444 = CARTESIAN_POINT ( 'NONE',  ( -3.755786496842897795E-14, 2.109375000341444206, -1.570758158831810247 ) ) ;
#106445 = CARTESIAN_POINT ( 'NONE',  ( 1.451354471725987860, 1.406072211568440755, 1.219298000798328507 ) ) ;
#106446 = CARTESIAN_POINT ( 'NONE',  ( 2.488948079679761172, 2.105553563057678712, 0.5292575070172370610 ) ) ;
#106447 = CARTESIAN_POINT ( 'NONE',  ( 4.137209430464448445, 7.978494768850520558, 1.040834085586084257E-14 ) ) ;
#106448 = CARTESIAN_POINT ( 'NONE',  ( 3.907435596788138010, -1.928258004016227378, 0.5899861904685861358 ) ) ;
#106449 = CARTESIAN_POINT ( 'NONE',  ( 1.875000000000001776, 2.052068128417950721, -1.077215146005767577E-13 ) ) ;
#106450 = CARTESIAN_POINT ( 'NONE',  ( -0.7500000000000215383, 3.222916667349487341, 1.299038105676671107 ) ) ;
#106451 = CARTESIAN_POINT ( 'NONE',  ( 0.4637318561061140043, 1.905900585730261110, -0.2794304195078872732 ) ) ;
#106452 = CARTESIAN_POINT ( 'NONE',  ( -1.364683531250010295, 13.88020833367473195, 0.7879004041258445001 ) ) ;
#106453 = CARTESIAN_POINT ( 'NONE',  ( 4.043395766388809598, 0.1113883285390921962, 2.218758960698932192 ) ) ;
#106454 = ORIENTED_EDGE ( 'NONE', *, *, #84254, .T. ) ;
#106455 = DIRECTION ( 'NONE',  ( 0.000000000000000000, -1.000000000000000000, -0.000000000000000000 ) ) ;
#106456 = CARTESIAN_POINT ( 'NONE',  ( 1.499999999999987121, -0.2458333333333099502, 0.8660254037844524744 ) ) ;
#106457 = CARTESIAN_POINT ( 'NONE',  ( 6.428537391173986038, 10.65171072301167854, 0.7998128361456462443 ) ) ;
#106458 = CARTESIAN_POINT ( 'NONE',  ( -0.6823417656250003738, 0.2177083336747515085, -1.181850606188749264 ) ) ;
#106459 = CARTESIAN_POINT ( 'NONE',  ( 0.6630925397578091296, 0.6502370396846578471, 2.123993688044391259 ) ) ;
#106460 = CARTESIAN_POINT ( 'NONE',  ( 4.598074495912657156, 0.8407358649686400565, -1.772743347989129692 ) ) ;
#106461 = CARTESIAN_POINT ( 'NONE',  ( 9.408995418203971894, 11.03987807840189816, 1.082531754730549967 ) ) ;
#106462 = CARTESIAN_POINT ( 'NONE',  ( 5.431070396044226811, 0.1588226897794122738, 2.256881284257936215 ) ) ;
#106463 = CARTESIAN_POINT ( 'NONE',  ( -6.021229618244897885, 7.157760988441397743, 1.082531754730548412 ) ) ;
#106464 = CARTESIAN_POINT ( 'NONE',  ( 3.473143217414649708, 1.863520296645693186, 0.8845801619412340111 ) ) ;
#106465 = CARTESIAN_POINT ( 'NONE',  ( -5.585069213825653023, 8.603332285183535433, -1.199719254218440723 ) ) ;
#106466 = CARTESIAN_POINT ( 'NONE',  ( -1.201851678989727383E-14, 3.243750000682814161, 1.732050807568877637 ) ) ;
#106467 = CARTESIAN_POINT ( 'NONE',  ( 1.364683531249988535, 5.467708333674750953, -0.7879004041258300672 ) ) ;
#106468 = CARTESIAN_POINT ( 'NONE',  ( 5.026551685794930613, 1.789549103570491573, 0.5443708928771497924 ) ) ;
#106469 = CARTESIAN_POINT ( 'NONE',  ( 3.217127751380299383, 1.692560603008624875, 0.3766165182450386117 ) ) ;
#106470 = CARTESIAN_POINT ( 'NONE',  ( 2.928976884739741493, -1.170936322307249089, -1.287801759770091925 ) ) ;
#106471 = CARTESIAN_POINT ( 'NONE',  ( 0.3809655214361170050, -0.2885804254640594868, -2.274098033663536356 ) ) ;
#106472 = CARTESIAN_POINT ( 'NONE',  ( 0.7806487521475922176, -1.224371414366259847, 1.835764474286231129 ) ) ;
#106473 = CARTESIAN_POINT ( 'NONE',  ( 5.144118995967028596, 0.6083014027435985627, 2.000272865920887266 ) ) ;
#106474 = CARTESIAN_POINT ( 'NONE',  ( 6.087830645824786835, -1.932811661901209010, -0.1881662411436606785 ) ) ;
#106476 = ORIENTED_EDGE ( 'NONE', *, *, #195653, .F. ) ;
#106475 = CARTESIAN_POINT ( 'NONE',  ( 8.279175489589290393, 15.22702719263014615, 8.688122134494948412 ) ) ;
#106477 = SURFACE_STYLE_USAGE ( .BOTH. , #4616 ) ;
#106478 = CARTESIAN_POINT ( 'NONE',  ( 0.4225002777262388265, -1.427939226333583500, -1.423959630194884696 ) ) ;
#106479 = CARTESIAN_POINT ( 'NONE',  ( 1.055114822555893728, 0.4192091730233596381, 2.078585086915801128 ) ) ;
#106480 = DIRECTION ( 'NONE',  ( 0.000000000000000000, 7.228014483236694583E-17, -1.000000000000000000 ) ) ;
#106481 = CARTESIAN_POINT ( 'NONE',  ( -1.400751299551194151, 7.315968950354509559, 4.333496285525718861 ) ) ;
#106482 = CARTESIAN_POINT ( 'NONE',  ( -9.612894607289142357, 11.17379744904754801, -1.199719254218441611 ) ) ;
#106483 = CARTESIAN_POINT ( 'NONE',  ( 5.472687561410540802, 9.536552588287639409, 0.7998128361456462443 ) ) ;
#106484 = FILL_AREA_STYLE ('',( #39297 ) ) ;
#106485 = CARTESIAN_POINT ( 'NONE',  ( 4.459475772512963232, 0.3974328844052883447, -1.781742007231662983 ) ) ;
#106486 = ORIENTED_EDGE ( 'NONE', *, *, #137412, .T. ) ;
#106487 = CARTESIAN_POINT ( 'NONE',  ( -4.462041952228957165, 5.338708711422782471, -1.082531754730549967 ) ) ;
#106488 = EDGE_CURVE ( 'NONE', #101986, #22926, #26997, .T. ) ;
#106489 = CARTESIAN_POINT ( 'NONE',  ( -0.4644097342743090384, -8.200000000000015277, -9.488641820551084294 ) ) ;
#106490 = CARTESIAN_POINT ( 'NONE',  ( -3.285556943750000514, -3.026041666188709733, -1.896917185911906500 ) ) ;
#106491 = CARTESIAN_POINT ( 'NONE',  ( -8.179646747746328828, 8.437342715325849341, -0.7998128361456291469 ) ) ;
#106492 = CARTESIAN_POINT ( 'NONE',  ( 1.793229165239007994, -0.1032543025433537293, -2.017296481459893709 ) ) ;
#106493 = CARTESIAN_POINT ( 'NONE',  ( 5.877994779194309238, 1.310017027744770246, 1.775731318763192013 ) ) ;
#106494 = CARTESIAN_POINT ( 'NONE',  ( -4.014095998097799267, 6.840806543492835345, -1.199719254218450271 ) ) ;
#106495 = CARTESIAN_POINT ( 'NONE',  ( 2.606119654932341767, 1.860434991719280173, 0.05107381154999082046 ) ) ;
#106496 = CARTESIAN_POINT ( 'NONE',  ( 4.162516854595432747, 4.815023404238158555, 1.199719254218464037 ) ) ;
#106497 = CARTESIAN_POINT ( 'NONE',  ( 4.909461021924240498, 7.781436054670031410, 1.082531754730549078 ) ) ;
#106498 = CARTESIAN_POINT ( 'NONE',  ( -3.744022975668147790, 7.519777238254810925, -0.7998128361456281477 ) ) ;
#106499 = CARTESIAN_POINT ( 'NONE',  ( -9.318531651294266638, 9.766041769465124034, -0.7998128361456291469 ) ) ;
#106500 = CARTESIAN_POINT ( 'NONE',  ( 4.582524934692378871, -1.771534430979417429, -0.4408631061849078714 ) ) ;
#106501 = CIRCLE ( 'NONE', #196431, 4.500000000000000000 ) ;
#106503 = CARTESIAN_POINT ( 'NONE',  ( -4.461457896923207933, 7.279594253155052819, -1.276495073192641883 ) ) ;
#106502 = CARTESIAN_POINT ( 'NONE',  ( -8.086512275908061653, 8.398962174839683215, 0.000000000000000000 ) ) ;
#106504 = CARTESIAN_POINT ( 'NONE',  ( 5.943507298343291723, 7.226397084328657350, -1.228854570503196575 ) ) ;
#106505 = CARTESIAN_POINT ( 'NONE',  ( 0.4207071466195873022, 0.6554624660736629860, 1.605403739708724631 ) ) ;
#106506 = CARTESIAN_POINT ( 'NONE',  ( 0.1810874682179625661, -0.8250252819957092365, 1.532327275369157915 ) ) ;
#106507 = CARTESIAN_POINT ( 'NONE',  ( 5.725286558339668375, -0.06233732282829743815, 2.307013574275817547 ) ) ;
#106508 = CARTESIAN_POINT ( 'NONE',  ( 6.201928923608456046, 6.200281597156833691, 0.7998128361456352531 ) ) ;
#106509 = CARTESIAN_POINT ( 'NONE',  ( 6.661405305706385782, 0.3767857563467743032, -2.128362917677539379 ) ) ;
#106510 = CARTESIAN_POINT ( 'NONE',  ( 5.524057522564145728, 8.532151978711786100, 1.199719254218462483 ) ) ;
#106511 = CARTESIAN_POINT ( 'NONE',  ( 5.677245700908649439, -1.026343684741271023, -2.056567161392281129 ) ) ;
#106512 = DIRECTION ( 'NONE',  ( 0.000000000000000000, 0.000000000000000000, 1.000000000000000000 ) ) ;
#106513 = CARTESIAN_POINT ( 'NONE',  ( -5.088052786878465739, 9.158088361325352977, 0.000000000000000000 ) ) ;
#106514 = CARTESIAN_POINT ( 'NONE',  ( 5.489076674590072535, 1.649195787720953987, -0.8828566466120502110 ) ) ;
#106515 = AXIS2_PLACEMENT_3D ( 'NONE', #23813, #101071, #84830 ) ;
#106517 = CARTESIAN_POINT ( 'NONE',  ( -5.646044625448194410, 5.551749915969804938, 0.000000000000000000 ) ) ;
#106516 = CARTESIAN_POINT ( 'NONE',  ( 3.164218664783400747, 1.912571728330178855, -0.004505864839042527346 ) ) ;
#106518 = CARTESIAN_POINT ( 'NONE',  ( 5.567066847960510323, -1.993696164035433371, -0.9465883713010987410 ) ) ;
#106519 = CARTESIAN_POINT ( 'NONE',  ( 4.557876730116875663, 1.221875164117897539, 1.729014733294547801 ) ) ;
#106520 = CARTESIAN_POINT ( 'NONE',  ( -2.754243431018125239E-14, 0.8750000006828161370, 1.414508159514559438 ) ) ;
#106521 = CARTESIAN_POINT ( 'NONE',  ( -10.41437568897905486, 3.950072978995299522, 5.872581675051923966 ) ) ;
#106522 = CARTESIAN_POINT ( 'NONE',  ( 6.346625304528514810, 6.577020074804287297, 0.000000000000000000 ) ) ;
#106523 = CARTESIAN_POINT ( 'NONE',  ( -5.763624699140883934, 6.857221916153382502, -1.082531754730549967 ) ) ;
#106524 = CARTESIAN_POINT ( 'NONE',  ( 5.883467998083113493, 0.1561420574479575329, -2.114776682634044391 ) ) ;
#106525 = CARTESIAN_POINT ( 'NONE',  ( 1.870602726103831381, 1.187374005633199836, 1.978520242944050711 ) ) ;
#106526 = CARTESIAN_POINT ( 'NONE',  ( 3.930091730393743710, 1.087902980620155891, 1.632394305395828304 ) ) ;
#106527 = CARTESIAN_POINT ( 'NONE',  ( -3.800028193580205826, 7.655393002477361541, -0.7998128361456481317 ) ) ;
#106528 = CARTESIAN_POINT ( 'NONE',  ( 6.016483441405136467, 0.8307744727026479259, 1.888021813390627246 ) ) ;
#106529 = CARTESIAN_POINT ( 'NONE',  ( 4.582292731738905722, 5.408724944192588424, -1.082531754730548412 ) ) ;
#106530 = CARTESIAN_POINT ( 'NONE',  ( 4.523580528814945545, 5.306540700819438960, 1.199719254218452047 ) ) ;
